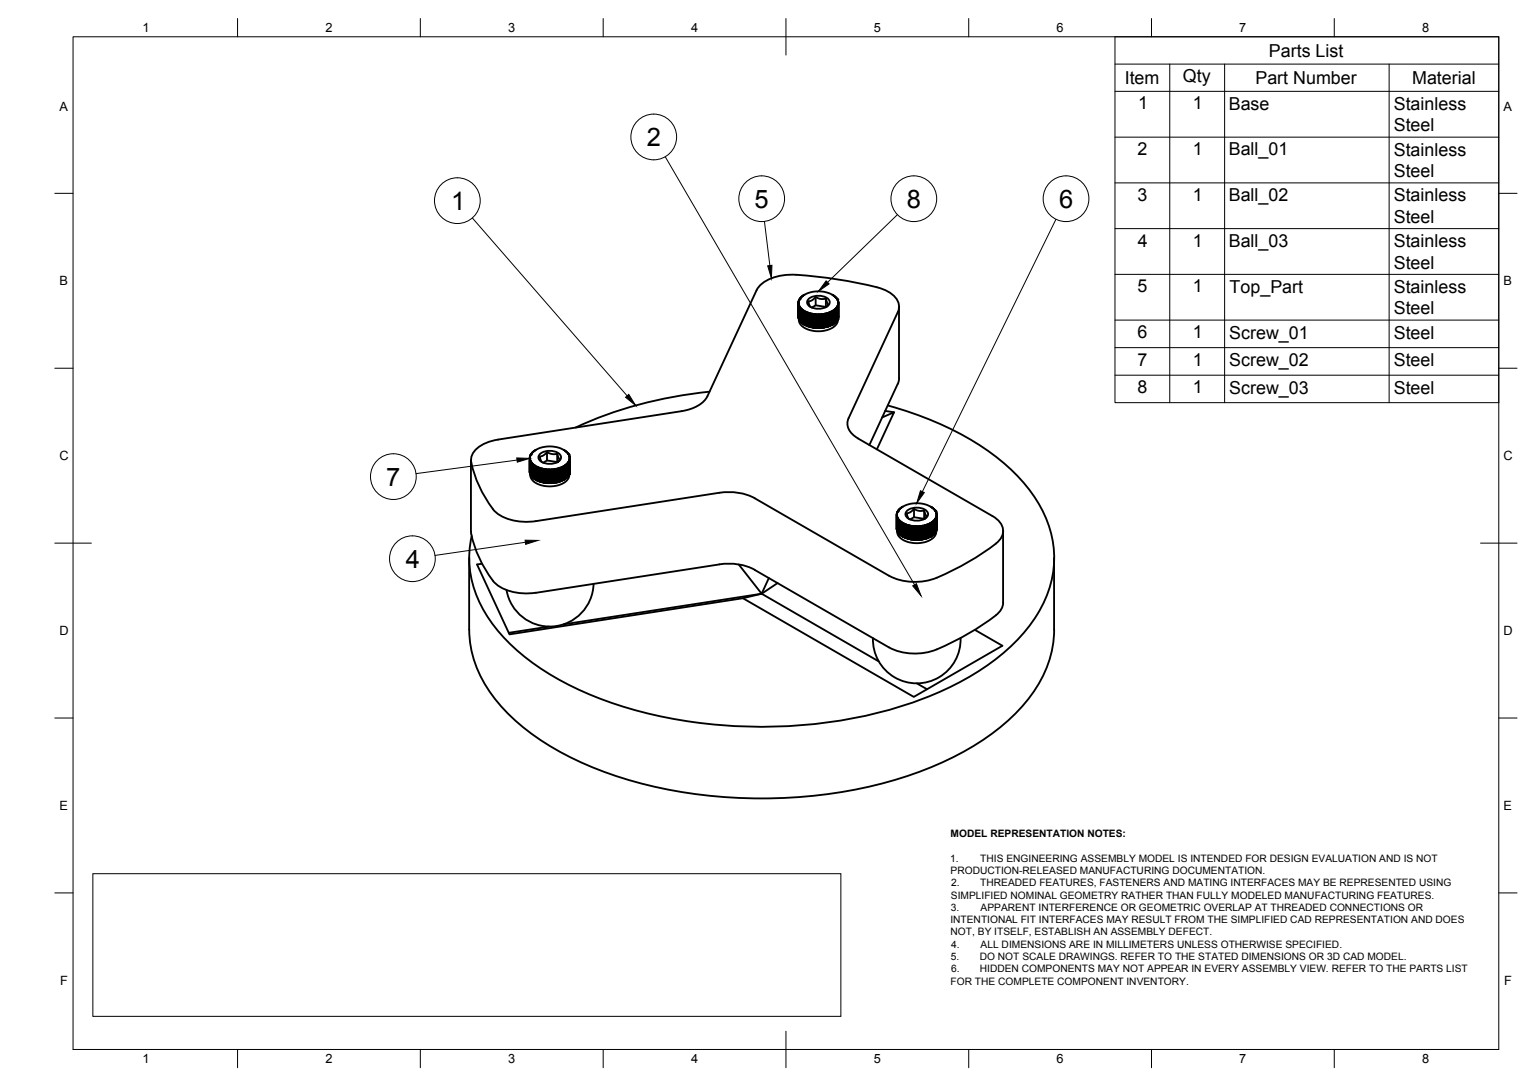
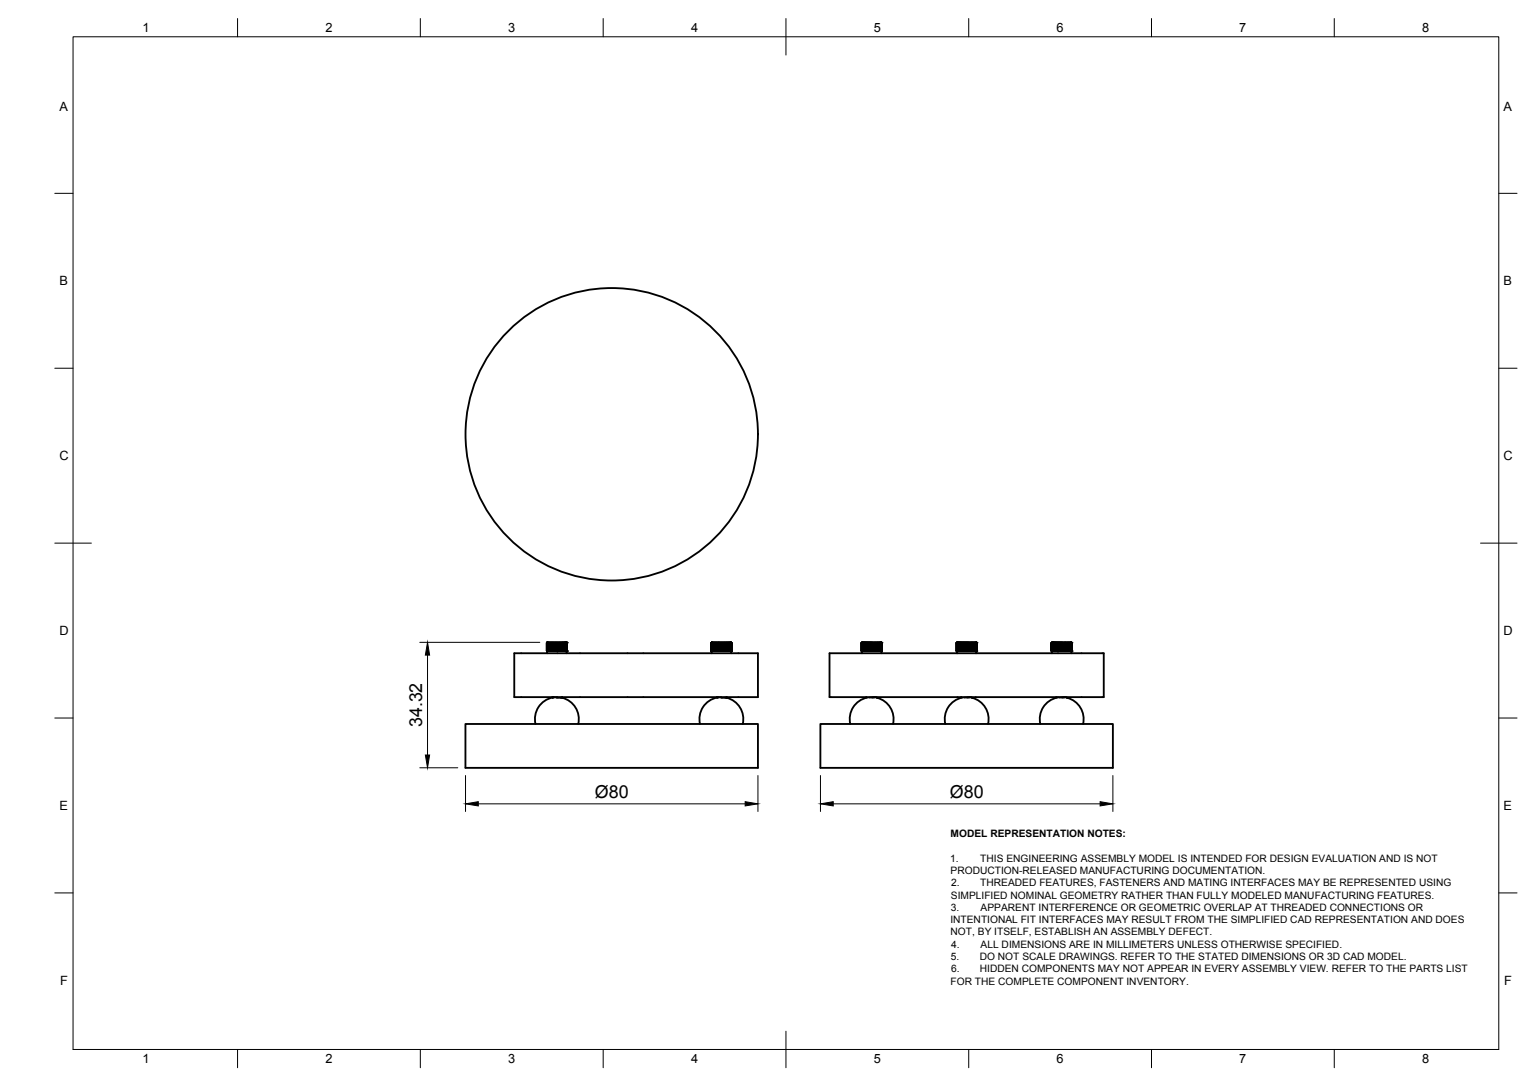
ISO-10303-21;
HEADER;
/* Generated by software containing ST-Developer
 * from STEP Tools, Inc. (www.steptools.com) 
 */

FILE_DESCRIPTION(
/* description */ (''),
/* implementation_level */ '2;1');

FILE_NAME(
/* name */ 'BR-152',
/* time_stamp */ '2026-10-05T00:14:20-07:00',
/* author */ (''),
/* organization */ (''),
/* preprocessor_version */ 'ST-DEVELOPER v20.2',
/* originating_system */ 'Autodesk Translation Framework v15.15.0.0',
/* authorisation */ '');

FILE_SCHEMA (('AUTOMOTIVE_DESIGN { 1 0 10303 214 3 1 1 }'));
ENDSEC;

DATA;
#10=MECHANICAL_DESIGN_GEOMETRIC_PRESENTATION_REPRESENTATION('',(#3371,#3372,
#3373,#3374,#3375,#3376,#3377,#3378),#75336);
#11=ITEM_DEFINED_TRANSFORMATION($,$,#32119,#36337);
#12=ITEM_DEFINED_TRANSFORMATION($,$,#32134,#36338);
#13=ITEM_DEFINED_TRANSFORMATION($,$,#32137,#36339);
#14=ITEM_DEFINED_TRANSFORMATION($,$,#32140,#36340);
#15=ITEM_DEFINED_TRANSFORMATION($,$,#32143,#36341);
#16=ITEM_DEFINED_TRANSFORMATION($,$,#32197,#36342);
#17=ITEM_DEFINED_TRANSFORMATION($,$,#33577,#36343);
#18=ITEM_DEFINED_TRANSFORMATION($,$,#34957,#36344);
#19=(
REPRESENTATION_RELATIONSHIP($,$,#75368,#75367)
REPRESENTATION_RELATIONSHIP_WITH_TRANSFORMATION(#11)
SHAPE_REPRESENTATION_RELATIONSHIP()
);
#20=(
REPRESENTATION_RELATIONSHIP($,$,#75369,#75367)
REPRESENTATION_RELATIONSHIP_WITH_TRANSFORMATION(#12)
SHAPE_REPRESENTATION_RELATIONSHIP()
);
#21=(
REPRESENTATION_RELATIONSHIP($,$,#75370,#75367)
REPRESENTATION_RELATIONSHIP_WITH_TRANSFORMATION(#13)
SHAPE_REPRESENTATION_RELATIONSHIP()
);
#22=(
REPRESENTATION_RELATIONSHIP($,$,#75371,#75367)
REPRESENTATION_RELATIONSHIP_WITH_TRANSFORMATION(#14)
SHAPE_REPRESENTATION_RELATIONSHIP()
);
#23=(
REPRESENTATION_RELATIONSHIP($,$,#75372,#75367)
REPRESENTATION_RELATIONSHIP_WITH_TRANSFORMATION(#15)
SHAPE_REPRESENTATION_RELATIONSHIP()
);
#24=(
REPRESENTATION_RELATIONSHIP($,$,#75373,#75367)
REPRESENTATION_RELATIONSHIP_WITH_TRANSFORMATION(#16)
SHAPE_REPRESENTATION_RELATIONSHIP()
);
#25=(
REPRESENTATION_RELATIONSHIP($,$,#75374,#75367)
REPRESENTATION_RELATIONSHIP_WITH_TRANSFORMATION(#17)
SHAPE_REPRESENTATION_RELATIONSHIP()
);
#26=(
REPRESENTATION_RELATIONSHIP($,$,#75375,#75367)
REPRESENTATION_RELATIONSHIP_WITH_TRANSFORMATION(#18)
SHAPE_REPRESENTATION_RELATIONSHIP()
);
#27=CONTEXT_DEPENDENT_SHAPE_REPRESENTATION(#19,#75359);
#28=CONTEXT_DEPENDENT_SHAPE_REPRESENTATION(#20,#75360);
#29=CONTEXT_DEPENDENT_SHAPE_REPRESENTATION(#21,#75361);
#30=CONTEXT_DEPENDENT_SHAPE_REPRESENTATION(#22,#75362);
#31=CONTEXT_DEPENDENT_SHAPE_REPRESENTATION(#23,#75363);
#32=CONTEXT_DEPENDENT_SHAPE_REPRESENTATION(#24,#75364);
#33=CONTEXT_DEPENDENT_SHAPE_REPRESENTATION(#25,#75365);
#34=CONTEXT_DEPENDENT_SHAPE_REPRESENTATION(#26,#75366);
#35=NEXT_ASSEMBLY_USAGE_OCCURRENCE('Base:1','Base:1','Base:1',#75377,#75378,
'Base:1');
#36=NEXT_ASSEMBLY_USAGE_OCCURRENCE('Ball_01:1','Ball_01:1','Ball_01:1',
#75377,#75379,'Ball_01:1');
#37=NEXT_ASSEMBLY_USAGE_OCCURRENCE('Ball_02:1','Ball_02:1','Ball_02:1',
#75377,#75380,'Ball_02:1');
#38=NEXT_ASSEMBLY_USAGE_OCCURRENCE('Ball_03:1','Ball_03:1','Ball_03:1',
#75377,#75381,'Ball_03:1');
#39=NEXT_ASSEMBLY_USAGE_OCCURRENCE('Top_Part:1','Top_Part:1',
'Top_Part:1',#75377,#75382,'Top_Part:1');
#40=NEXT_ASSEMBLY_USAGE_OCCURRENCE('Screw_01:1','Screw_01:1',
'Screw_01:1',#75377,#75383,'Screw_01:1');
#41=NEXT_ASSEMBLY_USAGE_OCCURRENCE('Screw_02:1','Screw_02:1',
'Screw_02:1',#75377,#75384,'Screw_02:1');
#42=NEXT_ASSEMBLY_USAGE_OCCURRENCE('Screw_03:1','Screw_03:1',
'Screw_03:1',#75377,#75385,'Screw_03:1');
#43=(
BOUNDED_SURFACE()
B_SPLINE_SURFACE(1,2,((#54054,#54055,#54056,#54057,#54058,#54059,#54060,
#54061,#54062,#54063,#54064,#54065,#54066,#54067,#54068,#54069,#54070,#54071,
#54072,#54073,#54074,#54075,#54076,#54077,#54078,#54079,#54080,#54081,#54082,
#54083,#54084,#54085,#54086,#54087,#54088,#54089,#54090,#54091,#54092,#54093,
#54094,#54095,#54096,#54097,#54098,#54099,#54100,#54101,#54102,#54103,#54104,
#54105,#54106,#54107,#54108,#54109,#54110,#54111,#54112,#54113,#54114,#54115,
#54116,#54117,#54118,#54119,#54120,#54121,#54122,#54123,#54124,#54125,#54126,
#54127,#54128,#54129,#54130,#54131,#54132,#54133,#54134,#54135,#54136,#54137,
#54138,#54139,#54140,#54141,#54142,#54143,#54144,#54145,#54146,#54147,#54148,
#54149,#54150,#54151,#54152,#54153,#54154,#54155,#54156,#54157,#54158,#54159,
#54160,#54161,#54162,#54163,#54164,#54165,#54166,#54167,#54168,#54169,#54170,
#54171,#54172,#54173,#54174,#54175,#54176,#54177,#54178,#54179,#54180,#54181,
#54182,#54183,#54184,#54185,#54186,#54187,#54188,#54189,#54190,#54191,#54192,
#54193,#54194,#54195,#54196,#54197,#54198,#54199,#54200,#54201,#54202,#54203,
#54204,#54205,#54206,#54207,#54208,#54209,#54210,#54211,#54212,#54213,#54214,
#54215,#54216,#54217,#54218,#54219,#54220,#54221,#54222,#54223,#54224,#54225,
#54226,#54227,#54228,#54229,#54230,#54231,#54232,#54233,#54234,#54235,#54236,
#54237,#54238,#54239,#54240,#54241,#54242,#54243,#54244,#54245,#54246,#54247,
#54248,#54249,#54250,#54251,#54252,#54253,#54254,#54255,#54256,#54257,#54258,
#54259,#54260,#54261,#54262,#54263,#54264,#54265,#54266,#54267,#54268,#54269,
#54270,#54271,#54272,#54273,#54274,#54275,#54276,#54277,#54278,#54279,#54280,
#54281,#54282,#54283,#54284,#54285,#54286,#54287,#54288,#54289,#54290,#54291,
#54292,#54293,#54294,#54295,#54296,#54297,#54298,#54299,#54300,#54301,#54302,
#54303,#54304,#54305,#54306,#54307,#54308,#54309,#54310,#54311,#54312,#54313,
#54314,#54315,#54316,#54317,#54318,#54319,#54320,#54321,#54322,#54323,#54324,
#54325,#54326,#54327,#54328,#54329,#54330,#54331,#54332,#54333,#54334,#54335,
#54336,#54337,#54338,#54339,#54340,#54341,#54342,#54343,#54344,#54345,#54346,
#54347,#54348,#54349,#54350,#54351,#54352,#54353,#54354,#54355,#54356,#54357,
#54358,#54359,#54360,#54361,#54362,#54363,#54364,#54365,#54366,#54367,#54368,
#54369,#54370,#54371,#54372,#54373,#54374,#54375,#54376,#54377,#54378,#54379,
#54380,#54381,#54382,#54383,#54384,#54385,#54386,#54387,#54388,#54389,#54390,
#54391,#54392,#54393,#54394,#54395,#54396,#54397,#54398,#54399,#54400,#54401,
#54402,#54403,#54404,#54405,#54406,#54407,#54408,#54409,#54410,#54411,#54412,
#54413,#54414,#54415,#54416,#54417,#54418,#54419,#54420,#54421,#54422,#54423,
#54424,#54425,#54426),(#54427,#54428,#54429,#54430,#54431,#54432,#54433,
#54434,#54435,#54436,#54437,#54438,#54439,#54440,#54441,#54442,#54443,#54444,
#54445,#54446,#54447,#54448,#54449,#54450,#54451,#54452,#54453,#54454,#54455,
#54456,#54457,#54458,#54459,#54460,#54461,#54462,#54463,#54464,#54465,#54466,
#54467,#54468,#54469,#54470,#54471,#54472,#54473,#54474,#54475,#54476,#54477,
#54478,#54479,#54480,#54481,#54482,#54483,#54484,#54485,#54486,#54487,#54488,
#54489,#54490,#54491,#54492,#54493,#54494,#54495,#54496,#54497,#54498,#54499,
#54500,#54501,#54502,#54503,#54504,#54505,#54506,#54507,#54508,#54509,#54510,
#54511,#54512,#54513,#54514,#54515,#54516,#54517,#54518,#54519,#54520,#54521,
#54522,#54523,#54524,#54525,#54526,#54527,#54528,#54529,#54530,#54531,#54532,
#54533,#54534,#54535,#54536,#54537,#54538,#54539,#54540,#54541,#54542,#54543,
#54544,#54545,#54546,#54547,#54548,#54549,#54550,#54551,#54552,#54553,#54554,
#54555,#54556,#54557,#54558,#54559,#54560,#54561,#54562,#54563,#54564,#54565,
#54566,#54567,#54568,#54569,#54570,#54571,#54572,#54573,#54574,#54575,#54576,
#54577,#54578,#54579,#54580,#54581,#54582,#54583,#54584,#54585,#54586,#54587,
#54588,#54589,#54590,#54591,#54592,#54593,#54594,#54595,#54596,#54597,#54598,
#54599,#54600,#54601,#54602,#54603,#54604,#54605,#54606,#54607,#54608,#54609,
#54610,#54611,#54612,#54613,#54614,#54615,#54616,#54617,#54618,#54619,#54620,
#54621,#54622,#54623,#54624,#54625,#54626,#54627,#54628,#54629,#54630,#54631,
#54632,#54633,#54634,#54635,#54636,#54637,#54638,#54639,#54640,#54641,#54642,
#54643,#54644,#54645,#54646,#54647,#54648,#54649,#54650,#54651,#54652,#54653,
#54654,#54655,#54656,#54657,#54658,#54659,#54660,#54661,#54662,#54663,#54664,
#54665,#54666,#54667,#54668,#54669,#54670,#54671,#54672,#54673,#54674,#54675,
#54676,#54677,#54678,#54679,#54680,#54681,#54682,#54683,#54684,#54685,#54686,
#54687,#54688,#54689,#54690,#54691,#54692,#54693,#54694,#54695,#54696,#54697,
#54698,#54699,#54700,#54701,#54702,#54703,#54704,#54705,#54706,#54707,#54708,
#54709,#54710,#54711,#54712,#54713,#54714,#54715,#54716,#54717,#54718,#54719,
#54720,#54721,#54722,#54723,#54724,#54725,#54726,#54727,#54728,#54729,#54730,
#54731,#54732,#54733,#54734,#54735,#54736,#54737,#54738,#54739,#54740,#54741,
#54742,#54743,#54744,#54745,#54746,#54747,#54748,#54749,#54750,#54751,#54752,
#54753,#54754,#54755,#54756,#54757,#54758,#54759,#54760,#54761,#54762,#54763,
#54764,#54765,#54766,#54767,#54768,#54769,#54770,#54771,#54772,#54773,#54774,
#54775,#54776,#54777,#54778,#54779,#54780,#54781,#54782,#54783,#54784,#54785,
#54786,#54787,#54788,#54789,#54790,#54791,#54792,#54793,#54794,#54795,#54796,
#54797,#54798,#54799)),.UNSPECIFIED.,.F.,.F.,.F.)
B_SPLINE_SURFACE_WITH_KNOTS((2,2),(3,2,2,2,2,2,2,2,2,2,2,2,2,2,2,2,2,2,
2,2,2,2,2,2,2,2,2,2,2,2,2,2,2,2,2,2,2,2,2,2,2,2,2,2,2,2,2,2,2,2,2,2,2,2,
2,2,2,2,2,2,2,2,2,2,2,2,2,2,2,2,2,2,2,2,2,2,2,2,2,2,2,2,2,2,2,2,2,2,2,2,
2,2,2,2,2,2,2,2,2,2,2,2,2,2,2,2,2,2,2,2,2,2,2,2,2,2,2,2,2,2,2,2,2,2,2,2,
2,2,2,2,2,2,2,2,2,2,2,2,2,2,2,2,2,2,2,2,2,2,2,2,2,2,2,2,2,2,2,2,2,2,2,2,
2,2,2,2,2,2,2,2,2,2,2,2,2,2,2,2,2,2,2,2,2,2,2,2,3),(-2.30253870309941E-5,
1.),(0.,0.00537634408602151,0.010752688172043,0.0161290322580645,0.021505376344086,
0.0268817204301075,0.032258064516129,0.0376344086021505,0.043010752688172,
0.0483870967741935,0.0537634408602151,0.0591397849462366,0.0645161290322581,
0.0698924731182796,0.0752688172043011,0.0806451612903226,0.0860215053763441,
0.0913978494623656,0.0967741935483871,0.102150537634409,0.10752688172043,
0.112903225806452,0.118279569892473,0.123655913978495,0.129032258064516,
0.134408602150538,0.139784946236559,0.145161290322581,0.150537634408602,
0.155913978494624,0.161290322580645,0.166666666666667,0.172043010752688,
0.17741935483871,0.182795698924731,0.188172043010753,0.193548387096774,
0.198924731182796,0.204301075268817,0.209677419354839,0.21505376344086,
0.220430107526882,0.225806451612903,0.231182795698925,0.236559139784946,
0.241935483870968,0.247311827956989,0.252688172043011,0.258064516129032,
0.263440860215054,0.268817204301075,0.274193548387097,0.279569892473118,
0.28494623655914,0.290322580645161,0.295698924731183,0.301075268817204,
0.306451612903226,0.311827956989247,0.317204301075269,0.32258064516129,
0.327956989247312,0.333333333333333,0.338709677419355,0.344086021505376,
0.349462365591398,0.354838709677419,0.360215053763441,0.365591397849462,
0.370967741935484,0.376344086021505,0.381720430107527,0.387096774193548,
0.39247311827957,0.397849462365591,0.403225806451613,0.408602150537634,
0.413978494623656,0.419354838709677,0.424731182795699,0.43010752688172,
0.435483870967742,0.440860215053763,0.446236559139785,0.451612903225806,
0.456989247311828,0.462365591397849,0.467741935483871,0.473118279569892,
0.478494623655914,0.483870967741935,0.489247311827957,0.494623655913978,
0.5,0.505376344086022,0.510752688172043,0.516129032258065,0.521505376344086,
0.526881720430108,0.532258064516129,0.537634408602151,0.543010752688172,
0.548387096774194,0.553763440860215,0.559139784946237,0.564516129032258,
0.56989247311828,0.575268817204301,0.580645161290323,0.586021505376344,
0.591397849462366,0.596774193548387,0.602150537634409,0.60752688172043,
0.612903225806452,0.618279569892473,0.623655913978495,0.629032258064516,
0.634408602150538,0.639784946236559,0.645161290322581,0.650537634408602,
0.655913978494624,0.661290322580645,0.666666666666667,0.672043010752688,
0.67741935483871,0.682795698924731,0.688172043010753,0.693548387096774,
0.698924731182796,0.704301075268817,0.709677419354839,0.71505376344086,
0.720430107526882,0.725806451612903,0.731182795698925,0.736559139784946,
0.741935483870968,0.747311827956989,0.752688172043011,0.758064516129032,
0.763440860215054,0.768817204301075,0.774193548387097,0.779569892473118,
0.78494623655914,0.790322580645161,0.795698924731183,0.801075268817204,
0.806451612903226,0.811827956989247,0.817204301075269,0.82258064516129,
0.827956989247312,0.833333333333333,0.838709677419355,0.844086021505376,
0.849462365591398,0.854838709677419,0.860215053763441,0.865591397849462,
0.870967741935484,0.876344086021505,0.881720430107527,0.887096774193548,
0.89247311827957,0.897849462365591,0.903225806451613,0.908602150537634,
0.913978494623656,0.919354838709677,0.924731182795699,0.93010752688172,
0.935483870967742,0.940860215053763,0.946236559139785,0.951612903225806,
0.956989247311828,0.962365591397849,0.967741935483871,0.973118279569892,
0.978494623655914,0.983870967741935,0.989247311827957,0.994623655913978,
1.),.UNSPECIFIED.)
GEOMETRIC_REPRESENTATION_ITEM()
RATIONAL_B_SPLINE_SURFACE(((1.,0.866025403784439,1.,0.866025403784439,1.,
0.866025403784439,1.,0.866025403784439,1.,0.866025403784439,1.,0.866025403784439,
1.,0.866025403784439,1.,0.866025403784439,1.,0.866025403784439,1.,0.866025403784439,
1.,0.866025403784439,1.,0.866025403784439,1.,0.866025403784439,1.,0.866025403784439,
1.,0.866025403784439,1.,0.866025403784439,1.,0.866025403784439,1.,0.866025403784439,
1.,0.866025403784439,1.,0.866025403784439,1.,0.866025403784439,1.,0.866025403784439,
1.,0.866025403784439,1.,0.866025403784439,1.,0.866025403784439,1.,0.866025403784439,
1.,0.866025403784439,1.,0.866025403784439,1.,0.866025403784439,1.,0.866025403784439,
1.,0.866025403784439,1.,0.866025403784439,1.,0.866025403784439,1.,0.866025403784439,
1.,0.866025403784439,1.,0.866025403784439,1.,0.866025403784439,1.,0.866025403784439,
1.,0.866025403784439,1.,0.866025403784439,1.,0.866025403784439,1.,0.866025403784439,
1.,0.866025403784439,1.,0.866025403784439,1.,0.866025403784439,1.,0.866025403784439,
1.,0.866025403784439,1.,0.866025403784439,1.,0.866025403784439,1.,0.866025403784439,
1.,0.866025403784439,1.,0.866025403784439,1.,0.866025403784439,1.,0.866025403784439,
1.,0.866025403784439,1.,0.866025403784439,1.,0.866025403784439,1.,0.866025403784439,
1.,0.866025403784439,1.,0.866025403784439,1.,0.866025403784439,1.,0.866025403784439,
1.,0.866025403784439,1.,0.866025403784439,1.,0.866025403784439,1.,0.866025403784439,
1.,0.866025403784439,1.,0.866025403784439,1.,0.866025403784439,1.,0.866025403784439,
1.,0.866025403784439,1.,0.866025403784439,1.,0.866025403784439,1.,0.866025403784439,
1.,0.866025403784439,1.,0.866025403784439,1.,0.866025403784439,1.,0.866025403784439,
1.,0.866025403784439,1.,0.866025403784439,1.,0.866025403784439,1.,0.866025403784439,
1.,0.866025403784439,1.,0.866025403784439,1.,0.866025403784439,1.,0.866025403784439,
1.,0.866025403784439,1.,0.866025403784439,1.,0.866025403784439,1.,0.866025403784439,
1.,0.866025403784439,1.,0.866025403784439,1.,0.866025403784439,1.,0.866025403784439,
1.,0.866025403784439,1.,0.866025403784439,1.,0.866025403784439,1.,0.866025403784439,
1.,0.866025403784439,1.,0.866025403784439,1.,0.866025403784439,1.,0.866025403784439,
1.,0.866025403784439,1.,0.866025403784439,1.,0.866025403784439,1.,0.866025403784439,
1.,0.866025403784439,1.,0.866025403784439,1.,0.866025403784439,1.,0.866025403784439,
1.,0.866025403784439,1.,0.866025403784439,1.,0.866025403784439,1.,0.866025403784439,
1.,0.866025403784439,1.,0.866025403784439,1.,0.866025403784439,1.,0.866025403784439,
1.,0.866025403784439,1.,0.866025403784439,1.,0.866025403784439,1.,0.866025403784439,
1.,0.866025403784439,1.,0.866025403784439,1.,0.866025403784439,1.,0.866025403784439,
1.,0.866025403784439,1.,0.866025403784439,1.,0.866025403784439,1.,0.866025403784439,
1.,0.866025403784439,1.,0.866025403784439,1.,0.866025403784439,1.,0.866025403784439,
1.,0.866025403784439,1.,0.866025403784439,1.,0.866025403784439,1.,0.866025403784439,
1.,0.866025403784439,1.,0.866025403784439,1.,0.866025403784439,1.,0.866025403784439,
1.,0.866025403784439,1.,0.866025403784439,1.,0.866025403784439,1.,0.866025403784439,
1.,0.866025403784439,1.,0.866025403784439,1.,0.866025403784439,1.,0.866025403784439,
1.,0.866025403784439,1.,0.866025403784439,1.,0.866025403784439,1.,0.866025403784439,
1.,0.866025403784439,1.,0.866025403784439,1.,0.866025403784439,1.,0.866025403784439,
1.,0.866025403784439,1.,0.866025403784439,1.,0.866025403784439,1.,0.866025403784439,
1.,0.866025403784439,1.,0.866025403784439,1.,0.866025403784439,1.,0.866025403784439,
1.,0.866025403784439,1.,0.866025403784439,1.,0.866025403784439,1.,0.866025403784439,
1.,0.866025403784439,1.,0.866025403784439,1.,0.866025403784439,1.,0.866025403784439,
1.,0.866025403784439,1.,0.866025403784439,1.,0.866025403784439,1.,0.866025403784439,
1.,0.866025403784439,1.,0.866025403784439,1.,0.866025403784439,1.,0.866025403784439,
1.,0.866025403784439,1.,0.866025403784439,1.,0.866025403784439,1.,0.866025403784439,
1.),(1.,0.866025403784439,1.,0.866025403784439,1.,0.866025403784439,1.,
0.866025403784439,1.,0.866025403784439,1.,0.866025403784439,1.,0.866025403784439,
1.,0.866025403784439,1.,0.866025403784439,1.,0.866025403784439,1.,0.866025403784439,
1.,0.866025403784439,1.,0.866025403784439,1.,0.866025403784439,1.,0.866025403784439,
1.,0.866025403784439,1.,0.866025403784439,1.,0.866025403784439,1.,0.866025403784439,
1.,0.866025403784439,1.,0.866025403784439,1.,0.866025403784439,1.,0.866025403784439,
1.,0.866025403784439,1.,0.866025403784439,1.,0.866025403784439,1.,0.866025403784439,
1.,0.866025403784439,1.,0.866025403784439,1.,0.866025403784439,1.,0.866025403784439,
1.,0.866025403784439,1.,0.866025403784439,1.,0.866025403784439,1.,0.866025403784439,
1.,0.866025403784439,1.,0.866025403784439,1.,0.866025403784439,1.,0.866025403784439,
1.,0.866025403784439,1.,0.866025403784439,1.,0.866025403784439,1.,0.866025403784439,
1.,0.866025403784439,1.,0.866025403784439,1.,0.866025403784439,1.,0.866025403784439,
1.,0.866025403784439,1.,0.866025403784439,1.,0.866025403784439,1.,0.866025403784439,
1.,0.866025403784439,1.,0.866025403784439,1.,0.866025403784439,1.,0.866025403784439,
1.,0.866025403784439,1.,0.866025403784439,1.,0.866025403784439,1.,0.866025403784439,
1.,0.866025403784439,1.,0.866025403784439,1.,0.866025403784439,1.,0.866025403784439,
1.,0.866025403784439,1.,0.866025403784439,1.,0.866025403784439,1.,0.866025403784439,
1.,0.866025403784439,1.,0.866025403784439,1.,0.866025403784439,1.,0.866025403784439,
1.,0.866025403784439,1.,0.866025403784439,1.,0.866025403784439,1.,0.866025403784439,
1.,0.866025403784439,1.,0.866025403784439,1.,0.866025403784439,1.,0.866025403784439,
1.,0.866025403784439,1.,0.866025403784439,1.,0.866025403784439,1.,0.866025403784439,
1.,0.866025403784439,1.,0.866025403784439,1.,0.866025403784439,1.,0.866025403784439,
1.,0.866025403784439,1.,0.866025403784439,1.,0.866025403784439,1.,0.866025403784439,
1.,0.866025403784439,1.,0.866025403784439,1.,0.866025403784439,1.,0.866025403784439,
1.,0.866025403784439,1.,0.866025403784439,1.,0.866025403784439,1.,0.866025403784439,
1.,0.866025403784439,1.,0.866025403784439,1.,0.866025403784439,1.,0.866025403784439,
1.,0.866025403784439,1.,0.866025403784439,1.,0.866025403784439,1.,0.866025403784439,
1.,0.866025403784439,1.,0.866025403784439,1.,0.866025403784439,1.,0.866025403784439,
1.,0.866025403784439,1.,0.866025403784439,1.,0.866025403784439,1.,0.866025403784439,
1.,0.866025403784439,1.,0.866025403784439,1.,0.866025403784439,1.,0.866025403784439,
1.,0.866025403784439,1.,0.866025403784439,1.,0.866025403784439,1.,0.866025403784439,
1.,0.866025403784439,1.,0.866025403784439,1.,0.866025403784439,1.,0.866025403784439,
1.,0.866025403784439,1.,0.866025403784439,1.,0.866025403784439,1.,0.866025403784439,
1.,0.866025403784439,1.,0.866025403784439,1.,0.866025403784439,1.,0.866025403784439,
1.,0.866025403784439,1.,0.866025403784439,1.,0.866025403784439,1.,0.866025403784439,
1.,0.866025403784439,1.,0.866025403784439,1.,0.866025403784439,1.,0.866025403784439,
1.,0.866025403784439,1.,0.866025403784439,1.,0.866025403784439,1.,0.866025403784439,
1.,0.866025403784439,1.,0.866025403784439,1.,0.866025403784439,1.,0.866025403784439,
1.,0.866025403784439,1.,0.866025403784439,1.,0.866025403784439,1.,0.866025403784439,
1.,0.866025403784439,1.,0.866025403784439,1.,0.866025403784439,1.,0.866025403784439,
1.,0.866025403784439,1.,0.866025403784439,1.,0.866025403784439,1.,0.866025403784439,
1.,0.866025403784439,1.,0.866025403784439,1.,0.866025403784439,1.,0.866025403784439,
1.,0.866025403784439,1.,0.866025403784439,1.,0.866025403784439,1.,0.866025403784439,
1.,0.866025403784439,1.,0.866025403784439,1.,0.866025403784439,1.,0.866025403784439,
1.,0.866025403784439,1.,0.866025403784439,1.,0.866025403784439,1.,0.866025403784439,
1.,0.866025403784439,1.,0.866025403784439,1.,0.866025403784439,1.,0.866025403784439,
1.,0.866025403784439,1.,0.866025403784439,1.,0.866025403784439,1.)))
REPRESENTATION_ITEM('')
SURFACE()
);
#44=(
BOUNDED_SURFACE()
B_SPLINE_SURFACE(1,2,((#54828,#54829,#54830,#54831,#54832,#54833,#54834,
#54835,#54836,#54837,#54838,#54839,#54840,#54841,#54842,#54843,#54844,#54845,
#54846,#54847,#54848,#54849,#54850,#54851,#54852,#54853,#54854,#54855,#54856,
#54857,#54858,#54859,#54860,#54861,#54862,#54863,#54864,#54865,#54866,#54867,
#54868,#54869,#54870,#54871,#54872,#54873,#54874,#54875,#54876,#54877,#54878,
#54879,#54880,#54881,#54882,#54883,#54884,#54885,#54886,#54887,#54888,#54889,
#54890,#54891,#54892,#54893,#54894,#54895,#54896,#54897,#54898,#54899,#54900,
#54901,#54902,#54903,#54904,#54905,#54906,#54907,#54908,#54909,#54910,#54911,
#54912,#54913,#54914,#54915,#54916,#54917,#54918,#54919,#54920,#54921,#54922,
#54923,#54924,#54925,#54926,#54927,#54928,#54929,#54930,#54931,#54932,#54933,
#54934,#54935,#54936,#54937,#54938,#54939,#54940,#54941,#54942,#54943,#54944,
#54945,#54946,#54947,#54948,#54949,#54950,#54951,#54952,#54953,#54954,#54955,
#54956,#54957,#54958,#54959,#54960,#54961,#54962,#54963,#54964,#54965,#54966,
#54967,#54968,#54969,#54970,#54971,#54972,#54973,#54974,#54975,#54976,#54977,
#54978,#54979,#54980,#54981,#54982,#54983,#54984,#54985,#54986,#54987,#54988,
#54989,#54990,#54991,#54992,#54993,#54994,#54995,#54996,#54997,#54998,#54999,
#55000,#55001,#55002,#55003,#55004,#55005,#55006,#55007,#55008,#55009,#55010,
#55011,#55012,#55013,#55014,#55015,#55016,#55017,#55018,#55019,#55020,#55021,
#55022,#55023,#55024,#55025,#55026,#55027,#55028,#55029,#55030,#55031,#55032,
#55033,#55034,#55035,#55036,#55037,#55038,#55039,#55040,#55041,#55042,#55043,
#55044,#55045,#55046,#55047,#55048,#55049,#55050,#55051,#55052,#55053,#55054,
#55055,#55056,#55057,#55058,#55059,#55060,#55061,#55062,#55063,#55064,#55065,
#55066,#55067,#55068,#55069,#55070,#55071,#55072,#55073,#55074,#55075,#55076,
#55077,#55078,#55079,#55080,#55081,#55082,#55083,#55084,#55085,#55086,#55087,
#55088,#55089,#55090,#55091,#55092,#55093,#55094,#55095,#55096,#55097,#55098,
#55099,#55100,#55101,#55102,#55103,#55104,#55105,#55106,#55107,#55108,#55109,
#55110,#55111,#55112,#55113,#55114,#55115,#55116,#55117,#55118,#55119,#55120,
#55121,#55122,#55123,#55124,#55125,#55126,#55127,#55128,#55129,#55130,#55131,
#55132,#55133,#55134,#55135,#55136,#55137,#55138,#55139,#55140,#55141,#55142,
#55143,#55144,#55145,#55146,#55147,#55148,#55149,#55150,#55151,#55152,#55153,
#55154,#55155,#55156,#55157,#55158,#55159,#55160,#55161,#55162,#55163,#55164,
#55165,#55166,#55167,#55168,#55169,#55170,#55171,#55172,#55173,#55174,#55175,
#55176,#55177,#55178,#55179,#55180,#55181,#55182,#55183,#55184,#55185,#55186,
#55187,#55188,#55189,#55190,#55191,#55192,#55193,#55194,#55195,#55196,#55197,
#55198,#55199,#55200),(#55201,#55202,#55203,#55204,#55205,#55206,#55207,
#55208,#55209,#55210,#55211,#55212,#55213,#55214,#55215,#55216,#55217,#55218,
#55219,#55220,#55221,#55222,#55223,#55224,#55225,#55226,#55227,#55228,#55229,
#55230,#55231,#55232,#55233,#55234,#55235,#55236,#55237,#55238,#55239,#55240,
#55241,#55242,#55243,#55244,#55245,#55246,#55247,#55248,#55249,#55250,#55251,
#55252,#55253,#55254,#55255,#55256,#55257,#55258,#55259,#55260,#55261,#55262,
#55263,#55264,#55265,#55266,#55267,#55268,#55269,#55270,#55271,#55272,#55273,
#55274,#55275,#55276,#55277,#55278,#55279,#55280,#55281,#55282,#55283,#55284,
#55285,#55286,#55287,#55288,#55289,#55290,#55291,#55292,#55293,#55294,#55295,
#55296,#55297,#55298,#55299,#55300,#55301,#55302,#55303,#55304,#55305,#55306,
#55307,#55308,#55309,#55310,#55311,#55312,#55313,#55314,#55315,#55316,#55317,
#55318,#55319,#55320,#55321,#55322,#55323,#55324,#55325,#55326,#55327,#55328,
#55329,#55330,#55331,#55332,#55333,#55334,#55335,#55336,#55337,#55338,#55339,
#55340,#55341,#55342,#55343,#55344,#55345,#55346,#55347,#55348,#55349,#55350,
#55351,#55352,#55353,#55354,#55355,#55356,#55357,#55358,#55359,#55360,#55361,
#55362,#55363,#55364,#55365,#55366,#55367,#55368,#55369,#55370,#55371,#55372,
#55373,#55374,#55375,#55376,#55377,#55378,#55379,#55380,#55381,#55382,#55383,
#55384,#55385,#55386,#55387,#55388,#55389,#55390,#55391,#55392,#55393,#55394,
#55395,#55396,#55397,#55398,#55399,#55400,#55401,#55402,#55403,#55404,#55405,
#55406,#55407,#55408,#55409,#55410,#55411,#55412,#55413,#55414,#55415,#55416,
#55417,#55418,#55419,#55420,#55421,#55422,#55423,#55424,#55425,#55426,#55427,
#55428,#55429,#55430,#55431,#55432,#55433,#55434,#55435,#55436,#55437,#55438,
#55439,#55440,#55441,#55442,#55443,#55444,#55445,#55446,#55447,#55448,#55449,
#55450,#55451,#55452,#55453,#55454,#55455,#55456,#55457,#55458,#55459,#55460,
#55461,#55462,#55463,#55464,#55465,#55466,#55467,#55468,#55469,#55470,#55471,
#55472,#55473,#55474,#55475,#55476,#55477,#55478,#55479,#55480,#55481,#55482,
#55483,#55484,#55485,#55486,#55487,#55488,#55489,#55490,#55491,#55492,#55493,
#55494,#55495,#55496,#55497,#55498,#55499,#55500,#55501,#55502,#55503,#55504,
#55505,#55506,#55507,#55508,#55509,#55510,#55511,#55512,#55513,#55514,#55515,
#55516,#55517,#55518,#55519,#55520,#55521,#55522,#55523,#55524,#55525,#55526,
#55527,#55528,#55529,#55530,#55531,#55532,#55533,#55534,#55535,#55536,#55537,
#55538,#55539,#55540,#55541,#55542,#55543,#55544,#55545,#55546,#55547,#55548,
#55549,#55550,#55551,#55552,#55553,#55554,#55555,#55556,#55557,#55558,#55559,
#55560,#55561,#55562,#55563,#55564,#55565,#55566,#55567,#55568,#55569,#55570,
#55571,#55572,#55573)),.UNSPECIFIED.,.F.,.F.,.F.)
B_SPLINE_SURFACE_WITH_KNOTS((2,2),(3,2,2,2,2,2,2,2,2,2,2,2,2,2,2,2,2,2,
2,2,2,2,2,2,2,2,2,2,2,2,2,2,2,2,2,2,2,2,2,2,2,2,2,2,2,2,2,2,2,2,2,2,2,2,
2,2,2,2,2,2,2,2,2,2,2,2,2,2,2,2,2,2,2,2,2,2,2,2,2,2,2,2,2,2,2,2,2,2,2,2,
2,2,2,2,2,2,2,2,2,2,2,2,2,2,2,2,2,2,2,2,2,2,2,2,2,2,2,2,2,2,2,2,2,2,2,2,
2,2,2,2,2,2,2,2,2,2,2,2,2,2,2,2,2,2,2,2,2,2,2,2,2,2,2,2,2,2,2,2,2,2,2,2,
2,2,2,2,2,2,2,2,2,2,2,2,2,2,2,2,2,2,2,2,2,2,2,2,3),(0.,1.00001535537392),
(0.,0.00537634408602151,0.010752688172043,0.0161290322580645,0.021505376344086,
0.0268817204301075,0.032258064516129,0.0376344086021505,0.043010752688172,
0.0483870967741935,0.0537634408602151,0.0591397849462366,0.0645161290322581,
0.0698924731182796,0.0752688172043011,0.0806451612903226,0.0860215053763441,
0.0913978494623656,0.0967741935483871,0.102150537634409,0.10752688172043,
0.112903225806452,0.118279569892473,0.123655913978495,0.129032258064516,
0.134408602150538,0.139784946236559,0.145161290322581,0.150537634408602,
0.155913978494624,0.161290322580645,0.166666666666667,0.172043010752688,
0.17741935483871,0.182795698924731,0.188172043010753,0.193548387096774,
0.198924731182796,0.204301075268817,0.209677419354839,0.21505376344086,
0.220430107526882,0.225806451612903,0.231182795698925,0.236559139784946,
0.241935483870968,0.247311827956989,0.252688172043011,0.258064516129032,
0.263440860215054,0.268817204301075,0.274193548387097,0.279569892473118,
0.28494623655914,0.290322580645161,0.295698924731183,0.301075268817204,
0.306451612903226,0.311827956989247,0.317204301075269,0.32258064516129,
0.327956989247312,0.333333333333333,0.338709677419355,0.344086021505376,
0.349462365591398,0.354838709677419,0.360215053763441,0.365591397849462,
0.370967741935484,0.376344086021505,0.381720430107527,0.387096774193548,
0.39247311827957,0.397849462365591,0.403225806451613,0.408602150537634,
0.413978494623656,0.419354838709677,0.424731182795699,0.43010752688172,
0.435483870967742,0.440860215053763,0.446236559139785,0.451612903225806,
0.456989247311828,0.462365591397849,0.467741935483871,0.473118279569892,
0.478494623655914,0.483870967741935,0.489247311827957,0.494623655913978,
0.5,0.505376344086022,0.510752688172043,0.516129032258065,0.521505376344086,
0.526881720430108,0.532258064516129,0.537634408602151,0.543010752688172,
0.548387096774194,0.553763440860215,0.559139784946237,0.564516129032258,
0.56989247311828,0.575268817204301,0.580645161290323,0.586021505376344,
0.591397849462366,0.596774193548387,0.602150537634409,0.60752688172043,
0.612903225806452,0.618279569892473,0.623655913978495,0.629032258064516,
0.634408602150538,0.639784946236559,0.645161290322581,0.650537634408602,
0.655913978494624,0.661290322580645,0.666666666666667,0.672043010752688,
0.67741935483871,0.682795698924731,0.688172043010753,0.693548387096774,
0.698924731182796,0.704301075268817,0.709677419354839,0.71505376344086,
0.720430107526882,0.725806451612903,0.731182795698925,0.736559139784946,
0.741935483870968,0.747311827956989,0.752688172043011,0.758064516129032,
0.763440860215054,0.768817204301075,0.774193548387097,0.779569892473118,
0.78494623655914,0.790322580645161,0.795698924731183,0.801075268817204,
0.806451612903226,0.811827956989247,0.817204301075269,0.82258064516129,
0.827956989247312,0.833333333333333,0.838709677419355,0.844086021505376,
0.849462365591398,0.854838709677419,0.860215053763441,0.865591397849462,
0.870967741935484,0.876344086021505,0.881720430107527,0.887096774193548,
0.89247311827957,0.897849462365591,0.903225806451613,0.908602150537634,
0.913978494623656,0.919354838709677,0.924731182795699,0.93010752688172,
0.935483870967742,0.940860215053763,0.946236559139785,0.951612903225806,
0.956989247311828,0.962365591397849,0.967741935483871,0.973118279569892,
0.978494623655914,0.983870967741935,0.989247311827957,0.994623655913978,
1.),.UNSPECIFIED.)
GEOMETRIC_REPRESENTATION_ITEM()
RATIONAL_B_SPLINE_SURFACE(((1.,0.866025403784439,1.,0.866025403784439,1.,
0.866025403784439,1.,0.866025403784439,1.,0.866025403784439,1.,0.866025403784439,
1.,0.866025403784439,1.,0.866025403784439,1.,0.866025403784439,1.,0.866025403784439,
1.,0.866025403784439,1.,0.866025403784439,1.,0.866025403784439,1.,0.866025403784439,
1.,0.866025403784439,1.,0.866025403784439,1.,0.866025403784439,1.,0.866025403784439,
1.,0.866025403784439,1.,0.866025403784439,1.,0.866025403784439,1.,0.866025403784439,
1.,0.866025403784439,1.,0.866025403784439,1.,0.866025403784439,1.,0.866025403784439,
1.,0.866025403784439,1.,0.866025403784439,1.,0.866025403784439,1.,0.866025403784439,
1.,0.866025403784439,1.,0.866025403784439,1.,0.866025403784439,1.,0.866025403784439,
1.,0.866025403784439,1.,0.866025403784439,1.,0.866025403784439,1.,0.866025403784439,
1.,0.866025403784439,1.,0.866025403784439,1.,0.866025403784439,1.,0.866025403784439,
1.,0.866025403784439,1.,0.866025403784439,1.,0.866025403784439,1.,0.866025403784439,
1.,0.866025403784439,1.,0.866025403784439,1.,0.866025403784439,1.,0.866025403784439,
1.,0.866025403784439,1.,0.866025403784439,1.,0.866025403784439,1.,0.866025403784439,
1.,0.866025403784439,1.,0.866025403784439,1.,0.866025403784439,1.,0.866025403784439,
1.,0.866025403784439,1.,0.866025403784439,1.,0.866025403784439,1.,0.866025403784439,
1.,0.866025403784439,1.,0.866025403784439,1.,0.866025403784439,1.,0.866025403784439,
1.,0.866025403784439,1.,0.866025403784439,1.,0.866025403784439,1.,0.866025403784439,
1.,0.866025403784439,1.,0.866025403784439,1.,0.866025403784439,1.,0.866025403784439,
1.,0.866025403784439,1.,0.866025403784439,1.,0.866025403784439,1.,0.866025403784439,
1.,0.866025403784439,1.,0.866025403784439,1.,0.866025403784439,1.,0.866025403784439,
1.,0.866025403784439,1.,0.866025403784439,1.,0.866025403784439,1.,0.866025403784439,
1.,0.866025403784439,1.,0.866025403784439,1.,0.866025403784439,1.,0.866025403784439,
1.,0.866025403784439,1.,0.866025403784439,1.,0.866025403784439,1.,0.866025403784439,
1.,0.866025403784439,1.,0.866025403784439,1.,0.866025403784439,1.,0.866025403784439,
1.,0.866025403784439,1.,0.866025403784439,1.,0.866025403784439,1.,0.866025403784439,
1.,0.866025403784439,1.,0.866025403784439,1.,0.866025403784439,1.,0.866025403784439,
1.,0.866025403784439,1.,0.866025403784439,1.,0.866025403784439,1.,0.866025403784439,
1.,0.866025403784439,1.,0.866025403784439,1.,0.866025403784439,1.,0.866025403784439,
1.,0.866025403784439,1.,0.866025403784439,1.,0.866025403784439,1.,0.866025403784439,
1.,0.866025403784439,1.,0.866025403784439,1.,0.866025403784439,1.,0.866025403784439,
1.,0.866025403784439,1.,0.866025403784439,1.,0.866025403784439,1.,0.866025403784439,
1.,0.866025403784439,1.,0.866025403784439,1.,0.866025403784439,1.,0.866025403784439,
1.,0.866025403784439,1.,0.866025403784439,1.,0.866025403784439,1.,0.866025403784439,
1.,0.866025403784439,1.,0.866025403784439,1.,0.866025403784439,1.,0.866025403784439,
1.,0.866025403784439,1.,0.866025403784439,1.,0.866025403784439,1.,0.866025403784439,
1.,0.866025403784439,1.,0.866025403784439,1.,0.866025403784439,1.,0.866025403784439,
1.,0.866025403784439,1.,0.866025403784439,1.,0.866025403784439,1.,0.866025403784439,
1.,0.866025403784439,1.,0.866025403784439,1.,0.866025403784439,1.,0.866025403784439,
1.,0.866025403784439,1.,0.866025403784439,1.,0.866025403784439,1.,0.866025403784439,
1.,0.866025403784439,1.,0.866025403784439,1.,0.866025403784439,1.,0.866025403784439,
1.,0.866025403784439,1.,0.866025403784439,1.,0.866025403784439,1.,0.866025403784439,
1.,0.866025403784439,1.,0.866025403784439,1.,0.866025403784439,1.,0.866025403784439,
1.,0.866025403784439,1.,0.866025403784439,1.,0.866025403784439,1.,0.866025403784439,
1.,0.866025403784439,1.,0.866025403784439,1.,0.866025403784439,1.,0.866025403784439,
1.,0.866025403784439,1.,0.866025403784439,1.,0.866025403784439,1.,0.866025403784439,
1.,0.866025403784439,1.,0.866025403784439,1.,0.866025403784439,1.,0.866025403784439,
1.),(1.,0.866025403784439,1.,0.866025403784439,1.,0.866025403784439,1.,
0.866025403784439,1.,0.866025403784439,1.,0.866025403784439,1.,0.866025403784439,
1.,0.866025403784439,1.,0.866025403784439,1.,0.866025403784439,1.,0.866025403784439,
1.,0.866025403784439,1.,0.866025403784439,1.,0.866025403784439,1.,0.866025403784439,
1.,0.866025403784439,1.,0.866025403784439,1.,0.866025403784439,1.,0.866025403784439,
1.,0.866025403784439,1.,0.866025403784439,1.,0.866025403784439,1.,0.866025403784439,
1.,0.866025403784439,1.,0.866025403784439,1.,0.866025403784439,1.,0.866025403784439,
1.,0.866025403784439,1.,0.866025403784439,1.,0.866025403784439,1.,0.866025403784439,
1.,0.866025403784439,1.,0.866025403784439,1.,0.866025403784439,1.,0.866025403784439,
1.,0.866025403784439,1.,0.866025403784439,1.,0.866025403784439,1.,0.866025403784439,
1.,0.866025403784439,1.,0.866025403784439,1.,0.866025403784439,1.,0.866025403784439,
1.,0.866025403784439,1.,0.866025403784439,1.,0.866025403784439,1.,0.866025403784439,
1.,0.866025403784439,1.,0.866025403784439,1.,0.866025403784439,1.,0.866025403784439,
1.,0.866025403784439,1.,0.866025403784439,1.,0.866025403784439,1.,0.866025403784439,
1.,0.866025403784439,1.,0.866025403784439,1.,0.866025403784439,1.,0.866025403784439,
1.,0.866025403784439,1.,0.866025403784439,1.,0.866025403784439,1.,0.866025403784439,
1.,0.866025403784439,1.,0.866025403784439,1.,0.866025403784439,1.,0.866025403784439,
1.,0.866025403784439,1.,0.866025403784439,1.,0.866025403784439,1.,0.866025403784439,
1.,0.866025403784439,1.,0.866025403784439,1.,0.866025403784439,1.,0.866025403784439,
1.,0.866025403784439,1.,0.866025403784439,1.,0.866025403784439,1.,0.866025403784439,
1.,0.866025403784439,1.,0.866025403784439,1.,0.866025403784439,1.,0.866025403784439,
1.,0.866025403784439,1.,0.866025403784439,1.,0.866025403784439,1.,0.866025403784439,
1.,0.866025403784439,1.,0.866025403784439,1.,0.866025403784439,1.,0.866025403784439,
1.,0.866025403784439,1.,0.866025403784439,1.,0.866025403784439,1.,0.866025403784439,
1.,0.866025403784439,1.,0.866025403784439,1.,0.866025403784439,1.,0.866025403784439,
1.,0.866025403784439,1.,0.866025403784439,1.,0.866025403784439,1.,0.866025403784439,
1.,0.866025403784439,1.,0.866025403784439,1.,0.866025403784439,1.,0.866025403784439,
1.,0.866025403784439,1.,0.866025403784439,1.,0.866025403784439,1.,0.866025403784439,
1.,0.866025403784439,1.,0.866025403784439,1.,0.866025403784439,1.,0.866025403784439,
1.,0.866025403784439,1.,0.866025403784439,1.,0.866025403784439,1.,0.866025403784439,
1.,0.866025403784439,1.,0.866025403784439,1.,0.866025403784439,1.,0.866025403784439,
1.,0.866025403784439,1.,0.866025403784439,1.,0.866025403784439,1.,0.866025403784439,
1.,0.866025403784439,1.,0.866025403784439,1.,0.866025403784439,1.,0.866025403784439,
1.,0.866025403784439,1.,0.866025403784439,1.,0.866025403784439,1.,0.866025403784439,
1.,0.866025403784439,1.,0.866025403784439,1.,0.866025403784439,1.,0.866025403784439,
1.,0.866025403784439,1.,0.866025403784439,1.,0.866025403784439,1.,0.866025403784439,
1.,0.866025403784439,1.,0.866025403784439,1.,0.866025403784439,1.,0.866025403784439,
1.,0.866025403784439,1.,0.866025403784439,1.,0.866025403784439,1.,0.866025403784439,
1.,0.866025403784439,1.,0.866025403784439,1.,0.866025403784439,1.,0.866025403784439,
1.,0.866025403784439,1.,0.866025403784439,1.,0.866025403784439,1.,0.866025403784439,
1.,0.866025403784439,1.,0.866025403784439,1.,0.866025403784439,1.,0.866025403784439,
1.,0.866025403784439,1.,0.866025403784439,1.,0.866025403784439,1.,0.866025403784439,
1.,0.866025403784439,1.,0.866025403784439,1.,0.866025403784439,1.,0.866025403784439,
1.,0.866025403784439,1.,0.866025403784439,1.,0.866025403784439,1.,0.866025403784439,
1.,0.866025403784439,1.,0.866025403784439,1.,0.866025403784439,1.,0.866025403784439,
1.,0.866025403784439,1.,0.866025403784439,1.,0.866025403784439,1.,0.866025403784439,
1.,0.866025403784439,1.,0.866025403784439,1.,0.866025403784439,1.)))
REPRESENTATION_ITEM('')
SURFACE()
);
#45=(
BOUNDED_SURFACE()
B_SPLINE_SURFACE(1,2,((#63743,#63744,#63745,#63746,#63747,#63748,#63749,
#63750,#63751,#63752,#63753,#63754,#63755,#63756,#63757,#63758,#63759,#63760,
#63761,#63762,#63763,#63764,#63765,#63766,#63767,#63768,#63769,#63770,#63771,
#63772,#63773,#63774,#63775,#63776,#63777,#63778,#63779,#63780,#63781,#63782,
#63783,#63784,#63785,#63786,#63787,#63788,#63789,#63790,#63791,#63792,#63793,
#63794,#63795,#63796,#63797,#63798,#63799,#63800,#63801,#63802,#63803,#63804,
#63805,#63806,#63807,#63808,#63809,#63810,#63811,#63812,#63813,#63814,#63815,
#63816,#63817,#63818,#63819,#63820,#63821,#63822,#63823,#63824,#63825,#63826,
#63827,#63828,#63829,#63830,#63831,#63832,#63833,#63834,#63835,#63836,#63837,
#63838,#63839,#63840,#63841,#63842,#63843,#63844,#63845,#63846,#63847,#63848,
#63849,#63850,#63851,#63852,#63853,#63854,#63855,#63856,#63857,#63858,#63859,
#63860,#63861,#63862,#63863,#63864,#63865,#63866,#63867,#63868,#63869,#63870,
#63871,#63872,#63873,#63874,#63875,#63876,#63877,#63878,#63879,#63880,#63881,
#63882,#63883,#63884,#63885,#63886,#63887,#63888,#63889,#63890,#63891,#63892,
#63893,#63894,#63895,#63896,#63897,#63898,#63899,#63900,#63901,#63902,#63903,
#63904,#63905,#63906,#63907,#63908,#63909,#63910,#63911,#63912,#63913,#63914,
#63915,#63916,#63917,#63918,#63919,#63920,#63921,#63922,#63923,#63924,#63925,
#63926,#63927,#63928,#63929,#63930,#63931,#63932,#63933,#63934,#63935,#63936,
#63937,#63938,#63939,#63940,#63941,#63942,#63943,#63944,#63945,#63946,#63947,
#63948,#63949,#63950,#63951,#63952,#63953,#63954,#63955,#63956,#63957,#63958,
#63959,#63960,#63961,#63962,#63963,#63964,#63965,#63966,#63967,#63968,#63969,
#63970,#63971,#63972,#63973,#63974,#63975,#63976,#63977,#63978,#63979,#63980,
#63981,#63982,#63983,#63984,#63985,#63986,#63987,#63988,#63989,#63990,#63991,
#63992,#63993,#63994,#63995,#63996,#63997,#63998,#63999,#64000,#64001,#64002,
#64003,#64004,#64005,#64006,#64007,#64008,#64009,#64010,#64011,#64012,#64013,
#64014,#64015,#64016,#64017,#64018,#64019,#64020,#64021,#64022,#64023,#64024,
#64025,#64026,#64027,#64028,#64029,#64030,#64031,#64032,#64033,#64034,#64035,
#64036,#64037,#64038,#64039,#64040,#64041,#64042,#64043,#64044,#64045,#64046,
#64047,#64048,#64049,#64050,#64051,#64052,#64053,#64054,#64055,#64056,#64057,
#64058,#64059,#64060,#64061,#64062,#64063,#64064,#64065,#64066,#64067,#64068,
#64069,#64070,#64071,#64072,#64073,#64074,#64075,#64076,#64077,#64078,#64079,
#64080,#64081,#64082,#64083,#64084,#64085,#64086,#64087,#64088,#64089,#64090,
#64091,#64092,#64093,#64094,#64095,#64096,#64097,#64098,#64099,#64100,#64101,
#64102,#64103,#64104,#64105,#64106,#64107,#64108,#64109,#64110,#64111,#64112,
#64113,#64114,#64115),(#64116,#64117,#64118,#64119,#64120,#64121,#64122,
#64123,#64124,#64125,#64126,#64127,#64128,#64129,#64130,#64131,#64132,#64133,
#64134,#64135,#64136,#64137,#64138,#64139,#64140,#64141,#64142,#64143,#64144,
#64145,#64146,#64147,#64148,#64149,#64150,#64151,#64152,#64153,#64154,#64155,
#64156,#64157,#64158,#64159,#64160,#64161,#64162,#64163,#64164,#64165,#64166,
#64167,#64168,#64169,#64170,#64171,#64172,#64173,#64174,#64175,#64176,#64177,
#64178,#64179,#64180,#64181,#64182,#64183,#64184,#64185,#64186,#64187,#64188,
#64189,#64190,#64191,#64192,#64193,#64194,#64195,#64196,#64197,#64198,#64199,
#64200,#64201,#64202,#64203,#64204,#64205,#64206,#64207,#64208,#64209,#64210,
#64211,#64212,#64213,#64214,#64215,#64216,#64217,#64218,#64219,#64220,#64221,
#64222,#64223,#64224,#64225,#64226,#64227,#64228,#64229,#64230,#64231,#64232,
#64233,#64234,#64235,#64236,#64237,#64238,#64239,#64240,#64241,#64242,#64243,
#64244,#64245,#64246,#64247,#64248,#64249,#64250,#64251,#64252,#64253,#64254,
#64255,#64256,#64257,#64258,#64259,#64260,#64261,#64262,#64263,#64264,#64265,
#64266,#64267,#64268,#64269,#64270,#64271,#64272,#64273,#64274,#64275,#64276,
#64277,#64278,#64279,#64280,#64281,#64282,#64283,#64284,#64285,#64286,#64287,
#64288,#64289,#64290,#64291,#64292,#64293,#64294,#64295,#64296,#64297,#64298,
#64299,#64300,#64301,#64302,#64303,#64304,#64305,#64306,#64307,#64308,#64309,
#64310,#64311,#64312,#64313,#64314,#64315,#64316,#64317,#64318,#64319,#64320,
#64321,#64322,#64323,#64324,#64325,#64326,#64327,#64328,#64329,#64330,#64331,
#64332,#64333,#64334,#64335,#64336,#64337,#64338,#64339,#64340,#64341,#64342,
#64343,#64344,#64345,#64346,#64347,#64348,#64349,#64350,#64351,#64352,#64353,
#64354,#64355,#64356,#64357,#64358,#64359,#64360,#64361,#64362,#64363,#64364,
#64365,#64366,#64367,#64368,#64369,#64370,#64371,#64372,#64373,#64374,#64375,
#64376,#64377,#64378,#64379,#64380,#64381,#64382,#64383,#64384,#64385,#64386,
#64387,#64388,#64389,#64390,#64391,#64392,#64393,#64394,#64395,#64396,#64397,
#64398,#64399,#64400,#64401,#64402,#64403,#64404,#64405,#64406,#64407,#64408,
#64409,#64410,#64411,#64412,#64413,#64414,#64415,#64416,#64417,#64418,#64419,
#64420,#64421,#64422,#64423,#64424,#64425,#64426,#64427,#64428,#64429,#64430,
#64431,#64432,#64433,#64434,#64435,#64436,#64437,#64438,#64439,#64440,#64441,
#64442,#64443,#64444,#64445,#64446,#64447,#64448,#64449,#64450,#64451,#64452,
#64453,#64454,#64455,#64456,#64457,#64458,#64459,#64460,#64461,#64462,#64463,
#64464,#64465,#64466,#64467,#64468,#64469,#64470,#64471,#64472,#64473,#64474,
#64475,#64476,#64477,#64478,#64479,#64480,#64481,#64482,#64483,#64484,#64485,
#64486,#64487,#64488)),.UNSPECIFIED.,.F.,.F.,.F.)
B_SPLINE_SURFACE_WITH_KNOTS((2,2),(3,2,2,2,2,2,2,2,2,2,2,2,2,2,2,2,2,2,
2,2,2,2,2,2,2,2,2,2,2,2,2,2,2,2,2,2,2,2,2,2,2,2,2,2,2,2,2,2,2,2,2,2,2,2,
2,2,2,2,2,2,2,2,2,2,2,2,2,2,2,2,2,2,2,2,2,2,2,2,2,2,2,2,2,2,2,2,2,2,2,2,
2,2,2,2,2,2,2,2,2,2,2,2,2,2,2,2,2,2,2,2,2,2,2,2,2,2,2,2,2,2,2,2,2,2,2,2,
2,2,2,2,2,2,2,2,2,2,2,2,2,2,2,2,2,2,2,2,2,2,2,2,2,2,2,2,2,2,2,2,2,2,2,2,
2,2,2,2,2,2,2,2,2,2,2,2,2,2,2,2,2,2,2,2,2,2,2,2,3),(-2.30253870309941E-5,
1.),(0.,0.00537634408602151,0.010752688172043,0.0161290322580645,0.021505376344086,
0.0268817204301075,0.032258064516129,0.0376344086021505,0.043010752688172,
0.0483870967741935,0.0537634408602151,0.0591397849462366,0.0645161290322581,
0.0698924731182796,0.0752688172043011,0.0806451612903226,0.0860215053763441,
0.0913978494623656,0.0967741935483871,0.102150537634409,0.10752688172043,
0.112903225806452,0.118279569892473,0.123655913978495,0.129032258064516,
0.134408602150538,0.139784946236559,0.145161290322581,0.150537634408602,
0.155913978494624,0.161290322580645,0.166666666666667,0.172043010752688,
0.17741935483871,0.182795698924731,0.188172043010753,0.193548387096774,
0.198924731182796,0.204301075268817,0.209677419354839,0.21505376344086,
0.220430107526882,0.225806451612903,0.231182795698925,0.236559139784946,
0.241935483870968,0.247311827956989,0.252688172043011,0.258064516129032,
0.263440860215054,0.268817204301075,0.274193548387097,0.279569892473118,
0.28494623655914,0.290322580645161,0.295698924731183,0.301075268817204,
0.306451612903226,0.311827956989247,0.317204301075269,0.32258064516129,
0.327956989247312,0.333333333333333,0.338709677419355,0.344086021505376,
0.349462365591398,0.354838709677419,0.360215053763441,0.365591397849462,
0.370967741935484,0.376344086021505,0.381720430107527,0.387096774193548,
0.39247311827957,0.397849462365591,0.403225806451613,0.408602150537634,
0.413978494623656,0.419354838709677,0.424731182795699,0.43010752688172,
0.435483870967742,0.440860215053763,0.446236559139785,0.451612903225806,
0.456989247311828,0.462365591397849,0.467741935483871,0.473118279569892,
0.478494623655914,0.483870967741935,0.489247311827957,0.494623655913978,
0.5,0.505376344086022,0.510752688172043,0.516129032258065,0.521505376344086,
0.526881720430108,0.532258064516129,0.537634408602151,0.543010752688172,
0.548387096774194,0.553763440860215,0.559139784946237,0.564516129032258,
0.56989247311828,0.575268817204301,0.580645161290323,0.586021505376344,
0.591397849462366,0.596774193548387,0.602150537634409,0.60752688172043,
0.612903225806452,0.618279569892473,0.623655913978495,0.629032258064516,
0.634408602150538,0.639784946236559,0.645161290322581,0.650537634408602,
0.655913978494624,0.661290322580645,0.666666666666667,0.672043010752688,
0.67741935483871,0.682795698924731,0.688172043010753,0.693548387096774,
0.698924731182796,0.704301075268817,0.709677419354839,0.71505376344086,
0.720430107526882,0.725806451612903,0.731182795698925,0.736559139784946,
0.741935483870968,0.747311827956989,0.752688172043011,0.758064516129032,
0.763440860215054,0.768817204301075,0.774193548387097,0.779569892473118,
0.78494623655914,0.790322580645161,0.795698924731183,0.801075268817204,
0.806451612903226,0.811827956989247,0.817204301075269,0.82258064516129,
0.827956989247312,0.833333333333333,0.838709677419355,0.844086021505376,
0.849462365591398,0.854838709677419,0.860215053763441,0.865591397849462,
0.870967741935484,0.876344086021505,0.881720430107527,0.887096774193548,
0.89247311827957,0.897849462365591,0.903225806451613,0.908602150537634,
0.913978494623656,0.919354838709677,0.924731182795699,0.93010752688172,
0.935483870967742,0.940860215053763,0.946236559139785,0.951612903225806,
0.956989247311828,0.962365591397849,0.967741935483871,0.973118279569892,
0.978494623655914,0.983870967741935,0.989247311827957,0.994623655913978,
1.),.UNSPECIFIED.)
GEOMETRIC_REPRESENTATION_ITEM()
RATIONAL_B_SPLINE_SURFACE(((1.,0.866025403784439,1.,0.866025403784439,1.,
0.866025403784439,1.,0.866025403784439,1.,0.866025403784439,1.,0.866025403784439,
1.,0.866025403784439,1.,0.866025403784439,1.,0.866025403784439,1.,0.866025403784439,
1.,0.866025403784439,1.,0.866025403784439,1.,0.866025403784439,1.,0.866025403784439,
1.,0.866025403784439,1.,0.866025403784439,1.,0.866025403784439,1.,0.866025403784439,
1.,0.866025403784439,1.,0.866025403784439,1.,0.866025403784439,1.,0.866025403784439,
1.,0.866025403784439,1.,0.866025403784439,1.,0.866025403784439,1.,0.866025403784439,
1.,0.866025403784439,1.,0.866025403784439,1.,0.866025403784439,1.,0.866025403784439,
1.,0.866025403784439,1.,0.866025403784439,1.,0.866025403784439,1.,0.866025403784439,
1.,0.866025403784439,1.,0.866025403784439,1.,0.866025403784439,1.,0.866025403784439,
1.,0.866025403784439,1.,0.866025403784439,1.,0.866025403784439,1.,0.866025403784439,
1.,0.866025403784439,1.,0.866025403784439,1.,0.866025403784439,1.,0.866025403784439,
1.,0.866025403784439,1.,0.866025403784439,1.,0.866025403784439,1.,0.866025403784439,
1.,0.866025403784439,1.,0.866025403784439,1.,0.866025403784439,1.,0.866025403784439,
1.,0.866025403784439,1.,0.866025403784439,1.,0.866025403784439,1.,0.866025403784439,
1.,0.866025403784439,1.,0.866025403784439,1.,0.866025403784439,1.,0.866025403784439,
1.,0.866025403784439,1.,0.866025403784439,1.,0.866025403784439,1.,0.866025403784439,
1.,0.866025403784439,1.,0.866025403784439,1.,0.866025403784439,1.,0.866025403784439,
1.,0.866025403784439,1.,0.866025403784439,1.,0.866025403784439,1.,0.866025403784439,
1.,0.866025403784439,1.,0.866025403784439,1.,0.866025403784439,1.,0.866025403784439,
1.,0.866025403784439,1.,0.866025403784439,1.,0.866025403784439,1.,0.866025403784439,
1.,0.866025403784439,1.,0.866025403784439,1.,0.866025403784439,1.,0.866025403784439,
1.,0.866025403784439,1.,0.866025403784439,1.,0.866025403784439,1.,0.866025403784439,
1.,0.866025403784439,1.,0.866025403784439,1.,0.866025403784439,1.,0.866025403784439,
1.,0.866025403784439,1.,0.866025403784439,1.,0.866025403784439,1.,0.866025403784439,
1.,0.866025403784439,1.,0.866025403784439,1.,0.866025403784439,1.,0.866025403784439,
1.,0.866025403784439,1.,0.866025403784439,1.,0.866025403784439,1.,0.866025403784439,
1.,0.866025403784439,1.,0.866025403784439,1.,0.866025403784439,1.,0.866025403784439,
1.,0.866025403784439,1.,0.866025403784439,1.,0.866025403784439,1.,0.866025403784439,
1.,0.866025403784439,1.,0.866025403784439,1.,0.866025403784439,1.,0.866025403784439,
1.,0.866025403784439,1.,0.866025403784439,1.,0.866025403784439,1.,0.866025403784439,
1.,0.866025403784439,1.,0.866025403784439,1.,0.866025403784439,1.,0.866025403784439,
1.,0.866025403784439,1.,0.866025403784439,1.,0.866025403784439,1.,0.866025403784439,
1.,0.866025403784439,1.,0.866025403784439,1.,0.866025403784439,1.,0.866025403784439,
1.,0.866025403784439,1.,0.866025403784439,1.,0.866025403784439,1.,0.866025403784439,
1.,0.866025403784439,1.,0.866025403784439,1.,0.866025403784439,1.,0.866025403784439,
1.,0.866025403784439,1.,0.866025403784439,1.,0.866025403784439,1.,0.866025403784439,
1.,0.866025403784439,1.,0.866025403784439,1.,0.866025403784439,1.,0.866025403784439,
1.,0.866025403784439,1.,0.866025403784439,1.,0.866025403784439,1.,0.866025403784439,
1.,0.866025403784439,1.,0.866025403784439,1.,0.866025403784439,1.,0.866025403784439,
1.,0.866025403784439,1.,0.866025403784439,1.,0.866025403784439,1.,0.866025403784439,
1.,0.866025403784439,1.,0.866025403784439,1.,0.866025403784439,1.,0.866025403784439,
1.,0.866025403784439,1.,0.866025403784439,1.,0.866025403784439,1.,0.866025403784439,
1.,0.866025403784439,1.,0.866025403784439,1.,0.866025403784439,1.,0.866025403784439,
1.,0.866025403784439,1.,0.866025403784439,1.,0.866025403784439,1.,0.866025403784439,
1.,0.866025403784439,1.,0.866025403784439,1.,0.866025403784439,1.,0.866025403784439,
1.,0.866025403784439,1.,0.866025403784439,1.,0.866025403784439,1.,0.866025403784439,
1.),(1.,0.866025403784439,1.,0.866025403784439,1.,0.866025403784439,1.,
0.866025403784439,1.,0.866025403784439,1.,0.866025403784439,1.,0.866025403784439,
1.,0.866025403784439,1.,0.866025403784439,1.,0.866025403784439,1.,0.866025403784439,
1.,0.866025403784439,1.,0.866025403784439,1.,0.866025403784439,1.,0.866025403784439,
1.,0.866025403784439,1.,0.866025403784439,1.,0.866025403784439,1.,0.866025403784439,
1.,0.866025403784439,1.,0.866025403784439,1.,0.866025403784439,1.,0.866025403784439,
1.,0.866025403784439,1.,0.866025403784439,1.,0.866025403784439,1.,0.866025403784439,
1.,0.866025403784439,1.,0.866025403784439,1.,0.866025403784439,1.,0.866025403784439,
1.,0.866025403784439,1.,0.866025403784439,1.,0.866025403784439,1.,0.866025403784439,
1.,0.866025403784439,1.,0.866025403784439,1.,0.866025403784439,1.,0.866025403784439,
1.,0.866025403784439,1.,0.866025403784439,1.,0.866025403784439,1.,0.866025403784439,
1.,0.866025403784439,1.,0.866025403784439,1.,0.866025403784439,1.,0.866025403784439,
1.,0.866025403784439,1.,0.866025403784439,1.,0.866025403784439,1.,0.866025403784439,
1.,0.866025403784439,1.,0.866025403784439,1.,0.866025403784439,1.,0.866025403784439,
1.,0.866025403784439,1.,0.866025403784439,1.,0.866025403784439,1.,0.866025403784439,
1.,0.866025403784439,1.,0.866025403784439,1.,0.866025403784439,1.,0.866025403784439,
1.,0.866025403784439,1.,0.866025403784439,1.,0.866025403784439,1.,0.866025403784439,
1.,0.866025403784439,1.,0.866025403784439,1.,0.866025403784439,1.,0.866025403784439,
1.,0.866025403784439,1.,0.866025403784439,1.,0.866025403784439,1.,0.866025403784439,
1.,0.866025403784439,1.,0.866025403784439,1.,0.866025403784439,1.,0.866025403784439,
1.,0.866025403784439,1.,0.866025403784439,1.,0.866025403784439,1.,0.866025403784439,
1.,0.866025403784439,1.,0.866025403784439,1.,0.866025403784439,1.,0.866025403784439,
1.,0.866025403784439,1.,0.866025403784439,1.,0.866025403784439,1.,0.866025403784439,
1.,0.866025403784439,1.,0.866025403784439,1.,0.866025403784439,1.,0.866025403784439,
1.,0.866025403784439,1.,0.866025403784439,1.,0.866025403784439,1.,0.866025403784439,
1.,0.866025403784439,1.,0.866025403784439,1.,0.866025403784439,1.,0.866025403784439,
1.,0.866025403784439,1.,0.866025403784439,1.,0.866025403784439,1.,0.866025403784439,
1.,0.866025403784439,1.,0.866025403784439,1.,0.866025403784439,1.,0.866025403784439,
1.,0.866025403784439,1.,0.866025403784439,1.,0.866025403784439,1.,0.866025403784439,
1.,0.866025403784439,1.,0.866025403784439,1.,0.866025403784439,1.,0.866025403784439,
1.,0.866025403784439,1.,0.866025403784439,1.,0.866025403784439,1.,0.866025403784439,
1.,0.866025403784439,1.,0.866025403784439,1.,0.866025403784439,1.,0.866025403784439,
1.,0.866025403784439,1.,0.866025403784439,1.,0.866025403784439,1.,0.866025403784439,
1.,0.866025403784439,1.,0.866025403784439,1.,0.866025403784439,1.,0.866025403784439,
1.,0.866025403784439,1.,0.866025403784439,1.,0.866025403784439,1.,0.866025403784439,
1.,0.866025403784439,1.,0.866025403784439,1.,0.866025403784439,1.,0.866025403784439,
1.,0.866025403784439,1.,0.866025403784439,1.,0.866025403784439,1.,0.866025403784439,
1.,0.866025403784439,1.,0.866025403784439,1.,0.866025403784439,1.,0.866025403784439,
1.,0.866025403784439,1.,0.866025403784439,1.,0.866025403784439,1.,0.866025403784439,
1.,0.866025403784439,1.,0.866025403784439,1.,0.866025403784439,1.,0.866025403784439,
1.,0.866025403784439,1.,0.866025403784439,1.,0.866025403784439,1.,0.866025403784439,
1.,0.866025403784439,1.,0.866025403784439,1.,0.866025403784439,1.,0.866025403784439,
1.,0.866025403784439,1.,0.866025403784439,1.,0.866025403784439,1.,0.866025403784439,
1.,0.866025403784439,1.,0.866025403784439,1.,0.866025403784439,1.,0.866025403784439,
1.,0.866025403784439,1.,0.866025403784439,1.,0.866025403784439,1.,0.866025403784439,
1.,0.866025403784439,1.,0.866025403784439,1.,0.866025403784439,1.,0.866025403784439,
1.,0.866025403784439,1.,0.866025403784439,1.,0.866025403784439,1.)))
REPRESENTATION_ITEM('')
SURFACE()
);
#46=(
BOUNDED_SURFACE()
B_SPLINE_SURFACE(1,2,((#64517,#64518,#64519,#64520,#64521,#64522,#64523,
#64524,#64525,#64526,#64527,#64528,#64529,#64530,#64531,#64532,#64533,#64534,
#64535,#64536,#64537,#64538,#64539,#64540,#64541,#64542,#64543,#64544,#64545,
#64546,#64547,#64548,#64549,#64550,#64551,#64552,#64553,#64554,#64555,#64556,
#64557,#64558,#64559,#64560,#64561,#64562,#64563,#64564,#64565,#64566,#64567,
#64568,#64569,#64570,#64571,#64572,#64573,#64574,#64575,#64576,#64577,#64578,
#64579,#64580,#64581,#64582,#64583,#64584,#64585,#64586,#64587,#64588,#64589,
#64590,#64591,#64592,#64593,#64594,#64595,#64596,#64597,#64598,#64599,#64600,
#64601,#64602,#64603,#64604,#64605,#64606,#64607,#64608,#64609,#64610,#64611,
#64612,#64613,#64614,#64615,#64616,#64617,#64618,#64619,#64620,#64621,#64622,
#64623,#64624,#64625,#64626,#64627,#64628,#64629,#64630,#64631,#64632,#64633,
#64634,#64635,#64636,#64637,#64638,#64639,#64640,#64641,#64642,#64643,#64644,
#64645,#64646,#64647,#64648,#64649,#64650,#64651,#64652,#64653,#64654,#64655,
#64656,#64657,#64658,#64659,#64660,#64661,#64662,#64663,#64664,#64665,#64666,
#64667,#64668,#64669,#64670,#64671,#64672,#64673,#64674,#64675,#64676,#64677,
#64678,#64679,#64680,#64681,#64682,#64683,#64684,#64685,#64686,#64687,#64688,
#64689,#64690,#64691,#64692,#64693,#64694,#64695,#64696,#64697,#64698,#64699,
#64700,#64701,#64702,#64703,#64704,#64705,#64706,#64707,#64708,#64709,#64710,
#64711,#64712,#64713,#64714,#64715,#64716,#64717,#64718,#64719,#64720,#64721,
#64722,#64723,#64724,#64725,#64726,#64727,#64728,#64729,#64730,#64731,#64732,
#64733,#64734,#64735,#64736,#64737,#64738,#64739,#64740,#64741,#64742,#64743,
#64744,#64745,#64746,#64747,#64748,#64749,#64750,#64751,#64752,#64753,#64754,
#64755,#64756,#64757,#64758,#64759,#64760,#64761,#64762,#64763,#64764,#64765,
#64766,#64767,#64768,#64769,#64770,#64771,#64772,#64773,#64774,#64775,#64776,
#64777,#64778,#64779,#64780,#64781,#64782,#64783,#64784,#64785,#64786,#64787,
#64788,#64789,#64790,#64791,#64792,#64793,#64794,#64795,#64796,#64797,#64798,
#64799,#64800,#64801,#64802,#64803,#64804,#64805,#64806,#64807,#64808,#64809,
#64810,#64811,#64812,#64813,#64814,#64815,#64816,#64817,#64818,#64819,#64820,
#64821,#64822,#64823,#64824,#64825,#64826,#64827,#64828,#64829,#64830,#64831,
#64832,#64833,#64834,#64835,#64836,#64837,#64838,#64839,#64840,#64841,#64842,
#64843,#64844,#64845,#64846,#64847,#64848,#64849,#64850,#64851,#64852,#64853,
#64854,#64855,#64856,#64857,#64858,#64859,#64860,#64861,#64862,#64863,#64864,
#64865,#64866,#64867,#64868,#64869,#64870,#64871,#64872,#64873,#64874,#64875,
#64876,#64877,#64878,#64879,#64880,#64881,#64882,#64883,#64884,#64885,#64886,
#64887,#64888,#64889),(#64890,#64891,#64892,#64893,#64894,#64895,#64896,
#64897,#64898,#64899,#64900,#64901,#64902,#64903,#64904,#64905,#64906,#64907,
#64908,#64909,#64910,#64911,#64912,#64913,#64914,#64915,#64916,#64917,#64918,
#64919,#64920,#64921,#64922,#64923,#64924,#64925,#64926,#64927,#64928,#64929,
#64930,#64931,#64932,#64933,#64934,#64935,#64936,#64937,#64938,#64939,#64940,
#64941,#64942,#64943,#64944,#64945,#64946,#64947,#64948,#64949,#64950,#64951,
#64952,#64953,#64954,#64955,#64956,#64957,#64958,#64959,#64960,#64961,#64962,
#64963,#64964,#64965,#64966,#64967,#64968,#64969,#64970,#64971,#64972,#64973,
#64974,#64975,#64976,#64977,#64978,#64979,#64980,#64981,#64982,#64983,#64984,
#64985,#64986,#64987,#64988,#64989,#64990,#64991,#64992,#64993,#64994,#64995,
#64996,#64997,#64998,#64999,#65000,#65001,#65002,#65003,#65004,#65005,#65006,
#65007,#65008,#65009,#65010,#65011,#65012,#65013,#65014,#65015,#65016,#65017,
#65018,#65019,#65020,#65021,#65022,#65023,#65024,#65025,#65026,#65027,#65028,
#65029,#65030,#65031,#65032,#65033,#65034,#65035,#65036,#65037,#65038,#65039,
#65040,#65041,#65042,#65043,#65044,#65045,#65046,#65047,#65048,#65049,#65050,
#65051,#65052,#65053,#65054,#65055,#65056,#65057,#65058,#65059,#65060,#65061,
#65062,#65063,#65064,#65065,#65066,#65067,#65068,#65069,#65070,#65071,#65072,
#65073,#65074,#65075,#65076,#65077,#65078,#65079,#65080,#65081,#65082,#65083,
#65084,#65085,#65086,#65087,#65088,#65089,#65090,#65091,#65092,#65093,#65094,
#65095,#65096,#65097,#65098,#65099,#65100,#65101,#65102,#65103,#65104,#65105,
#65106,#65107,#65108,#65109,#65110,#65111,#65112,#65113,#65114,#65115,#65116,
#65117,#65118,#65119,#65120,#65121,#65122,#65123,#65124,#65125,#65126,#65127,
#65128,#65129,#65130,#65131,#65132,#65133,#65134,#65135,#65136,#65137,#65138,
#65139,#65140,#65141,#65142,#65143,#65144,#65145,#65146,#65147,#65148,#65149,
#65150,#65151,#65152,#65153,#65154,#65155,#65156,#65157,#65158,#65159,#65160,
#65161,#65162,#65163,#65164,#65165,#65166,#65167,#65168,#65169,#65170,#65171,
#65172,#65173,#65174,#65175,#65176,#65177,#65178,#65179,#65180,#65181,#65182,
#65183,#65184,#65185,#65186,#65187,#65188,#65189,#65190,#65191,#65192,#65193,
#65194,#65195,#65196,#65197,#65198,#65199,#65200,#65201,#65202,#65203,#65204,
#65205,#65206,#65207,#65208,#65209,#65210,#65211,#65212,#65213,#65214,#65215,
#65216,#65217,#65218,#65219,#65220,#65221,#65222,#65223,#65224,#65225,#65226,
#65227,#65228,#65229,#65230,#65231,#65232,#65233,#65234,#65235,#65236,#65237,
#65238,#65239,#65240,#65241,#65242,#65243,#65244,#65245,#65246,#65247,#65248,
#65249,#65250,#65251,#65252,#65253,#65254,#65255,#65256,#65257,#65258,#65259,
#65260,#65261,#65262)),.UNSPECIFIED.,.F.,.F.,.F.)
B_SPLINE_SURFACE_WITH_KNOTS((2,2),(3,2,2,2,2,2,2,2,2,2,2,2,2,2,2,2,2,2,
2,2,2,2,2,2,2,2,2,2,2,2,2,2,2,2,2,2,2,2,2,2,2,2,2,2,2,2,2,2,2,2,2,2,2,2,
2,2,2,2,2,2,2,2,2,2,2,2,2,2,2,2,2,2,2,2,2,2,2,2,2,2,2,2,2,2,2,2,2,2,2,2,
2,2,2,2,2,2,2,2,2,2,2,2,2,2,2,2,2,2,2,2,2,2,2,2,2,2,2,2,2,2,2,2,2,2,2,2,
2,2,2,2,2,2,2,2,2,2,2,2,2,2,2,2,2,2,2,2,2,2,2,2,2,2,2,2,2,2,2,2,2,2,2,2,
2,2,2,2,2,2,2,2,2,2,2,2,2,2,2,2,2,2,2,2,2,2,2,2,3),(0.,1.00001535537392),
(0.,0.00537634408602151,0.010752688172043,0.0161290322580645,0.021505376344086,
0.0268817204301075,0.032258064516129,0.0376344086021505,0.043010752688172,
0.0483870967741935,0.0537634408602151,0.0591397849462366,0.0645161290322581,
0.0698924731182796,0.0752688172043011,0.0806451612903226,0.0860215053763441,
0.0913978494623656,0.0967741935483871,0.102150537634409,0.10752688172043,
0.112903225806452,0.118279569892473,0.123655913978495,0.129032258064516,
0.134408602150538,0.139784946236559,0.145161290322581,0.150537634408602,
0.155913978494624,0.161290322580645,0.166666666666667,0.172043010752688,
0.17741935483871,0.182795698924731,0.188172043010753,0.193548387096774,
0.198924731182796,0.204301075268817,0.209677419354839,0.21505376344086,
0.220430107526882,0.225806451612903,0.231182795698925,0.236559139784946,
0.241935483870968,0.247311827956989,0.252688172043011,0.258064516129032,
0.263440860215054,0.268817204301075,0.274193548387097,0.279569892473118,
0.28494623655914,0.290322580645161,0.295698924731183,0.301075268817204,
0.306451612903226,0.311827956989247,0.317204301075269,0.32258064516129,
0.327956989247312,0.333333333333333,0.338709677419355,0.344086021505376,
0.349462365591398,0.354838709677419,0.360215053763441,0.365591397849462,
0.370967741935484,0.376344086021505,0.381720430107527,0.387096774193548,
0.39247311827957,0.397849462365591,0.403225806451613,0.408602150537634,
0.413978494623656,0.419354838709677,0.424731182795699,0.43010752688172,
0.435483870967742,0.440860215053763,0.446236559139785,0.451612903225806,
0.456989247311828,0.462365591397849,0.467741935483871,0.473118279569892,
0.478494623655914,0.483870967741935,0.489247311827957,0.494623655913978,
0.5,0.505376344086022,0.510752688172043,0.516129032258065,0.521505376344086,
0.526881720430108,0.532258064516129,0.537634408602151,0.543010752688172,
0.548387096774194,0.553763440860215,0.559139784946237,0.564516129032258,
0.56989247311828,0.575268817204301,0.580645161290323,0.586021505376344,
0.591397849462366,0.596774193548387,0.602150537634409,0.60752688172043,
0.612903225806452,0.618279569892473,0.623655913978495,0.629032258064516,
0.634408602150538,0.639784946236559,0.645161290322581,0.650537634408602,
0.655913978494624,0.661290322580645,0.666666666666667,0.672043010752688,
0.67741935483871,0.682795698924731,0.688172043010753,0.693548387096774,
0.698924731182796,0.704301075268817,0.709677419354839,0.71505376344086,
0.720430107526882,0.725806451612903,0.731182795698925,0.736559139784946,
0.741935483870968,0.747311827956989,0.752688172043011,0.758064516129032,
0.763440860215054,0.768817204301075,0.774193548387097,0.779569892473118,
0.78494623655914,0.790322580645161,0.795698924731183,0.801075268817204,
0.806451612903226,0.811827956989247,0.817204301075269,0.82258064516129,
0.827956989247312,0.833333333333333,0.838709677419355,0.844086021505376,
0.849462365591398,0.854838709677419,0.860215053763441,0.865591397849462,
0.870967741935484,0.876344086021505,0.881720430107527,0.887096774193548,
0.89247311827957,0.897849462365591,0.903225806451613,0.908602150537634,
0.913978494623656,0.919354838709677,0.924731182795699,0.93010752688172,
0.935483870967742,0.940860215053763,0.946236559139785,0.951612903225806,
0.956989247311828,0.962365591397849,0.967741935483871,0.973118279569892,
0.978494623655914,0.983870967741935,0.989247311827957,0.994623655913978,
1.),.UNSPECIFIED.)
GEOMETRIC_REPRESENTATION_ITEM()
RATIONAL_B_SPLINE_SURFACE(((1.,0.866025403784439,1.,0.866025403784439,1.,
0.866025403784439,1.,0.866025403784439,1.,0.866025403784439,1.,0.866025403784439,
1.,0.866025403784439,1.,0.866025403784439,1.,0.866025403784439,1.,0.866025403784439,
1.,0.866025403784439,1.,0.866025403784439,1.,0.866025403784439,1.,0.866025403784439,
1.,0.866025403784439,1.,0.866025403784439,1.,0.866025403784439,1.,0.866025403784439,
1.,0.866025403784439,1.,0.866025403784439,1.,0.866025403784439,1.,0.866025403784439,
1.,0.866025403784439,1.,0.866025403784439,1.,0.866025403784439,1.,0.866025403784439,
1.,0.866025403784439,1.,0.866025403784439,1.,0.866025403784439,1.,0.866025403784439,
1.,0.866025403784439,1.,0.866025403784439,1.,0.866025403784439,1.,0.866025403784439,
1.,0.866025403784439,1.,0.866025403784439,1.,0.866025403784439,1.,0.866025403784439,
1.,0.866025403784439,1.,0.866025403784439,1.,0.866025403784439,1.,0.866025403784439,
1.,0.866025403784439,1.,0.866025403784439,1.,0.866025403784439,1.,0.866025403784439,
1.,0.866025403784439,1.,0.866025403784439,1.,0.866025403784439,1.,0.866025403784439,
1.,0.866025403784439,1.,0.866025403784439,1.,0.866025403784439,1.,0.866025403784439,
1.,0.866025403784439,1.,0.866025403784439,1.,0.866025403784439,1.,0.866025403784439,
1.,0.866025403784439,1.,0.866025403784439,1.,0.866025403784439,1.,0.866025403784439,
1.,0.866025403784439,1.,0.866025403784439,1.,0.866025403784439,1.,0.866025403784439,
1.,0.866025403784439,1.,0.866025403784439,1.,0.866025403784439,1.,0.866025403784439,
1.,0.866025403784439,1.,0.866025403784439,1.,0.866025403784439,1.,0.866025403784439,
1.,0.866025403784439,1.,0.866025403784439,1.,0.866025403784439,1.,0.866025403784439,
1.,0.866025403784439,1.,0.866025403784439,1.,0.866025403784439,1.,0.866025403784439,
1.,0.866025403784439,1.,0.866025403784439,1.,0.866025403784439,1.,0.866025403784439,
1.,0.866025403784439,1.,0.866025403784439,1.,0.866025403784439,1.,0.866025403784439,
1.,0.866025403784439,1.,0.866025403784439,1.,0.866025403784439,1.,0.866025403784439,
1.,0.866025403784439,1.,0.866025403784439,1.,0.866025403784439,1.,0.866025403784439,
1.,0.866025403784439,1.,0.866025403784439,1.,0.866025403784439,1.,0.866025403784439,
1.,0.866025403784439,1.,0.866025403784439,1.,0.866025403784439,1.,0.866025403784439,
1.,0.866025403784439,1.,0.866025403784439,1.,0.866025403784439,1.,0.866025403784439,
1.,0.866025403784439,1.,0.866025403784439,1.,0.866025403784439,1.,0.866025403784439,
1.,0.866025403784439,1.,0.866025403784439,1.,0.866025403784439,1.,0.866025403784439,
1.,0.866025403784439,1.,0.866025403784439,1.,0.866025403784439,1.,0.866025403784439,
1.,0.866025403784439,1.,0.866025403784439,1.,0.866025403784439,1.,0.866025403784439,
1.,0.866025403784439,1.,0.866025403784439,1.,0.866025403784439,1.,0.866025403784439,
1.,0.866025403784439,1.,0.866025403784439,1.,0.866025403784439,1.,0.866025403784439,
1.,0.866025403784439,1.,0.866025403784439,1.,0.866025403784439,1.,0.866025403784439,
1.,0.866025403784439,1.,0.866025403784439,1.,0.866025403784439,1.,0.866025403784439,
1.,0.866025403784439,1.,0.866025403784439,1.,0.866025403784439,1.,0.866025403784439,
1.,0.866025403784439,1.,0.866025403784439,1.,0.866025403784439,1.,0.866025403784439,
1.,0.866025403784439,1.,0.866025403784439,1.,0.866025403784439,1.,0.866025403784439,
1.,0.866025403784439,1.,0.866025403784439,1.,0.866025403784439,1.,0.866025403784439,
1.,0.866025403784439,1.,0.866025403784439,1.,0.866025403784439,1.,0.866025403784439,
1.,0.866025403784439,1.,0.866025403784439,1.,0.866025403784439,1.,0.866025403784439,
1.,0.866025403784439,1.,0.866025403784439,1.,0.866025403784439,1.,0.866025403784439,
1.,0.866025403784439,1.,0.866025403784439,1.,0.866025403784439,1.,0.866025403784439,
1.,0.866025403784439,1.,0.866025403784439,1.,0.866025403784439,1.,0.866025403784439,
1.,0.866025403784439,1.,0.866025403784439,1.,0.866025403784439,1.,0.866025403784439,
1.,0.866025403784439,1.,0.866025403784439,1.,0.866025403784439,1.,0.866025403784439,
1.),(1.,0.866025403784439,1.,0.866025403784439,1.,0.866025403784439,1.,
0.866025403784439,1.,0.866025403784439,1.,0.866025403784439,1.,0.866025403784439,
1.,0.866025403784439,1.,0.866025403784439,1.,0.866025403784439,1.,0.866025403784439,
1.,0.866025403784439,1.,0.866025403784439,1.,0.866025403784439,1.,0.866025403784439,
1.,0.866025403784439,1.,0.866025403784439,1.,0.866025403784439,1.,0.866025403784439,
1.,0.866025403784439,1.,0.866025403784439,1.,0.866025403784439,1.,0.866025403784439,
1.,0.866025403784439,1.,0.866025403784439,1.,0.866025403784439,1.,0.866025403784439,
1.,0.866025403784439,1.,0.866025403784439,1.,0.866025403784439,1.,0.866025403784439,
1.,0.866025403784439,1.,0.866025403784439,1.,0.866025403784439,1.,0.866025403784439,
1.,0.866025403784439,1.,0.866025403784439,1.,0.866025403784439,1.,0.866025403784439,
1.,0.866025403784439,1.,0.866025403784439,1.,0.866025403784439,1.,0.866025403784439,
1.,0.866025403784439,1.,0.866025403784439,1.,0.866025403784439,1.,0.866025403784439,
1.,0.866025403784439,1.,0.866025403784439,1.,0.866025403784439,1.,0.866025403784439,
1.,0.866025403784439,1.,0.866025403784439,1.,0.866025403784439,1.,0.866025403784439,
1.,0.866025403784439,1.,0.866025403784439,1.,0.866025403784439,1.,0.866025403784439,
1.,0.866025403784439,1.,0.866025403784439,1.,0.866025403784439,1.,0.866025403784439,
1.,0.866025403784439,1.,0.866025403784439,1.,0.866025403784439,1.,0.866025403784439,
1.,0.866025403784439,1.,0.866025403784439,1.,0.866025403784439,1.,0.866025403784439,
1.,0.866025403784439,1.,0.866025403784439,1.,0.866025403784439,1.,0.866025403784439,
1.,0.866025403784439,1.,0.866025403784439,1.,0.866025403784439,1.,0.866025403784439,
1.,0.866025403784439,1.,0.866025403784439,1.,0.866025403784439,1.,0.866025403784439,
1.,0.866025403784439,1.,0.866025403784439,1.,0.866025403784439,1.,0.866025403784439,
1.,0.866025403784439,1.,0.866025403784439,1.,0.866025403784439,1.,0.866025403784439,
1.,0.866025403784439,1.,0.866025403784439,1.,0.866025403784439,1.,0.866025403784439,
1.,0.866025403784439,1.,0.866025403784439,1.,0.866025403784439,1.,0.866025403784439,
1.,0.866025403784439,1.,0.866025403784439,1.,0.866025403784439,1.,0.866025403784439,
1.,0.866025403784439,1.,0.866025403784439,1.,0.866025403784439,1.,0.866025403784439,
1.,0.866025403784439,1.,0.866025403784439,1.,0.866025403784439,1.,0.866025403784439,
1.,0.866025403784439,1.,0.866025403784439,1.,0.866025403784439,1.,0.866025403784439,
1.,0.866025403784439,1.,0.866025403784439,1.,0.866025403784439,1.,0.866025403784439,
1.,0.866025403784439,1.,0.866025403784439,1.,0.866025403784439,1.,0.866025403784439,
1.,0.866025403784439,1.,0.866025403784439,1.,0.866025403784439,1.,0.866025403784439,
1.,0.866025403784439,1.,0.866025403784439,1.,0.866025403784439,1.,0.866025403784439,
1.,0.866025403784439,1.,0.866025403784439,1.,0.866025403784439,1.,0.866025403784439,
1.,0.866025403784439,1.,0.866025403784439,1.,0.866025403784439,1.,0.866025403784439,
1.,0.866025403784439,1.,0.866025403784439,1.,0.866025403784439,1.,0.866025403784439,
1.,0.866025403784439,1.,0.866025403784439,1.,0.866025403784439,1.,0.866025403784439,
1.,0.866025403784439,1.,0.866025403784439,1.,0.866025403784439,1.,0.866025403784439,
1.,0.866025403784439,1.,0.866025403784439,1.,0.866025403784439,1.,0.866025403784439,
1.,0.866025403784439,1.,0.866025403784439,1.,0.866025403784439,1.,0.866025403784439,
1.,0.866025403784439,1.,0.866025403784439,1.,0.866025403784439,1.,0.866025403784439,
1.,0.866025403784439,1.,0.866025403784439,1.,0.866025403784439,1.,0.866025403784439,
1.,0.866025403784439,1.,0.866025403784439,1.,0.866025403784439,1.,0.866025403784439,
1.,0.866025403784439,1.,0.866025403784439,1.,0.866025403784439,1.,0.866025403784439,
1.,0.866025403784439,1.,0.866025403784439,1.,0.866025403784439,1.,0.866025403784439,
1.,0.866025403784439,1.,0.866025403784439,1.,0.866025403784439,1.,0.866025403784439,
1.,0.866025403784439,1.,0.866025403784439,1.,0.866025403784439,1.)))
REPRESENTATION_ITEM('')
SURFACE()
);
#47=(
BOUNDED_SURFACE()
B_SPLINE_SURFACE(1,2,((#73432,#73433,#73434,#73435,#73436,#73437,#73438,
#73439,#73440,#73441,#73442,#73443,#73444,#73445,#73446,#73447,#73448,#73449,
#73450,#73451,#73452,#73453,#73454,#73455,#73456,#73457,#73458,#73459,#73460,
#73461,#73462,#73463,#73464,#73465,#73466,#73467,#73468,#73469,#73470,#73471,
#73472,#73473,#73474,#73475,#73476,#73477,#73478,#73479,#73480,#73481,#73482,
#73483,#73484,#73485,#73486,#73487,#73488,#73489,#73490,#73491,#73492,#73493,
#73494,#73495,#73496,#73497,#73498,#73499,#73500,#73501,#73502,#73503,#73504,
#73505,#73506,#73507,#73508,#73509,#73510,#73511,#73512,#73513,#73514,#73515,
#73516,#73517,#73518,#73519,#73520,#73521,#73522,#73523,#73524,#73525,#73526,
#73527,#73528,#73529,#73530,#73531,#73532,#73533,#73534,#73535,#73536,#73537,
#73538,#73539,#73540,#73541,#73542,#73543,#73544,#73545,#73546,#73547,#73548,
#73549,#73550,#73551,#73552,#73553,#73554,#73555,#73556,#73557,#73558,#73559,
#73560,#73561,#73562,#73563,#73564,#73565,#73566,#73567,#73568,#73569,#73570,
#73571,#73572,#73573,#73574,#73575,#73576,#73577,#73578,#73579,#73580,#73581,
#73582,#73583,#73584,#73585,#73586,#73587,#73588,#73589,#73590,#73591,#73592,
#73593,#73594,#73595,#73596,#73597,#73598,#73599,#73600,#73601,#73602,#73603,
#73604,#73605,#73606,#73607,#73608,#73609,#73610,#73611,#73612,#73613,#73614,
#73615,#73616,#73617,#73618,#73619,#73620,#73621,#73622,#73623,#73624,#73625,
#73626,#73627,#73628,#73629,#73630,#73631,#73632,#73633,#73634,#73635,#73636,
#73637,#73638,#73639,#73640,#73641,#73642,#73643,#73644,#73645,#73646,#73647,
#73648,#73649,#73650,#73651,#73652,#73653,#73654,#73655,#73656,#73657,#73658,
#73659,#73660,#73661,#73662,#73663,#73664,#73665,#73666,#73667,#73668,#73669,
#73670,#73671,#73672,#73673,#73674,#73675,#73676,#73677,#73678,#73679,#73680,
#73681,#73682,#73683,#73684,#73685,#73686,#73687,#73688,#73689,#73690,#73691,
#73692,#73693,#73694,#73695,#73696,#73697,#73698,#73699,#73700,#73701,#73702,
#73703,#73704,#73705,#73706,#73707,#73708,#73709,#73710,#73711,#73712,#73713,
#73714,#73715,#73716,#73717,#73718,#73719,#73720,#73721,#73722,#73723,#73724,
#73725,#73726,#73727,#73728,#73729,#73730,#73731,#73732,#73733,#73734,#73735,
#73736,#73737,#73738,#73739,#73740,#73741,#73742,#73743,#73744,#73745,#73746,
#73747,#73748,#73749,#73750,#73751,#73752,#73753,#73754,#73755,#73756,#73757,
#73758,#73759,#73760,#73761,#73762,#73763,#73764,#73765,#73766,#73767,#73768,
#73769,#73770,#73771,#73772,#73773,#73774,#73775,#73776,#73777,#73778,#73779,
#73780,#73781,#73782,#73783,#73784,#73785,#73786,#73787,#73788,#73789,#73790,
#73791,#73792,#73793,#73794,#73795,#73796,#73797,#73798,#73799,#73800,#73801,
#73802,#73803,#73804),(#73805,#73806,#73807,#73808,#73809,#73810,#73811,
#73812,#73813,#73814,#73815,#73816,#73817,#73818,#73819,#73820,#73821,#73822,
#73823,#73824,#73825,#73826,#73827,#73828,#73829,#73830,#73831,#73832,#73833,
#73834,#73835,#73836,#73837,#73838,#73839,#73840,#73841,#73842,#73843,#73844,
#73845,#73846,#73847,#73848,#73849,#73850,#73851,#73852,#73853,#73854,#73855,
#73856,#73857,#73858,#73859,#73860,#73861,#73862,#73863,#73864,#73865,#73866,
#73867,#73868,#73869,#73870,#73871,#73872,#73873,#73874,#73875,#73876,#73877,
#73878,#73879,#73880,#73881,#73882,#73883,#73884,#73885,#73886,#73887,#73888,
#73889,#73890,#73891,#73892,#73893,#73894,#73895,#73896,#73897,#73898,#73899,
#73900,#73901,#73902,#73903,#73904,#73905,#73906,#73907,#73908,#73909,#73910,
#73911,#73912,#73913,#73914,#73915,#73916,#73917,#73918,#73919,#73920,#73921,
#73922,#73923,#73924,#73925,#73926,#73927,#73928,#73929,#73930,#73931,#73932,
#73933,#73934,#73935,#73936,#73937,#73938,#73939,#73940,#73941,#73942,#73943,
#73944,#73945,#73946,#73947,#73948,#73949,#73950,#73951,#73952,#73953,#73954,
#73955,#73956,#73957,#73958,#73959,#73960,#73961,#73962,#73963,#73964,#73965,
#73966,#73967,#73968,#73969,#73970,#73971,#73972,#73973,#73974,#73975,#73976,
#73977,#73978,#73979,#73980,#73981,#73982,#73983,#73984,#73985,#73986,#73987,
#73988,#73989,#73990,#73991,#73992,#73993,#73994,#73995,#73996,#73997,#73998,
#73999,#74000,#74001,#74002,#74003,#74004,#74005,#74006,#74007,#74008,#74009,
#74010,#74011,#74012,#74013,#74014,#74015,#74016,#74017,#74018,#74019,#74020,
#74021,#74022,#74023,#74024,#74025,#74026,#74027,#74028,#74029,#74030,#74031,
#74032,#74033,#74034,#74035,#74036,#74037,#74038,#74039,#74040,#74041,#74042,
#74043,#74044,#74045,#74046,#74047,#74048,#74049,#74050,#74051,#74052,#74053,
#74054,#74055,#74056,#74057,#74058,#74059,#74060,#74061,#74062,#74063,#74064,
#74065,#74066,#74067,#74068,#74069,#74070,#74071,#74072,#74073,#74074,#74075,
#74076,#74077,#74078,#74079,#74080,#74081,#74082,#74083,#74084,#74085,#74086,
#74087,#74088,#74089,#74090,#74091,#74092,#74093,#74094,#74095,#74096,#74097,
#74098,#74099,#74100,#74101,#74102,#74103,#74104,#74105,#74106,#74107,#74108,
#74109,#74110,#74111,#74112,#74113,#74114,#74115,#74116,#74117,#74118,#74119,
#74120,#74121,#74122,#74123,#74124,#74125,#74126,#74127,#74128,#74129,#74130,
#74131,#74132,#74133,#74134,#74135,#74136,#74137,#74138,#74139,#74140,#74141,
#74142,#74143,#74144,#74145,#74146,#74147,#74148,#74149,#74150,#74151,#74152,
#74153,#74154,#74155,#74156,#74157,#74158,#74159,#74160,#74161,#74162,#74163,
#74164,#74165,#74166,#74167,#74168,#74169,#74170,#74171,#74172,#74173,#74174,
#74175,#74176,#74177)),.UNSPECIFIED.,.F.,.F.,.F.)
B_SPLINE_SURFACE_WITH_KNOTS((2,2),(3,2,2,2,2,2,2,2,2,2,2,2,2,2,2,2,2,2,
2,2,2,2,2,2,2,2,2,2,2,2,2,2,2,2,2,2,2,2,2,2,2,2,2,2,2,2,2,2,2,2,2,2,2,2,
2,2,2,2,2,2,2,2,2,2,2,2,2,2,2,2,2,2,2,2,2,2,2,2,2,2,2,2,2,2,2,2,2,2,2,2,
2,2,2,2,2,2,2,2,2,2,2,2,2,2,2,2,2,2,2,2,2,2,2,2,2,2,2,2,2,2,2,2,2,2,2,2,
2,2,2,2,2,2,2,2,2,2,2,2,2,2,2,2,2,2,2,2,2,2,2,2,2,2,2,2,2,2,2,2,2,2,2,2,
2,2,2,2,2,2,2,2,2,2,2,2,2,2,2,2,2,2,2,2,2,2,2,2,3),(-2.30253870309941E-5,
1.),(0.,0.00537634408602151,0.010752688172043,0.0161290322580645,0.021505376344086,
0.0268817204301075,0.032258064516129,0.0376344086021505,0.043010752688172,
0.0483870967741935,0.0537634408602151,0.0591397849462366,0.0645161290322581,
0.0698924731182796,0.0752688172043011,0.0806451612903226,0.0860215053763441,
0.0913978494623656,0.0967741935483871,0.102150537634409,0.10752688172043,
0.112903225806452,0.118279569892473,0.123655913978495,0.129032258064516,
0.134408602150538,0.139784946236559,0.145161290322581,0.150537634408602,
0.155913978494624,0.161290322580645,0.166666666666667,0.172043010752688,
0.17741935483871,0.182795698924731,0.188172043010753,0.193548387096774,
0.198924731182796,0.204301075268817,0.209677419354839,0.21505376344086,
0.220430107526882,0.225806451612903,0.231182795698925,0.236559139784946,
0.241935483870968,0.247311827956989,0.252688172043011,0.258064516129032,
0.263440860215054,0.268817204301075,0.274193548387097,0.279569892473118,
0.28494623655914,0.290322580645161,0.295698924731183,0.301075268817204,
0.306451612903226,0.311827956989247,0.317204301075269,0.32258064516129,
0.327956989247312,0.333333333333333,0.338709677419355,0.344086021505376,
0.349462365591398,0.354838709677419,0.360215053763441,0.365591397849462,
0.370967741935484,0.376344086021505,0.381720430107527,0.387096774193548,
0.39247311827957,0.397849462365591,0.403225806451613,0.408602150537634,
0.413978494623656,0.419354838709677,0.424731182795699,0.43010752688172,
0.435483870967742,0.440860215053763,0.446236559139785,0.451612903225806,
0.456989247311828,0.462365591397849,0.467741935483871,0.473118279569892,
0.478494623655914,0.483870967741935,0.489247311827957,0.494623655913978,
0.5,0.505376344086022,0.510752688172043,0.516129032258065,0.521505376344086,
0.526881720430108,0.532258064516129,0.537634408602151,0.543010752688172,
0.548387096774194,0.553763440860215,0.559139784946237,0.564516129032258,
0.56989247311828,0.575268817204301,0.580645161290323,0.586021505376344,
0.591397849462366,0.596774193548387,0.602150537634409,0.60752688172043,
0.612903225806452,0.618279569892473,0.623655913978495,0.629032258064516,
0.634408602150538,0.639784946236559,0.645161290322581,0.650537634408602,
0.655913978494624,0.661290322580645,0.666666666666667,0.672043010752688,
0.67741935483871,0.682795698924731,0.688172043010753,0.693548387096774,
0.698924731182796,0.704301075268817,0.709677419354839,0.71505376344086,
0.720430107526882,0.725806451612903,0.731182795698925,0.736559139784946,
0.741935483870968,0.747311827956989,0.752688172043011,0.758064516129032,
0.763440860215054,0.768817204301075,0.774193548387097,0.779569892473118,
0.78494623655914,0.790322580645161,0.795698924731183,0.801075268817204,
0.806451612903226,0.811827956989247,0.817204301075269,0.82258064516129,
0.827956989247312,0.833333333333333,0.838709677419355,0.844086021505376,
0.849462365591398,0.854838709677419,0.860215053763441,0.865591397849462,
0.870967741935484,0.876344086021505,0.881720430107527,0.887096774193548,
0.89247311827957,0.897849462365591,0.903225806451613,0.908602150537634,
0.913978494623656,0.919354838709677,0.924731182795699,0.93010752688172,
0.935483870967742,0.940860215053763,0.946236559139785,0.951612903225806,
0.956989247311828,0.962365591397849,0.967741935483871,0.973118279569892,
0.978494623655914,0.983870967741935,0.989247311827957,0.994623655913978,
1.),.UNSPECIFIED.)
GEOMETRIC_REPRESENTATION_ITEM()
RATIONAL_B_SPLINE_SURFACE(((1.,0.866025403784439,1.,0.866025403784439,1.,
0.866025403784439,1.,0.866025403784439,1.,0.866025403784439,1.,0.866025403784439,
1.,0.866025403784439,1.,0.866025403784439,1.,0.866025403784439,1.,0.866025403784439,
1.,0.866025403784439,1.,0.866025403784439,1.,0.866025403784439,1.,0.866025403784439,
1.,0.866025403784439,1.,0.866025403784439,1.,0.866025403784439,1.,0.866025403784439,
1.,0.866025403784439,1.,0.866025403784439,1.,0.866025403784439,1.,0.866025403784439,
1.,0.866025403784439,1.,0.866025403784439,1.,0.866025403784439,1.,0.866025403784439,
1.,0.866025403784439,1.,0.866025403784439,1.,0.866025403784439,1.,0.866025403784439,
1.,0.866025403784439,1.,0.866025403784439,1.,0.866025403784439,1.,0.866025403784439,
1.,0.866025403784439,1.,0.866025403784439,1.,0.866025403784439,1.,0.866025403784439,
1.,0.866025403784439,1.,0.866025403784439,1.,0.866025403784439,1.,0.866025403784439,
1.,0.866025403784439,1.,0.866025403784439,1.,0.866025403784439,1.,0.866025403784439,
1.,0.866025403784439,1.,0.866025403784439,1.,0.866025403784439,1.,0.866025403784439,
1.,0.866025403784439,1.,0.866025403784439,1.,0.866025403784439,1.,0.866025403784439,
1.,0.866025403784439,1.,0.866025403784439,1.,0.866025403784439,1.,0.866025403784439,
1.,0.866025403784439,1.,0.866025403784439,1.,0.866025403784439,1.,0.866025403784439,
1.,0.866025403784439,1.,0.866025403784439,1.,0.866025403784439,1.,0.866025403784439,
1.,0.866025403784439,1.,0.866025403784439,1.,0.866025403784439,1.,0.866025403784439,
1.,0.866025403784439,1.,0.866025403784439,1.,0.866025403784439,1.,0.866025403784439,
1.,0.866025403784439,1.,0.866025403784439,1.,0.866025403784439,1.,0.866025403784439,
1.,0.866025403784439,1.,0.866025403784439,1.,0.866025403784439,1.,0.866025403784439,
1.,0.866025403784439,1.,0.866025403784439,1.,0.866025403784439,1.,0.866025403784439,
1.,0.866025403784439,1.,0.866025403784439,1.,0.866025403784439,1.,0.866025403784439,
1.,0.866025403784439,1.,0.866025403784439,1.,0.866025403784439,1.,0.866025403784439,
1.,0.866025403784439,1.,0.866025403784439,1.,0.866025403784439,1.,0.866025403784439,
1.,0.866025403784439,1.,0.866025403784439,1.,0.866025403784439,1.,0.866025403784439,
1.,0.866025403784439,1.,0.866025403784439,1.,0.866025403784439,1.,0.866025403784439,
1.,0.866025403784439,1.,0.866025403784439,1.,0.866025403784439,1.,0.866025403784439,
1.,0.866025403784439,1.,0.866025403784439,1.,0.866025403784439,1.,0.866025403784439,
1.,0.866025403784439,1.,0.866025403784439,1.,0.866025403784439,1.,0.866025403784439,
1.,0.866025403784439,1.,0.866025403784439,1.,0.866025403784439,1.,0.866025403784439,
1.,0.866025403784439,1.,0.866025403784439,1.,0.866025403784439,1.,0.866025403784439,
1.,0.866025403784439,1.,0.866025403784439,1.,0.866025403784439,1.,0.866025403784439,
1.,0.866025403784439,1.,0.866025403784439,1.,0.866025403784439,1.,0.866025403784439,
1.,0.866025403784439,1.,0.866025403784439,1.,0.866025403784439,1.,0.866025403784439,
1.,0.866025403784439,1.,0.866025403784439,1.,0.866025403784439,1.,0.866025403784439,
1.,0.866025403784439,1.,0.866025403784439,1.,0.866025403784439,1.,0.866025403784439,
1.,0.866025403784439,1.,0.866025403784439,1.,0.866025403784439,1.,0.866025403784439,
1.,0.866025403784439,1.,0.866025403784439,1.,0.866025403784439,1.,0.866025403784439,
1.,0.866025403784439,1.,0.866025403784439,1.,0.866025403784439,1.,0.866025403784439,
1.,0.866025403784439,1.,0.866025403784439,1.,0.866025403784439,1.,0.866025403784439,
1.,0.866025403784439,1.,0.866025403784439,1.,0.866025403784439,1.,0.866025403784439,
1.,0.866025403784439,1.,0.866025403784439,1.,0.866025403784439,1.,0.866025403784439,
1.,0.866025403784439,1.,0.866025403784439,1.,0.866025403784439,1.,0.866025403784439,
1.,0.866025403784439,1.,0.866025403784439,1.,0.866025403784439,1.,0.866025403784439,
1.,0.866025403784439,1.,0.866025403784439,1.,0.866025403784439,1.,0.866025403784439,
1.,0.866025403784439,1.,0.866025403784439,1.,0.866025403784439,1.,0.866025403784439,
1.),(1.,0.866025403784439,1.,0.866025403784439,1.,0.866025403784439,1.,
0.866025403784439,1.,0.866025403784439,1.,0.866025403784439,1.,0.866025403784439,
1.,0.866025403784439,1.,0.866025403784439,1.,0.866025403784439,1.,0.866025403784439,
1.,0.866025403784439,1.,0.866025403784439,1.,0.866025403784439,1.,0.866025403784439,
1.,0.866025403784439,1.,0.866025403784439,1.,0.866025403784439,1.,0.866025403784439,
1.,0.866025403784439,1.,0.866025403784439,1.,0.866025403784439,1.,0.866025403784439,
1.,0.866025403784439,1.,0.866025403784439,1.,0.866025403784439,1.,0.866025403784439,
1.,0.866025403784439,1.,0.866025403784439,1.,0.866025403784439,1.,0.866025403784439,
1.,0.866025403784439,1.,0.866025403784439,1.,0.866025403784439,1.,0.866025403784439,
1.,0.866025403784439,1.,0.866025403784439,1.,0.866025403784439,1.,0.866025403784439,
1.,0.866025403784439,1.,0.866025403784439,1.,0.866025403784439,1.,0.866025403784439,
1.,0.866025403784439,1.,0.866025403784439,1.,0.866025403784439,1.,0.866025403784439,
1.,0.866025403784439,1.,0.866025403784439,1.,0.866025403784439,1.,0.866025403784439,
1.,0.866025403784439,1.,0.866025403784439,1.,0.866025403784439,1.,0.866025403784439,
1.,0.866025403784439,1.,0.866025403784439,1.,0.866025403784439,1.,0.866025403784439,
1.,0.866025403784439,1.,0.866025403784439,1.,0.866025403784439,1.,0.866025403784439,
1.,0.866025403784439,1.,0.866025403784439,1.,0.866025403784439,1.,0.866025403784439,
1.,0.866025403784439,1.,0.866025403784439,1.,0.866025403784439,1.,0.866025403784439,
1.,0.866025403784439,1.,0.866025403784439,1.,0.866025403784439,1.,0.866025403784439,
1.,0.866025403784439,1.,0.866025403784439,1.,0.866025403784439,1.,0.866025403784439,
1.,0.866025403784439,1.,0.866025403784439,1.,0.866025403784439,1.,0.866025403784439,
1.,0.866025403784439,1.,0.866025403784439,1.,0.866025403784439,1.,0.866025403784439,
1.,0.866025403784439,1.,0.866025403784439,1.,0.866025403784439,1.,0.866025403784439,
1.,0.866025403784439,1.,0.866025403784439,1.,0.866025403784439,1.,0.866025403784439,
1.,0.866025403784439,1.,0.866025403784439,1.,0.866025403784439,1.,0.866025403784439,
1.,0.866025403784439,1.,0.866025403784439,1.,0.866025403784439,1.,0.866025403784439,
1.,0.866025403784439,1.,0.866025403784439,1.,0.866025403784439,1.,0.866025403784439,
1.,0.866025403784439,1.,0.866025403784439,1.,0.866025403784439,1.,0.866025403784439,
1.,0.866025403784439,1.,0.866025403784439,1.,0.866025403784439,1.,0.866025403784439,
1.,0.866025403784439,1.,0.866025403784439,1.,0.866025403784439,1.,0.866025403784439,
1.,0.866025403784439,1.,0.866025403784439,1.,0.866025403784439,1.,0.866025403784439,
1.,0.866025403784439,1.,0.866025403784439,1.,0.866025403784439,1.,0.866025403784439,
1.,0.866025403784439,1.,0.866025403784439,1.,0.866025403784439,1.,0.866025403784439,
1.,0.866025403784439,1.,0.866025403784439,1.,0.866025403784439,1.,0.866025403784439,
1.,0.866025403784439,1.,0.866025403784439,1.,0.866025403784439,1.,0.866025403784439,
1.,0.866025403784439,1.,0.866025403784439,1.,0.866025403784439,1.,0.866025403784439,
1.,0.866025403784439,1.,0.866025403784439,1.,0.866025403784439,1.,0.866025403784439,
1.,0.866025403784439,1.,0.866025403784439,1.,0.866025403784439,1.,0.866025403784439,
1.,0.866025403784439,1.,0.866025403784439,1.,0.866025403784439,1.,0.866025403784439,
1.,0.866025403784439,1.,0.866025403784439,1.,0.866025403784439,1.,0.866025403784439,
1.,0.866025403784439,1.,0.866025403784439,1.,0.866025403784439,1.,0.866025403784439,
1.,0.866025403784439,1.,0.866025403784439,1.,0.866025403784439,1.,0.866025403784439,
1.,0.866025403784439,1.,0.866025403784439,1.,0.866025403784439,1.,0.866025403784439,
1.,0.866025403784439,1.,0.866025403784439,1.,0.866025403784439,1.,0.866025403784439,
1.,0.866025403784439,1.,0.866025403784439,1.,0.866025403784439,1.,0.866025403784439,
1.,0.866025403784439,1.,0.866025403784439,1.,0.866025403784439,1.,0.866025403784439,
1.,0.866025403784439,1.,0.866025403784439,1.,0.866025403784439,1.)))
REPRESENTATION_ITEM('')
SURFACE()
);
#48=(
BOUNDED_SURFACE()
B_SPLINE_SURFACE(1,2,((#74206,#74207,#74208,#74209,#74210,#74211,#74212,
#74213,#74214,#74215,#74216,#74217,#74218,#74219,#74220,#74221,#74222,#74223,
#74224,#74225,#74226,#74227,#74228,#74229,#74230,#74231,#74232,#74233,#74234,
#74235,#74236,#74237,#74238,#74239,#74240,#74241,#74242,#74243,#74244,#74245,
#74246,#74247,#74248,#74249,#74250,#74251,#74252,#74253,#74254,#74255,#74256,
#74257,#74258,#74259,#74260,#74261,#74262,#74263,#74264,#74265,#74266,#74267,
#74268,#74269,#74270,#74271,#74272,#74273,#74274,#74275,#74276,#74277,#74278,
#74279,#74280,#74281,#74282,#74283,#74284,#74285,#74286,#74287,#74288,#74289,
#74290,#74291,#74292,#74293,#74294,#74295,#74296,#74297,#74298,#74299,#74300,
#74301,#74302,#74303,#74304,#74305,#74306,#74307,#74308,#74309,#74310,#74311,
#74312,#74313,#74314,#74315,#74316,#74317,#74318,#74319,#74320,#74321,#74322,
#74323,#74324,#74325,#74326,#74327,#74328,#74329,#74330,#74331,#74332,#74333,
#74334,#74335,#74336,#74337,#74338,#74339,#74340,#74341,#74342,#74343,#74344,
#74345,#74346,#74347,#74348,#74349,#74350,#74351,#74352,#74353,#74354,#74355,
#74356,#74357,#74358,#74359,#74360,#74361,#74362,#74363,#74364,#74365,#74366,
#74367,#74368,#74369,#74370,#74371,#74372,#74373,#74374,#74375,#74376,#74377,
#74378,#74379,#74380,#74381,#74382,#74383,#74384,#74385,#74386,#74387,#74388,
#74389,#74390,#74391,#74392,#74393,#74394,#74395,#74396,#74397,#74398,#74399,
#74400,#74401,#74402,#74403,#74404,#74405,#74406,#74407,#74408,#74409,#74410,
#74411,#74412,#74413,#74414,#74415,#74416,#74417,#74418,#74419,#74420,#74421,
#74422,#74423,#74424,#74425,#74426,#74427,#74428,#74429,#74430,#74431,#74432,
#74433,#74434,#74435,#74436,#74437,#74438,#74439,#74440,#74441,#74442,#74443,
#74444,#74445,#74446,#74447,#74448,#74449,#74450,#74451,#74452,#74453,#74454,
#74455,#74456,#74457,#74458,#74459,#74460,#74461,#74462,#74463,#74464,#74465,
#74466,#74467,#74468,#74469,#74470,#74471,#74472,#74473,#74474,#74475,#74476,
#74477,#74478,#74479,#74480,#74481,#74482,#74483,#74484,#74485,#74486,#74487,
#74488,#74489,#74490,#74491,#74492,#74493,#74494,#74495,#74496,#74497,#74498,
#74499,#74500,#74501,#74502,#74503,#74504,#74505,#74506,#74507,#74508,#74509,
#74510,#74511,#74512,#74513,#74514,#74515,#74516,#74517,#74518,#74519,#74520,
#74521,#74522,#74523,#74524,#74525,#74526,#74527,#74528,#74529,#74530,#74531,
#74532,#74533,#74534,#74535,#74536,#74537,#74538,#74539,#74540,#74541,#74542,
#74543,#74544,#74545,#74546,#74547,#74548,#74549,#74550,#74551,#74552,#74553,
#74554,#74555,#74556,#74557,#74558,#74559,#74560,#74561,#74562,#74563,#74564,
#74565,#74566,#74567,#74568,#74569,#74570,#74571,#74572,#74573,#74574,#74575,
#74576,#74577,#74578),(#74579,#74580,#74581,#74582,#74583,#74584,#74585,
#74586,#74587,#74588,#74589,#74590,#74591,#74592,#74593,#74594,#74595,#74596,
#74597,#74598,#74599,#74600,#74601,#74602,#74603,#74604,#74605,#74606,#74607,
#74608,#74609,#74610,#74611,#74612,#74613,#74614,#74615,#74616,#74617,#74618,
#74619,#74620,#74621,#74622,#74623,#74624,#74625,#74626,#74627,#74628,#74629,
#74630,#74631,#74632,#74633,#74634,#74635,#74636,#74637,#74638,#74639,#74640,
#74641,#74642,#74643,#74644,#74645,#74646,#74647,#74648,#74649,#74650,#74651,
#74652,#74653,#74654,#74655,#74656,#74657,#74658,#74659,#74660,#74661,#74662,
#74663,#74664,#74665,#74666,#74667,#74668,#74669,#74670,#74671,#74672,#74673,
#74674,#74675,#74676,#74677,#74678,#74679,#74680,#74681,#74682,#74683,#74684,
#74685,#74686,#74687,#74688,#74689,#74690,#74691,#74692,#74693,#74694,#74695,
#74696,#74697,#74698,#74699,#74700,#74701,#74702,#74703,#74704,#74705,#74706,
#74707,#74708,#74709,#74710,#74711,#74712,#74713,#74714,#74715,#74716,#74717,
#74718,#74719,#74720,#74721,#74722,#74723,#74724,#74725,#74726,#74727,#74728,
#74729,#74730,#74731,#74732,#74733,#74734,#74735,#74736,#74737,#74738,#74739,
#74740,#74741,#74742,#74743,#74744,#74745,#74746,#74747,#74748,#74749,#74750,
#74751,#74752,#74753,#74754,#74755,#74756,#74757,#74758,#74759,#74760,#74761,
#74762,#74763,#74764,#74765,#74766,#74767,#74768,#74769,#74770,#74771,#74772,
#74773,#74774,#74775,#74776,#74777,#74778,#74779,#74780,#74781,#74782,#74783,
#74784,#74785,#74786,#74787,#74788,#74789,#74790,#74791,#74792,#74793,#74794,
#74795,#74796,#74797,#74798,#74799,#74800,#74801,#74802,#74803,#74804,#74805,
#74806,#74807,#74808,#74809,#74810,#74811,#74812,#74813,#74814,#74815,#74816,
#74817,#74818,#74819,#74820,#74821,#74822,#74823,#74824,#74825,#74826,#74827,
#74828,#74829,#74830,#74831,#74832,#74833,#74834,#74835,#74836,#74837,#74838,
#74839,#74840,#74841,#74842,#74843,#74844,#74845,#74846,#74847,#74848,#74849,
#74850,#74851,#74852,#74853,#74854,#74855,#74856,#74857,#74858,#74859,#74860,
#74861,#74862,#74863,#74864,#74865,#74866,#74867,#74868,#74869,#74870,#74871,
#74872,#74873,#74874,#74875,#74876,#74877,#74878,#74879,#74880,#74881,#74882,
#74883,#74884,#74885,#74886,#74887,#74888,#74889,#74890,#74891,#74892,#74893,
#74894,#74895,#74896,#74897,#74898,#74899,#74900,#74901,#74902,#74903,#74904,
#74905,#74906,#74907,#74908,#74909,#74910,#74911,#74912,#74913,#74914,#74915,
#74916,#74917,#74918,#74919,#74920,#74921,#74922,#74923,#74924,#74925,#74926,
#74927,#74928,#74929,#74930,#74931,#74932,#74933,#74934,#74935,#74936,#74937,
#74938,#74939,#74940,#74941,#74942,#74943,#74944,#74945,#74946,#74947,#74948,
#74949,#74950,#74951)),.UNSPECIFIED.,.F.,.F.,.F.)
B_SPLINE_SURFACE_WITH_KNOTS((2,2),(3,2,2,2,2,2,2,2,2,2,2,2,2,2,2,2,2,2,
2,2,2,2,2,2,2,2,2,2,2,2,2,2,2,2,2,2,2,2,2,2,2,2,2,2,2,2,2,2,2,2,2,2,2,2,
2,2,2,2,2,2,2,2,2,2,2,2,2,2,2,2,2,2,2,2,2,2,2,2,2,2,2,2,2,2,2,2,2,2,2,2,
2,2,2,2,2,2,2,2,2,2,2,2,2,2,2,2,2,2,2,2,2,2,2,2,2,2,2,2,2,2,2,2,2,2,2,2,
2,2,2,2,2,2,2,2,2,2,2,2,2,2,2,2,2,2,2,2,2,2,2,2,2,2,2,2,2,2,2,2,2,2,2,2,
2,2,2,2,2,2,2,2,2,2,2,2,2,2,2,2,2,2,2,2,2,2,2,2,3),(0.,1.00001535537392),
(0.,0.00537634408602151,0.010752688172043,0.0161290322580645,0.021505376344086,
0.0268817204301075,0.032258064516129,0.0376344086021505,0.043010752688172,
0.0483870967741935,0.0537634408602151,0.0591397849462366,0.0645161290322581,
0.0698924731182796,0.0752688172043011,0.0806451612903226,0.0860215053763441,
0.0913978494623656,0.0967741935483871,0.102150537634409,0.10752688172043,
0.112903225806452,0.118279569892473,0.123655913978495,0.129032258064516,
0.134408602150538,0.139784946236559,0.145161290322581,0.150537634408602,
0.155913978494624,0.161290322580645,0.166666666666667,0.172043010752688,
0.17741935483871,0.182795698924731,0.188172043010753,0.193548387096774,
0.198924731182796,0.204301075268817,0.209677419354839,0.21505376344086,
0.220430107526882,0.225806451612903,0.231182795698925,0.236559139784946,
0.241935483870968,0.247311827956989,0.252688172043011,0.258064516129032,
0.263440860215054,0.268817204301075,0.274193548387097,0.279569892473118,
0.28494623655914,0.290322580645161,0.295698924731183,0.301075268817204,
0.306451612903226,0.311827956989247,0.317204301075269,0.32258064516129,
0.327956989247312,0.333333333333333,0.338709677419355,0.344086021505376,
0.349462365591398,0.354838709677419,0.360215053763441,0.365591397849462,
0.370967741935484,0.376344086021505,0.381720430107527,0.387096774193548,
0.39247311827957,0.397849462365591,0.403225806451613,0.408602150537634,
0.413978494623656,0.419354838709677,0.424731182795699,0.43010752688172,
0.435483870967742,0.440860215053763,0.446236559139785,0.451612903225806,
0.456989247311828,0.462365591397849,0.467741935483871,0.473118279569892,
0.478494623655914,0.483870967741935,0.489247311827957,0.494623655913978,
0.5,0.505376344086022,0.510752688172043,0.516129032258065,0.521505376344086,
0.526881720430108,0.532258064516129,0.537634408602151,0.543010752688172,
0.548387096774194,0.553763440860215,0.559139784946237,0.564516129032258,
0.56989247311828,0.575268817204301,0.580645161290323,0.586021505376344,
0.591397849462366,0.596774193548387,0.602150537634409,0.60752688172043,
0.612903225806452,0.618279569892473,0.623655913978495,0.629032258064516,
0.634408602150538,0.639784946236559,0.645161290322581,0.650537634408602,
0.655913978494624,0.661290322580645,0.666666666666667,0.672043010752688,
0.67741935483871,0.682795698924731,0.688172043010753,0.693548387096774,
0.698924731182796,0.704301075268817,0.709677419354839,0.71505376344086,
0.720430107526882,0.725806451612903,0.731182795698925,0.736559139784946,
0.741935483870968,0.747311827956989,0.752688172043011,0.758064516129032,
0.763440860215054,0.768817204301075,0.774193548387097,0.779569892473118,
0.78494623655914,0.790322580645161,0.795698924731183,0.801075268817204,
0.806451612903226,0.811827956989247,0.817204301075269,0.82258064516129,
0.827956989247312,0.833333333333333,0.838709677419355,0.844086021505376,
0.849462365591398,0.854838709677419,0.860215053763441,0.865591397849462,
0.870967741935484,0.876344086021505,0.881720430107527,0.887096774193548,
0.89247311827957,0.897849462365591,0.903225806451613,0.908602150537634,
0.913978494623656,0.919354838709677,0.924731182795699,0.93010752688172,
0.935483870967742,0.940860215053763,0.946236559139785,0.951612903225806,
0.956989247311828,0.962365591397849,0.967741935483871,0.973118279569892,
0.978494623655914,0.983870967741935,0.989247311827957,0.994623655913978,
1.),.UNSPECIFIED.)
GEOMETRIC_REPRESENTATION_ITEM()
RATIONAL_B_SPLINE_SURFACE(((1.,0.866025403784439,1.,0.866025403784439,1.,
0.866025403784439,1.,0.866025403784439,1.,0.866025403784439,1.,0.866025403784439,
1.,0.866025403784439,1.,0.866025403784439,1.,0.866025403784439,1.,0.866025403784439,
1.,0.866025403784439,1.,0.866025403784439,1.,0.866025403784439,1.,0.866025403784439,
1.,0.866025403784439,1.,0.866025403784439,1.,0.866025403784439,1.,0.866025403784439,
1.,0.866025403784439,1.,0.866025403784439,1.,0.866025403784439,1.,0.866025403784439,
1.,0.866025403784439,1.,0.866025403784439,1.,0.866025403784439,1.,0.866025403784439,
1.,0.866025403784439,1.,0.866025403784439,1.,0.866025403784439,1.,0.866025403784439,
1.,0.866025403784439,1.,0.866025403784439,1.,0.866025403784439,1.,0.866025403784439,
1.,0.866025403784439,1.,0.866025403784439,1.,0.866025403784439,1.,0.866025403784439,
1.,0.866025403784439,1.,0.866025403784439,1.,0.866025403784439,1.,0.866025403784439,
1.,0.866025403784439,1.,0.866025403784439,1.,0.866025403784439,1.,0.866025403784439,
1.,0.866025403784439,1.,0.866025403784439,1.,0.866025403784439,1.,0.866025403784439,
1.,0.866025403784439,1.,0.866025403784439,1.,0.866025403784439,1.,0.866025403784439,
1.,0.866025403784439,1.,0.866025403784439,1.,0.866025403784439,1.,0.866025403784439,
1.,0.866025403784439,1.,0.866025403784439,1.,0.866025403784439,1.,0.866025403784439,
1.,0.866025403784439,1.,0.866025403784439,1.,0.866025403784439,1.,0.866025403784439,
1.,0.866025403784439,1.,0.866025403784439,1.,0.866025403784439,1.,0.866025403784439,
1.,0.866025403784439,1.,0.866025403784439,1.,0.866025403784439,1.,0.866025403784439,
1.,0.866025403784439,1.,0.866025403784439,1.,0.866025403784439,1.,0.866025403784439,
1.,0.866025403784439,1.,0.866025403784439,1.,0.866025403784439,1.,0.866025403784439,
1.,0.866025403784439,1.,0.866025403784439,1.,0.866025403784439,1.,0.866025403784439,
1.,0.866025403784439,1.,0.866025403784439,1.,0.866025403784439,1.,0.866025403784439,
1.,0.866025403784439,1.,0.866025403784439,1.,0.866025403784439,1.,0.866025403784439,
1.,0.866025403784439,1.,0.866025403784439,1.,0.866025403784439,1.,0.866025403784439,
1.,0.866025403784439,1.,0.866025403784439,1.,0.866025403784439,1.,0.866025403784439,
1.,0.866025403784439,1.,0.866025403784439,1.,0.866025403784439,1.,0.866025403784439,
1.,0.866025403784439,1.,0.866025403784439,1.,0.866025403784439,1.,0.866025403784439,
1.,0.866025403784439,1.,0.866025403784439,1.,0.866025403784439,1.,0.866025403784439,
1.,0.866025403784439,1.,0.866025403784439,1.,0.866025403784439,1.,0.866025403784439,
1.,0.866025403784439,1.,0.866025403784439,1.,0.866025403784439,1.,0.866025403784439,
1.,0.866025403784439,1.,0.866025403784439,1.,0.866025403784439,1.,0.866025403784439,
1.,0.866025403784439,1.,0.866025403784439,1.,0.866025403784439,1.,0.866025403784439,
1.,0.866025403784439,1.,0.866025403784439,1.,0.866025403784439,1.,0.866025403784439,
1.,0.866025403784439,1.,0.866025403784439,1.,0.866025403784439,1.,0.866025403784439,
1.,0.866025403784439,1.,0.866025403784439,1.,0.866025403784439,1.,0.866025403784439,
1.,0.866025403784439,1.,0.866025403784439,1.,0.866025403784439,1.,0.866025403784439,
1.,0.866025403784439,1.,0.866025403784439,1.,0.866025403784439,1.,0.866025403784439,
1.,0.866025403784439,1.,0.866025403784439,1.,0.866025403784439,1.,0.866025403784439,
1.,0.866025403784439,1.,0.866025403784439,1.,0.866025403784439,1.,0.866025403784439,
1.,0.866025403784439,1.,0.866025403784439,1.,0.866025403784439,1.,0.866025403784439,
1.,0.866025403784439,1.,0.866025403784439,1.,0.866025403784439,1.,0.866025403784439,
1.,0.866025403784439,1.,0.866025403784439,1.,0.866025403784439,1.,0.866025403784439,
1.,0.866025403784439,1.,0.866025403784439,1.,0.866025403784439,1.,0.866025403784439,
1.,0.866025403784439,1.,0.866025403784439,1.,0.866025403784439,1.,0.866025403784439,
1.,0.866025403784439,1.,0.866025403784439,1.,0.866025403784439,1.,0.866025403784439,
1.,0.866025403784439,1.,0.866025403784439,1.,0.866025403784439,1.,0.866025403784439,
1.),(1.,0.866025403784439,1.,0.866025403784439,1.,0.866025403784439,1.,
0.866025403784439,1.,0.866025403784439,1.,0.866025403784439,1.,0.866025403784439,
1.,0.866025403784439,1.,0.866025403784439,1.,0.866025403784439,1.,0.866025403784439,
1.,0.866025403784439,1.,0.866025403784439,1.,0.866025403784439,1.,0.866025403784439,
1.,0.866025403784439,1.,0.866025403784439,1.,0.866025403784439,1.,0.866025403784439,
1.,0.866025403784439,1.,0.866025403784439,1.,0.866025403784439,1.,0.866025403784439,
1.,0.866025403784439,1.,0.866025403784439,1.,0.866025403784439,1.,0.866025403784439,
1.,0.866025403784439,1.,0.866025403784439,1.,0.866025403784439,1.,0.866025403784439,
1.,0.866025403784439,1.,0.866025403784439,1.,0.866025403784439,1.,0.866025403784439,
1.,0.866025403784439,1.,0.866025403784439,1.,0.866025403784439,1.,0.866025403784439,
1.,0.866025403784439,1.,0.866025403784439,1.,0.866025403784439,1.,0.866025403784439,
1.,0.866025403784439,1.,0.866025403784439,1.,0.866025403784439,1.,0.866025403784439,
1.,0.866025403784439,1.,0.866025403784439,1.,0.866025403784439,1.,0.866025403784439,
1.,0.866025403784439,1.,0.866025403784439,1.,0.866025403784439,1.,0.866025403784439,
1.,0.866025403784439,1.,0.866025403784439,1.,0.866025403784439,1.,0.866025403784439,
1.,0.866025403784439,1.,0.866025403784439,1.,0.866025403784439,1.,0.866025403784439,
1.,0.866025403784439,1.,0.866025403784439,1.,0.866025403784439,1.,0.866025403784439,
1.,0.866025403784439,1.,0.866025403784439,1.,0.866025403784439,1.,0.866025403784439,
1.,0.866025403784439,1.,0.866025403784439,1.,0.866025403784439,1.,0.866025403784439,
1.,0.866025403784439,1.,0.866025403784439,1.,0.866025403784439,1.,0.866025403784439,
1.,0.866025403784439,1.,0.866025403784439,1.,0.866025403784439,1.,0.866025403784439,
1.,0.866025403784439,1.,0.866025403784439,1.,0.866025403784439,1.,0.866025403784439,
1.,0.866025403784439,1.,0.866025403784439,1.,0.866025403784439,1.,0.866025403784439,
1.,0.866025403784439,1.,0.866025403784439,1.,0.866025403784439,1.,0.866025403784439,
1.,0.866025403784439,1.,0.866025403784439,1.,0.866025403784439,1.,0.866025403784439,
1.,0.866025403784439,1.,0.866025403784439,1.,0.866025403784439,1.,0.866025403784439,
1.,0.866025403784439,1.,0.866025403784439,1.,0.866025403784439,1.,0.866025403784439,
1.,0.866025403784439,1.,0.866025403784439,1.,0.866025403784439,1.,0.866025403784439,
1.,0.866025403784439,1.,0.866025403784439,1.,0.866025403784439,1.,0.866025403784439,
1.,0.866025403784439,1.,0.866025403784439,1.,0.866025403784439,1.,0.866025403784439,
1.,0.866025403784439,1.,0.866025403784439,1.,0.866025403784439,1.,0.866025403784439,
1.,0.866025403784439,1.,0.866025403784439,1.,0.866025403784439,1.,0.866025403784439,
1.,0.866025403784439,1.,0.866025403784439,1.,0.866025403784439,1.,0.866025403784439,
1.,0.866025403784439,1.,0.866025403784439,1.,0.866025403784439,1.,0.866025403784439,
1.,0.866025403784439,1.,0.866025403784439,1.,0.866025403784439,1.,0.866025403784439,
1.,0.866025403784439,1.,0.866025403784439,1.,0.866025403784439,1.,0.866025403784439,
1.,0.866025403784439,1.,0.866025403784439,1.,0.866025403784439,1.,0.866025403784439,
1.,0.866025403784439,1.,0.866025403784439,1.,0.866025403784439,1.,0.866025403784439,
1.,0.866025403784439,1.,0.866025403784439,1.,0.866025403784439,1.,0.866025403784439,
1.,0.866025403784439,1.,0.866025403784439,1.,0.866025403784439,1.,0.866025403784439,
1.,0.866025403784439,1.,0.866025403784439,1.,0.866025403784439,1.,0.866025403784439,
1.,0.866025403784439,1.,0.866025403784439,1.,0.866025403784439,1.,0.866025403784439,
1.,0.866025403784439,1.,0.866025403784439,1.,0.866025403784439,1.,0.866025403784439,
1.,0.866025403784439,1.,0.866025403784439,1.,0.866025403784439,1.,0.866025403784439,
1.,0.866025403784439,1.,0.866025403784439,1.,0.866025403784439,1.,0.866025403784439,
1.,0.866025403784439,1.,0.866025403784439,1.,0.866025403784439,1.,0.866025403784439,
1.,0.866025403784439,1.,0.866025403784439,1.,0.866025403784439,1.)))
REPRESENTATION_ITEM('')
SURFACE()
);
#49=TOROIDAL_SURFACE('',#32314,2.58058373926377,0.0468749999999982);
#50=TOROIDAL_SURFACE('',#32610,2.721875,0.0468749999999996);
#51=TOROIDAL_SURFACE('',#32615,2.60625,0.0687500000000002);
#52=TOROIDAL_SURFACE('',#32618,1.65,0.15);
#53=TOROIDAL_SURFACE('',#32621,2.703125,0.0468750000000018);
#54=TOROIDAL_SURFACE('',#32625,2.703125,0.0468750000000018);
#55=TOROIDAL_SURFACE('',#32629,2.703125,0.0468750000000018);
#56=TOROIDAL_SURFACE('',#32633,2.703125,0.0468750000000018);
#57=TOROIDAL_SURFACE('',#32637,2.703125,0.0468750000000018);
#58=TOROIDAL_SURFACE('',#32641,2.703125,0.0468750000000018);
#59=TOROIDAL_SURFACE('',#32645,2.703125,0.0468750000000018);
#60=TOROIDAL_SURFACE('',#32649,2.703125,0.0468750000000018);
#61=TOROIDAL_SURFACE('',#32653,2.703125,0.0468750000000018);
#62=TOROIDAL_SURFACE('',#32657,2.703125,0.0468750000000018);
#63=TOROIDAL_SURFACE('',#32661,2.703125,0.0468750000000018);
#64=TOROIDAL_SURFACE('',#32665,2.703125,0.0468750000000018);
#65=TOROIDAL_SURFACE('',#32669,2.703125,0.0468750000000018);
#66=TOROIDAL_SURFACE('',#32673,2.703125,0.0468750000000018);
#67=TOROIDAL_SURFACE('',#32677,2.703125,0.0468750000000018);
#68=TOROIDAL_SURFACE('',#32681,2.703125,0.0468750000000018);
#69=TOROIDAL_SURFACE('',#32685,2.703125,0.0468750000000018);
#70=TOROIDAL_SURFACE('',#32689,2.703125,0.0468750000000018);
#71=TOROIDAL_SURFACE('',#32693,2.703125,0.0468750000000018);
#72=TOROIDAL_SURFACE('',#32697,2.703125,0.0468750000000018);
#73=TOROIDAL_SURFACE('',#32701,2.703125,0.0468750000000018);
#74=TOROIDAL_SURFACE('',#32705,2.703125,0.0468750000000018);
#75=TOROIDAL_SURFACE('',#32709,2.703125,0.0468750000000018);
#76=TOROIDAL_SURFACE('',#32713,2.703125,0.0468750000000018);
#77=TOROIDAL_SURFACE('',#32717,2.703125,0.0468750000000018);
#78=TOROIDAL_SURFACE('',#32721,2.703125,0.0468750000000018);
#79=TOROIDAL_SURFACE('',#32725,2.703125,0.0468750000000018);
#80=TOROIDAL_SURFACE('',#32729,2.703125,0.0468750000000018);
#81=TOROIDAL_SURFACE('',#32733,2.703125,0.0468750000000018);
#82=TOROIDAL_SURFACE('',#32737,2.703125,0.0468750000000018);
#83=TOROIDAL_SURFACE('',#32741,2.703125,0.0468750000000018);
#84=TOROIDAL_SURFACE('',#32745,2.703125,0.0468750000000018);
#85=TOROIDAL_SURFACE('',#32749,2.703125,0.0468750000000018);
#86=TOROIDAL_SURFACE('',#32753,2.703125,0.0468750000000018);
#87=TOROIDAL_SURFACE('',#32757,2.703125,0.0468750000000018);
#88=TOROIDAL_SURFACE('',#32761,2.703125,0.0468750000000018);
#89=TOROIDAL_SURFACE('',#32765,2.703125,0.0468750000000018);
#90=TOROIDAL_SURFACE('',#32769,2.703125,0.0468750000000018);
#91=TOROIDAL_SURFACE('',#32773,2.703125,0.0468750000000018);
#92=TOROIDAL_SURFACE('',#32777,2.703125,0.0468750000000018);
#93=TOROIDAL_SURFACE('',#32781,2.703125,0.0468750000000018);
#94=TOROIDAL_SURFACE('',#32785,2.703125,0.0468750000000018);
#95=TOROIDAL_SURFACE('',#32789,2.703125,0.0468750000000018);
#96=TOROIDAL_SURFACE('',#32793,2.703125,0.0468750000000018);
#97=TOROIDAL_SURFACE('',#32797,2.703125,0.0468750000000018);
#98=TOROIDAL_SURFACE('',#32801,2.703125,0.0468750000000018);
#99=TOROIDAL_SURFACE('',#32805,2.703125,0.0468750000000018);
#100=TOROIDAL_SURFACE('',#32809,2.703125,0.0468750000000018);
#101=TOROIDAL_SURFACE('',#32813,2.703125,0.0468750000000018);
#102=TOROIDAL_SURFACE('',#32817,2.703125,0.0468750000000018);
#103=TOROIDAL_SURFACE('',#32821,2.703125,0.0468750000000018);
#104=TOROIDAL_SURFACE('',#32825,2.703125,0.0468750000000018);
#105=TOROIDAL_SURFACE('',#32829,2.703125,0.0468750000000018);
#106=TOROIDAL_SURFACE('',#32833,2.703125,0.0468750000000018);
#107=TOROIDAL_SURFACE('',#32837,2.703125,0.0468750000000018);
#108=TOROIDAL_SURFACE('',#32841,2.703125,0.0468750000000018);
#109=TOROIDAL_SURFACE('',#32845,2.703125,0.0468750000000018);
#110=TOROIDAL_SURFACE('',#32849,2.703125,0.0468750000000018);
#111=TOROIDAL_SURFACE('',#32853,2.703125,0.0468750000000018);
#112=TOROIDAL_SURFACE('',#32857,2.703125,0.0468750000000018);
#113=TOROIDAL_SURFACE('',#32861,2.703125,0.0468750000000018);
#114=TOROIDAL_SURFACE('',#32865,2.703125,0.0468750000000018);
#115=TOROIDAL_SURFACE('',#32869,2.703125,0.0468750000000018);
#116=TOROIDAL_SURFACE('',#32873,2.703125,0.0468750000000018);
#117=TOROIDAL_SURFACE('',#32877,2.703125,0.0468750000000018);
#118=TOROIDAL_SURFACE('',#32881,2.703125,0.0468750000000018);
#119=TOROIDAL_SURFACE('',#32885,2.703125,0.0468750000000018);
#120=TOROIDAL_SURFACE('',#32889,2.703125,0.0468750000000018);
#121=TOROIDAL_SURFACE('',#32893,2.703125,0.0468750000000018);
#122=TOROIDAL_SURFACE('',#32897,2.703125,0.0468750000000018);
#123=TOROIDAL_SURFACE('',#32901,2.703125,0.0468750000000018);
#124=TOROIDAL_SURFACE('',#32905,2.703125,0.0468750000000018);
#125=TOROIDAL_SURFACE('',#32909,2.703125,0.0468750000000018);
#126=TOROIDAL_SURFACE('',#32913,2.703125,0.0468750000000018);
#127=TOROIDAL_SURFACE('',#32917,2.703125,0.0468750000000018);
#128=TOROIDAL_SURFACE('',#32921,2.703125,0.0468750000000018);
#129=TOROIDAL_SURFACE('',#32925,2.703125,0.0468750000000018);
#130=TOROIDAL_SURFACE('',#32929,2.703125,0.0468750000000018);
#131=TOROIDAL_SURFACE('',#32933,2.703125,0.0468750000000018);
#132=TOROIDAL_SURFACE('',#33095,2.703125,0.046874999999999);
#133=TOROIDAL_SURFACE('',#33098,2.703125,0.046874999999999);
#134=TOROIDAL_SURFACE('',#33101,2.703125,0.046874999999999);
#135=TOROIDAL_SURFACE('',#33104,2.703125,0.046874999999999);
#136=TOROIDAL_SURFACE('',#33107,2.703125,0.046874999999999);
#137=TOROIDAL_SURFACE('',#33110,2.703125,0.046874999999999);
#138=TOROIDAL_SURFACE('',#33113,2.703125,0.046874999999999);
#139=TOROIDAL_SURFACE('',#33116,2.703125,0.046874999999999);
#140=TOROIDAL_SURFACE('',#33119,2.703125,0.046874999999999);
#141=TOROIDAL_SURFACE('',#33122,2.703125,0.046874999999999);
#142=TOROIDAL_SURFACE('',#33125,2.703125,0.046874999999999);
#143=TOROIDAL_SURFACE('',#33128,2.703125,0.046874999999999);
#144=TOROIDAL_SURFACE('',#33131,2.703125,0.046874999999999);
#145=TOROIDAL_SURFACE('',#33134,2.703125,0.046874999999999);
#146=TOROIDAL_SURFACE('',#33137,2.703125,0.046874999999999);
#147=TOROIDAL_SURFACE('',#33140,2.703125,0.046874999999999);
#148=TOROIDAL_SURFACE('',#33143,2.703125,0.046874999999999);
#149=TOROIDAL_SURFACE('',#33146,2.703125,0.046874999999999);
#150=TOROIDAL_SURFACE('',#33149,2.703125,0.046874999999999);
#151=TOROIDAL_SURFACE('',#33152,2.703125,0.046874999999999);
#152=TOROIDAL_SURFACE('',#33155,2.703125,0.046874999999999);
#153=TOROIDAL_SURFACE('',#33158,2.703125,0.046874999999999);
#154=TOROIDAL_SURFACE('',#33161,2.703125,0.046874999999999);
#155=TOROIDAL_SURFACE('',#33164,2.703125,0.046874999999999);
#156=TOROIDAL_SURFACE('',#33167,2.703125,0.046874999999999);
#157=TOROIDAL_SURFACE('',#33170,2.703125,0.046874999999999);
#158=TOROIDAL_SURFACE('',#33173,2.703125,0.046874999999999);
#159=TOROIDAL_SURFACE('',#33176,2.703125,0.046874999999999);
#160=TOROIDAL_SURFACE('',#33179,2.703125,0.046874999999999);
#161=TOROIDAL_SURFACE('',#33182,2.703125,0.046874999999999);
#162=TOROIDAL_SURFACE('',#33185,2.703125,0.046874999999999);
#163=TOROIDAL_SURFACE('',#33188,2.703125,0.046874999999999);
#164=TOROIDAL_SURFACE('',#33191,2.703125,0.046874999999999);
#165=TOROIDAL_SURFACE('',#33194,2.703125,0.046874999999999);
#166=TOROIDAL_SURFACE('',#33197,2.703125,0.046874999999999);
#167=TOROIDAL_SURFACE('',#33200,2.703125,0.046874999999999);
#168=TOROIDAL_SURFACE('',#33203,2.703125,0.046874999999999);
#169=TOROIDAL_SURFACE('',#33206,2.703125,0.046874999999999);
#170=TOROIDAL_SURFACE('',#33209,2.703125,0.046874999999999);
#171=TOROIDAL_SURFACE('',#33212,2.703125,0.046874999999999);
#172=TOROIDAL_SURFACE('',#33215,2.703125,0.046874999999999);
#173=TOROIDAL_SURFACE('',#33218,2.703125,0.046874999999999);
#174=TOROIDAL_SURFACE('',#33221,2.703125,0.046874999999999);
#175=TOROIDAL_SURFACE('',#33224,2.703125,0.046874999999999);
#176=TOROIDAL_SURFACE('',#33227,2.703125,0.046874999999999);
#177=TOROIDAL_SURFACE('',#33230,2.703125,0.046874999999999);
#178=TOROIDAL_SURFACE('',#33233,2.703125,0.046874999999999);
#179=TOROIDAL_SURFACE('',#33236,2.703125,0.046874999999999);
#180=TOROIDAL_SURFACE('',#33239,2.703125,0.046874999999999);
#181=TOROIDAL_SURFACE('',#33242,2.703125,0.046874999999999);
#182=TOROIDAL_SURFACE('',#33245,2.703125,0.046874999999999);
#183=TOROIDAL_SURFACE('',#33248,2.703125,0.046874999999999);
#184=TOROIDAL_SURFACE('',#33251,2.703125,0.046874999999999);
#185=TOROIDAL_SURFACE('',#33254,2.703125,0.046874999999999);
#186=TOROIDAL_SURFACE('',#33257,2.703125,0.046874999999999);
#187=TOROIDAL_SURFACE('',#33260,2.703125,0.046874999999999);
#188=TOROIDAL_SURFACE('',#33263,2.703125,0.046874999999999);
#189=TOROIDAL_SURFACE('',#33266,2.703125,0.046874999999999);
#190=TOROIDAL_SURFACE('',#33269,2.703125,0.046874999999999);
#191=TOROIDAL_SURFACE('',#33272,2.703125,0.046874999999999);
#192=TOROIDAL_SURFACE('',#33275,2.703125,0.046874999999999);
#193=TOROIDAL_SURFACE('',#33278,2.703125,0.046874999999999);
#194=TOROIDAL_SURFACE('',#33281,2.703125,0.046874999999999);
#195=TOROIDAL_SURFACE('',#33284,2.703125,0.046874999999999);
#196=TOROIDAL_SURFACE('',#33287,2.703125,0.046874999999999);
#197=TOROIDAL_SURFACE('',#33290,2.703125,0.046874999999999);
#198=TOROIDAL_SURFACE('',#33293,2.703125,0.046874999999999);
#199=TOROIDAL_SURFACE('',#33296,2.703125,0.046874999999999);
#200=TOROIDAL_SURFACE('',#33299,2.703125,0.046874999999999);
#201=TOROIDAL_SURFACE('',#33302,2.703125,0.046874999999999);
#202=TOROIDAL_SURFACE('',#33305,2.703125,0.046874999999999);
#203=TOROIDAL_SURFACE('',#33308,2.703125,0.046874999999999);
#204=TOROIDAL_SURFACE('',#33311,2.703125,0.046874999999999);
#205=TOROIDAL_SURFACE('',#33314,2.703125,0.046874999999999);
#206=TOROIDAL_SURFACE('',#33317,2.703125,0.046874999999999);
#207=TOROIDAL_SURFACE('',#33320,2.703125,0.046874999999999);
#208=TOROIDAL_SURFACE('',#33323,2.703125,0.046874999999999);
#209=TOROIDAL_SURFACE('',#33326,2.703125,0.046874999999999);
#210=TOROIDAL_SURFACE('',#33329,2.703125,0.046874999999999);
#211=TOROIDAL_SURFACE('',#33334,2.703125,0.0468750000000018);
#212=TOROIDAL_SURFACE('',#33340,2.703125,0.046874999999999);
#213=TOROIDAL_SURFACE('',#33694,2.58058373926377,0.0468749999999982);
#214=TOROIDAL_SURFACE('',#33990,2.721875,0.0468749999999996);
#215=TOROIDAL_SURFACE('',#33995,2.60625,0.0687500000000002);
#216=TOROIDAL_SURFACE('',#33998,1.65,0.15);
#217=TOROIDAL_SURFACE('',#34001,2.703125,0.0468750000000018);
#218=TOROIDAL_SURFACE('',#34005,2.703125,0.0468750000000018);
#219=TOROIDAL_SURFACE('',#34009,2.703125,0.0468750000000018);
#220=TOROIDAL_SURFACE('',#34013,2.703125,0.0468750000000018);
#221=TOROIDAL_SURFACE('',#34017,2.703125,0.0468750000000018);
#222=TOROIDAL_SURFACE('',#34021,2.703125,0.0468750000000018);
#223=TOROIDAL_SURFACE('',#34025,2.703125,0.0468750000000018);
#224=TOROIDAL_SURFACE('',#34029,2.703125,0.0468750000000018);
#225=TOROIDAL_SURFACE('',#34033,2.703125,0.0468750000000018);
#226=TOROIDAL_SURFACE('',#34037,2.703125,0.0468750000000018);
#227=TOROIDAL_SURFACE('',#34041,2.703125,0.0468750000000018);
#228=TOROIDAL_SURFACE('',#34045,2.703125,0.0468750000000018);
#229=TOROIDAL_SURFACE('',#34049,2.703125,0.0468750000000018);
#230=TOROIDAL_SURFACE('',#34053,2.703125,0.0468750000000018);
#231=TOROIDAL_SURFACE('',#34057,2.703125,0.0468750000000018);
#232=TOROIDAL_SURFACE('',#34061,2.703125,0.0468750000000018);
#233=TOROIDAL_SURFACE('',#34065,2.703125,0.0468750000000018);
#234=TOROIDAL_SURFACE('',#34069,2.703125,0.0468750000000018);
#235=TOROIDAL_SURFACE('',#34073,2.703125,0.0468750000000018);
#236=TOROIDAL_SURFACE('',#34077,2.703125,0.0468750000000018);
#237=TOROIDAL_SURFACE('',#34081,2.703125,0.0468750000000018);
#238=TOROIDAL_SURFACE('',#34085,2.703125,0.0468750000000018);
#239=TOROIDAL_SURFACE('',#34089,2.703125,0.0468750000000018);
#240=TOROIDAL_SURFACE('',#34093,2.703125,0.0468750000000018);
#241=TOROIDAL_SURFACE('',#34097,2.703125,0.0468750000000018);
#242=TOROIDAL_SURFACE('',#34101,2.703125,0.0468750000000018);
#243=TOROIDAL_SURFACE('',#34105,2.703125,0.0468750000000018);
#244=TOROIDAL_SURFACE('',#34109,2.703125,0.0468750000000018);
#245=TOROIDAL_SURFACE('',#34113,2.703125,0.0468750000000018);
#246=TOROIDAL_SURFACE('',#34117,2.703125,0.0468750000000018);
#247=TOROIDAL_SURFACE('',#34121,2.703125,0.0468750000000018);
#248=TOROIDAL_SURFACE('',#34125,2.703125,0.0468750000000018);
#249=TOROIDAL_SURFACE('',#34129,2.703125,0.0468750000000018);
#250=TOROIDAL_SURFACE('',#34133,2.703125,0.0468750000000018);
#251=TOROIDAL_SURFACE('',#34137,2.703125,0.0468750000000018);
#252=TOROIDAL_SURFACE('',#34141,2.703125,0.0468750000000018);
#253=TOROIDAL_SURFACE('',#34145,2.703125,0.0468750000000018);
#254=TOROIDAL_SURFACE('',#34149,2.703125,0.0468750000000018);
#255=TOROIDAL_SURFACE('',#34153,2.703125,0.0468750000000018);
#256=TOROIDAL_SURFACE('',#34157,2.703125,0.0468750000000018);
#257=TOROIDAL_SURFACE('',#34161,2.703125,0.0468750000000018);
#258=TOROIDAL_SURFACE('',#34165,2.703125,0.0468750000000018);
#259=TOROIDAL_SURFACE('',#34169,2.703125,0.0468750000000018);
#260=TOROIDAL_SURFACE('',#34173,2.703125,0.0468750000000018);
#261=TOROIDAL_SURFACE('',#34177,2.703125,0.0468750000000018);
#262=TOROIDAL_SURFACE('',#34181,2.703125,0.0468750000000018);
#263=TOROIDAL_SURFACE('',#34185,2.703125,0.0468750000000018);
#264=TOROIDAL_SURFACE('',#34189,2.703125,0.0468750000000018);
#265=TOROIDAL_SURFACE('',#34193,2.703125,0.0468750000000018);
#266=TOROIDAL_SURFACE('',#34197,2.703125,0.0468750000000018);
#267=TOROIDAL_SURFACE('',#34201,2.703125,0.0468750000000018);
#268=TOROIDAL_SURFACE('',#34205,2.703125,0.0468750000000018);
#269=TOROIDAL_SURFACE('',#34209,2.703125,0.0468750000000018);
#270=TOROIDAL_SURFACE('',#34213,2.703125,0.0468750000000018);
#271=TOROIDAL_SURFACE('',#34217,2.703125,0.0468750000000018);
#272=TOROIDAL_SURFACE('',#34221,2.703125,0.0468750000000018);
#273=TOROIDAL_SURFACE('',#34225,2.703125,0.0468750000000018);
#274=TOROIDAL_SURFACE('',#34229,2.703125,0.0468750000000018);
#275=TOROIDAL_SURFACE('',#34233,2.703125,0.0468750000000018);
#276=TOROIDAL_SURFACE('',#34237,2.703125,0.0468750000000018);
#277=TOROIDAL_SURFACE('',#34241,2.703125,0.0468750000000018);
#278=TOROIDAL_SURFACE('',#34245,2.703125,0.0468750000000018);
#279=TOROIDAL_SURFACE('',#34249,2.703125,0.0468750000000018);
#280=TOROIDAL_SURFACE('',#34253,2.703125,0.0468750000000018);
#281=TOROIDAL_SURFACE('',#34257,2.703125,0.0468750000000018);
#282=TOROIDAL_SURFACE('',#34261,2.703125,0.0468750000000018);
#283=TOROIDAL_SURFACE('',#34265,2.703125,0.0468750000000018);
#284=TOROIDAL_SURFACE('',#34269,2.703125,0.0468750000000018);
#285=TOROIDAL_SURFACE('',#34273,2.703125,0.0468750000000018);
#286=TOROIDAL_SURFACE('',#34277,2.703125,0.0468750000000018);
#287=TOROIDAL_SURFACE('',#34281,2.703125,0.0468750000000018);
#288=TOROIDAL_SURFACE('',#34285,2.703125,0.0468750000000018);
#289=TOROIDAL_SURFACE('',#34289,2.703125,0.0468750000000018);
#290=TOROIDAL_SURFACE('',#34293,2.703125,0.0468750000000018);
#291=TOROIDAL_SURFACE('',#34297,2.703125,0.0468750000000018);
#292=TOROIDAL_SURFACE('',#34301,2.703125,0.0468750000000018);
#293=TOROIDAL_SURFACE('',#34305,2.703125,0.0468750000000018);
#294=TOROIDAL_SURFACE('',#34309,2.703125,0.0468750000000018);
#295=TOROIDAL_SURFACE('',#34313,2.703125,0.0468750000000018);
#296=TOROIDAL_SURFACE('',#34475,2.703125,0.046874999999999);
#297=TOROIDAL_SURFACE('',#34478,2.703125,0.046874999999999);
#298=TOROIDAL_SURFACE('',#34481,2.703125,0.046874999999999);
#299=TOROIDAL_SURFACE('',#34484,2.703125,0.046874999999999);
#300=TOROIDAL_SURFACE('',#34487,2.703125,0.046874999999999);
#301=TOROIDAL_SURFACE('',#34490,2.703125,0.046874999999999);
#302=TOROIDAL_SURFACE('',#34493,2.703125,0.046874999999999);
#303=TOROIDAL_SURFACE('',#34496,2.703125,0.046874999999999);
#304=TOROIDAL_SURFACE('',#34499,2.703125,0.046874999999999);
#305=TOROIDAL_SURFACE('',#34502,2.703125,0.046874999999999);
#306=TOROIDAL_SURFACE('',#34505,2.703125,0.046874999999999);
#307=TOROIDAL_SURFACE('',#34508,2.703125,0.046874999999999);
#308=TOROIDAL_SURFACE('',#34511,2.703125,0.046874999999999);
#309=TOROIDAL_SURFACE('',#34514,2.703125,0.046874999999999);
#310=TOROIDAL_SURFACE('',#34517,2.703125,0.046874999999999);
#311=TOROIDAL_SURFACE('',#34520,2.703125,0.046874999999999);
#312=TOROIDAL_SURFACE('',#34523,2.703125,0.046874999999999);
#313=TOROIDAL_SURFACE('',#34526,2.703125,0.046874999999999);
#314=TOROIDAL_SURFACE('',#34529,2.703125,0.046874999999999);
#315=TOROIDAL_SURFACE('',#34532,2.703125,0.046874999999999);
#316=TOROIDAL_SURFACE('',#34535,2.703125,0.046874999999999);
#317=TOROIDAL_SURFACE('',#34538,2.703125,0.046874999999999);
#318=TOROIDAL_SURFACE('',#34541,2.703125,0.046874999999999);
#319=TOROIDAL_SURFACE('',#34544,2.703125,0.046874999999999);
#320=TOROIDAL_SURFACE('',#34547,2.703125,0.046874999999999);
#321=TOROIDAL_SURFACE('',#34550,2.703125,0.046874999999999);
#322=TOROIDAL_SURFACE('',#34553,2.703125,0.046874999999999);
#323=TOROIDAL_SURFACE('',#34556,2.703125,0.046874999999999);
#324=TOROIDAL_SURFACE('',#34559,2.703125,0.046874999999999);
#325=TOROIDAL_SURFACE('',#34562,2.703125,0.046874999999999);
#326=TOROIDAL_SURFACE('',#34565,2.703125,0.046874999999999);
#327=TOROIDAL_SURFACE('',#34568,2.703125,0.046874999999999);
#328=TOROIDAL_SURFACE('',#34571,2.703125,0.046874999999999);
#329=TOROIDAL_SURFACE('',#34574,2.703125,0.046874999999999);
#330=TOROIDAL_SURFACE('',#34577,2.703125,0.046874999999999);
#331=TOROIDAL_SURFACE('',#34580,2.703125,0.046874999999999);
#332=TOROIDAL_SURFACE('',#34583,2.703125,0.046874999999999);
#333=TOROIDAL_SURFACE('',#34586,2.703125,0.046874999999999);
#334=TOROIDAL_SURFACE('',#34589,2.703125,0.046874999999999);
#335=TOROIDAL_SURFACE('',#34592,2.703125,0.046874999999999);
#336=TOROIDAL_SURFACE('',#34595,2.703125,0.046874999999999);
#337=TOROIDAL_SURFACE('',#34598,2.703125,0.046874999999999);
#338=TOROIDAL_SURFACE('',#34601,2.703125,0.046874999999999);
#339=TOROIDAL_SURFACE('',#34604,2.703125,0.046874999999999);
#340=TOROIDAL_SURFACE('',#34607,2.703125,0.046874999999999);
#341=TOROIDAL_SURFACE('',#34610,2.703125,0.046874999999999);
#342=TOROIDAL_SURFACE('',#34613,2.703125,0.046874999999999);
#343=TOROIDAL_SURFACE('',#34616,2.703125,0.046874999999999);
#344=TOROIDAL_SURFACE('',#34619,2.703125,0.046874999999999);
#345=TOROIDAL_SURFACE('',#34622,2.703125,0.046874999999999);
#346=TOROIDAL_SURFACE('',#34625,2.703125,0.046874999999999);
#347=TOROIDAL_SURFACE('',#34628,2.703125,0.046874999999999);
#348=TOROIDAL_SURFACE('',#34631,2.703125,0.046874999999999);
#349=TOROIDAL_SURFACE('',#34634,2.703125,0.046874999999999);
#350=TOROIDAL_SURFACE('',#34637,2.703125,0.046874999999999);
#351=TOROIDAL_SURFACE('',#34640,2.703125,0.046874999999999);
#352=TOROIDAL_SURFACE('',#34643,2.703125,0.046874999999999);
#353=TOROIDAL_SURFACE('',#34646,2.703125,0.046874999999999);
#354=TOROIDAL_SURFACE('',#34649,2.703125,0.046874999999999);
#355=TOROIDAL_SURFACE('',#34652,2.703125,0.046874999999999);
#356=TOROIDAL_SURFACE('',#34655,2.703125,0.046874999999999);
#357=TOROIDAL_SURFACE('',#34658,2.703125,0.046874999999999);
#358=TOROIDAL_SURFACE('',#34661,2.703125,0.046874999999999);
#359=TOROIDAL_SURFACE('',#34664,2.703125,0.046874999999999);
#360=TOROIDAL_SURFACE('',#34667,2.703125,0.046874999999999);
#361=TOROIDAL_SURFACE('',#34670,2.703125,0.046874999999999);
#362=TOROIDAL_SURFACE('',#34673,2.703125,0.046874999999999);
#363=TOROIDAL_SURFACE('',#34676,2.703125,0.046874999999999);
#364=TOROIDAL_SURFACE('',#34679,2.703125,0.046874999999999);
#365=TOROIDAL_SURFACE('',#34682,2.703125,0.046874999999999);
#366=TOROIDAL_SURFACE('',#34685,2.703125,0.046874999999999);
#367=TOROIDAL_SURFACE('',#34688,2.703125,0.046874999999999);
#368=TOROIDAL_SURFACE('',#34691,2.703125,0.046874999999999);
#369=TOROIDAL_SURFACE('',#34694,2.703125,0.046874999999999);
#370=TOROIDAL_SURFACE('',#34697,2.703125,0.046874999999999);
#371=TOROIDAL_SURFACE('',#34700,2.703125,0.046874999999999);
#372=TOROIDAL_SURFACE('',#34703,2.703125,0.046874999999999);
#373=TOROIDAL_SURFACE('',#34706,2.703125,0.046874999999999);
#374=TOROIDAL_SURFACE('',#34709,2.703125,0.046874999999999);
#375=TOROIDAL_SURFACE('',#34714,2.703125,0.0468750000000018);
#376=TOROIDAL_SURFACE('',#34720,2.703125,0.046874999999999);
#377=TOROIDAL_SURFACE('',#35074,2.58058373926377,0.0468749999999982);
#378=TOROIDAL_SURFACE('',#35370,2.721875,0.0468749999999996);
#379=TOROIDAL_SURFACE('',#35375,2.60625,0.0687500000000002);
#380=TOROIDAL_SURFACE('',#35378,1.65,0.15);
#381=TOROIDAL_SURFACE('',#35381,2.703125,0.0468750000000018);
#382=TOROIDAL_SURFACE('',#35385,2.703125,0.0468750000000018);
#383=TOROIDAL_SURFACE('',#35389,2.703125,0.0468750000000018);
#384=TOROIDAL_SURFACE('',#35393,2.703125,0.0468750000000018);
#385=TOROIDAL_SURFACE('',#35397,2.703125,0.0468750000000018);
#386=TOROIDAL_SURFACE('',#35401,2.703125,0.0468750000000018);
#387=TOROIDAL_SURFACE('',#35405,2.703125,0.0468750000000018);
#388=TOROIDAL_SURFACE('',#35409,2.703125,0.0468750000000018);
#389=TOROIDAL_SURFACE('',#35413,2.703125,0.0468750000000018);
#390=TOROIDAL_SURFACE('',#35417,2.703125,0.0468750000000018);
#391=TOROIDAL_SURFACE('',#35421,2.703125,0.0468750000000018);
#392=TOROIDAL_SURFACE('',#35425,2.703125,0.0468750000000018);
#393=TOROIDAL_SURFACE('',#35429,2.703125,0.0468750000000018);
#394=TOROIDAL_SURFACE('',#35433,2.703125,0.0468750000000018);
#395=TOROIDAL_SURFACE('',#35437,2.703125,0.0468750000000018);
#396=TOROIDAL_SURFACE('',#35441,2.703125,0.0468750000000018);
#397=TOROIDAL_SURFACE('',#35445,2.703125,0.0468750000000018);
#398=TOROIDAL_SURFACE('',#35449,2.703125,0.0468750000000018);
#399=TOROIDAL_SURFACE('',#35453,2.703125,0.0468750000000018);
#400=TOROIDAL_SURFACE('',#35457,2.703125,0.0468750000000018);
#401=TOROIDAL_SURFACE('',#35461,2.703125,0.0468750000000018);
#402=TOROIDAL_SURFACE('',#35465,2.703125,0.0468750000000018);
#403=TOROIDAL_SURFACE('',#35469,2.703125,0.0468750000000018);
#404=TOROIDAL_SURFACE('',#35473,2.703125,0.0468750000000018);
#405=TOROIDAL_SURFACE('',#35477,2.703125,0.0468750000000018);
#406=TOROIDAL_SURFACE('',#35481,2.703125,0.0468750000000018);
#407=TOROIDAL_SURFACE('',#35485,2.703125,0.0468750000000018);
#408=TOROIDAL_SURFACE('',#35489,2.703125,0.0468750000000018);
#409=TOROIDAL_SURFACE('',#35493,2.703125,0.0468750000000018);
#410=TOROIDAL_SURFACE('',#35497,2.703125,0.0468750000000018);
#411=TOROIDAL_SURFACE('',#35501,2.703125,0.0468750000000018);
#412=TOROIDAL_SURFACE('',#35505,2.703125,0.0468750000000018);
#413=TOROIDAL_SURFACE('',#35509,2.703125,0.0468750000000018);
#414=TOROIDAL_SURFACE('',#35513,2.703125,0.0468750000000018);
#415=TOROIDAL_SURFACE('',#35517,2.703125,0.0468750000000018);
#416=TOROIDAL_SURFACE('',#35521,2.703125,0.0468750000000018);
#417=TOROIDAL_SURFACE('',#35525,2.703125,0.0468750000000018);
#418=TOROIDAL_SURFACE('',#35529,2.703125,0.0468750000000018);
#419=TOROIDAL_SURFACE('',#35533,2.703125,0.0468750000000018);
#420=TOROIDAL_SURFACE('',#35537,2.703125,0.0468750000000018);
#421=TOROIDAL_SURFACE('',#35541,2.703125,0.0468750000000018);
#422=TOROIDAL_SURFACE('',#35545,2.703125,0.0468750000000018);
#423=TOROIDAL_SURFACE('',#35549,2.703125,0.0468750000000018);
#424=TOROIDAL_SURFACE('',#35553,2.703125,0.0468750000000018);
#425=TOROIDAL_SURFACE('',#35557,2.703125,0.0468750000000018);
#426=TOROIDAL_SURFACE('',#35561,2.703125,0.0468750000000018);
#427=TOROIDAL_SURFACE('',#35565,2.703125,0.0468750000000018);
#428=TOROIDAL_SURFACE('',#35569,2.703125,0.0468750000000018);
#429=TOROIDAL_SURFACE('',#35573,2.703125,0.0468750000000018);
#430=TOROIDAL_SURFACE('',#35577,2.703125,0.0468750000000018);
#431=TOROIDAL_SURFACE('',#35581,2.703125,0.0468750000000018);
#432=TOROIDAL_SURFACE('',#35585,2.703125,0.0468750000000018);
#433=TOROIDAL_SURFACE('',#35589,2.703125,0.0468750000000018);
#434=TOROIDAL_SURFACE('',#35593,2.703125,0.0468750000000018);
#435=TOROIDAL_SURFACE('',#35597,2.703125,0.0468750000000018);
#436=TOROIDAL_SURFACE('',#35601,2.703125,0.0468750000000018);
#437=TOROIDAL_SURFACE('',#35605,2.703125,0.0468750000000018);
#438=TOROIDAL_SURFACE('',#35609,2.703125,0.0468750000000018);
#439=TOROIDAL_SURFACE('',#35613,2.703125,0.0468750000000018);
#440=TOROIDAL_SURFACE('',#35617,2.703125,0.0468750000000018);
#441=TOROIDAL_SURFACE('',#35621,2.703125,0.0468750000000018);
#442=TOROIDAL_SURFACE('',#35625,2.703125,0.0468750000000018);
#443=TOROIDAL_SURFACE('',#35629,2.703125,0.0468750000000018);
#444=TOROIDAL_SURFACE('',#35633,2.703125,0.0468750000000018);
#445=TOROIDAL_SURFACE('',#35637,2.703125,0.0468750000000018);
#446=TOROIDAL_SURFACE('',#35641,2.703125,0.0468750000000018);
#447=TOROIDAL_SURFACE('',#35645,2.703125,0.0468750000000018);
#448=TOROIDAL_SURFACE('',#35649,2.703125,0.0468750000000018);
#449=TOROIDAL_SURFACE('',#35653,2.703125,0.0468750000000018);
#450=TOROIDAL_SURFACE('',#35657,2.703125,0.0468750000000018);
#451=TOROIDAL_SURFACE('',#35661,2.703125,0.0468750000000018);
#452=TOROIDAL_SURFACE('',#35665,2.703125,0.0468750000000018);
#453=TOROIDAL_SURFACE('',#35669,2.703125,0.0468750000000018);
#454=TOROIDAL_SURFACE('',#35673,2.703125,0.0468750000000018);
#455=TOROIDAL_SURFACE('',#35677,2.703125,0.0468750000000018);
#456=TOROIDAL_SURFACE('',#35681,2.703125,0.0468750000000018);
#457=TOROIDAL_SURFACE('',#35685,2.703125,0.0468750000000018);
#458=TOROIDAL_SURFACE('',#35689,2.703125,0.0468750000000018);
#459=TOROIDAL_SURFACE('',#35693,2.703125,0.0468750000000018);
#460=TOROIDAL_SURFACE('',#35855,2.703125,0.046874999999999);
#461=TOROIDAL_SURFACE('',#35858,2.703125,0.046874999999999);
#462=TOROIDAL_SURFACE('',#35861,2.703125,0.046874999999999);
#463=TOROIDAL_SURFACE('',#35864,2.703125,0.046874999999999);
#464=TOROIDAL_SURFACE('',#35867,2.703125,0.046874999999999);
#465=TOROIDAL_SURFACE('',#35870,2.703125,0.046874999999999);
#466=TOROIDAL_SURFACE('',#35873,2.703125,0.046874999999999);
#467=TOROIDAL_SURFACE('',#35876,2.703125,0.046874999999999);
#468=TOROIDAL_SURFACE('',#35879,2.703125,0.046874999999999);
#469=TOROIDAL_SURFACE('',#35882,2.703125,0.046874999999999);
#470=TOROIDAL_SURFACE('',#35885,2.703125,0.046874999999999);
#471=TOROIDAL_SURFACE('',#35888,2.703125,0.046874999999999);
#472=TOROIDAL_SURFACE('',#35891,2.703125,0.046874999999999);
#473=TOROIDAL_SURFACE('',#35894,2.703125,0.046874999999999);
#474=TOROIDAL_SURFACE('',#35897,2.703125,0.046874999999999);
#475=TOROIDAL_SURFACE('',#35900,2.703125,0.046874999999999);
#476=TOROIDAL_SURFACE('',#35903,2.703125,0.046874999999999);
#477=TOROIDAL_SURFACE('',#35906,2.703125,0.046874999999999);
#478=TOROIDAL_SURFACE('',#35909,2.703125,0.046874999999999);
#479=TOROIDAL_SURFACE('',#35912,2.703125,0.046874999999999);
#480=TOROIDAL_SURFACE('',#35915,2.703125,0.046874999999999);
#481=TOROIDAL_SURFACE('',#35918,2.703125,0.046874999999999);
#482=TOROIDAL_SURFACE('',#35921,2.703125,0.046874999999999);
#483=TOROIDAL_SURFACE('',#35924,2.703125,0.046874999999999);
#484=TOROIDAL_SURFACE('',#35927,2.703125,0.046874999999999);
#485=TOROIDAL_SURFACE('',#35930,2.703125,0.046874999999999);
#486=TOROIDAL_SURFACE('',#35933,2.703125,0.046874999999999);
#487=TOROIDAL_SURFACE('',#35936,2.703125,0.046874999999999);
#488=TOROIDAL_SURFACE('',#35939,2.703125,0.046874999999999);
#489=TOROIDAL_SURFACE('',#35942,2.703125,0.046874999999999);
#490=TOROIDAL_SURFACE('',#35945,2.703125,0.046874999999999);
#491=TOROIDAL_SURFACE('',#35948,2.703125,0.046874999999999);
#492=TOROIDAL_SURFACE('',#35951,2.703125,0.046874999999999);
#493=TOROIDAL_SURFACE('',#35954,2.703125,0.046874999999999);
#494=TOROIDAL_SURFACE('',#35957,2.703125,0.046874999999999);
#495=TOROIDAL_SURFACE('',#35960,2.703125,0.046874999999999);
#496=TOROIDAL_SURFACE('',#35963,2.703125,0.046874999999999);
#497=TOROIDAL_SURFACE('',#35966,2.703125,0.046874999999999);
#498=TOROIDAL_SURFACE('',#35969,2.703125,0.046874999999999);
#499=TOROIDAL_SURFACE('',#35972,2.703125,0.046874999999999);
#500=TOROIDAL_SURFACE('',#35975,2.703125,0.046874999999999);
#501=TOROIDAL_SURFACE('',#35978,2.703125,0.046874999999999);
#502=TOROIDAL_SURFACE('',#35981,2.703125,0.046874999999999);
#503=TOROIDAL_SURFACE('',#35984,2.703125,0.046874999999999);
#504=TOROIDAL_SURFACE('',#35987,2.703125,0.046874999999999);
#505=TOROIDAL_SURFACE('',#35990,2.703125,0.046874999999999);
#506=TOROIDAL_SURFACE('',#35993,2.703125,0.046874999999999);
#507=TOROIDAL_SURFACE('',#35996,2.703125,0.046874999999999);
#508=TOROIDAL_SURFACE('',#35999,2.703125,0.046874999999999);
#509=TOROIDAL_SURFACE('',#36002,2.703125,0.046874999999999);
#510=TOROIDAL_SURFACE('',#36005,2.703125,0.046874999999999);
#511=TOROIDAL_SURFACE('',#36008,2.703125,0.046874999999999);
#512=TOROIDAL_SURFACE('',#36011,2.703125,0.046874999999999);
#513=TOROIDAL_SURFACE('',#36014,2.703125,0.046874999999999);
#514=TOROIDAL_SURFACE('',#36017,2.703125,0.046874999999999);
#515=TOROIDAL_SURFACE('',#36020,2.703125,0.046874999999999);
#516=TOROIDAL_SURFACE('',#36023,2.703125,0.046874999999999);
#517=TOROIDAL_SURFACE('',#36026,2.703125,0.046874999999999);
#518=TOROIDAL_SURFACE('',#36029,2.703125,0.046874999999999);
#519=TOROIDAL_SURFACE('',#36032,2.703125,0.046874999999999);
#520=TOROIDAL_SURFACE('',#36035,2.703125,0.046874999999999);
#521=TOROIDAL_SURFACE('',#36038,2.703125,0.046874999999999);
#522=TOROIDAL_SURFACE('',#36041,2.703125,0.046874999999999);
#523=TOROIDAL_SURFACE('',#36044,2.703125,0.046874999999999);
#524=TOROIDAL_SURFACE('',#36047,2.703125,0.046874999999999);
#525=TOROIDAL_SURFACE('',#36050,2.703125,0.046874999999999);
#526=TOROIDAL_SURFACE('',#36053,2.703125,0.046874999999999);
#527=TOROIDAL_SURFACE('',#36056,2.703125,0.046874999999999);
#528=TOROIDAL_SURFACE('',#36059,2.703125,0.046874999999999);
#529=TOROIDAL_SURFACE('',#36062,2.703125,0.046874999999999);
#530=TOROIDAL_SURFACE('',#36065,2.703125,0.046874999999999);
#531=TOROIDAL_SURFACE('',#36068,2.703125,0.046874999999999);
#532=TOROIDAL_SURFACE('',#36071,2.703125,0.046874999999999);
#533=TOROIDAL_SURFACE('',#36074,2.703125,0.046874999999999);
#534=TOROIDAL_SURFACE('',#36077,2.703125,0.046874999999999);
#535=TOROIDAL_SURFACE('',#36080,2.703125,0.046874999999999);
#536=TOROIDAL_SURFACE('',#36083,2.703125,0.046874999999999);
#537=TOROIDAL_SURFACE('',#36086,2.703125,0.046874999999999);
#538=TOROIDAL_SURFACE('',#36089,2.703125,0.046874999999999);
#539=TOROIDAL_SURFACE('',#36094,2.703125,0.0468750000000018);
#540=TOROIDAL_SURFACE('',#36100,2.703125,0.046874999999999);
#541=(
BOUNDED_CURVE()
B_SPLINE_CURVE(2,(#50905,#50906,#50907),.UNSPECIFIED.,.F.,.F.)
B_SPLINE_CURVE_WITH_KNOTS((3,3),(-0.375752880509706,-0.25773139970398),
 .UNSPECIFIED.)
CURVE()
GEOMETRIC_REPRESENTATION_ITEM()
RATIONAL_B_SPLINE_CURVE((1.41147367097488,1.52065153937885,1.52065153937885))
REPRESENTATION_ITEM('')
);
#542=(
BOUNDED_CURVE()
B_SPLINE_CURVE(2,(#50909,#50910,#50911),.UNSPECIFIED.,.F.,.F.)
B_SPLINE_CURVE_WITH_KNOTS((3,3),(-0.375752880509709,-0.139709918898254),
 .UNSPECIFIED.)
CURVE()
GEOMETRIC_REPRESENTATION_ITEM()
RATIONAL_B_SPLINE_CURVE((1.41147367097488,1.62982940778282,1.41147367097488))
REPRESENTATION_ITEM('')
);
#543=(
BOUNDED_CURVE()
B_SPLINE_CURVE(2,(#50913,#50914,#50915),.UNSPECIFIED.,.F.,.F.)
B_SPLINE_CURVE_WITH_KNOTS((3,3),(-0.375752880509709,-0.139709918898254),
 .UNSPECIFIED.)
CURVE()
GEOMETRIC_REPRESENTATION_ITEM()
RATIONAL_B_SPLINE_CURVE((1.41147367097488,1.62982940778282,1.41147367097488))
REPRESENTATION_ITEM('')
);
#544=(
BOUNDED_CURVE()
B_SPLINE_CURVE(2,(#50917,#50918,#50919),.UNSPECIFIED.,.F.,.F.)
B_SPLINE_CURVE_WITH_KNOTS((3,3),(-0.375752880509708,-0.139709918898254),
 .UNSPECIFIED.)
CURVE()
GEOMETRIC_REPRESENTATION_ITEM()
RATIONAL_B_SPLINE_CURVE((1.41147367097487,1.62982940778281,1.41147367097487))
REPRESENTATION_ITEM('')
);
#545=(
BOUNDED_CURVE()
B_SPLINE_CURVE(2,(#50921,#50922,#50923),.UNSPECIFIED.,.F.,.F.)
B_SPLINE_CURVE_WITH_KNOTS((3,3),(-0.375752880509709,-0.139709918898253),
 .UNSPECIFIED.)
CURVE()
GEOMETRIC_REPRESENTATION_ITEM()
RATIONAL_B_SPLINE_CURVE((1.41147367097488,1.62982940778282,1.41147367097488))
REPRESENTATION_ITEM('')
);
#546=(
BOUNDED_CURVE()
B_SPLINE_CURVE(2,(#50925,#50926,#50927),.UNSPECIFIED.,.F.,.F.)
B_SPLINE_CURVE_WITH_KNOTS((3,3),(-0.375752880509709,-0.139709918898254),
 .UNSPECIFIED.)
CURVE()
GEOMETRIC_REPRESENTATION_ITEM()
RATIONAL_B_SPLINE_CURVE((1.41147367097488,1.62982940778282,1.41147367097488))
REPRESENTATION_ITEM('')
);
#547=(
BOUNDED_CURVE()
B_SPLINE_CURVE(2,(#50928,#50929,#50930),.UNSPECIFIED.,.F.,.F.)
B_SPLINE_CURVE_WITH_KNOTS((3,3),(-0.25773139970398,-0.139709918898256),
 .UNSPECIFIED.)
CURVE()
GEOMETRIC_REPRESENTATION_ITEM()
RATIONAL_B_SPLINE_CURVE((1.52065153937885,1.52065153937885,1.41147367097488))
REPRESENTATION_ITEM('')
);
#548=(
BOUNDED_CURVE()
B_SPLINE_CURVE(2,(#50952,#50953,#50954),.UNSPECIFIED.,.F.,.F.)
B_SPLINE_CURVE_WITH_KNOTS((3,3),(0.367644516946548,0.373830527582523),
 .UNSPECIFIED.)
CURVE()
GEOMETRIC_REPRESENTATION_ITEM()
RATIONAL_B_SPLINE_CURVE((1.13426390111316,1.13389822901309,1.13348223894575))
REPRESENTATION_ITEM('')
);
#549=(
BOUNDED_CURVE()
B_SPLINE_CURVE(2,(#50958,#50959,#50960),.UNSPECIFIED.,.F.,.F.)
B_SPLINE_CURVE_WITH_KNOTS((3,3),(0.271548216895916,0.277734227531904),
 .UNSPECIFIED.)
CURVE()
GEOMETRIC_REPRESENTATION_ITEM()
RATIONAL_B_SPLINE_CURVE((1.13348223894615,1.1338982290135,1.13426390111357))
REPRESENTATION_ITEM('')
);
#550=(
BOUNDED_CURVE()
B_SPLINE_CURVE(2,(#50964,#50965,#50966),.UNSPECIFIED.,.F.,.F.)
B_SPLINE_CURVE_WITH_KNOTS((3,3),(0.36764451694656,0.373830527582529),
 .UNSPECIFIED.)
CURVE()
GEOMETRIC_REPRESENTATION_ITEM()
RATIONAL_B_SPLINE_CURVE((1.13426390111306,1.13389822901299,1.13348223894565))
REPRESENTATION_ITEM('')
);
#551=(
BOUNDED_CURVE()
B_SPLINE_CURVE(2,(#50970,#50971,#50972),.UNSPECIFIED.,.F.,.F.)
B_SPLINE_CURVE_WITH_KNOTS((3,3),(0.271548216895914,0.277734227531901),
 .UNSPECIFIED.)
CURVE()
GEOMETRIC_REPRESENTATION_ITEM()
RATIONAL_B_SPLINE_CURVE((1.13348223894612,1.13389822901347,1.13426390111354))
REPRESENTATION_ITEM('')
);
#552=(
BOUNDED_CURVE()
B_SPLINE_CURVE(2,(#50976,#50977,#50978),.UNSPECIFIED.,.F.,.F.)
B_SPLINE_CURVE_WITH_KNOTS((3,3),(0.367644516946562,0.373830527582532),
 .UNSPECIFIED.)
CURVE()
GEOMETRIC_REPRESENTATION_ITEM()
RATIONAL_B_SPLINE_CURVE((1.13426390111304,1.13389822901297,1.13348223894563))
REPRESENTATION_ITEM('')
);
#553=(
BOUNDED_CURVE()
B_SPLINE_CURVE(2,(#50982,#50983,#50984),.UNSPECIFIED.,.F.,.F.)
B_SPLINE_CURVE_WITH_KNOTS((3,3),(0.27154821689591,0.277734227531895),
 .UNSPECIFIED.)
CURVE()
GEOMETRIC_REPRESENTATION_ITEM()
RATIONAL_B_SPLINE_CURVE((1.13348223894613,1.13389822901348,1.13426390111355))
REPRESENTATION_ITEM('')
);
#554=(
BOUNDED_CURVE()
B_SPLINE_CURVE(2,(#50988,#50989,#50990),.UNSPECIFIED.,.F.,.F.)
B_SPLINE_CURVE_WITH_KNOTS((3,3),(0.367644516946554,0.373830527582529),
 .UNSPECIFIED.)
CURVE()
GEOMETRIC_REPRESENTATION_ITEM()
RATIONAL_B_SPLINE_CURVE((1.13426390111305,1.13389822901299,1.13348223894564))
REPRESENTATION_ITEM('')
);
#555=(
BOUNDED_CURVE()
B_SPLINE_CURVE(2,(#50994,#50995,#50996),.UNSPECIFIED.,.F.,.F.)
B_SPLINE_CURVE_WITH_KNOTS((3,3),(0.271548216895907,0.277734227531893),
 .UNSPECIFIED.)
CURVE()
GEOMETRIC_REPRESENTATION_ITEM()
RATIONAL_B_SPLINE_CURVE((1.13348223894611,1.13389822901346,1.13426390111353))
REPRESENTATION_ITEM('')
);
#556=(
BOUNDED_CURVE()
B_SPLINE_CURVE(2,(#51000,#51001,#51002),.UNSPECIFIED.,.F.,.F.)
B_SPLINE_CURVE_WITH_KNOTS((3,3),(0.367644516946562,0.373830527582532),
 .UNSPECIFIED.)
CURVE()
GEOMETRIC_REPRESENTATION_ITEM()
RATIONAL_B_SPLINE_CURVE((1.13426390111302,1.13389822901296,1.13348223894561))
REPRESENTATION_ITEM('')
);
#557=(
BOUNDED_CURVE()
B_SPLINE_CURVE(2,(#51006,#51007,#51008),.UNSPECIFIED.,.F.,.F.)
B_SPLINE_CURVE_WITH_KNOTS((3,3),(0.271548216895914,0.277734227531899),
 .UNSPECIFIED.)
CURVE()
GEOMETRIC_REPRESENTATION_ITEM()
RATIONAL_B_SPLINE_CURVE((1.13348223894609,1.13389822901344,1.13426390111351))
REPRESENTATION_ITEM('')
);
#558=(
BOUNDED_CURVE()
B_SPLINE_CURVE(2,(#51012,#51013,#51014),.UNSPECIFIED.,.F.,.F.)
B_SPLINE_CURVE_WITH_KNOTS((3,3),(0.36764451694656,0.373830527582535),
 .UNSPECIFIED.)
CURVE()
GEOMETRIC_REPRESENTATION_ITEM()
RATIONAL_B_SPLINE_CURVE((1.13426390111302,1.13389822901295,1.1334822389456))
REPRESENTATION_ITEM('')
);
#559=(
BOUNDED_CURVE()
B_SPLINE_CURVE(2,(#51018,#51019,#51020),.UNSPECIFIED.,.F.,.F.)
B_SPLINE_CURVE_WITH_KNOTS((3,3),(0.271548216895908,0.277734227531894),
 .UNSPECIFIED.)
CURVE()
GEOMETRIC_REPRESENTATION_ITEM()
RATIONAL_B_SPLINE_CURVE((1.1334822389461,1.13389822901345,1.13426390111352))
REPRESENTATION_ITEM('')
);
#560=(
BOUNDED_CURVE()
B_SPLINE_CURVE(2,(#51024,#51025,#51026),.UNSPECIFIED.,.F.,.F.)
B_SPLINE_CURVE_WITH_KNOTS((3,3),(0.367644516946558,0.373830527582536),
 .UNSPECIFIED.)
CURVE()
GEOMETRIC_REPRESENTATION_ITEM()
RATIONAL_B_SPLINE_CURVE((1.13426390111302,1.13389822901295,1.13348223894561))
REPRESENTATION_ITEM('')
);
#561=(
BOUNDED_CURVE()
B_SPLINE_CURVE(2,(#51030,#51031,#51032),.UNSPECIFIED.,.F.,.F.)
B_SPLINE_CURVE_WITH_KNOTS((3,3),(0.271548216895914,0.277734227531899),
 .UNSPECIFIED.)
CURVE()
GEOMETRIC_REPRESENTATION_ITEM()
RATIONAL_B_SPLINE_CURVE((1.13348223894613,1.13389822901348,1.13426390111355))
REPRESENTATION_ITEM('')
);
#562=(
BOUNDED_CURVE()
B_SPLINE_CURVE(2,(#51036,#51037,#51038),.UNSPECIFIED.,.F.,.F.)
B_SPLINE_CURVE_WITH_KNOTS((3,3),(0.367644516946564,0.373830527582534),
 .UNSPECIFIED.)
CURVE()
GEOMETRIC_REPRESENTATION_ITEM()
RATIONAL_B_SPLINE_CURVE((1.13426390111303,1.13389822901296,1.13348223894561))
REPRESENTATION_ITEM('')
);
#563=(
BOUNDED_CURVE()
B_SPLINE_CURVE(2,(#51042,#51043,#51044),.UNSPECIFIED.,.F.,.F.)
B_SPLINE_CURVE_WITH_KNOTS((3,3),(0.271548216895916,0.277734227531901),
 .UNSPECIFIED.)
CURVE()
GEOMETRIC_REPRESENTATION_ITEM()
RATIONAL_B_SPLINE_CURVE((1.13348223894614,1.13389822901349,1.13426390111357))
REPRESENTATION_ITEM('')
);
#564=(
BOUNDED_CURVE()
B_SPLINE_CURVE(2,(#51048,#51049,#51050),.UNSPECIFIED.,.F.,.F.)
B_SPLINE_CURVE_WITH_KNOTS((3,3),(0.367644516946554,0.373830527582527),
 .UNSPECIFIED.)
CURVE()
GEOMETRIC_REPRESENTATION_ITEM()
RATIONAL_B_SPLINE_CURVE((1.13426390111312,1.13389822901305,1.13348223894571))
REPRESENTATION_ITEM('')
);
#565=(
BOUNDED_CURVE()
B_SPLINE_CURVE(2,(#51054,#51055,#51056),.UNSPECIFIED.,.F.,.F.)
B_SPLINE_CURVE_WITH_KNOTS((3,3),(0.271548216895913,0.2777342275319),
 .UNSPECIFIED.)
CURVE()
GEOMETRIC_REPRESENTATION_ITEM()
RATIONAL_B_SPLINE_CURVE((1.13348223894615,1.1338982290135,1.13426390111358))
REPRESENTATION_ITEM('')
);
#566=(
BOUNDED_CURVE()
B_SPLINE_CURVE(2,(#51060,#51061,#51062),.UNSPECIFIED.,.F.,.F.)
B_SPLINE_CURVE_WITH_KNOTS((3,3),(0.367644516946564,0.373830527582538),
 .UNSPECIFIED.)
CURVE()
GEOMETRIC_REPRESENTATION_ITEM()
RATIONAL_B_SPLINE_CURVE((1.134263901113,1.13389822901293,1.13348223894559))
REPRESENTATION_ITEM('')
);
#567=(
BOUNDED_CURVE()
B_SPLINE_CURVE(2,(#51066,#51067,#51068),.UNSPECIFIED.,.F.,.F.)
B_SPLINE_CURVE_WITH_KNOTS((3,3),(0.271548216895908,0.277734227531895),
 .UNSPECIFIED.)
CURVE()
GEOMETRIC_REPRESENTATION_ITEM()
RATIONAL_B_SPLINE_CURVE((1.13348223894615,1.1338982290135,1.13426390111358))
REPRESENTATION_ITEM('')
);
#568=(
BOUNDED_CURVE()
B_SPLINE_CURVE(2,(#51072,#51073,#51074),.UNSPECIFIED.,.F.,.F.)
B_SPLINE_CURVE_WITH_KNOTS((3,3),(0.367644516946561,0.373830527582532),
 .UNSPECIFIED.)
CURVE()
GEOMETRIC_REPRESENTATION_ITEM()
RATIONAL_B_SPLINE_CURVE((1.13426390111309,1.13389822901302,1.13348223894568))
REPRESENTATION_ITEM('')
);
#569=(
BOUNDED_CURVE()
B_SPLINE_CURVE(2,(#51078,#51079,#51080),.UNSPECIFIED.,.F.,.F.)
B_SPLINE_CURVE_WITH_KNOTS((3,3),(0.271548216895921,0.277734227531907),
 .UNSPECIFIED.)
CURVE()
GEOMETRIC_REPRESENTATION_ITEM()
RATIONAL_B_SPLINE_CURVE((1.13348223894616,1.13389822901351,1.13426390111358))
REPRESENTATION_ITEM('')
);
#570=(
BOUNDED_CURVE()
B_SPLINE_CURVE(2,(#51084,#51085,#51086),.UNSPECIFIED.,.F.,.F.)
B_SPLINE_CURVE_WITH_KNOTS((3,3),(0.367644516946558,0.373830527582535),
 .UNSPECIFIED.)
CURVE()
GEOMETRIC_REPRESENTATION_ITEM()
RATIONAL_B_SPLINE_CURVE((1.13426390111305,1.13389822901298,1.13348223894564))
REPRESENTATION_ITEM('')
);
#571=(
BOUNDED_CURVE()
B_SPLINE_CURVE(2,(#51090,#51091,#51092),.UNSPECIFIED.,.F.,.F.)
B_SPLINE_CURVE_WITH_KNOTS((3,3),(0.271548216895908,0.27773422753189),
 .UNSPECIFIED.)
CURVE()
GEOMETRIC_REPRESENTATION_ITEM()
RATIONAL_B_SPLINE_CURVE((1.13348223894616,1.13389822901351,1.13426390111359))
REPRESENTATION_ITEM('')
);
#572=(
BOUNDED_CURVE()
B_SPLINE_CURVE(2,(#51096,#51097,#51098),.UNSPECIFIED.,.F.,.F.)
B_SPLINE_CURVE_WITH_KNOTS((3,3),(0.367644516946548,0.373830527582523),
 .UNSPECIFIED.)
CURVE()
GEOMETRIC_REPRESENTATION_ITEM()
RATIONAL_B_SPLINE_CURVE((1.13426390111314,1.13389822901308,1.13348223894573))
REPRESENTATION_ITEM('')
);
#573=(
BOUNDED_CURVE()
B_SPLINE_CURVE(2,(#51102,#51103,#51104),.UNSPECIFIED.,.F.,.F.)
B_SPLINE_CURVE_WITH_KNOTS((3,3),(0.271548216895905,0.277734227531892),
 .UNSPECIFIED.)
CURVE()
GEOMETRIC_REPRESENTATION_ITEM()
RATIONAL_B_SPLINE_CURVE((1.13348223894608,1.13389822901343,1.1342639011135))
REPRESENTATION_ITEM('')
);
#574=(
BOUNDED_CURVE()
B_SPLINE_CURVE(2,(#51108,#51109,#51110),.UNSPECIFIED.,.F.,.F.)
B_SPLINE_CURVE_WITH_KNOTS((3,3),(0.36764451694655,0.373830527582528),
 .UNSPECIFIED.)
CURVE()
GEOMETRIC_REPRESENTATION_ITEM()
RATIONAL_B_SPLINE_CURVE((1.1342639011131,1.13389822901304,1.13348223894569))
REPRESENTATION_ITEM('')
);
#575=(
BOUNDED_CURVE()
B_SPLINE_CURVE(2,(#51114,#51115,#51116),.UNSPECIFIED.,.F.,.F.)
B_SPLINE_CURVE_WITH_KNOTS((3,3),(0.27154821689591,0.277734227531895),
 .UNSPECIFIED.)
CURVE()
GEOMETRIC_REPRESENTATION_ITEM()
RATIONAL_B_SPLINE_CURVE((1.13348223894612,1.13389822901347,1.13426390111354))
REPRESENTATION_ITEM('')
);
#576=(
BOUNDED_CURVE()
B_SPLINE_CURVE(2,(#51120,#51121,#51122),.UNSPECIFIED.,.F.,.F.)
B_SPLINE_CURVE_WITH_KNOTS((3,3),(0.367644516946551,0.373830527582525),
 .UNSPECIFIED.)
CURVE()
GEOMETRIC_REPRESENTATION_ITEM()
RATIONAL_B_SPLINE_CURVE((1.13426390111313,1.13389822901307,1.13348223894572))
REPRESENTATION_ITEM('')
);
#577=(
BOUNDED_CURVE()
B_SPLINE_CURVE(2,(#51126,#51127,#51128),.UNSPECIFIED.,.F.,.F.)
B_SPLINE_CURVE_WITH_KNOTS((3,3),(0.271548216895914,0.277734227531894),
 .UNSPECIFIED.)
CURVE()
GEOMETRIC_REPRESENTATION_ITEM()
RATIONAL_B_SPLINE_CURVE((1.13348223894619,1.13389822901354,1.13426390111361))
REPRESENTATION_ITEM('')
);
#578=(
BOUNDED_CURVE()
B_SPLINE_CURVE(2,(#51132,#51133,#51134),.UNSPECIFIED.,.F.,.F.)
B_SPLINE_CURVE_WITH_KNOTS((3,3),(0.367644516946565,0.373830527582531),
 .UNSPECIFIED.)
CURVE()
GEOMETRIC_REPRESENTATION_ITEM()
RATIONAL_B_SPLINE_CURVE((1.134263901113,1.13389822901293,1.13348223894559))
REPRESENTATION_ITEM('')
);
#579=(
BOUNDED_CURVE()
B_SPLINE_CURVE(2,(#51138,#51139,#51140),.UNSPECIFIED.,.F.,.F.)
B_SPLINE_CURVE_WITH_KNOTS((3,3),(0.271548216895912,0.277734227531896),
 .UNSPECIFIED.)
CURVE()
GEOMETRIC_REPRESENTATION_ITEM()
RATIONAL_B_SPLINE_CURVE((1.13348223894612,1.13389822901347,1.13426390111354))
REPRESENTATION_ITEM('')
);
#580=(
BOUNDED_CURVE()
B_SPLINE_CURVE(2,(#51144,#51145,#51146),.UNSPECIFIED.,.F.,.F.)
B_SPLINE_CURVE_WITH_KNOTS((3,3),(0.367644516946563,0.373830527582537),
 .UNSPECIFIED.)
CURVE()
GEOMETRIC_REPRESENTATION_ITEM()
RATIONAL_B_SPLINE_CURVE((1.13426390111305,1.13389822901298,1.13348223894564))
REPRESENTATION_ITEM('')
);
#581=(
BOUNDED_CURVE()
B_SPLINE_CURVE(2,(#51150,#51151,#51152),.UNSPECIFIED.,.F.,.F.)
B_SPLINE_CURVE_WITH_KNOTS((3,3),(0.271548216895909,0.277734227531891),
 .UNSPECIFIED.)
CURVE()
GEOMETRIC_REPRESENTATION_ITEM()
RATIONAL_B_SPLINE_CURVE((1.13348223894604,1.13389822901339,1.13426390111346))
REPRESENTATION_ITEM('')
);
#582=(
BOUNDED_CURVE()
B_SPLINE_CURVE(2,(#51156,#51157,#51158),.UNSPECIFIED.,.F.,.F.)
B_SPLINE_CURVE_WITH_KNOTS((3,3),(0.367644516946552,0.373830527582532),
 .UNSPECIFIED.)
CURVE()
GEOMETRIC_REPRESENTATION_ITEM()
RATIONAL_B_SPLINE_CURVE((1.13426390111305,1.13389822901299,1.13348223894564))
REPRESENTATION_ITEM('')
);
#583=(
BOUNDED_CURVE()
B_SPLINE_CURVE(2,(#51162,#51163,#51164),.UNSPECIFIED.,.F.,.F.)
B_SPLINE_CURVE_WITH_KNOTS((3,3),(0.271548216895916,0.277734227531902),
 .UNSPECIFIED.)
CURVE()
GEOMETRIC_REPRESENTATION_ITEM()
RATIONAL_B_SPLINE_CURVE((1.13348223894616,1.13389822901351,1.13426390111359))
REPRESENTATION_ITEM('')
);
#584=(
BOUNDED_CURVE()
B_SPLINE_CURVE(2,(#51168,#51169,#51170),.UNSPECIFIED.,.F.,.F.)
B_SPLINE_CURVE_WITH_KNOTS((3,3),(0.367644516946562,0.373830527582535),
 .UNSPECIFIED.)
CURVE()
GEOMETRIC_REPRESENTATION_ITEM()
RATIONAL_B_SPLINE_CURVE((1.13426390111309,1.13389822901302,1.13348223894568))
REPRESENTATION_ITEM('')
);
#585=(
BOUNDED_CURVE()
B_SPLINE_CURVE(2,(#51174,#51175,#51176),.UNSPECIFIED.,.F.,.F.)
B_SPLINE_CURVE_WITH_KNOTS((3,3),(0.271548216895913,0.277734227531904),
 .UNSPECIFIED.)
CURVE()
GEOMETRIC_REPRESENTATION_ITEM()
RATIONAL_B_SPLINE_CURVE((1.13348223894619,1.13389822901354,1.13426390111362))
REPRESENTATION_ITEM('')
);
#586=(
BOUNDED_CURVE()
B_SPLINE_CURVE(2,(#51180,#51181,#51182),.UNSPECIFIED.,.F.,.F.)
B_SPLINE_CURVE_WITH_KNOTS((3,3),(0.36764451694655,0.373830527582524),
 .UNSPECIFIED.)
CURVE()
GEOMETRIC_REPRESENTATION_ITEM()
RATIONAL_B_SPLINE_CURVE((1.13426390111312,1.13389822901305,1.13348223894571))
REPRESENTATION_ITEM('')
);
#587=(
BOUNDED_CURVE()
B_SPLINE_CURVE(2,(#51186,#51187,#51188),.UNSPECIFIED.,.F.,.F.)
B_SPLINE_CURVE_WITH_KNOTS((3,3),(0.271548216895921,0.277734227531899),
 .UNSPECIFIED.)
CURVE()
GEOMETRIC_REPRESENTATION_ITEM()
RATIONAL_B_SPLINE_CURVE((1.13348223894619,1.13389822901354,1.13426390111361))
REPRESENTATION_ITEM('')
);
#588=(
BOUNDED_CURVE()
B_SPLINE_CURVE(2,(#51192,#51193,#51194),.UNSPECIFIED.,.F.,.F.)
B_SPLINE_CURVE_WITH_KNOTS((3,3),(0.367644516946559,0.373830527582526),
 .UNSPECIFIED.)
CURVE()
GEOMETRIC_REPRESENTATION_ITEM()
RATIONAL_B_SPLINE_CURVE((1.1342639011131,1.13389822901303,1.13348223894569))
REPRESENTATION_ITEM('')
);
#589=(
BOUNDED_CURVE()
B_SPLINE_CURVE(2,(#51198,#51199,#51200),.UNSPECIFIED.,.F.,.F.)
B_SPLINE_CURVE_WITH_KNOTS((3,3),(0.271548216895914,0.2777342275319),
 .UNSPECIFIED.)
CURVE()
GEOMETRIC_REPRESENTATION_ITEM()
RATIONAL_B_SPLINE_CURVE((1.13348223894616,1.13389822901351,1.13426390111358))
REPRESENTATION_ITEM('')
);
#590=(
BOUNDED_CURVE()
B_SPLINE_CURVE(2,(#51204,#51205,#51206),.UNSPECIFIED.,.F.,.F.)
B_SPLINE_CURVE_WITH_KNOTS((3,3),(0.367644516946557,0.373830527582536),
 .UNSPECIFIED.)
CURVE()
GEOMETRIC_REPRESENTATION_ITEM()
RATIONAL_B_SPLINE_CURVE((1.13426390111309,1.13389822901303,1.13348223894568))
REPRESENTATION_ITEM('')
);
#591=(
BOUNDED_CURVE()
B_SPLINE_CURVE(2,(#51210,#51211,#51212),.UNSPECIFIED.,.F.,.F.)
B_SPLINE_CURVE_WITH_KNOTS((3,3),(0.271548216895912,0.277734227531897),
 .UNSPECIFIED.)
CURVE()
GEOMETRIC_REPRESENTATION_ITEM()
RATIONAL_B_SPLINE_CURVE((1.13348223894616,1.13389822901351,1.13426390111358))
REPRESENTATION_ITEM('')
);
#592=(
BOUNDED_CURVE()
B_SPLINE_CURVE(2,(#51216,#51217,#51218),.UNSPECIFIED.,.F.,.F.)
B_SPLINE_CURVE_WITH_KNOTS((3,3),(0.367644516946558,0.373830527582532),
 .UNSPECIFIED.)
CURVE()
GEOMETRIC_REPRESENTATION_ITEM()
RATIONAL_B_SPLINE_CURVE((1.13426390111307,1.13389822901301,1.13348223894566))
REPRESENTATION_ITEM('')
);
#593=(
BOUNDED_CURVE()
B_SPLINE_CURVE(2,(#51222,#51223,#51224),.UNSPECIFIED.,.F.,.F.)
B_SPLINE_CURVE_WITH_KNOTS((3,3),(0.271548216895914,0.277734227531905),
 .UNSPECIFIED.)
CURVE()
GEOMETRIC_REPRESENTATION_ITEM()
RATIONAL_B_SPLINE_CURVE((1.13348223894616,1.13389822901351,1.13426390111358))
REPRESENTATION_ITEM('')
);
#594=(
BOUNDED_CURVE()
B_SPLINE_CURVE(2,(#51228,#51229,#51230),.UNSPECIFIED.,.F.,.F.)
B_SPLINE_CURVE_WITH_KNOTS((3,3),(0.367644516946569,0.373830527582539),
 .UNSPECIFIED.)
CURVE()
GEOMETRIC_REPRESENTATION_ITEM()
RATIONAL_B_SPLINE_CURVE((1.13426390111301,1.13389822901295,1.1334822389456))
REPRESENTATION_ITEM('')
);
#595=(
BOUNDED_CURVE()
B_SPLINE_CURVE(2,(#51234,#51235,#51236),.UNSPECIFIED.,.F.,.F.)
B_SPLINE_CURVE_WITH_KNOTS((3,3),(0.271548216895913,0.2777342275319),
 .UNSPECIFIED.)
CURVE()
GEOMETRIC_REPRESENTATION_ITEM()
RATIONAL_B_SPLINE_CURVE((1.13348223894614,1.13389822901349,1.13426390111356))
REPRESENTATION_ITEM('')
);
#596=(
BOUNDED_CURVE()
B_SPLINE_CURVE(2,(#51240,#51241,#51242),.UNSPECIFIED.,.F.,.F.)
B_SPLINE_CURVE_WITH_KNOTS((3,3),(0.367644516946566,0.373830527582539),
 .UNSPECIFIED.)
CURVE()
GEOMETRIC_REPRESENTATION_ITEM()
RATIONAL_B_SPLINE_CURVE((1.13426390111297,1.1338982290129,1.13348223894556))
REPRESENTATION_ITEM('')
);
#597=(
BOUNDED_CURVE()
B_SPLINE_CURVE(2,(#51246,#51247,#51248),.UNSPECIFIED.,.F.,.F.)
B_SPLINE_CURVE_WITH_KNOTS((3,3),(0.271548216895926,0.277734227531904),
 .UNSPECIFIED.)
CURVE()
GEOMETRIC_REPRESENTATION_ITEM()
RATIONAL_B_SPLINE_CURVE((1.13348223894627,1.13389822901362,1.1342639011137))
REPRESENTATION_ITEM('')
);
#598=(
BOUNDED_CURVE()
B_SPLINE_CURVE(2,(#51252,#51253,#51254),.UNSPECIFIED.,.F.,.F.)
B_SPLINE_CURVE_WITH_KNOTS((3,3),(0.367644516946557,0.373830527582532),
 .UNSPECIFIED.)
CURVE()
GEOMETRIC_REPRESENTATION_ITEM()
RATIONAL_B_SPLINE_CURVE((1.13426390111306,1.13389822901299,1.13348223894565))
REPRESENTATION_ITEM('')
);
#599=(
BOUNDED_CURVE()
B_SPLINE_CURVE(2,(#51258,#51259,#51260),.UNSPECIFIED.,.F.,.F.)
B_SPLINE_CURVE_WITH_KNOTS((3,3),(0.271548216895913,0.277734227531899),
 .UNSPECIFIED.)
CURVE()
GEOMETRIC_REPRESENTATION_ITEM()
RATIONAL_B_SPLINE_CURVE((1.13348223894618,1.13389822901353,1.13426390111361))
REPRESENTATION_ITEM('')
);
#600=(
BOUNDED_CURVE()
B_SPLINE_CURVE(2,(#51264,#51265,#51266),.UNSPECIFIED.,.F.,.F.)
B_SPLINE_CURVE_WITH_KNOTS((3,3),(0.367644516946561,0.373830527582535),
 .UNSPECIFIED.)
CURVE()
GEOMETRIC_REPRESENTATION_ITEM()
RATIONAL_B_SPLINE_CURVE((1.13426390111305,1.13389822901298,1.13348223894564))
REPRESENTATION_ITEM('')
);
#601=(
BOUNDED_CURVE()
B_SPLINE_CURVE(2,(#51270,#51271,#51272),.UNSPECIFIED.,.F.,.F.)
B_SPLINE_CURVE_WITH_KNOTS((3,3),(0.271548216895915,0.277734227531905),
 .UNSPECIFIED.)
CURVE()
GEOMETRIC_REPRESENTATION_ITEM()
RATIONAL_B_SPLINE_CURVE((1.13348223894613,1.13389822901348,1.13426390111356))
REPRESENTATION_ITEM('')
);
#602=(
BOUNDED_CURVE()
B_SPLINE_CURVE(2,(#51276,#51277,#51278),.UNSPECIFIED.,.F.,.F.)
B_SPLINE_CURVE_WITH_KNOTS((3,3),(0.367644516946559,0.373830527582528),
 .UNSPECIFIED.)
CURVE()
GEOMETRIC_REPRESENTATION_ITEM()
RATIONAL_B_SPLINE_CURVE((1.13426390111303,1.13389822901297,1.13348223894562))
REPRESENTATION_ITEM('')
);
#603=(
BOUNDED_CURVE()
B_SPLINE_CURVE(2,(#51282,#51283,#51284),.UNSPECIFIED.,.F.,.F.)
B_SPLINE_CURVE_WITH_KNOTS((3,3),(0.271548216895913,0.277734227531899),
 .UNSPECIFIED.)
CURVE()
GEOMETRIC_REPRESENTATION_ITEM()
RATIONAL_B_SPLINE_CURVE((1.13348223894613,1.13389822901348,1.13426390111356))
REPRESENTATION_ITEM('')
);
#604=(
BOUNDED_CURVE()
B_SPLINE_CURVE(2,(#51288,#51289,#51290),.UNSPECIFIED.,.F.,.F.)
B_SPLINE_CURVE_WITH_KNOTS((3,3),(0.367644516946557,0.373830527582533),
 .UNSPECIFIED.)
CURVE()
GEOMETRIC_REPRESENTATION_ITEM()
RATIONAL_B_SPLINE_CURVE((1.13426390111302,1.13389822901296,1.13348223894561))
REPRESENTATION_ITEM('')
);
#605=(
BOUNDED_CURVE()
B_SPLINE_CURVE(2,(#51294,#51295,#51296),.UNSPECIFIED.,.F.,.F.)
B_SPLINE_CURVE_WITH_KNOTS((3,3),(0.271548216895926,0.277734227531906),
 .UNSPECIFIED.)
CURVE()
GEOMETRIC_REPRESENTATION_ITEM()
RATIONAL_B_SPLINE_CURVE((1.13348223894624,1.13389822901359,1.13426390111366))
REPRESENTATION_ITEM('')
);
#606=(
BOUNDED_CURVE()
B_SPLINE_CURVE(2,(#51300,#51301,#51302),.UNSPECIFIED.,.F.,.F.)
B_SPLINE_CURVE_WITH_KNOTS((3,3),(0.367644516946561,0.373830527582536),
 .UNSPECIFIED.)
CURVE()
GEOMETRIC_REPRESENTATION_ITEM()
RATIONAL_B_SPLINE_CURVE((1.13426390111306,1.13389822901299,1.13348223894564))
REPRESENTATION_ITEM('')
);
#607=(
BOUNDED_CURVE()
B_SPLINE_CURVE(2,(#51306,#51307,#51308),.UNSPECIFIED.,.F.,.F.)
B_SPLINE_CURVE_WITH_KNOTS((3,3),(0.271548216895911,0.277734227531901),
 .UNSPECIFIED.)
CURVE()
GEOMETRIC_REPRESENTATION_ITEM()
RATIONAL_B_SPLINE_CURVE((1.13348223894609,1.13389822901344,1.13426390111352))
REPRESENTATION_ITEM('')
);
#608=(
BOUNDED_CURVE()
B_SPLINE_CURVE(2,(#51312,#51313,#51314),.UNSPECIFIED.,.F.,.F.)
B_SPLINE_CURVE_WITH_KNOTS((3,3),(0.367644516946558,0.373830527582533),
 .UNSPECIFIED.)
CURVE()
GEOMETRIC_REPRESENTATION_ITEM()
RATIONAL_B_SPLINE_CURVE((1.1342639011131,1.13389822901303,1.13348223894569))
REPRESENTATION_ITEM('')
);
#609=(
BOUNDED_CURVE()
B_SPLINE_CURVE(2,(#51318,#51319,#51320),.UNSPECIFIED.,.F.,.F.)
B_SPLINE_CURVE_WITH_KNOTS((3,3),(0.271548216895922,0.277734227531909),
 .UNSPECIFIED.)
CURVE()
GEOMETRIC_REPRESENTATION_ITEM()
RATIONAL_B_SPLINE_CURVE((1.13348223894623,1.13389822901358,1.13426390111366))
REPRESENTATION_ITEM('')
);
#610=(
BOUNDED_CURVE()
B_SPLINE_CURVE(2,(#51324,#51325,#51326),.UNSPECIFIED.,.F.,.F.)
B_SPLINE_CURVE_WITH_KNOTS((3,3),(0.367644516946562,0.373830527582538),
 .UNSPECIFIED.)
CURVE()
GEOMETRIC_REPRESENTATION_ITEM()
RATIONAL_B_SPLINE_CURVE((1.13426390111305,1.13389822901298,1.13348223894563))
REPRESENTATION_ITEM('')
);
#611=(
BOUNDED_CURVE()
B_SPLINE_CURVE(2,(#51330,#51331,#51332),.UNSPECIFIED.,.F.,.F.)
B_SPLINE_CURVE_WITH_KNOTS((3,3),(0.271548216895906,0.277734227531898),
 .UNSPECIFIED.)
CURVE()
GEOMETRIC_REPRESENTATION_ITEM()
RATIONAL_B_SPLINE_CURVE((1.13348223894604,1.13389822901339,1.13426390111346))
REPRESENTATION_ITEM('')
);
#612=(
BOUNDED_CURVE()
B_SPLINE_CURVE(2,(#51336,#51337,#51338),.UNSPECIFIED.,.F.,.F.)
B_SPLINE_CURVE_WITH_KNOTS((3,3),(0.367644516946563,0.373830527582537),
 .UNSPECIFIED.)
CURVE()
GEOMETRIC_REPRESENTATION_ITEM()
RATIONAL_B_SPLINE_CURVE((1.134263901113,1.13389822901294,1.13348223894559))
REPRESENTATION_ITEM('')
);
#613=(
BOUNDED_CURVE()
B_SPLINE_CURVE(2,(#51342,#51343,#51344),.UNSPECIFIED.,.F.,.F.)
B_SPLINE_CURVE_WITH_KNOTS((3,3),(0.271548216895914,0.277734227531897),
 .UNSPECIFIED.)
CURVE()
GEOMETRIC_REPRESENTATION_ITEM()
RATIONAL_B_SPLINE_CURVE((1.13348223894613,1.13389822901348,1.13426390111355))
REPRESENTATION_ITEM('')
);
#614=(
BOUNDED_CURVE()
B_SPLINE_CURVE(2,(#51348,#51349,#51350),.UNSPECIFIED.,.F.,.F.)
B_SPLINE_CURVE_WITH_KNOTS((3,3),(0.367644516946558,0.373830527582532),
 .UNSPECIFIED.)
CURVE()
GEOMETRIC_REPRESENTATION_ITEM()
RATIONAL_B_SPLINE_CURVE((1.13426390111307,1.133898229013,1.13348223894566))
REPRESENTATION_ITEM('')
);
#615=(
BOUNDED_CURVE()
B_SPLINE_CURVE(2,(#51354,#51355,#51356),.UNSPECIFIED.,.F.,.F.)
B_SPLINE_CURVE_WITH_KNOTS((3,3),(0.271548216895917,0.277734227531901),
 .UNSPECIFIED.)
CURVE()
GEOMETRIC_REPRESENTATION_ITEM()
RATIONAL_B_SPLINE_CURVE((1.13348223894616,1.1338982290135,1.13426390111358))
REPRESENTATION_ITEM('')
);
#616=(
BOUNDED_CURVE()
B_SPLINE_CURVE(2,(#51360,#51361,#51362),.UNSPECIFIED.,.F.,.F.)
B_SPLINE_CURVE_WITH_KNOTS((3,3),(0.367644516946556,0.37383052758253),
 .UNSPECIFIED.)
CURVE()
GEOMETRIC_REPRESENTATION_ITEM()
RATIONAL_B_SPLINE_CURVE((1.13426390111304,1.13389822901297,1.13348223894563))
REPRESENTATION_ITEM('')
);
#617=(
BOUNDED_CURVE()
B_SPLINE_CURVE(2,(#51366,#51367,#51368),.UNSPECIFIED.,.F.,.F.)
B_SPLINE_CURVE_WITH_KNOTS((3,3),(0.271548216895911,0.277734227531893),
 .UNSPECIFIED.)
CURVE()
GEOMETRIC_REPRESENTATION_ITEM()
RATIONAL_B_SPLINE_CURVE((1.13348223894607,1.13389822901342,1.13426390111349))
REPRESENTATION_ITEM('')
);
#618=(
BOUNDED_CURVE()
B_SPLINE_CURVE(2,(#51372,#51373,#51374),.UNSPECIFIED.,.F.,.F.)
B_SPLINE_CURVE_WITH_KNOTS((3,3),(0.367644516946565,0.373830527582539),
 .UNSPECIFIED.)
CURVE()
GEOMETRIC_REPRESENTATION_ITEM()
RATIONAL_B_SPLINE_CURVE((1.13426390111301,1.13389822901295,1.1334822389456))
REPRESENTATION_ITEM('')
);
#619=(
BOUNDED_CURVE()
B_SPLINE_CURVE(2,(#51378,#51379,#51380),.UNSPECIFIED.,.F.,.F.)
B_SPLINE_CURVE_WITH_KNOTS((3,3),(0.271548216895916,0.277734227531897),
 .UNSPECIFIED.)
CURVE()
GEOMETRIC_REPRESENTATION_ITEM()
RATIONAL_B_SPLINE_CURVE((1.13348223894613,1.13389822901348,1.13426390111355))
REPRESENTATION_ITEM('')
);
#620=(
BOUNDED_CURVE()
B_SPLINE_CURVE(2,(#51384,#51385,#51386),.UNSPECIFIED.,.F.,.F.)
B_SPLINE_CURVE_WITH_KNOTS((3,3),(0.36764451694656,0.373830527582534),
 .UNSPECIFIED.)
CURVE()
GEOMETRIC_REPRESENTATION_ITEM()
RATIONAL_B_SPLINE_CURVE((1.13426390111306,1.13389822901299,1.13348223894564))
REPRESENTATION_ITEM('')
);
#621=(
BOUNDED_CURVE()
B_SPLINE_CURVE(2,(#51390,#51391,#51392),.UNSPECIFIED.,.F.,.F.)
B_SPLINE_CURVE_WITH_KNOTS((3,3),(0.271548216895918,0.277734227531904),
 .UNSPECIFIED.)
CURVE()
GEOMETRIC_REPRESENTATION_ITEM()
RATIONAL_B_SPLINE_CURVE((1.13348223894613,1.13389822901348,1.13426390111355))
REPRESENTATION_ITEM('')
);
#622=(
BOUNDED_CURVE()
B_SPLINE_CURVE(2,(#51396,#51397,#51398),.UNSPECIFIED.,.F.,.F.)
B_SPLINE_CURVE_WITH_KNOTS((3,3),(0.367644516946555,0.373830527582533),
 .UNSPECIFIED.)
CURVE()
GEOMETRIC_REPRESENTATION_ITEM()
RATIONAL_B_SPLINE_CURVE((1.13426390111305,1.13389822901298,1.13348223894564))
REPRESENTATION_ITEM('')
);
#623=(
BOUNDED_CURVE()
B_SPLINE_CURVE(2,(#51402,#51403,#51404),.UNSPECIFIED.,.F.,.F.)
B_SPLINE_CURVE_WITH_KNOTS((3,3),(0.271548216895928,0.277734227531916),
 .UNSPECIFIED.)
CURVE()
GEOMETRIC_REPRESENTATION_ITEM()
RATIONAL_B_SPLINE_CURVE((1.13348223894621,1.13389822901356,1.13426390111363))
REPRESENTATION_ITEM('')
);
#624=(
BOUNDED_CURVE()
B_SPLINE_CURVE(2,(#51408,#51409,#51410),.UNSPECIFIED.,.F.,.F.)
B_SPLINE_CURVE_WITH_KNOTS((3,3),(0.367644516946548,0.373830527582523),
 .UNSPECIFIED.)
CURVE()
GEOMETRIC_REPRESENTATION_ITEM()
RATIONAL_B_SPLINE_CURVE((1.13426390111312,1.13389822901305,1.13348223894571))
REPRESENTATION_ITEM('')
);
#625=(
BOUNDED_CURVE()
B_SPLINE_CURVE(2,(#51414,#51415,#51416),.UNSPECIFIED.,.F.,.F.)
B_SPLINE_CURVE_WITH_KNOTS((3,3),(0.271548216895918,0.277734227531905),
 .UNSPECIFIED.)
CURVE()
GEOMETRIC_REPRESENTATION_ITEM()
RATIONAL_B_SPLINE_CURVE((1.13348223894611,1.13389822901346,1.13426390111354))
REPRESENTATION_ITEM('')
);
#626=(
BOUNDED_CURVE()
B_SPLINE_CURVE(2,(#51420,#51421,#51422),.UNSPECIFIED.,.F.,.F.)
B_SPLINE_CURVE_WITH_KNOTS((3,3),(0.367644516946559,0.373830527582532),
 .UNSPECIFIED.)
CURVE()
GEOMETRIC_REPRESENTATION_ITEM()
RATIONAL_B_SPLINE_CURVE((1.13426390111305,1.13389822901298,1.13348223894564))
REPRESENTATION_ITEM('')
);
#627=(
BOUNDED_CURVE()
B_SPLINE_CURVE(2,(#51426,#51427,#51428),.UNSPECIFIED.,.F.,.F.)
B_SPLINE_CURVE_WITH_KNOTS((3,3),(0.271548216895915,0.277734227531901),
 .UNSPECIFIED.)
CURVE()
GEOMETRIC_REPRESENTATION_ITEM()
RATIONAL_B_SPLINE_CURVE((1.13348223894615,1.1338982290135,1.13426390111357))
REPRESENTATION_ITEM('')
);
#628=(
BOUNDED_CURVE()
B_SPLINE_CURVE(2,(#51432,#51433,#51434),.UNSPECIFIED.,.F.,.F.)
B_SPLINE_CURVE_WITH_KNOTS((3,3),(0.367644516946548,0.373830527582526),
 .UNSPECIFIED.)
CURVE()
GEOMETRIC_REPRESENTATION_ITEM()
RATIONAL_B_SPLINE_CURVE((1.13426390111308,1.13389822901302,1.13348223894567))
REPRESENTATION_ITEM('')
);
#629=(
BOUNDED_CURVE()
B_SPLINE_CURVE(2,(#51438,#51439,#51440),.UNSPECIFIED.,.F.,.F.)
B_SPLINE_CURVE_WITH_KNOTS((3,3),(0.271548216895917,0.277734227531902),
 .UNSPECIFIED.)
CURVE()
GEOMETRIC_REPRESENTATION_ITEM()
RATIONAL_B_SPLINE_CURVE((1.13348223894615,1.1338982290135,1.13426390111358))
REPRESENTATION_ITEM('')
);
#630=(
BOUNDED_CURVE()
B_SPLINE_CURVE(2,(#51444,#51445,#51446),.UNSPECIFIED.,.F.,.F.)
B_SPLINE_CURVE_WITH_KNOTS((3,3),(0.367644516946561,0.373830527582534),
 .UNSPECIFIED.)
CURVE()
GEOMETRIC_REPRESENTATION_ITEM()
RATIONAL_B_SPLINE_CURVE((1.13426390111303,1.13389822901296,1.13348223894562))
REPRESENTATION_ITEM('')
);
#631=(
BOUNDED_CURVE()
B_SPLINE_CURVE(2,(#51450,#51451,#51452),.UNSPECIFIED.,.F.,.F.)
B_SPLINE_CURVE_WITH_KNOTS((3,3),(0.271548216895922,0.277734227531908),
 .UNSPECIFIED.)
CURVE()
GEOMETRIC_REPRESENTATION_ITEM()
RATIONAL_B_SPLINE_CURVE((1.13348223894617,1.13389822901352,1.1342639011136))
REPRESENTATION_ITEM('')
);
#632=(
BOUNDED_CURVE()
B_SPLINE_CURVE(2,(#51456,#51457,#51458),.UNSPECIFIED.,.F.,.F.)
B_SPLINE_CURVE_WITH_KNOTS((3,3),(0.367644516946555,0.373830527582532),
 .UNSPECIFIED.)
CURVE()
GEOMETRIC_REPRESENTATION_ITEM()
RATIONAL_B_SPLINE_CURVE((1.13426390111307,1.133898229013,1.13348223894566))
REPRESENTATION_ITEM('')
);
#633=(
BOUNDED_CURVE()
B_SPLINE_CURVE(2,(#51462,#51463,#51464),.UNSPECIFIED.,.F.,.F.)
B_SPLINE_CURVE_WITH_KNOTS((3,3),(0.27154821689592,0.277734227531907),
 .UNSPECIFIED.)
CURVE()
GEOMETRIC_REPRESENTATION_ITEM()
RATIONAL_B_SPLINE_CURVE((1.13348223894614,1.13389822901349,1.13426390111356))
REPRESENTATION_ITEM('')
);
#634=(
BOUNDED_CURVE()
B_SPLINE_CURVE(2,(#51468,#51469,#51470),.UNSPECIFIED.,.F.,.F.)
B_SPLINE_CURVE_WITH_KNOTS((3,3),(0.367644516946564,0.373830527582538),
 .UNSPECIFIED.)
CURVE()
GEOMETRIC_REPRESENTATION_ITEM()
RATIONAL_B_SPLINE_CURVE((1.13426390111299,1.13389822901292,1.13348223894557))
REPRESENTATION_ITEM('')
);
#635=(
BOUNDED_CURVE()
B_SPLINE_CURVE(2,(#51474,#51475,#51476),.UNSPECIFIED.,.F.,.F.)
B_SPLINE_CURVE_WITH_KNOTS((3,3),(0.271548216895926,0.277734227531912),
 .UNSPECIFIED.)
CURVE()
GEOMETRIC_REPRESENTATION_ITEM()
RATIONAL_B_SPLINE_CURVE((1.13348223894617,1.13389822901352,1.13426390111359))
REPRESENTATION_ITEM('')
);
#636=(
BOUNDED_CURVE()
B_SPLINE_CURVE(2,(#51480,#51481,#51482),.UNSPECIFIED.,.F.,.F.)
B_SPLINE_CURVE_WITH_KNOTS((3,3),(0.367644516946548,0.373830527582525),
 .UNSPECIFIED.)
CURVE()
GEOMETRIC_REPRESENTATION_ITEM()
RATIONAL_B_SPLINE_CURVE((1.13426390111308,1.13389822901301,1.13348223894567))
REPRESENTATION_ITEM('')
);
#637=(
BOUNDED_CURVE()
B_SPLINE_CURVE(2,(#51486,#51487,#51488),.UNSPECIFIED.,.F.,.F.)
B_SPLINE_CURVE_WITH_KNOTS((3,3),(0.271548216895921,0.277734227531907),
 .UNSPECIFIED.)
CURVE()
GEOMETRIC_REPRESENTATION_ITEM()
RATIONAL_B_SPLINE_CURVE((1.13348223894617,1.13389822901352,1.13426390111359))
REPRESENTATION_ITEM('')
);
#638=(
BOUNDED_CURVE()
B_SPLINE_CURVE(2,(#51492,#51493,#51494),.UNSPECIFIED.,.F.,.F.)
B_SPLINE_CURVE_WITH_KNOTS((3,3),(0.367644516946557,0.373830527582527),
 .UNSPECIFIED.)
CURVE()
GEOMETRIC_REPRESENTATION_ITEM()
RATIONAL_B_SPLINE_CURVE((1.1342639011131,1.13389822901303,1.13348223894569))
REPRESENTATION_ITEM('')
);
#639=(
BOUNDED_CURVE()
B_SPLINE_CURVE(2,(#51497,#51498,#51499),.UNSPECIFIED.,.F.,.F.)
B_SPLINE_CURVE_WITH_KNOTS((3,3),(0.271548216895922,0.277734227531908),
 .UNSPECIFIED.)
CURVE()
GEOMETRIC_REPRESENTATION_ITEM()
RATIONAL_B_SPLINE_CURVE((1.13348223894615,1.1338982290135,1.13426390111358))
REPRESENTATION_ITEM('')
);
#640=(
BOUNDED_CURVE()
B_SPLINE_CURVE(2,(#51501,#51502,#51503),.UNSPECIFIED.,.F.,.F.)
B_SPLINE_CURVE_WITH_KNOTS((3,3),(0.367644516946556,0.373830527582529),
 .UNSPECIFIED.)
CURVE()
GEOMETRIC_REPRESENTATION_ITEM()
RATIONAL_B_SPLINE_CURVE((1.13426390111308,1.13389822901301,1.13348223894567))
REPRESENTATION_ITEM('')
);
#641=(
BOUNDED_CURVE()
B_SPLINE_CURVE(2,(#51506,#51507,#51508),.UNSPECIFIED.,.F.,.F.)
B_SPLINE_CURVE_WITH_KNOTS((3,3),(0.271548216895921,0.277734227531909),
 .UNSPECIFIED.)
CURVE()
GEOMETRIC_REPRESENTATION_ITEM()
RATIONAL_B_SPLINE_CURVE((1.13348223894619,1.13389822901354,1.13426390111361))
REPRESENTATION_ITEM('')
);
#642=(
BOUNDED_CURVE()
B_SPLINE_CURVE(2,(#51510,#51511,#51512),.UNSPECIFIED.,.F.,.F.)
B_SPLINE_CURVE_WITH_KNOTS((3,3),(0.36764451694656,0.37383052758253),
 .UNSPECIFIED.)
CURVE()
GEOMETRIC_REPRESENTATION_ITEM()
RATIONAL_B_SPLINE_CURVE((1.13426390111303,1.13389822901296,1.13348223894562))
REPRESENTATION_ITEM('')
);
#643=(
BOUNDED_CURVE()
B_SPLINE_CURVE(2,(#51515,#51516,#51517),.UNSPECIFIED.,.F.,.F.)
B_SPLINE_CURVE_WITH_KNOTS((3,3),(0.271548216895921,0.277734227531907),
 .UNSPECIFIED.)
CURVE()
GEOMETRIC_REPRESENTATION_ITEM()
RATIONAL_B_SPLINE_CURVE((1.13348223894618,1.13389822901353,1.1342639011136))
REPRESENTATION_ITEM('')
);
#644=(
BOUNDED_CURVE()
B_SPLINE_CURVE(2,(#51519,#51520,#51521),.UNSPECIFIED.,.F.,.F.)
B_SPLINE_CURVE_WITH_KNOTS((3,3),(0.367644516946553,0.373830527582534),
 .UNSPECIFIED.)
CURVE()
GEOMETRIC_REPRESENTATION_ITEM()
RATIONAL_B_SPLINE_CURVE((1.13426390111306,1.13389822901299,1.13348223894565))
REPRESENTATION_ITEM('')
);
#645=(
BOUNDED_CURVE()
B_SPLINE_CURVE(2,(#51524,#51525,#51526),.UNSPECIFIED.,.F.,.F.)
B_SPLINE_CURVE_WITH_KNOTS((3,3),(0.271548216895916,0.277734227531903),
 .UNSPECIFIED.)
CURVE()
GEOMETRIC_REPRESENTATION_ITEM()
RATIONAL_B_SPLINE_CURVE((1.13348223894615,1.1338982290135,1.13426390111357))
REPRESENTATION_ITEM('')
);
#646=(
BOUNDED_CURVE()
B_SPLINE_CURVE(2,(#51528,#51529,#51530),.UNSPECIFIED.,.F.,.F.)
B_SPLINE_CURVE_WITH_KNOTS((3,3),(0.367644516946558,0.373830527582532),
 .UNSPECIFIED.)
CURVE()
GEOMETRIC_REPRESENTATION_ITEM()
RATIONAL_B_SPLINE_CURVE((1.13426390111307,1.13389822901301,1.13348223894566))
REPRESENTATION_ITEM('')
);
#647=(
BOUNDED_CURVE()
B_SPLINE_CURVE(2,(#51533,#51534,#51535),.UNSPECIFIED.,.F.,.F.)
B_SPLINE_CURVE_WITH_KNOTS((3,3),(0.271548216895911,0.277734227531895),
 .UNSPECIFIED.)
CURVE()
GEOMETRIC_REPRESENTATION_ITEM()
RATIONAL_B_SPLINE_CURVE((1.13348223894606,1.13389822901341,1.13426390111348))
REPRESENTATION_ITEM('')
);
#648=(
BOUNDED_CURVE()
B_SPLINE_CURVE(2,(#51537,#51538,#51539),.UNSPECIFIED.,.F.,.F.)
B_SPLINE_CURVE_WITH_KNOTS((3,3),(0.367644516946553,0.373830527582531),
 .UNSPECIFIED.)
CURVE()
GEOMETRIC_REPRESENTATION_ITEM()
RATIONAL_B_SPLINE_CURVE((1.13426390111307,1.133898229013,1.13348223894566))
REPRESENTATION_ITEM('')
);
#649=(
BOUNDED_CURVE()
B_SPLINE_CURVE(2,(#51542,#51543,#51544),.UNSPECIFIED.,.F.,.F.)
B_SPLINE_CURVE_WITH_KNOTS((3,3),(0.271548216895918,0.277734227531903),
 .UNSPECIFIED.)
CURVE()
GEOMETRIC_REPRESENTATION_ITEM()
RATIONAL_B_SPLINE_CURVE((1.13348223894611,1.13389822901346,1.13426390111353))
REPRESENTATION_ITEM('')
);
#650=(
BOUNDED_CURVE()
B_SPLINE_CURVE(2,(#51546,#51547,#51548),.UNSPECIFIED.,.F.,.F.)
B_SPLINE_CURVE_WITH_KNOTS((3,3),(0.367644516946551,0.373830527582526),
 .UNSPECIFIED.)
CURVE()
GEOMETRIC_REPRESENTATION_ITEM()
RATIONAL_B_SPLINE_CURVE((1.1342639011131,1.13389822901304,1.13348223894569))
REPRESENTATION_ITEM('')
);
#651=(
BOUNDED_CURVE()
B_SPLINE_CURVE(2,(#51551,#51552,#51553),.UNSPECIFIED.,.F.,.F.)
B_SPLINE_CURVE_WITH_KNOTS((3,3),(0.271548216895922,0.277734227531909),
 .UNSPECIFIED.)
CURVE()
GEOMETRIC_REPRESENTATION_ITEM()
RATIONAL_B_SPLINE_CURVE((1.13348223894615,1.1338982290135,1.13426390111357))
REPRESENTATION_ITEM('')
);
#652=(
BOUNDED_CURVE()
B_SPLINE_CURVE(2,(#51555,#51556,#51557),.UNSPECIFIED.,.F.,.F.)
B_SPLINE_CURVE_WITH_KNOTS((3,3),(0.36764451694656,0.373830527582534),
 .UNSPECIFIED.)
CURVE()
GEOMETRIC_REPRESENTATION_ITEM()
RATIONAL_B_SPLINE_CURVE((1.13426390111304,1.13389822901297,1.13348223894563))
REPRESENTATION_ITEM('')
);
#653=(
BOUNDED_CURVE()
B_SPLINE_CURVE(2,(#51560,#51561,#51562),.UNSPECIFIED.,.F.,.F.)
B_SPLINE_CURVE_WITH_KNOTS((3,3),(0.271548216895917,0.277734227531904),
 .UNSPECIFIED.)
CURVE()
GEOMETRIC_REPRESENTATION_ITEM()
RATIONAL_B_SPLINE_CURVE((1.13348223894616,1.13389822901351,1.13426390111359))
REPRESENTATION_ITEM('')
);
#654=(
BOUNDED_CURVE()
B_SPLINE_CURVE(2,(#51564,#51565,#51566),.UNSPECIFIED.,.F.,.F.)
B_SPLINE_CURVE_WITH_KNOTS((3,3),(0.367644516946562,0.373830527582537),
 .UNSPECIFIED.)
CURVE()
GEOMETRIC_REPRESENTATION_ITEM()
RATIONAL_B_SPLINE_CURVE((1.13426390111298,1.13389822901291,1.13348223894556))
REPRESENTATION_ITEM('')
);
#655=(
BOUNDED_CURVE()
B_SPLINE_CURVE(2,(#51569,#51570,#51571),.UNSPECIFIED.,.F.,.F.)
B_SPLINE_CURVE_WITH_KNOTS((3,3),(0.271548216895925,0.277734227531911),
 .UNSPECIFIED.)
CURVE()
GEOMETRIC_REPRESENTATION_ITEM()
RATIONAL_B_SPLINE_CURVE((1.13348223894616,1.13389822901351,1.13426390111359))
REPRESENTATION_ITEM('')
);
#656=(
BOUNDED_CURVE()
B_SPLINE_CURVE(2,(#51573,#51574,#51575),.UNSPECIFIED.,.F.,.F.)
B_SPLINE_CURVE_WITH_KNOTS((3,3),(0.367644516946555,0.373830527582529),
 .UNSPECIFIED.)
CURVE()
GEOMETRIC_REPRESENTATION_ITEM()
RATIONAL_B_SPLINE_CURVE((1.13426390111312,1.13389822901305,1.13348223894571))
REPRESENTATION_ITEM('')
);
#657=(
BOUNDED_CURVE()
B_SPLINE_CURVE(2,(#51578,#51579,#51580),.UNSPECIFIED.,.F.,.F.)
B_SPLINE_CURVE_WITH_KNOTS((3,3),(0.271548216895925,0.277734227531912),
 .UNSPECIFIED.)
CURVE()
GEOMETRIC_REPRESENTATION_ITEM()
RATIONAL_B_SPLINE_CURVE((1.13348223894618,1.13389822901353,1.1342639011136))
REPRESENTATION_ITEM('')
);
#658=(
BOUNDED_CURVE()
B_SPLINE_CURVE(2,(#51582,#51583,#51584),.UNSPECIFIED.,.F.,.F.)
B_SPLINE_CURVE_WITH_KNOTS((3,3),(0.367644516946557,0.373830527582532),
 .UNSPECIFIED.)
CURVE()
GEOMETRIC_REPRESENTATION_ITEM()
RATIONAL_B_SPLINE_CURVE((1.13426390111306,1.13389822901299,1.13348223894564))
REPRESENTATION_ITEM('')
);
#659=(
BOUNDED_CURVE()
B_SPLINE_CURVE(2,(#51587,#51588,#51589),.UNSPECIFIED.,.F.,.F.)
B_SPLINE_CURVE_WITH_KNOTS((3,3),(0.271548216895908,0.277734227531892),
 .UNSPECIFIED.)
CURVE()
GEOMETRIC_REPRESENTATION_ITEM()
RATIONAL_B_SPLINE_CURVE((1.13348223894609,1.13389822901344,1.13426390111352))
REPRESENTATION_ITEM('')
);
#660=(
BOUNDED_CURVE()
B_SPLINE_CURVE(2,(#51591,#51592,#51593),.UNSPECIFIED.,.F.,.F.)
B_SPLINE_CURVE_WITH_KNOTS((3,3),(0.367644516946557,0.373830527582522),
 .UNSPECIFIED.)
CURVE()
GEOMETRIC_REPRESENTATION_ITEM()
RATIONAL_B_SPLINE_CURVE((1.13426390111309,1.13389822901302,1.13348223894568))
REPRESENTATION_ITEM('')
);
#661=(
BOUNDED_CURVE()
B_SPLINE_CURVE(2,(#51596,#51597,#51598),.UNSPECIFIED.,.F.,.F.)
B_SPLINE_CURVE_WITH_KNOTS((3,3),(0.271548216895913,0.277734227531902),
 .UNSPECIFIED.)
CURVE()
GEOMETRIC_REPRESENTATION_ITEM()
RATIONAL_B_SPLINE_CURVE((1.1334822389461,1.13389822901345,1.13426390111352))
REPRESENTATION_ITEM('')
);
#662=(
BOUNDED_CURVE()
B_SPLINE_CURVE(2,(#51600,#51601,#51602),.UNSPECIFIED.,.F.,.F.)
B_SPLINE_CURVE_WITH_KNOTS((3,3),(0.367644516946559,0.373830527582539),
 .UNSPECIFIED.)
CURVE()
GEOMETRIC_REPRESENTATION_ITEM()
RATIONAL_B_SPLINE_CURVE((1.13426390111296,1.13389822901289,1.13348223894555))
REPRESENTATION_ITEM('')
);
#663=(
BOUNDED_CURVE()
B_SPLINE_CURVE(2,(#51605,#51606,#51607),.UNSPECIFIED.,.F.,.F.)
B_SPLINE_CURVE_WITH_KNOTS((3,3),(0.271548216895926,0.277734227531913),
 .UNSPECIFIED.)
CURVE()
GEOMETRIC_REPRESENTATION_ITEM()
RATIONAL_B_SPLINE_CURVE((1.13348223894622,1.13389822901357,1.13426390111365))
REPRESENTATION_ITEM('')
);
#664=(
BOUNDED_CURVE()
B_SPLINE_CURVE(2,(#51609,#51610,#51611),.UNSPECIFIED.,.F.,.F.)
B_SPLINE_CURVE_WITH_KNOTS((3,3),(0.36764451694656,0.373830527582534),
 .UNSPECIFIED.)
CURVE()
GEOMETRIC_REPRESENTATION_ITEM()
RATIONAL_B_SPLINE_CURVE((1.13426390111298,1.13389822901291,1.13348223894557))
REPRESENTATION_ITEM('')
);
#665=(
BOUNDED_CURVE()
B_SPLINE_CURVE(2,(#51614,#51615,#51616),.UNSPECIFIED.,.F.,.F.)
B_SPLINE_CURVE_WITH_KNOTS((3,3),(0.271548216895926,0.277734227531909),
 .UNSPECIFIED.)
CURVE()
GEOMETRIC_REPRESENTATION_ITEM()
RATIONAL_B_SPLINE_CURVE((1.13348223894617,1.13389822901352,1.13426390111359))
REPRESENTATION_ITEM('')
);
#666=(
BOUNDED_CURVE()
B_SPLINE_CURVE(2,(#51618,#51619,#51620),.UNSPECIFIED.,.F.,.F.)
B_SPLINE_CURVE_WITH_KNOTS((3,3),(0.367644516946566,0.373830527582539),
 .UNSPECIFIED.)
CURVE()
GEOMETRIC_REPRESENTATION_ITEM()
RATIONAL_B_SPLINE_CURVE((1.13426390111296,1.13389822901289,1.13348223894555))
REPRESENTATION_ITEM('')
);
#667=(
BOUNDED_CURVE()
B_SPLINE_CURVE(2,(#51623,#51624,#51625),.UNSPECIFIED.,.F.,.F.)
B_SPLINE_CURVE_WITH_KNOTS((3,3),(0.271548216895918,0.277734227531904),
 .UNSPECIFIED.)
CURVE()
GEOMETRIC_REPRESENTATION_ITEM()
RATIONAL_B_SPLINE_CURVE((1.13348223894611,1.13389822901346,1.13426390111353))
REPRESENTATION_ITEM('')
);
#668=(
BOUNDED_CURVE()
B_SPLINE_CURVE(2,(#51627,#51628,#51629),.UNSPECIFIED.,.F.,.F.)
B_SPLINE_CURVE_WITH_KNOTS((3,3),(0.367644516946555,0.373830527582529),
 .UNSPECIFIED.)
CURVE()
GEOMETRIC_REPRESENTATION_ITEM()
RATIONAL_B_SPLINE_CURVE((1.13426390111303,1.13389822901296,1.13348223894562))
REPRESENTATION_ITEM('')
);
#669=(
BOUNDED_CURVE()
B_SPLINE_CURVE(2,(#51633,#51634,#51635),.UNSPECIFIED.,.F.,.F.)
B_SPLINE_CURVE_WITH_KNOTS((3,3),(0.271548216895927,0.277734227531913),
 .UNSPECIFIED.)
CURVE()
GEOMETRIC_REPRESENTATION_ITEM()
RATIONAL_B_SPLINE_CURVE((1.13348223894624,1.13389822901359,1.13426390111366))
REPRESENTATION_ITEM('')
);
#670=(
BOUNDED_CURVE()
B_SPLINE_CURVE(2,(#51639,#51640,#51641),.UNSPECIFIED.,.F.,.F.)
B_SPLINE_CURVE_WITH_KNOTS((3,3),(0.367644516946557,0.373830527582527),
 .UNSPECIFIED.)
CURVE()
GEOMETRIC_REPRESENTATION_ITEM()
RATIONAL_B_SPLINE_CURVE((1.1342639011131,1.13389822901303,1.13348223894569))
REPRESENTATION_ITEM('')
);
#671=(
BOUNDED_CURVE()
B_SPLINE_CURVE(2,(#51645,#51646,#51647),.UNSPECIFIED.,.F.,.F.)
B_SPLINE_CURVE_WITH_KNOTS((3,3),(0.27154821689592,0.277734227531904),
 .UNSPECIFIED.)
CURVE()
GEOMETRIC_REPRESENTATION_ITEM()
RATIONAL_B_SPLINE_CURVE((1.13348223894613,1.13389822901348,1.13426390111355))
REPRESENTATION_ITEM('')
);
#672=(
BOUNDED_CURVE()
B_SPLINE_CURVE(2,(#51651,#51652,#51653),.UNSPECIFIED.,.F.,.F.)
B_SPLINE_CURVE_WITH_KNOTS((3,3),(0.367644516946566,0.373830527582538),
 .UNSPECIFIED.)
CURVE()
GEOMETRIC_REPRESENTATION_ITEM()
RATIONAL_B_SPLINE_CURVE((1.13426390111301,1.13389822901294,1.1334822389456))
REPRESENTATION_ITEM('')
);
#673=(
BOUNDED_CURVE()
B_SPLINE_CURVE(2,(#51657,#51658,#51659),.UNSPECIFIED.,.F.,.F.)
B_SPLINE_CURVE_WITH_KNOTS((3,3),(0.27154821689592,0.277734227531902),
 .UNSPECIFIED.)
CURVE()
GEOMETRIC_REPRESENTATION_ITEM()
RATIONAL_B_SPLINE_CURVE((1.1334822389461,1.13389822901344,1.13426390111352))
REPRESENTATION_ITEM('')
);
#674=(
BOUNDED_CURVE()
B_SPLINE_CURVE(2,(#51663,#51664,#51665),.UNSPECIFIED.,.F.,.F.)
B_SPLINE_CURVE_WITH_KNOTS((3,3),(0.367644516946558,0.373830527582536),
 .UNSPECIFIED.)
CURVE()
GEOMETRIC_REPRESENTATION_ITEM()
RATIONAL_B_SPLINE_CURVE((1.13426390111303,1.13389822901296,1.13348223894562))
REPRESENTATION_ITEM('')
);
#675=(
BOUNDED_CURVE()
B_SPLINE_CURVE(2,(#51669,#51670,#51671),.UNSPECIFIED.,.F.,.F.)
B_SPLINE_CURVE_WITH_KNOTS((3,3),(0.271548216895916,0.277734227531903),
 .UNSPECIFIED.)
CURVE()
GEOMETRIC_REPRESENTATION_ITEM()
RATIONAL_B_SPLINE_CURVE((1.13348223894608,1.13389822901343,1.1342639011135))
REPRESENTATION_ITEM('')
);
#676=(
BOUNDED_CURVE()
B_SPLINE_CURVE(2,(#51675,#51676,#51677),.UNSPECIFIED.,.F.,.F.)
B_SPLINE_CURVE_WITH_KNOTS((3,3),(0.367644516946558,0.373830527582538),
 .UNSPECIFIED.)
CURVE()
GEOMETRIC_REPRESENTATION_ITEM()
RATIONAL_B_SPLINE_CURVE((1.13426390111299,1.13389822901292,1.13348223894558))
REPRESENTATION_ITEM('')
);
#677=(
BOUNDED_CURVE()
B_SPLINE_CURVE(2,(#51681,#51682,#51683),.UNSPECIFIED.,.F.,.F.)
B_SPLINE_CURVE_WITH_KNOTS((3,3),(0.271548216895918,0.277734227531905),
 .UNSPECIFIED.)
CURVE()
GEOMETRIC_REPRESENTATION_ITEM()
RATIONAL_B_SPLINE_CURVE((1.13348223894618,1.13389822901353,1.1342639011136))
REPRESENTATION_ITEM('')
);
#678=(
BOUNDED_CURVE()
B_SPLINE_CURVE(2,(#51687,#51688,#51689),.UNSPECIFIED.,.F.,.F.)
B_SPLINE_CURVE_WITH_KNOTS((3,3),(0.367644516946549,0.373830527582523),
 .UNSPECIFIED.)
CURVE()
GEOMETRIC_REPRESENTATION_ITEM()
RATIONAL_B_SPLINE_CURVE((1.13426390111313,1.13389822901306,1.13348223894572))
REPRESENTATION_ITEM('')
);
#679=(
BOUNDED_CURVE()
B_SPLINE_CURVE(2,(#51693,#51694,#51695),.UNSPECIFIED.,.F.,.F.)
B_SPLINE_CURVE_WITH_KNOTS((3,3),(0.271548216895918,0.277734227531904),
 .UNSPECIFIED.)
CURVE()
GEOMETRIC_REPRESENTATION_ITEM()
RATIONAL_B_SPLINE_CURVE((1.13348223894607,1.13389822901342,1.1342639011135))
REPRESENTATION_ITEM('')
);
#680=(
BOUNDED_CURVE()
B_SPLINE_CURVE(2,(#51699,#51700,#51701),.UNSPECIFIED.,.F.,.F.)
B_SPLINE_CURVE_WITH_KNOTS((3,3),(0.367644516946553,0.373830527582525),
 .UNSPECIFIED.)
CURVE()
GEOMETRIC_REPRESENTATION_ITEM()
RATIONAL_B_SPLINE_CURVE((1.13426390111306,1.133898229013,1.13348223894565))
REPRESENTATION_ITEM('')
);
#681=(
BOUNDED_CURVE()
B_SPLINE_CURVE(2,(#51705,#51706,#51707),.UNSPECIFIED.,.F.,.F.)
B_SPLINE_CURVE_WITH_KNOTS((3,3),(0.271548216895918,0.277734227531897),
 .UNSPECIFIED.)
CURVE()
GEOMETRIC_REPRESENTATION_ITEM()
RATIONAL_B_SPLINE_CURVE((1.13348223894613,1.13389822901348,1.13426390111355))
REPRESENTATION_ITEM('')
);
#682=(
BOUNDED_CURVE()
B_SPLINE_CURVE(2,(#51711,#51712,#51713),.UNSPECIFIED.,.F.,.F.)
B_SPLINE_CURVE_WITH_KNOTS((3,3),(0.367644516946551,0.373830527582524),
 .UNSPECIFIED.)
CURVE()
GEOMETRIC_REPRESENTATION_ITEM()
RATIONAL_B_SPLINE_CURVE((1.13426390111309,1.13389822901302,1.13348223894568))
REPRESENTATION_ITEM('')
);
#683=(
BOUNDED_CURVE()
B_SPLINE_CURVE(2,(#51717,#51718,#51719),.UNSPECIFIED.,.F.,.F.)
B_SPLINE_CURVE_WITH_KNOTS((3,3),(0.271548216895914,0.2777342275319),
 .UNSPECIFIED.)
CURVE()
GEOMETRIC_REPRESENTATION_ITEM()
RATIONAL_B_SPLINE_CURVE((1.13348223894608,1.13389822901343,1.13426390111351))
REPRESENTATION_ITEM('')
);
#684=(
BOUNDED_CURVE()
B_SPLINE_CURVE(2,(#51723,#51724,#51725),.UNSPECIFIED.,.F.,.F.)
B_SPLINE_CURVE_WITH_KNOTS((3,3),(0.367644516946559,0.373830527582536),
 .UNSPECIFIED.)
CURVE()
GEOMETRIC_REPRESENTATION_ITEM()
RATIONAL_B_SPLINE_CURVE((1.13426390111305,1.13389822901298,1.13348223894564))
REPRESENTATION_ITEM('')
);
#685=(
BOUNDED_CURVE()
B_SPLINE_CURVE(2,(#51729,#51730,#51731),.UNSPECIFIED.,.F.,.F.)
B_SPLINE_CURVE_WITH_KNOTS((3,3),(0.27154821689591,0.277734227531898),
 .UNSPECIFIED.)
CURVE()
GEOMETRIC_REPRESENTATION_ITEM()
RATIONAL_B_SPLINE_CURVE((1.13348223894607,1.13389822901342,1.1342639011135))
REPRESENTATION_ITEM('')
);
#686=(
BOUNDED_CURVE()
B_SPLINE_CURVE(2,(#51735,#51736,#51737),.UNSPECIFIED.,.F.,.F.)
B_SPLINE_CURVE_WITH_KNOTS((3,3),(0.367644516946559,0.373830527582532),
 .UNSPECIFIED.)
CURVE()
GEOMETRIC_REPRESENTATION_ITEM()
RATIONAL_B_SPLINE_CURVE((1.13426390111307,1.133898229013,1.13348223894566))
REPRESENTATION_ITEM('')
);
#687=(
BOUNDED_CURVE()
B_SPLINE_CURVE(2,(#51741,#51742,#51743),.UNSPECIFIED.,.F.,.F.)
B_SPLINE_CURVE_WITH_KNOTS((3,3),(0.271548216895924,0.277734227531905),
 .UNSPECIFIED.)
CURVE()
GEOMETRIC_REPRESENTATION_ITEM()
RATIONAL_B_SPLINE_CURVE((1.13348223894618,1.13389822901353,1.1342639011136))
REPRESENTATION_ITEM('')
);
#688=(
BOUNDED_CURVE()
B_SPLINE_CURVE(2,(#51747,#51748,#51749),.UNSPECIFIED.,.F.,.F.)
B_SPLINE_CURVE_WITH_KNOTS((3,3),(0.367644516946555,0.373830527582531),
 .UNSPECIFIED.)
CURVE()
GEOMETRIC_REPRESENTATION_ITEM()
RATIONAL_B_SPLINE_CURVE((1.134263901113,1.13389822901293,1.13348223894559))
REPRESENTATION_ITEM('')
);
#689=(
BOUNDED_CURVE()
B_SPLINE_CURVE(2,(#51753,#51754,#51755),.UNSPECIFIED.,.F.,.F.)
B_SPLINE_CURVE_WITH_KNOTS((3,3),(0.271548216895916,0.277734227531902),
 .UNSPECIFIED.)
CURVE()
GEOMETRIC_REPRESENTATION_ITEM()
RATIONAL_B_SPLINE_CURVE((1.13348223894612,1.13389822901347,1.13426390111355))
REPRESENTATION_ITEM('')
);
#690=(
BOUNDED_CURVE()
B_SPLINE_CURVE(2,(#51759,#51760,#51761),.UNSPECIFIED.,.F.,.F.)
B_SPLINE_CURVE_WITH_KNOTS((3,3),(0.36764451694656,0.373830527582534),
 .UNSPECIFIED.)
CURVE()
GEOMETRIC_REPRESENTATION_ITEM()
RATIONAL_B_SPLINE_CURVE((1.13426390111302,1.13389822901296,1.13348223894561))
REPRESENTATION_ITEM('')
);
#691=(
BOUNDED_CURVE()
B_SPLINE_CURVE(2,(#51765,#51766,#51767),.UNSPECIFIED.,.F.,.F.)
B_SPLINE_CURVE_WITH_KNOTS((3,3),(0.271548216895913,0.277734227531896),
 .UNSPECIFIED.)
CURVE()
GEOMETRIC_REPRESENTATION_ITEM()
RATIONAL_B_SPLINE_CURVE((1.13348223894608,1.13389822901343,1.1342639011135))
REPRESENTATION_ITEM('')
);
#692=(
BOUNDED_CURVE()
B_SPLINE_CURVE(2,(#51771,#51772,#51773),.UNSPECIFIED.,.F.,.F.)
B_SPLINE_CURVE_WITH_KNOTS((3,3),(0.367644516946558,0.373830527582535),
 .UNSPECIFIED.)
CURVE()
GEOMETRIC_REPRESENTATION_ITEM()
RATIONAL_B_SPLINE_CURVE((1.13426390111305,1.13389822901298,1.13348223894563))
REPRESENTATION_ITEM('')
);
#693=(
BOUNDED_CURVE()
B_SPLINE_CURVE(2,(#51777,#51778,#51779),.UNSPECIFIED.,.F.,.F.)
B_SPLINE_CURVE_WITH_KNOTS((3,3),(0.271548216895911,0.277734227531902),
 .UNSPECIFIED.)
CURVE()
GEOMETRIC_REPRESENTATION_ITEM()
RATIONAL_B_SPLINE_CURVE((1.13348223894613,1.13389822901348,1.13426390111355))
REPRESENTATION_ITEM('')
);
#694=(
BOUNDED_CURVE()
B_SPLINE_CURVE(2,(#51783,#51784,#51785),.UNSPECIFIED.,.F.,.F.)
B_SPLINE_CURVE_WITH_KNOTS((3,3),(0.367644516946552,0.373830527582527),
 .UNSPECIFIED.)
CURVE()
GEOMETRIC_REPRESENTATION_ITEM()
RATIONAL_B_SPLINE_CURVE((1.13426390111308,1.13389822901301,1.13348223894567))
REPRESENTATION_ITEM('')
);
#695=(
BOUNDED_CURVE()
B_SPLINE_CURVE(2,(#51789,#51790,#51791),.UNSPECIFIED.,.F.,.F.)
B_SPLINE_CURVE_WITH_KNOTS((3,3),(0.271548216895913,0.277734227531896),
 .UNSPECIFIED.)
CURVE()
GEOMETRIC_REPRESENTATION_ITEM()
RATIONAL_B_SPLINE_CURVE((1.13348223894609,1.13389822901344,1.13426390111351))
REPRESENTATION_ITEM('')
);
#696=(
BOUNDED_CURVE()
B_SPLINE_CURVE(2,(#51795,#51796,#51797),.UNSPECIFIED.,.F.,.F.)
B_SPLINE_CURVE_WITH_KNOTS((3,3),(0.367644516946554,0.373830527582527),
 .UNSPECIFIED.)
CURVE()
GEOMETRIC_REPRESENTATION_ITEM()
RATIONAL_B_SPLINE_CURVE((1.13426390111307,1.13389822901301,1.13348223894566))
REPRESENTATION_ITEM('')
);
#697=(
BOUNDED_CURVE()
B_SPLINE_CURVE(2,(#51801,#51802,#51803),.UNSPECIFIED.,.F.,.F.)
B_SPLINE_CURVE_WITH_KNOTS((3,3),(0.271548216895912,0.277734227531901),
 .UNSPECIFIED.)
CURVE()
GEOMETRIC_REPRESENTATION_ITEM()
RATIONAL_B_SPLINE_CURVE((1.13348223894619,1.13389822901354,1.13426390111361))
REPRESENTATION_ITEM('')
);
#698=(
BOUNDED_CURVE()
B_SPLINE_CURVE(2,(#51807,#51808,#51809),.UNSPECIFIED.,.F.,.F.)
B_SPLINE_CURVE_WITH_KNOTS((3,3),(0.367644516946552,0.373830527582526),
 .UNSPECIFIED.)
CURVE()
GEOMETRIC_REPRESENTATION_ITEM()
RATIONAL_B_SPLINE_CURVE((1.13426390111306,1.13389822901299,1.13348223894565))
REPRESENTATION_ITEM('')
);
#699=(
BOUNDED_CURVE()
B_SPLINE_CURVE(2,(#51813,#51814,#51815),.UNSPECIFIED.,.F.,.F.)
B_SPLINE_CURVE_WITH_KNOTS((3,3),(0.271548216895908,0.277734227531896),
 .UNSPECIFIED.)
CURVE()
GEOMETRIC_REPRESENTATION_ITEM()
RATIONAL_B_SPLINE_CURVE((1.13348223894609,1.13389822901344,1.13426390111351))
REPRESENTATION_ITEM('')
);
#700=(
BOUNDED_CURVE()
B_SPLINE_CURVE(2,(#51819,#51820,#51821),.UNSPECIFIED.,.F.,.F.)
B_SPLINE_CURVE_WITH_KNOTS((3,3),(0.367644516946558,0.373830527582532),
 .UNSPECIFIED.)
CURVE()
GEOMETRIC_REPRESENTATION_ITEM()
RATIONAL_B_SPLINE_CURVE((1.13426390111305,1.13389822901298,1.13348223894564))
REPRESENTATION_ITEM('')
);
#701=(
BOUNDED_CURVE()
B_SPLINE_CURVE(2,(#51825,#51826,#51827),.UNSPECIFIED.,.F.,.F.)
B_SPLINE_CURVE_WITH_KNOTS((3,3),(0.271548216895918,0.27773422753191),
 .UNSPECIFIED.)
CURVE()
GEOMETRIC_REPRESENTATION_ITEM()
RATIONAL_B_SPLINE_CURVE((1.1334822389462,1.13389822901355,1.13426390111362))
REPRESENTATION_ITEM('')
);
#702=(
BOUNDED_CURVE()
B_SPLINE_CURVE(2,(#51831,#51832,#51833),.UNSPECIFIED.,.F.,.F.)
B_SPLINE_CURVE_WITH_KNOTS((3,3),(0.367644516946559,0.373830527582532),
 .UNSPECIFIED.)
CURVE()
GEOMETRIC_REPRESENTATION_ITEM()
RATIONAL_B_SPLINE_CURVE((1.13426390111305,1.13389822901299,1.13348223894564))
REPRESENTATION_ITEM('')
);
#703=(
BOUNDED_CURVE()
B_SPLINE_CURVE(2,(#51837,#51838,#51839),.UNSPECIFIED.,.F.,.F.)
B_SPLINE_CURVE_WITH_KNOTS((3,3),(0.271548216895917,0.277734227531899),
 .UNSPECIFIED.)
CURVE()
GEOMETRIC_REPRESENTATION_ITEM()
RATIONAL_B_SPLINE_CURVE((1.13348223894612,1.13389822901347,1.13426390111355))
REPRESENTATION_ITEM('')
);
#704=(
BOUNDED_CURVE()
B_SPLINE_CURVE(2,(#51843,#51844,#51845),.UNSPECIFIED.,.F.,.F.)
B_SPLINE_CURVE_WITH_KNOTS((3,3),(0.367644516946562,0.373830527582533),
 .UNSPECIFIED.)
CURVE()
GEOMETRIC_REPRESENTATION_ITEM()
RATIONAL_B_SPLINE_CURVE((1.13426390111306,1.13389822901299,1.13348223894564))
REPRESENTATION_ITEM('')
);
#705=(
BOUNDED_CURVE()
B_SPLINE_CURVE(2,(#51849,#51850,#51851),.UNSPECIFIED.,.F.,.F.)
B_SPLINE_CURVE_WITH_KNOTS((3,3),(0.271548216895905,0.277734227531891),
 .UNSPECIFIED.)
CURVE()
GEOMETRIC_REPRESENTATION_ITEM()
RATIONAL_B_SPLINE_CURVE((1.13348223894609,1.13389822901344,1.13426390111351))
REPRESENTATION_ITEM('')
);
#706=(
BOUNDED_CURVE()
B_SPLINE_CURVE(2,(#51855,#51856,#51857),.UNSPECIFIED.,.F.,.F.)
B_SPLINE_CURVE_WITH_KNOTS((3,3),(0.367644516946557,0.373830527582533),
 .UNSPECIFIED.)
CURVE()
GEOMETRIC_REPRESENTATION_ITEM()
RATIONAL_B_SPLINE_CURVE((1.13426390111305,1.13389822901299,1.13348223894564))
REPRESENTATION_ITEM('')
);
#707=(
BOUNDED_CURVE()
B_SPLINE_CURVE(2,(#51861,#51862,#51863),.UNSPECIFIED.,.F.,.F.)
B_SPLINE_CURVE_WITH_KNOTS((3,3),(0.271548216895918,0.277734227531906),
 .UNSPECIFIED.)
CURVE()
GEOMETRIC_REPRESENTATION_ITEM()
RATIONAL_B_SPLINE_CURVE((1.13348223894616,1.13389822901351,1.13426390111358))
REPRESENTATION_ITEM('')
);
#708=(
BOUNDED_CURVE()
B_SPLINE_CURVE(2,(#51885,#51886,#51887),.UNSPECIFIED.,.F.,.F.)
B_SPLINE_CURVE_WITH_KNOTS((3,3),(0.376641898803529,0.382940702095941),
 .UNSPECIFIED.)
CURVE()
GEOMETRIC_REPRESENTATION_ITEM()
RATIONAL_B_SPLINE_CURVE((1.12071541658433,1.1202411994692,1.11971735964528))
REPRESENTATION_ITEM('')
);
#709=(
BOUNDED_CURVE()
B_SPLINE_CURVE(2,(#51891,#51892,#51893),.UNSPECIFIED.,.F.,.F.)
B_SPLINE_CURVE_WITH_KNOTS((3,3),(0.249954652430657,0.25625345571807),
 .UNSPECIFIED.)
CURVE()
GEOMETRIC_REPRESENTATION_ITEM()
RATIONAL_B_SPLINE_CURVE((1.1197173596462,1.12024119946966,1.12071541658442))
REPRESENTATION_ITEM('')
);
#710=(
BOUNDED_CURVE()
B_SPLINE_CURVE(2,(#51897,#51898,#51899),.UNSPECIFIED.,.F.,.F.)
B_SPLINE_CURVE_WITH_KNOTS((3,3),(0.376641898803524,0.382940702095934),
 .UNSPECIFIED.)
CURVE()
GEOMETRIC_REPRESENTATION_ITEM()
RATIONAL_B_SPLINE_CURVE((1.12071541658448,1.12024119946934,1.11971735964542))
REPRESENTATION_ITEM('')
);
#711=(
BOUNDED_CURVE()
B_SPLINE_CURVE(2,(#51903,#51904,#51905),.UNSPECIFIED.,.F.,.F.)
B_SPLINE_CURVE_WITH_KNOTS((3,3),(0.249954652430655,0.256253455718069),
 .UNSPECIFIED.)
CURVE()
GEOMETRIC_REPRESENTATION_ITEM()
RATIONAL_B_SPLINE_CURVE((1.11971735964613,1.1202411994696,1.12071541658435))
REPRESENTATION_ITEM('')
);
#712=(
BOUNDED_CURVE()
B_SPLINE_CURVE(2,(#51909,#51910,#51911),.UNSPECIFIED.,.F.,.F.)
B_SPLINE_CURVE_WITH_KNOTS((3,3),(0.376641898803532,0.382940702095944),
 .UNSPECIFIED.)
CURVE()
GEOMETRIC_REPRESENTATION_ITEM()
RATIONAL_B_SPLINE_CURVE((1.12071541658434,1.12024119946921,1.11971735964529))
REPRESENTATION_ITEM('')
);
#713=(
BOUNDED_CURVE()
B_SPLINE_CURVE(2,(#51915,#51916,#51917),.UNSPECIFIED.,.F.,.F.)
B_SPLINE_CURVE_WITH_KNOTS((3,3),(0.249954652430645,0.256253455718059),
 .UNSPECIFIED.)
CURVE()
GEOMETRIC_REPRESENTATION_ITEM()
RATIONAL_B_SPLINE_CURVE((1.11971735964598,1.12024119946945,1.1207154165842))
REPRESENTATION_ITEM('')
);
#714=(
BOUNDED_CURVE()
B_SPLINE_CURVE(2,(#51921,#51922,#51923),.UNSPECIFIED.,.F.,.F.)
B_SPLINE_CURVE_WITH_KNOTS((3,3),(0.376641898803521,0.382940702095933),
 .UNSPECIFIED.)
CURVE()
GEOMETRIC_REPRESENTATION_ITEM()
RATIONAL_B_SPLINE_CURVE((1.1207154165845,1.12024119946936,1.11971735964544))
REPRESENTATION_ITEM('')
);
#715=(
BOUNDED_CURVE()
B_SPLINE_CURVE(2,(#51927,#51928,#51929),.UNSPECIFIED.,.F.,.F.)
B_SPLINE_CURVE_WITH_KNOTS((3,3),(0.249954652430661,0.256253455718076),
 .UNSPECIFIED.)
CURVE()
GEOMETRIC_REPRESENTATION_ITEM()
RATIONAL_B_SPLINE_CURVE((1.1197173596463,1.12024119946977,1.12071541658453))
REPRESENTATION_ITEM('')
);
#716=(
BOUNDED_CURVE()
B_SPLINE_CURVE(2,(#51933,#51934,#51935),.UNSPECIFIED.,.F.,.F.)
B_SPLINE_CURVE_WITH_KNOTS((3,3),(0.376641898803535,0.382940702095943),
 .UNSPECIFIED.)
CURVE()
GEOMETRIC_REPRESENTATION_ITEM()
RATIONAL_B_SPLINE_CURVE((1.12071541658437,1.12024119946923,1.11971735964532))
REPRESENTATION_ITEM('')
);
#717=(
BOUNDED_CURVE()
B_SPLINE_CURVE(2,(#51939,#51940,#51941),.UNSPECIFIED.,.F.,.F.)
B_SPLINE_CURVE_WITH_KNOTS((3,3),(0.249954652430645,0.256253455718058),
 .UNSPECIFIED.)
CURVE()
GEOMETRIC_REPRESENTATION_ITEM()
RATIONAL_B_SPLINE_CURVE((1.11971735964609,1.12024119946955,1.12071541658431))
REPRESENTATION_ITEM('')
);
#718=(
BOUNDED_CURVE()
B_SPLINE_CURVE(2,(#51945,#51946,#51947),.UNSPECIFIED.,.F.,.F.)
B_SPLINE_CURVE_WITH_KNOTS((3,3),(0.376641898803531,0.382940702095942),
 .UNSPECIFIED.)
CURVE()
GEOMETRIC_REPRESENTATION_ITEM()
RATIONAL_B_SPLINE_CURVE((1.12071541658437,1.12024119946923,1.11971735964532))
REPRESENTATION_ITEM('')
);
#719=(
BOUNDED_CURVE()
B_SPLINE_CURVE(2,(#51951,#51952,#51953),.UNSPECIFIED.,.F.,.F.)
B_SPLINE_CURVE_WITH_KNOTS((3,3),(0.249954652430646,0.256253455718059),
 .UNSPECIFIED.)
CURVE()
GEOMETRIC_REPRESENTATION_ITEM()
RATIONAL_B_SPLINE_CURVE((1.11971735964605,1.12024119946951,1.12071541658427))
REPRESENTATION_ITEM('')
);
#720=(
BOUNDED_CURVE()
B_SPLINE_CURVE(2,(#51957,#51958,#51959),.UNSPECIFIED.,.F.,.F.)
B_SPLINE_CURVE_WITH_KNOTS((3,3),(0.376641898803521,0.382940702095931),
 .UNSPECIFIED.)
CURVE()
GEOMETRIC_REPRESENTATION_ITEM()
RATIONAL_B_SPLINE_CURVE((1.12071541658451,1.12024119946938,1.11971735964546))
REPRESENTATION_ITEM('')
);
#721=(
BOUNDED_CURVE()
B_SPLINE_CURVE(2,(#51963,#51964,#51965),.UNSPECIFIED.,.F.,.F.)
B_SPLINE_CURVE_WITH_KNOTS((3,3),(0.249954652430639,0.256253455718052),
 .UNSPECIFIED.)
CURVE()
GEOMETRIC_REPRESENTATION_ITEM()
RATIONAL_B_SPLINE_CURVE((1.11971735964601,1.12024119946948,1.12071541658424))
REPRESENTATION_ITEM('')
);
#722=(
BOUNDED_CURVE()
B_SPLINE_CURVE(2,(#51969,#51970,#51971),.UNSPECIFIED.,.F.,.F.)
B_SPLINE_CURVE_WITH_KNOTS((3,3),(0.376641898803533,0.382940702095945),
 .UNSPECIFIED.)
CURVE()
GEOMETRIC_REPRESENTATION_ITEM()
RATIONAL_B_SPLINE_CURVE((1.12071541658434,1.1202411994692,1.11971735964528))
REPRESENTATION_ITEM('')
);
#723=(
BOUNDED_CURVE()
B_SPLINE_CURVE(2,(#51975,#51976,#51977),.UNSPECIFIED.,.F.,.F.)
B_SPLINE_CURVE_WITH_KNOTS((3,3),(0.249954652430659,0.256253455718072),
 .UNSPECIFIED.)
CURVE()
GEOMETRIC_REPRESENTATION_ITEM()
RATIONAL_B_SPLINE_CURVE((1.11971735964624,1.12024119946971,1.12071541658447))
REPRESENTATION_ITEM('')
);
#724=(
BOUNDED_CURVE()
B_SPLINE_CURVE(2,(#51981,#51982,#51983),.UNSPECIFIED.,.F.,.F.)
B_SPLINE_CURVE_WITH_KNOTS((3,3),(0.376641898803529,0.382940702095948),
 .UNSPECIFIED.)
CURVE()
GEOMETRIC_REPRESENTATION_ITEM()
RATIONAL_B_SPLINE_CURVE((1.12071541658446,1.12024119946932,1.1197173596454))
REPRESENTATION_ITEM('')
);
#725=(
BOUNDED_CURVE()
B_SPLINE_CURVE(2,(#51987,#51988,#51989),.UNSPECIFIED.,.F.,.F.)
B_SPLINE_CURVE_WITH_KNOTS((3,3),(0.249954652430643,0.256253455718057),
 .UNSPECIFIED.)
CURVE()
GEOMETRIC_REPRESENTATION_ITEM()
RATIONAL_B_SPLINE_CURVE((1.11971735964609,1.12024119946956,1.12071541658432))
REPRESENTATION_ITEM('')
);
#726=(
BOUNDED_CURVE()
B_SPLINE_CURVE(2,(#51993,#51994,#51995),.UNSPECIFIED.,.F.,.F.)
B_SPLINE_CURVE_WITH_KNOTS((3,3),(0.376641898803523,0.382940702095941),
 .UNSPECIFIED.)
CURVE()
GEOMETRIC_REPRESENTATION_ITEM()
RATIONAL_B_SPLINE_CURVE((1.12071541658451,1.12024119946937,1.11971735964545))
REPRESENTATION_ITEM('')
);
#727=(
BOUNDED_CURVE()
B_SPLINE_CURVE(2,(#51999,#52000,#52001),.UNSPECIFIED.,.F.,.F.)
B_SPLINE_CURVE_WITH_KNOTS((3,3),(0.249954652430644,0.256253455718058),
 .UNSPECIFIED.)
CURVE()
GEOMETRIC_REPRESENTATION_ITEM()
RATIONAL_B_SPLINE_CURVE((1.11971735964615,1.12024119946961,1.12071541658437))
REPRESENTATION_ITEM('')
);
#728=(
BOUNDED_CURVE()
B_SPLINE_CURVE(2,(#52005,#52006,#52007),.UNSPECIFIED.,.F.,.F.)
B_SPLINE_CURVE_WITH_KNOTS((3,3),(0.376641898803536,0.382940702095946),
 .UNSPECIFIED.)
CURVE()
GEOMETRIC_REPRESENTATION_ITEM()
RATIONAL_B_SPLINE_CURVE((1.12071541658451,1.12024119946938,1.11971735964546))
REPRESENTATION_ITEM('')
);
#729=(
BOUNDED_CURVE()
B_SPLINE_CURVE(2,(#52011,#52012,#52013),.UNSPECIFIED.,.F.,.F.)
B_SPLINE_CURVE_WITH_KNOTS((3,3),(0.24995465243065,0.256253455718062),
 .UNSPECIFIED.)
CURVE()
GEOMETRIC_REPRESENTATION_ITEM()
RATIONAL_B_SPLINE_CURVE((1.11971735964599,1.12024119946946,1.12071541658421))
REPRESENTATION_ITEM('')
);
#730=(
BOUNDED_CURVE()
B_SPLINE_CURVE(2,(#52017,#52018,#52019),.UNSPECIFIED.,.F.,.F.)
B_SPLINE_CURVE_WITH_KNOTS((3,3),(0.376641898803523,0.38294070209593),
 .UNSPECIFIED.)
CURVE()
GEOMETRIC_REPRESENTATION_ITEM()
RATIONAL_B_SPLINE_CURVE((1.1207154165845,1.12024119946936,1.11971735964544))
REPRESENTATION_ITEM('')
);
#731=(
BOUNDED_CURVE()
B_SPLINE_CURVE(2,(#52023,#52024,#52025),.UNSPECIFIED.,.F.,.F.)
B_SPLINE_CURVE_WITH_KNOTS((3,3),(0.249954652430653,0.256253455718064),
 .UNSPECIFIED.)
CURVE()
GEOMETRIC_REPRESENTATION_ITEM()
RATIONAL_B_SPLINE_CURVE((1.11971735964611,1.12024119946957,1.12071541658433))
REPRESENTATION_ITEM('')
);
#732=(
BOUNDED_CURVE()
B_SPLINE_CURVE(2,(#52029,#52030,#52031),.UNSPECIFIED.,.F.,.F.)
B_SPLINE_CURVE_WITH_KNOTS((3,3),(0.376641898803521,0.382940702095931),
 .UNSPECIFIED.)
CURVE()
GEOMETRIC_REPRESENTATION_ITEM()
RATIONAL_B_SPLINE_CURVE((1.12071541658461,1.12024119946947,1.11971735964555))
REPRESENTATION_ITEM('')
);
#733=(
BOUNDED_CURVE()
B_SPLINE_CURVE(2,(#52035,#52036,#52037),.UNSPECIFIED.,.F.,.F.)
B_SPLINE_CURVE_WITH_KNOTS((3,3),(0.249954652430661,0.256253455718072),
 .UNSPECIFIED.)
CURVE()
GEOMETRIC_REPRESENTATION_ITEM()
RATIONAL_B_SPLINE_CURVE((1.11971735964623,1.1202411994697,1.12071541658446))
REPRESENTATION_ITEM('')
);
#734=(
BOUNDED_CURVE()
B_SPLINE_CURVE(2,(#52041,#52042,#52043),.UNSPECIFIED.,.F.,.F.)
B_SPLINE_CURVE_WITH_KNOTS((3,3),(0.376641898803537,0.382940702095947),
 .UNSPECIFIED.)
CURVE()
GEOMETRIC_REPRESENTATION_ITEM()
RATIONAL_B_SPLINE_CURVE((1.1207154165845,1.12024119946936,1.11971735964544))
REPRESENTATION_ITEM('')
);
#735=(
BOUNDED_CURVE()
B_SPLINE_CURVE(2,(#52047,#52048,#52049),.UNSPECIFIED.,.F.,.F.)
B_SPLINE_CURVE_WITH_KNOTS((3,3),(0.249954652430645,0.256253455718056),
 .UNSPECIFIED.)
CURVE()
GEOMETRIC_REPRESENTATION_ITEM()
RATIONAL_B_SPLINE_CURVE((1.11971735964613,1.1202411994696,1.12071541658435))
REPRESENTATION_ITEM('')
);
#736=(
BOUNDED_CURVE()
B_SPLINE_CURVE(2,(#52053,#52054,#52055),.UNSPECIFIED.,.F.,.F.)
B_SPLINE_CURVE_WITH_KNOTS((3,3),(0.376641898803536,0.382940702095954),
 .UNSPECIFIED.)
CURVE()
GEOMETRIC_REPRESENTATION_ITEM()
RATIONAL_B_SPLINE_CURVE((1.12071541658435,1.12024119946922,1.1197173596453))
REPRESENTATION_ITEM('')
);
#737=(
BOUNDED_CURVE()
B_SPLINE_CURVE(2,(#52059,#52060,#52061),.UNSPECIFIED.,.F.,.F.)
B_SPLINE_CURVE_WITH_KNOTS((3,3),(0.249954652430663,0.256253455718072),
 .UNSPECIFIED.)
CURVE()
GEOMETRIC_REPRESENTATION_ITEM()
RATIONAL_B_SPLINE_CURVE((1.11971735964633,1.1202411994698,1.12071541658456))
REPRESENTATION_ITEM('')
);
#738=(
BOUNDED_CURVE()
B_SPLINE_CURVE(2,(#52065,#52066,#52067),.UNSPECIFIED.,.F.,.F.)
B_SPLINE_CURVE_WITH_KNOTS((3,3),(0.376641898803512,0.382940702095922),
 .UNSPECIFIED.)
CURVE()
GEOMETRIC_REPRESENTATION_ITEM()
RATIONAL_B_SPLINE_CURVE((1.12071541658461,1.12024119946947,1.11971735964555))
REPRESENTATION_ITEM('')
);
#739=(
BOUNDED_CURVE()
B_SPLINE_CURVE(2,(#52071,#52072,#52073),.UNSPECIFIED.,.F.,.F.)
B_SPLINE_CURVE_WITH_KNOTS((3,3),(0.249954652430648,0.256253455718062),
 .UNSPECIFIED.)
CURVE()
GEOMETRIC_REPRESENTATION_ITEM()
RATIONAL_B_SPLINE_CURVE((1.11971735964605,1.12024119946951,1.12071541658427))
REPRESENTATION_ITEM('')
);
#740=(
BOUNDED_CURVE()
B_SPLINE_CURVE(2,(#52077,#52078,#52079),.UNSPECIFIED.,.F.,.F.)
B_SPLINE_CURVE_WITH_KNOTS((3,3),(0.376641898803527,0.382940702095944),
 .UNSPECIFIED.)
CURVE()
GEOMETRIC_REPRESENTATION_ITEM()
RATIONAL_B_SPLINE_CURVE((1.12071541658444,1.12024119946931,1.11971735964539))
REPRESENTATION_ITEM('')
);
#741=(
BOUNDED_CURVE()
B_SPLINE_CURVE(2,(#52083,#52084,#52085),.UNSPECIFIED.,.F.,.F.)
B_SPLINE_CURVE_WITH_KNOTS((3,3),(0.24995465243065,0.256253455718066),
 .UNSPECIFIED.)
CURVE()
GEOMETRIC_REPRESENTATION_ITEM()
RATIONAL_B_SPLINE_CURVE((1.11971735964612,1.12024119946958,1.12071541658434))
REPRESENTATION_ITEM('')
);
#742=(
BOUNDED_CURVE()
B_SPLINE_CURVE(2,(#52089,#52090,#52091),.UNSPECIFIED.,.F.,.F.)
B_SPLINE_CURVE_WITH_KNOTS((3,3),(0.37664189880352,0.382940702095936),
 .UNSPECIFIED.)
CURVE()
GEOMETRIC_REPRESENTATION_ITEM()
RATIONAL_B_SPLINE_CURVE((1.12071541658452,1.12024119946938,1.11971735964546))
REPRESENTATION_ITEM('')
);
#743=(
BOUNDED_CURVE()
B_SPLINE_CURVE(2,(#52095,#52096,#52097),.UNSPECIFIED.,.F.,.F.)
B_SPLINE_CURVE_WITH_KNOTS((3,3),(0.249954652430664,0.25625345571808),
 .UNSPECIFIED.)
CURVE()
GEOMETRIC_REPRESENTATION_ITEM()
RATIONAL_B_SPLINE_CURVE((1.11971735964628,1.12024119946975,1.12071541658451))
REPRESENTATION_ITEM('')
);
#744=(
BOUNDED_CURVE()
B_SPLINE_CURVE(2,(#52101,#52102,#52103),.UNSPECIFIED.,.F.,.F.)
B_SPLINE_CURVE_WITH_KNOTS((3,3),(0.376641898803518,0.382940702095937),
 .UNSPECIFIED.)
CURVE()
GEOMETRIC_REPRESENTATION_ITEM()
RATIONAL_B_SPLINE_CURVE((1.12071541658454,1.12024119946941,1.11971735964549))
REPRESENTATION_ITEM('')
);
#745=(
BOUNDED_CURVE()
B_SPLINE_CURVE(2,(#52107,#52108,#52109),.UNSPECIFIED.,.F.,.F.)
B_SPLINE_CURVE_WITH_KNOTS((3,3),(0.249954652430639,0.256253455718056),
 .UNSPECIFIED.)
CURVE()
GEOMETRIC_REPRESENTATION_ITEM()
RATIONAL_B_SPLINE_CURVE((1.11971735964609,1.12024119946956,1.12071541658432))
REPRESENTATION_ITEM('')
);
#746=(
BOUNDED_CURVE()
B_SPLINE_CURVE(2,(#52113,#52114,#52115),.UNSPECIFIED.,.F.,.F.)
B_SPLINE_CURVE_WITH_KNOTS((3,3),(0.376641898803522,0.382940702095936),
 .UNSPECIFIED.)
CURVE()
GEOMETRIC_REPRESENTATION_ITEM()
RATIONAL_B_SPLINE_CURVE((1.12071541658447,1.12024119946934,1.11971735964542))
REPRESENTATION_ITEM('')
);
#747=(
BOUNDED_CURVE()
B_SPLINE_CURVE(2,(#52119,#52120,#52121),.UNSPECIFIED.,.F.,.F.)
B_SPLINE_CURVE_WITH_KNOTS((3,3),(0.249954652430657,0.256253455718066),
 .UNSPECIFIED.)
CURVE()
GEOMETRIC_REPRESENTATION_ITEM()
RATIONAL_B_SPLINE_CURVE((1.11971735964622,1.12024119946968,1.12071541658444))
REPRESENTATION_ITEM('')
);
#748=(
BOUNDED_CURVE()
B_SPLINE_CURVE(2,(#52125,#52126,#52127),.UNSPECIFIED.,.F.,.F.)
B_SPLINE_CURVE_WITH_KNOTS((3,3),(0.376641898803533,0.38294070209594),
 .UNSPECIFIED.)
CURVE()
GEOMETRIC_REPRESENTATION_ITEM()
RATIONAL_B_SPLINE_CURVE((1.12071541658433,1.1202411994692,1.11971735964528))
REPRESENTATION_ITEM('')
);
#749=(
BOUNDED_CURVE()
B_SPLINE_CURVE(2,(#52131,#52132,#52133),.UNSPECIFIED.,.F.,.F.)
B_SPLINE_CURVE_WITH_KNOTS((3,3),(0.249954652430642,0.256253455718055),
 .UNSPECIFIED.)
CURVE()
GEOMETRIC_REPRESENTATION_ITEM()
RATIONAL_B_SPLINE_CURVE((1.11971735964602,1.12024119946948,1.12071541658424))
REPRESENTATION_ITEM('')
);
#750=(
BOUNDED_CURVE()
B_SPLINE_CURVE(2,(#52137,#52138,#52139),.UNSPECIFIED.,.F.,.F.)
B_SPLINE_CURVE_WITH_KNOTS((3,3),(0.376641898803547,0.382940702095962),
 .UNSPECIFIED.)
CURVE()
GEOMETRIC_REPRESENTATION_ITEM()
RATIONAL_B_SPLINE_CURVE((1.12071541658418,1.12024119946904,1.11971735964512))
REPRESENTATION_ITEM('')
);
#751=(
BOUNDED_CURVE()
B_SPLINE_CURVE(2,(#52143,#52144,#52145),.UNSPECIFIED.,.F.,.F.)
B_SPLINE_CURVE_WITH_KNOTS((3,3),(0.249954652430658,0.256253455718078),
 .UNSPECIFIED.)
CURVE()
GEOMETRIC_REPRESENTATION_ITEM()
RATIONAL_B_SPLINE_CURVE((1.1197173596463,1.12024119946977,1.12071541658453))
REPRESENTATION_ITEM('')
);
#752=(
BOUNDED_CURVE()
B_SPLINE_CURVE(2,(#52149,#52150,#52151),.UNSPECIFIED.,.F.,.F.)
B_SPLINE_CURVE_WITH_KNOTS((3,3),(0.376641898803522,0.382940702095938),
 .UNSPECIFIED.)
CURVE()
GEOMETRIC_REPRESENTATION_ITEM()
RATIONAL_B_SPLINE_CURVE((1.12071541658451,1.12024119946937,1.11971735964545))
REPRESENTATION_ITEM('')
);
#753=(
BOUNDED_CURVE()
B_SPLINE_CURVE(2,(#52155,#52156,#52157),.UNSPECIFIED.,.F.,.F.)
B_SPLINE_CURVE_WITH_KNOTS((3,3),(0.249954652430655,0.25625345571807),
 .UNSPECIFIED.)
CURVE()
GEOMETRIC_REPRESENTATION_ITEM()
RATIONAL_B_SPLINE_CURVE((1.11971735964625,1.12024119946971,1.12071541658447))
REPRESENTATION_ITEM('')
);
#754=(
BOUNDED_CURVE()
B_SPLINE_CURVE(2,(#52161,#52162,#52163),.UNSPECIFIED.,.F.,.F.)
B_SPLINE_CURVE_WITH_KNOTS((3,3),(0.376641898803531,0.382940702095945),
 .UNSPECIFIED.)
CURVE()
GEOMETRIC_REPRESENTATION_ITEM()
RATIONAL_B_SPLINE_CURVE((1.12071541658432,1.12024119946919,1.11971735964527))
REPRESENTATION_ITEM('')
);
#755=(
BOUNDED_CURVE()
B_SPLINE_CURVE(2,(#52167,#52168,#52169),.UNSPECIFIED.,.F.,.F.)
B_SPLINE_CURVE_WITH_KNOTS((3,3),(0.249954652430637,0.256253455718055),
 .UNSPECIFIED.)
CURVE()
GEOMETRIC_REPRESENTATION_ITEM()
RATIONAL_B_SPLINE_CURVE((1.11971735964599,1.12024119946945,1.12071541658421))
REPRESENTATION_ITEM('')
);
#756=(
BOUNDED_CURVE()
B_SPLINE_CURVE(2,(#52173,#52174,#52175),.UNSPECIFIED.,.F.,.F.)
B_SPLINE_CURVE_WITH_KNOTS((3,3),(0.376641898803544,0.382940702095957),
 .UNSPECIFIED.)
CURVE()
GEOMETRIC_REPRESENTATION_ITEM()
RATIONAL_B_SPLINE_CURVE((1.12071541658422,1.12024119946908,1.11971735964516))
REPRESENTATION_ITEM('')
);
#757=(
BOUNDED_CURVE()
B_SPLINE_CURVE(2,(#52179,#52180,#52181),.UNSPECIFIED.,.F.,.F.)
B_SPLINE_CURVE_WITH_KNOTS((3,3),(0.249954652430653,0.256253455718062),
 .UNSPECIFIED.)
CURVE()
GEOMETRIC_REPRESENTATION_ITEM()
RATIONAL_B_SPLINE_CURVE((1.11971735964616,1.12024119946962,1.12071541658438))
REPRESENTATION_ITEM('')
);
#758=(
BOUNDED_CURVE()
B_SPLINE_CURVE(2,(#52185,#52186,#52187),.UNSPECIFIED.,.F.,.F.)
B_SPLINE_CURVE_WITH_KNOTS((3,3),(0.376641898803539,0.38294070209595),
 .UNSPECIFIED.)
CURVE()
GEOMETRIC_REPRESENTATION_ITEM()
RATIONAL_B_SPLINE_CURVE((1.12071541658449,1.12024119946935,1.11971735964543))
REPRESENTATION_ITEM('')
);
#759=(
BOUNDED_CURVE()
B_SPLINE_CURVE(2,(#52191,#52192,#52193),.UNSPECIFIED.,.F.,.F.)
B_SPLINE_CURVE_WITH_KNOTS((3,3),(0.249954652430653,0.256253455718071),
 .UNSPECIFIED.)
CURVE()
GEOMETRIC_REPRESENTATION_ITEM()
RATIONAL_B_SPLINE_CURVE((1.11971735964627,1.12024119946973,1.12071541658449))
REPRESENTATION_ITEM('')
);
#760=(
BOUNDED_CURVE()
B_SPLINE_CURVE(2,(#52197,#52198,#52199),.UNSPECIFIED.,.F.,.F.)
B_SPLINE_CURVE_WITH_KNOTS((3,3),(0.376641898803533,0.382940702095944),
 .UNSPECIFIED.)
CURVE()
GEOMETRIC_REPRESENTATION_ITEM()
RATIONAL_B_SPLINE_CURVE((1.12071541658435,1.12024119946922,1.1197173596453))
REPRESENTATION_ITEM('')
);
#761=(
BOUNDED_CURVE()
B_SPLINE_CURVE(2,(#52203,#52204,#52205),.UNSPECIFIED.,.F.,.F.)
B_SPLINE_CURVE_WITH_KNOTS((3,3),(0.249954652430647,0.256253455718059),
 .UNSPECIFIED.)
CURVE()
GEOMETRIC_REPRESENTATION_ITEM()
RATIONAL_B_SPLINE_CURVE((1.11971735964614,1.12024119946961,1.12071541658437))
REPRESENTATION_ITEM('')
);
#762=(
BOUNDED_CURVE()
B_SPLINE_CURVE(2,(#52209,#52210,#52211),.UNSPECIFIED.,.F.,.F.)
B_SPLINE_CURVE_WITH_KNOTS((3,3),(0.376641898803539,0.382940702095955),
 .UNSPECIFIED.)
CURVE()
GEOMETRIC_REPRESENTATION_ITEM()
RATIONAL_B_SPLINE_CURVE((1.12071541658434,1.1202411994692,1.11971735964528))
REPRESENTATION_ITEM('')
);
#763=(
BOUNDED_CURVE()
B_SPLINE_CURVE(2,(#52215,#52216,#52217),.UNSPECIFIED.,.F.,.F.)
B_SPLINE_CURVE_WITH_KNOTS((3,3),(0.249954652430656,0.256253455718067),
 .UNSPECIFIED.)
CURVE()
GEOMETRIC_REPRESENTATION_ITEM()
RATIONAL_B_SPLINE_CURVE((1.11971735964622,1.12024119946969,1.12071541658444))
REPRESENTATION_ITEM('')
);
#764=(
BOUNDED_CURVE()
B_SPLINE_CURVE(2,(#52221,#52222,#52223),.UNSPECIFIED.,.F.,.F.)
B_SPLINE_CURVE_WITH_KNOTS((3,3),(0.376641898803524,0.382940702095936),
 .UNSPECIFIED.)
CURVE()
GEOMETRIC_REPRESENTATION_ITEM()
RATIONAL_B_SPLINE_CURVE((1.12071541658457,1.12024119946943,1.11971735964551))
REPRESENTATION_ITEM('')
);
#765=(
BOUNDED_CURVE()
B_SPLINE_CURVE(2,(#52227,#52228,#52229),.UNSPECIFIED.,.F.,.F.)
B_SPLINE_CURVE_WITH_KNOTS((3,3),(0.249954652430651,0.256253455718065),
 .UNSPECIFIED.)
CURVE()
GEOMETRIC_REPRESENTATION_ITEM()
RATIONAL_B_SPLINE_CURVE((1.11971735964615,1.12024119946961,1.12071541658437))
REPRESENTATION_ITEM('')
);
#766=(
BOUNDED_CURVE()
B_SPLINE_CURVE(2,(#52233,#52234,#52235),.UNSPECIFIED.,.F.,.F.)
B_SPLINE_CURVE_WITH_KNOTS((3,3),(0.376641898803518,0.382940702095931),
 .UNSPECIFIED.)
CURVE()
GEOMETRIC_REPRESENTATION_ITEM()
RATIONAL_B_SPLINE_CURVE((1.12071541658449,1.12024119946936,1.11971735964544))
REPRESENTATION_ITEM('')
);
#767=(
BOUNDED_CURVE()
B_SPLINE_CURVE(2,(#52239,#52240,#52241),.UNSPECIFIED.,.F.,.F.)
B_SPLINE_CURVE_WITH_KNOTS((3,3),(0.249954652430648,0.256253455718058),
 .UNSPECIFIED.)
CURVE()
GEOMETRIC_REPRESENTATION_ITEM()
RATIONAL_B_SPLINE_CURVE((1.11971735964614,1.1202411994696,1.12071541658436))
REPRESENTATION_ITEM('')
);
#768=(
BOUNDED_CURVE()
B_SPLINE_CURVE(2,(#52245,#52246,#52247),.UNSPECIFIED.,.F.,.F.)
B_SPLINE_CURVE_WITH_KNOTS((3,3),(0.376641898803531,0.382940702095945),
 .UNSPECIFIED.)
CURVE()
GEOMETRIC_REPRESENTATION_ITEM()
RATIONAL_B_SPLINE_CURVE((1.12071541658451,1.12024119946937,1.11971735964545))
REPRESENTATION_ITEM('')
);
#769=(
BOUNDED_CURVE()
B_SPLINE_CURVE(2,(#52251,#52252,#52253),.UNSPECIFIED.,.F.,.F.)
B_SPLINE_CURVE_WITH_KNOTS((3,3),(0.249954652430648,0.256253455718067),
 .UNSPECIFIED.)
CURVE()
GEOMETRIC_REPRESENTATION_ITEM()
RATIONAL_B_SPLINE_CURVE((1.11971735964618,1.12024119946964,1.1207154165844))
REPRESENTATION_ITEM('')
);
#770=(
BOUNDED_CURVE()
B_SPLINE_CURVE(2,(#52257,#52258,#52259),.UNSPECIFIED.,.F.,.F.)
B_SPLINE_CURVE_WITH_KNOTS((3,3),(0.376641898803536,0.382940702095949),
 .UNSPECIFIED.)
CURVE()
GEOMETRIC_REPRESENTATION_ITEM()
RATIONAL_B_SPLINE_CURVE((1.12071541658431,1.12024119946918,1.11971735964526))
REPRESENTATION_ITEM('')
);
#771=(
BOUNDED_CURVE()
B_SPLINE_CURVE(2,(#52263,#52264,#52265),.UNSPECIFIED.,.F.,.F.)
B_SPLINE_CURVE_WITH_KNOTS((3,3),(0.249954652430665,0.256253455718077),
 .UNSPECIFIED.)
CURVE()
GEOMETRIC_REPRESENTATION_ITEM()
RATIONAL_B_SPLINE_CURVE((1.11971735964631,1.12024119946977,1.12071541658453))
REPRESENTATION_ITEM('')
);
#772=(
BOUNDED_CURVE()
B_SPLINE_CURVE(2,(#52269,#52270,#52271),.UNSPECIFIED.,.F.,.F.)
B_SPLINE_CURVE_WITH_KNOTS((3,3),(0.376641898803534,0.382940702095945),
 .UNSPECIFIED.)
CURVE()
GEOMETRIC_REPRESENTATION_ITEM()
RATIONAL_B_SPLINE_CURVE((1.12071541658427,1.12024119946914,1.11971735964522))
REPRESENTATION_ITEM('')
);
#773=(
BOUNDED_CURVE()
B_SPLINE_CURVE(2,(#52275,#52276,#52277),.UNSPECIFIED.,.F.,.F.)
B_SPLINE_CURVE_WITH_KNOTS((3,3),(0.249954652430654,0.256253455718069),
 .UNSPECIFIED.)
CURVE()
GEOMETRIC_REPRESENTATION_ITEM()
RATIONAL_B_SPLINE_CURVE((1.11971735964621,1.12024119946968,1.12071541658444))
REPRESENTATION_ITEM('')
);
#774=(
BOUNDED_CURVE()
B_SPLINE_CURVE(2,(#52281,#52282,#52283),.UNSPECIFIED.,.F.,.F.)
B_SPLINE_CURVE_WITH_KNOTS((3,3),(0.376641898803532,0.382940702095944),
 .UNSPECIFIED.)
CURVE()
GEOMETRIC_REPRESENTATION_ITEM()
RATIONAL_B_SPLINE_CURVE((1.12071541658432,1.12024119946919,1.11971735964527))
REPRESENTATION_ITEM('')
);
#775=(
BOUNDED_CURVE()
B_SPLINE_CURVE(2,(#52287,#52288,#52289),.UNSPECIFIED.,.F.,.F.)
B_SPLINE_CURVE_WITH_KNOTS((3,3),(0.249954652430654,0.256253455718072),
 .UNSPECIFIED.)
CURVE()
GEOMETRIC_REPRESENTATION_ITEM()
RATIONAL_B_SPLINE_CURVE((1.11971735964625,1.12024119946971,1.12071541658447))
REPRESENTATION_ITEM('')
);
#776=(
BOUNDED_CURVE()
B_SPLINE_CURVE(2,(#52293,#52294,#52295),.UNSPECIFIED.,.F.,.F.)
B_SPLINE_CURVE_WITH_KNOTS((3,3),(0.376641898803539,0.382940702095952),
 .UNSPECIFIED.)
CURVE()
GEOMETRIC_REPRESENTATION_ITEM()
RATIONAL_B_SPLINE_CURVE((1.1207154165844,1.12024119946926,1.11971735964534))
REPRESENTATION_ITEM('')
);
#777=(
BOUNDED_CURVE()
B_SPLINE_CURVE(2,(#52299,#52300,#52301),.UNSPECIFIED.,.F.,.F.)
B_SPLINE_CURVE_WITH_KNOTS((3,3),(0.249954652430648,0.256253455718062),
 .UNSPECIFIED.)
CURVE()
GEOMETRIC_REPRESENTATION_ITEM()
RATIONAL_B_SPLINE_CURVE((1.11971735964618,1.12024119946965,1.12071541658441))
REPRESENTATION_ITEM('')
);
#778=(
BOUNDED_CURVE()
B_SPLINE_CURVE(2,(#52305,#52306,#52307),.UNSPECIFIED.,.F.,.F.)
B_SPLINE_CURVE_WITH_KNOTS((3,3),(0.376641898803519,0.382940702095932),
 .UNSPECIFIED.)
CURVE()
GEOMETRIC_REPRESENTATION_ITEM()
RATIONAL_B_SPLINE_CURVE((1.12071541658452,1.12024119946938,1.11971735964546))
REPRESENTATION_ITEM('')
);
#779=(
BOUNDED_CURVE()
B_SPLINE_CURVE(2,(#52311,#52312,#52313),.UNSPECIFIED.,.F.,.F.)
B_SPLINE_CURVE_WITH_KNOTS((3,3),(0.249954652430659,0.256253455718071),
 .UNSPECIFIED.)
CURVE()
GEOMETRIC_REPRESENTATION_ITEM()
RATIONAL_B_SPLINE_CURVE((1.11971735964627,1.12024119946974,1.1207154165845))
REPRESENTATION_ITEM('')
);
#780=(
BOUNDED_CURVE()
B_SPLINE_CURVE(2,(#52317,#52318,#52319),.UNSPECIFIED.,.F.,.F.)
B_SPLINE_CURVE_WITH_KNOTS((3,3),(0.376641898803527,0.382940702095942),
 .UNSPECIFIED.)
CURVE()
GEOMETRIC_REPRESENTATION_ITEM()
RATIONAL_B_SPLINE_CURVE((1.12071541658453,1.1202411994694,1.11971735964547))
REPRESENTATION_ITEM('')
);
#781=(
BOUNDED_CURVE()
B_SPLINE_CURVE(2,(#52323,#52324,#52325),.UNSPECIFIED.,.F.,.F.)
B_SPLINE_CURVE_WITH_KNOTS((3,3),(0.249954652430662,0.256253455718075),
 .UNSPECIFIED.)
CURVE()
GEOMETRIC_REPRESENTATION_ITEM()
RATIONAL_B_SPLINE_CURVE((1.11971735964629,1.12024119946976,1.12071541658452))
REPRESENTATION_ITEM('')
);
#782=(
BOUNDED_CURVE()
B_SPLINE_CURVE(2,(#52329,#52330,#52331),.UNSPECIFIED.,.F.,.F.)
B_SPLINE_CURVE_WITH_KNOTS((3,3),(0.376641898803543,0.382940702095954),
 .UNSPECIFIED.)
CURVE()
GEOMETRIC_REPRESENTATION_ITEM()
RATIONAL_B_SPLINE_CURVE((1.12071541658423,1.1202411994691,1.11971735964518))
REPRESENTATION_ITEM('')
);
#783=(
BOUNDED_CURVE()
B_SPLINE_CURVE(2,(#52335,#52336,#52337),.UNSPECIFIED.,.F.,.F.)
B_SPLINE_CURVE_WITH_KNOTS((3,3),(0.249954652430648,0.256253455718061),
 .UNSPECIFIED.)
CURVE()
GEOMETRIC_REPRESENTATION_ITEM()
RATIONAL_B_SPLINE_CURVE((1.11971735964609,1.12024119946956,1.12071541658431))
REPRESENTATION_ITEM('')
);
#784=(
BOUNDED_CURVE()
B_SPLINE_CURVE(2,(#52341,#52342,#52343),.UNSPECIFIED.,.F.,.F.)
B_SPLINE_CURVE_WITH_KNOTS((3,3),(0.376641898803529,0.382940702095943),
 .UNSPECIFIED.)
CURVE()
GEOMETRIC_REPRESENTATION_ITEM()
RATIONAL_B_SPLINE_CURVE((1.12071541658438,1.12024119946925,1.11971735964533))
REPRESENTATION_ITEM('')
);
#785=(
BOUNDED_CURVE()
B_SPLINE_CURVE(2,(#52347,#52348,#52349),.UNSPECIFIED.,.F.,.F.)
B_SPLINE_CURVE_WITH_KNOTS((3,3),(0.249954652430657,0.256253455718069),
 .UNSPECIFIED.)
CURVE()
GEOMETRIC_REPRESENTATION_ITEM()
RATIONAL_B_SPLINE_CURVE((1.11971735964625,1.12024119946971,1.12071541658447))
REPRESENTATION_ITEM('')
);
#786=(
BOUNDED_CURVE()
B_SPLINE_CURVE(2,(#52353,#52354,#52355),.UNSPECIFIED.,.F.,.F.)
B_SPLINE_CURVE_WITH_KNOTS((3,3),(0.376641898803529,0.382940702095941),
 .UNSPECIFIED.)
CURVE()
GEOMETRIC_REPRESENTATION_ITEM()
RATIONAL_B_SPLINE_CURVE((1.12071541658439,1.12024119946925,1.11971735964533))
REPRESENTATION_ITEM('')
);
#787=(
BOUNDED_CURVE()
B_SPLINE_CURVE(2,(#52359,#52360,#52361),.UNSPECIFIED.,.F.,.F.)
B_SPLINE_CURVE_WITH_KNOTS((3,3),(0.24995465243065,0.256253455718062),
 .UNSPECIFIED.)
CURVE()
GEOMETRIC_REPRESENTATION_ITEM()
RATIONAL_B_SPLINE_CURVE((1.11971735964607,1.12024119946954,1.12071541658429))
REPRESENTATION_ITEM('')
);
#788=(
BOUNDED_CURVE()
B_SPLINE_CURVE(2,(#52365,#52366,#52367),.UNSPECIFIED.,.F.,.F.)
B_SPLINE_CURVE_WITH_KNOTS((3,3),(0.376641898803544,0.382940702095955),
 .UNSPECIFIED.)
CURVE()
GEOMETRIC_REPRESENTATION_ITEM()
RATIONAL_B_SPLINE_CURVE((1.12071541658421,1.12024119946907,1.11971735964515))
REPRESENTATION_ITEM('')
);
#789=(
BOUNDED_CURVE()
B_SPLINE_CURVE(2,(#52371,#52372,#52373),.UNSPECIFIED.,.F.,.F.)
B_SPLINE_CURVE_WITH_KNOTS((3,3),(0.249954652430658,0.256253455718075),
 .UNSPECIFIED.)
CURVE()
GEOMETRIC_REPRESENTATION_ITEM()
RATIONAL_B_SPLINE_CURVE((1.11971735964629,1.12024119946976,1.12071541658452))
REPRESENTATION_ITEM('')
);
#790=(
BOUNDED_CURVE()
B_SPLINE_CURVE(2,(#52377,#52378,#52379),.UNSPECIFIED.,.F.,.F.)
B_SPLINE_CURVE_WITH_KNOTS((3,3),(0.376641898803543,0.382940702095958),
 .UNSPECIFIED.)
CURVE()
GEOMETRIC_REPRESENTATION_ITEM()
RATIONAL_B_SPLINE_CURVE((1.12071541658432,1.12024119946919,1.11971735964527))
REPRESENTATION_ITEM('')
);
#791=(
BOUNDED_CURVE()
B_SPLINE_CURVE(2,(#52383,#52384,#52385),.UNSPECIFIED.,.F.,.F.)
B_SPLINE_CURVE_WITH_KNOTS((3,3),(0.249954652430663,0.256253455718076),
 .UNSPECIFIED.)
CURVE()
GEOMETRIC_REPRESENTATION_ITEM()
RATIONAL_B_SPLINE_CURVE((1.11971735964633,1.12024119946979,1.12071541658455))
REPRESENTATION_ITEM('')
);
#792=(
BOUNDED_CURVE()
B_SPLINE_CURVE(2,(#52389,#52390,#52391),.UNSPECIFIED.,.F.,.F.)
B_SPLINE_CURVE_WITH_KNOTS((3,3),(0.37664189880352,0.382940702095933),
 .UNSPECIFIED.)
CURVE()
GEOMETRIC_REPRESENTATION_ITEM()
RATIONAL_B_SPLINE_CURVE((1.1207154165845,1.12024119946936,1.11971735964544))
REPRESENTATION_ITEM('')
);
#793=(
BOUNDED_CURVE()
B_SPLINE_CURVE(2,(#52395,#52396,#52397),.UNSPECIFIED.,.F.,.F.)
B_SPLINE_CURVE_WITH_KNOTS((3,3),(0.249954652430661,0.256253455718074),
 .UNSPECIFIED.)
CURVE()
GEOMETRIC_REPRESENTATION_ITEM()
RATIONAL_B_SPLINE_CURVE((1.11971735964627,1.12024119946973,1.12071541658449))
REPRESENTATION_ITEM('')
);
#794=(
BOUNDED_CURVE()
B_SPLINE_CURVE(2,(#52401,#52402,#52403),.UNSPECIFIED.,.F.,.F.)
B_SPLINE_CURVE_WITH_KNOTS((3,3),(0.376641898803524,0.382940702095942),
 .UNSPECIFIED.)
CURVE()
GEOMETRIC_REPRESENTATION_ITEM()
RATIONAL_B_SPLINE_CURVE((1.12071541658449,1.12024119946935,1.11971735964543))
REPRESENTATION_ITEM('')
);
#795=(
BOUNDED_CURVE()
B_SPLINE_CURVE(2,(#52407,#52408,#52409),.UNSPECIFIED.,.F.,.F.)
B_SPLINE_CURVE_WITH_KNOTS((3,3),(0.249954652430645,0.256253455718058),
 .UNSPECIFIED.)
CURVE()
GEOMETRIC_REPRESENTATION_ITEM()
RATIONAL_B_SPLINE_CURVE((1.11971735964602,1.12024119946949,1.12071541658425))
REPRESENTATION_ITEM('')
);
#796=(
BOUNDED_CURVE()
B_SPLINE_CURVE(2,(#52413,#52414,#52415),.UNSPECIFIED.,.F.,.F.)
B_SPLINE_CURVE_WITH_KNOTS((3,3),(0.376641898803526,0.382940702095943),
 .UNSPECIFIED.)
CURVE()
GEOMETRIC_REPRESENTATION_ITEM()
RATIONAL_B_SPLINE_CURVE((1.12071541658447,1.12024119946934,1.11971735964542))
REPRESENTATION_ITEM('')
);
#797=(
BOUNDED_CURVE()
B_SPLINE_CURVE(2,(#52419,#52420,#52421),.UNSPECIFIED.,.F.,.F.)
B_SPLINE_CURVE_WITH_KNOTS((3,3),(0.249954652430656,0.25625345571807),
 .UNSPECIFIED.)
CURVE()
GEOMETRIC_REPRESENTATION_ITEM()
RATIONAL_B_SPLINE_CURVE((1.11971735964623,1.12024119946969,1.12071541658445))
REPRESENTATION_ITEM('')
);
#798=(
BOUNDED_CURVE()
B_SPLINE_CURVE(2,(#52425,#52426,#52427),.UNSPECIFIED.,.F.,.F.)
B_SPLINE_CURVE_WITH_KNOTS((3,3),(0.376641898803539,0.382940702095953),
 .UNSPECIFIED.)
CURVE()
GEOMETRIC_REPRESENTATION_ITEM()
RATIONAL_B_SPLINE_CURVE((1.12071541658437,1.12024119946923,1.11971735964531))
REPRESENTATION_ITEM('')
);
#799=(
BOUNDED_CURVE()
B_SPLINE_CURVE(2,(#52431,#52432,#52433),.UNSPECIFIED.,.F.,.F.)
B_SPLINE_CURVE_WITH_KNOTS((3,3),(0.249954652430661,0.256253455718075),
 .UNSPECIFIED.)
CURVE()
GEOMETRIC_REPRESENTATION_ITEM()
RATIONAL_B_SPLINE_CURVE((1.11971735964628,1.12024119946974,1.1207154165845))
REPRESENTATION_ITEM('')
);
#800=(
BOUNDED_CURVE()
B_SPLINE_CURVE(2,(#52437,#52438,#52439),.UNSPECIFIED.,.F.,.F.)
B_SPLINE_CURVE_WITH_KNOTS((3,3),(0.376641898803538,0.382940702095948),
 .UNSPECIFIED.)
CURVE()
GEOMETRIC_REPRESENTATION_ITEM()
RATIONAL_B_SPLINE_CURVE((1.12071541658433,1.1202411994692,1.11971735964528))
REPRESENTATION_ITEM('')
);
#801=(
BOUNDED_CURVE()
B_SPLINE_CURVE(2,(#52443,#52444,#52445),.UNSPECIFIED.,.F.,.F.)
B_SPLINE_CURVE_WITH_KNOTS((3,3),(0.249954652430662,0.256253455718076),
 .UNSPECIFIED.)
CURVE()
GEOMETRIC_REPRESENTATION_ITEM()
RATIONAL_B_SPLINE_CURVE((1.11971735964622,1.12024119946968,1.12071541658444))
REPRESENTATION_ITEM('')
);
#802=(
BOUNDED_CURVE()
B_SPLINE_CURVE(2,(#52449,#52450,#52451),.UNSPECIFIED.,.F.,.F.)
B_SPLINE_CURVE_WITH_KNOTS((3,3),(0.37664189880352,0.382940702095935),
 .UNSPECIFIED.)
CURVE()
GEOMETRIC_REPRESENTATION_ITEM()
RATIONAL_B_SPLINE_CURVE((1.12071541658454,1.12024119946941,1.11971735964549))
REPRESENTATION_ITEM('')
);
#803=(
BOUNDED_CURVE()
B_SPLINE_CURVE(2,(#52455,#52456,#52457),.UNSPECIFIED.,.F.,.F.)
B_SPLINE_CURVE_WITH_KNOTS((3,3),(0.24995465243066,0.256253455718075),
 .UNSPECIFIED.)
CURVE()
GEOMETRIC_REPRESENTATION_ITEM()
RATIONAL_B_SPLINE_CURVE((1.1197173596463,1.12024119946976,1.12071541658452))
REPRESENTATION_ITEM('')
);
#804=(
BOUNDED_CURVE()
B_SPLINE_CURVE(2,(#52461,#52462,#52463),.UNSPECIFIED.,.F.,.F.)
B_SPLINE_CURVE_WITH_KNOTS((3,3),(0.376641898803523,0.382940702095934),
 .UNSPECIFIED.)
CURVE()
GEOMETRIC_REPRESENTATION_ITEM()
RATIONAL_B_SPLINE_CURVE((1.12071541658448,1.12024119946934,1.11971735964542))
REPRESENTATION_ITEM('')
);
#805=(
BOUNDED_CURVE()
B_SPLINE_CURVE(2,(#52467,#52468,#52469),.UNSPECIFIED.,.F.,.F.)
B_SPLINE_CURVE_WITH_KNOTS((3,3),(0.249954652430663,0.256253455718077),
 .UNSPECIFIED.)
CURVE()
GEOMETRIC_REPRESENTATION_ITEM()
RATIONAL_B_SPLINE_CURVE((1.11971735964627,1.12024119946973,1.12071541658449))
REPRESENTATION_ITEM('')
);
#806=(
BOUNDED_CURVE()
B_SPLINE_CURVE(2,(#52473,#52474,#52475),.UNSPECIFIED.,.F.,.F.)
B_SPLINE_CURVE_WITH_KNOTS((3,3),(0.376641898803548,0.382940702095957),
 .UNSPECIFIED.)
CURVE()
GEOMETRIC_REPRESENTATION_ITEM()
RATIONAL_B_SPLINE_CURVE((1.12071541658418,1.12024119946905,1.11971735964513))
REPRESENTATION_ITEM('')
);
#807=(
BOUNDED_CURVE()
B_SPLINE_CURVE(2,(#52479,#52480,#52481),.UNSPECIFIED.,.F.,.F.)
B_SPLINE_CURVE_WITH_KNOTS((3,3),(0.249954652430651,0.256253455718065),
 .UNSPECIFIED.)
CURVE()
GEOMETRIC_REPRESENTATION_ITEM()
RATIONAL_B_SPLINE_CURVE((1.1197173596461,1.12024119946956,1.12071541658432))
REPRESENTATION_ITEM('')
);
#808=(
BOUNDED_CURVE()
B_SPLINE_CURVE(2,(#52485,#52486,#52487),.UNSPECIFIED.,.F.,.F.)
B_SPLINE_CURVE_WITH_KNOTS((3,3),(0.376641898803522,0.382940702095932),
 .UNSPECIFIED.)
CURVE()
GEOMETRIC_REPRESENTATION_ITEM()
RATIONAL_B_SPLINE_CURVE((1.12071541658448,1.12024119946934,1.11971735964542))
REPRESENTATION_ITEM('')
);
#809=(
BOUNDED_CURVE()
B_SPLINE_CURVE(2,(#52491,#52492,#52493),.UNSPECIFIED.,.F.,.F.)
B_SPLINE_CURVE_WITH_KNOTS((3,3),(0.249954652430654,0.256253455718068),
 .UNSPECIFIED.)
CURVE()
GEOMETRIC_REPRESENTATION_ITEM()
RATIONAL_B_SPLINE_CURVE((1.11971735964629,1.12024119946976,1.12071541658452))
REPRESENTATION_ITEM('')
);
#810=(
BOUNDED_CURVE()
B_SPLINE_CURVE(2,(#52497,#52498,#52499),.UNSPECIFIED.,.F.,.F.)
B_SPLINE_CURVE_WITH_KNOTS((3,3),(0.376641898803521,0.382940702095935),
 .UNSPECIFIED.)
CURVE()
GEOMETRIC_REPRESENTATION_ITEM()
RATIONAL_B_SPLINE_CURVE((1.12071541658442,1.12024119946928,1.11971735964536))
REPRESENTATION_ITEM('')
);
#811=(
BOUNDED_CURVE()
B_SPLINE_CURVE(2,(#52503,#52504,#52505),.UNSPECIFIED.,.F.,.F.)
B_SPLINE_CURVE_WITH_KNOTS((3,3),(0.24995465243066,0.256253455718076),
 .UNSPECIFIED.)
CURVE()
GEOMETRIC_REPRESENTATION_ITEM()
RATIONAL_B_SPLINE_CURVE((1.11971735964628,1.12024119946975,1.12071541658451))
REPRESENTATION_ITEM('')
);
#812=(
BOUNDED_CURVE()
B_SPLINE_CURVE(2,(#52509,#52510,#52511),.UNSPECIFIED.,.F.,.F.)
B_SPLINE_CURVE_WITH_KNOTS((3,3),(0.37664189880352,0.382940702095931),
 .UNSPECIFIED.)
CURVE()
GEOMETRIC_REPRESENTATION_ITEM()
RATIONAL_B_SPLINE_CURVE((1.12071541658452,1.12024119946938,1.11971735964546))
REPRESENTATION_ITEM('')
);
#813=(
BOUNDED_CURVE()
B_SPLINE_CURVE(2,(#52515,#52516,#52517),.UNSPECIFIED.,.F.,.F.)
B_SPLINE_CURVE_WITH_KNOTS((3,3),(0.249954652430663,0.25625345571808),
 .UNSPECIFIED.)
CURVE()
GEOMETRIC_REPRESENTATION_ITEM()
RATIONAL_B_SPLINE_CURVE((1.11971735964629,1.12024119946975,1.12071541658451))
REPRESENTATION_ITEM('')
);
#814=(
BOUNDED_CURVE()
B_SPLINE_CURVE(2,(#52521,#52522,#52523),.UNSPECIFIED.,.F.,.F.)
B_SPLINE_CURVE_WITH_KNOTS((3,3),(0.376641898803514,0.382940702095925),
 .UNSPECIFIED.)
CURVE()
GEOMETRIC_REPRESENTATION_ITEM()
RATIONAL_B_SPLINE_CURVE((1.12071541658449,1.12024119946936,1.11971735964544))
REPRESENTATION_ITEM('')
);
#815=(
BOUNDED_CURVE()
B_SPLINE_CURVE(2,(#52527,#52528,#52529),.UNSPECIFIED.,.F.,.F.)
B_SPLINE_CURVE_WITH_KNOTS((3,3),(0.249954652430668,0.25625345571808),
 .UNSPECIFIED.)
CURVE()
GEOMETRIC_REPRESENTATION_ITEM()
RATIONAL_B_SPLINE_CURVE((1.11971735964628,1.12024119946974,1.1207154165845))
REPRESENTATION_ITEM('')
);
#816=(
BOUNDED_CURVE()
B_SPLINE_CURVE(2,(#52533,#52534,#52535),.UNSPECIFIED.,.F.,.F.)
B_SPLINE_CURVE_WITH_KNOTS((3,3),(0.376641898803516,0.382940702095925),
 .UNSPECIFIED.)
CURVE()
GEOMETRIC_REPRESENTATION_ITEM()
RATIONAL_B_SPLINE_CURVE((1.1207154165845,1.12024119946936,1.11971735964544))
REPRESENTATION_ITEM('')
);
#817=(
BOUNDED_CURVE()
B_SPLINE_CURVE(2,(#52539,#52540,#52541),.UNSPECIFIED.,.F.,.F.)
B_SPLINE_CURVE_WITH_KNOTS((3,3),(0.24995465243065,0.256253455718064),
 .UNSPECIFIED.)
CURVE()
GEOMETRIC_REPRESENTATION_ITEM()
RATIONAL_B_SPLINE_CURVE((1.11971735964608,1.12024119946955,1.1207154165843))
REPRESENTATION_ITEM('')
);
#818=(
BOUNDED_CURVE()
B_SPLINE_CURVE(2,(#52545,#52546,#52547),.UNSPECIFIED.,.F.,.F.)
B_SPLINE_CURVE_WITH_KNOTS((3,3),(0.376641898803537,0.382940702095953),
 .UNSPECIFIED.)
CURVE()
GEOMETRIC_REPRESENTATION_ITEM()
RATIONAL_B_SPLINE_CURVE((1.12071541658421,1.12024119946908,1.11971735964516))
REPRESENTATION_ITEM('')
);
#819=(
BOUNDED_CURVE()
B_SPLINE_CURVE(2,(#52551,#52552,#52553),.UNSPECIFIED.,.F.,.F.)
B_SPLINE_CURVE_WITH_KNOTS((3,3),(0.249954652430652,0.256253455718068),
 .UNSPECIFIED.)
CURVE()
GEOMETRIC_REPRESENTATION_ITEM()
RATIONAL_B_SPLINE_CURVE((1.11971735964626,1.12024119946972,1.12071541658448))
REPRESENTATION_ITEM('')
);
#820=(
BOUNDED_CURVE()
B_SPLINE_CURVE(2,(#52557,#52558,#52559),.UNSPECIFIED.,.F.,.F.)
B_SPLINE_CURVE_WITH_KNOTS((3,3),(0.376641898803534,0.382940702095941),
 .UNSPECIFIED.)
CURVE()
GEOMETRIC_REPRESENTATION_ITEM()
RATIONAL_B_SPLINE_CURVE((1.12071541658423,1.1202411994691,1.11971735964518))
REPRESENTATION_ITEM('')
);
#821=(
BOUNDED_CURVE()
B_SPLINE_CURVE(2,(#52563,#52564,#52565),.UNSPECIFIED.,.F.,.F.)
B_SPLINE_CURVE_WITH_KNOTS((3,3),(0.249954652430639,0.256253455718054),
 .UNSPECIFIED.)
CURVE()
GEOMETRIC_REPRESENTATION_ITEM()
RATIONAL_B_SPLINE_CURVE((1.11971735964598,1.12024119946944,1.1207154165842))
REPRESENTATION_ITEM('')
);
#822=(
BOUNDED_CURVE()
B_SPLINE_CURVE(2,(#52569,#52570,#52571),.UNSPECIFIED.,.F.,.F.)
B_SPLINE_CURVE_WITH_KNOTS((3,3),(0.376641898803521,0.382940702095926),
 .UNSPECIFIED.)
CURVE()
GEOMETRIC_REPRESENTATION_ITEM()
RATIONAL_B_SPLINE_CURVE((1.12071541658441,1.12024119946928,1.11971735964536))
REPRESENTATION_ITEM('')
);
#823=(
BOUNDED_CURVE()
B_SPLINE_CURVE(2,(#52575,#52576,#52577),.UNSPECIFIED.,.F.,.F.)
B_SPLINE_CURVE_WITH_KNOTS((3,3),(0.249954652430644,0.256253455718059),
 .UNSPECIFIED.)
CURVE()
GEOMETRIC_REPRESENTATION_ITEM()
RATIONAL_B_SPLINE_CURVE((1.11971735964605,1.12024119946951,1.12071541658427))
REPRESENTATION_ITEM('')
);
#824=(
BOUNDED_CURVE()
B_SPLINE_CURVE(2,(#52581,#52582,#52583),.UNSPECIFIED.,.F.,.F.)
B_SPLINE_CURVE_WITH_KNOTS((3,3),(0.376641898803522,0.382940702095933),
 .UNSPECIFIED.)
CURVE()
GEOMETRIC_REPRESENTATION_ITEM()
RATIONAL_B_SPLINE_CURVE((1.12071541658452,1.12024119946939,1.11971735964547))
REPRESENTATION_ITEM('')
);
#825=(
BOUNDED_CURVE()
B_SPLINE_CURVE(2,(#52587,#52588,#52589),.UNSPECIFIED.,.F.,.F.)
B_SPLINE_CURVE_WITH_KNOTS((3,3),(0.249954652430652,0.256253455718069),
 .UNSPECIFIED.)
CURVE()
GEOMETRIC_REPRESENTATION_ITEM()
RATIONAL_B_SPLINE_CURVE((1.11971735964616,1.12024119946962,1.12071541658438))
REPRESENTATION_ITEM('')
);
#826=(
BOUNDED_CURVE()
B_SPLINE_CURVE(2,(#52593,#52594,#52595),.UNSPECIFIED.,.F.,.F.)
B_SPLINE_CURVE_WITH_KNOTS((3,3),(0.376641898803538,0.38294070209595),
 .UNSPECIFIED.)
CURVE()
GEOMETRIC_REPRESENTATION_ITEM()
RATIONAL_B_SPLINE_CURVE((1.12071541658426,1.12024119946913,1.11971735964521))
REPRESENTATION_ITEM('')
);
#827=(
BOUNDED_CURVE()
B_SPLINE_CURVE(2,(#52598,#52599,#52600),.UNSPECIFIED.,.F.,.F.)
B_SPLINE_CURVE_WITH_KNOTS((3,3),(0.249954652430655,0.256253455718073),
 .UNSPECIFIED.)
CURVE()
GEOMETRIC_REPRESENTATION_ITEM()
RATIONAL_B_SPLINE_CURVE((1.11971735964623,1.1202411994697,1.12071541658446))
REPRESENTATION_ITEM('')
);
#828=(
BOUNDED_CURVE()
B_SPLINE_CURVE(2,(#52602,#52603,#52604),.UNSPECIFIED.,.F.,.F.)
B_SPLINE_CURVE_WITH_KNOTS((3,3),(0.376641898803523,0.38294070209594),
 .UNSPECIFIED.)
CURVE()
GEOMETRIC_REPRESENTATION_ITEM()
RATIONAL_B_SPLINE_CURVE((1.12071541658441,1.12024119946928,1.11971735964536))
REPRESENTATION_ITEM('')
);
#829=(
BOUNDED_CURVE()
B_SPLINE_CURVE(2,(#52607,#52608,#52609),.UNSPECIFIED.,.F.,.F.)
B_SPLINE_CURVE_WITH_KNOTS((3,3),(0.249954652430659,0.256253455718073),
 .UNSPECIFIED.)
CURVE()
GEOMETRIC_REPRESENTATION_ITEM()
RATIONAL_B_SPLINE_CURVE((1.11971735964623,1.12024119946969,1.12071541658445))
REPRESENTATION_ITEM('')
);
#830=(
BOUNDED_CURVE()
B_SPLINE_CURVE(2,(#52611,#52612,#52613),.UNSPECIFIED.,.F.,.F.)
B_SPLINE_CURVE_WITH_KNOTS((3,3),(0.376641898803521,0.382940702095929),
 .UNSPECIFIED.)
CURVE()
GEOMETRIC_REPRESENTATION_ITEM()
RATIONAL_B_SPLINE_CURVE((1.12071541658454,1.1202411994694,1.11971735964548))
REPRESENTATION_ITEM('')
);
#831=(
BOUNDED_CURVE()
B_SPLINE_CURVE(2,(#52616,#52617,#52618),.UNSPECIFIED.,.F.,.F.)
B_SPLINE_CURVE_WITH_KNOTS((3,3),(0.249954652430646,0.256253455718056),
 .UNSPECIFIED.)
CURVE()
GEOMETRIC_REPRESENTATION_ITEM()
RATIONAL_B_SPLINE_CURVE((1.11971735964596,1.12024119946942,1.12071541658418))
REPRESENTATION_ITEM('')
);
#832=(
BOUNDED_CURVE()
B_SPLINE_CURVE(2,(#52620,#52621,#52622),.UNSPECIFIED.,.F.,.F.)
B_SPLINE_CURVE_WITH_KNOTS((3,3),(0.376641898803528,0.382940702095943),
 .UNSPECIFIED.)
CURVE()
GEOMETRIC_REPRESENTATION_ITEM()
RATIONAL_B_SPLINE_CURVE((1.12071541658433,1.1202411994692,1.11971735964528))
REPRESENTATION_ITEM('')
);
#833=(
BOUNDED_CURVE()
B_SPLINE_CURVE(2,(#52625,#52626,#52627),.UNSPECIFIED.,.F.,.F.)
B_SPLINE_CURVE_WITH_KNOTS((3,3),(0.24995465243066,0.256253455718077),
 .UNSPECIFIED.)
CURVE()
GEOMETRIC_REPRESENTATION_ITEM()
RATIONAL_B_SPLINE_CURVE((1.11971735964636,1.12024119946983,1.12071541658459))
REPRESENTATION_ITEM('')
);
#834=(
BOUNDED_CURVE()
B_SPLINE_CURVE(2,(#52629,#52630,#52631),.UNSPECIFIED.,.F.,.F.)
B_SPLINE_CURVE_WITH_KNOTS((3,3),(0.376641898803527,0.382940702095942),
 .UNSPECIFIED.)
CURVE()
GEOMETRIC_REPRESENTATION_ITEM()
RATIONAL_B_SPLINE_CURVE((1.12071541658443,1.12024119946929,1.11971735964537))
REPRESENTATION_ITEM('')
);
#835=(
BOUNDED_CURVE()
B_SPLINE_CURVE(2,(#52634,#52635,#52636),.UNSPECIFIED.,.F.,.F.)
B_SPLINE_CURVE_WITH_KNOTS((3,3),(0.249954652430663,0.256253455718073),
 .UNSPECIFIED.)
CURVE()
GEOMETRIC_REPRESENTATION_ITEM()
RATIONAL_B_SPLINE_CURVE((1.11971735964622,1.12024119946969,1.12071541658445))
REPRESENTATION_ITEM('')
);
#836=(
BOUNDED_CURVE()
B_SPLINE_CURVE(2,(#52638,#52639,#52640),.UNSPECIFIED.,.F.,.F.)
B_SPLINE_CURVE_WITH_KNOTS((3,3),(0.376641898803534,0.382940702095947),
 .UNSPECIFIED.)
CURVE()
GEOMETRIC_REPRESENTATION_ITEM()
RATIONAL_B_SPLINE_CURVE((1.12071541658425,1.12024119946912,1.1197173596452))
REPRESENTATION_ITEM('')
);
#837=(
BOUNDED_CURVE()
B_SPLINE_CURVE(2,(#52643,#52644,#52645),.UNSPECIFIED.,.F.,.F.)
B_SPLINE_CURVE_WITH_KNOTS((3,3),(0.249954652430658,0.256253455718067),
 .UNSPECIFIED.)
CURVE()
GEOMETRIC_REPRESENTATION_ITEM()
RATIONAL_B_SPLINE_CURVE((1.1197173596462,1.12024119946966,1.12071541658442))
REPRESENTATION_ITEM('')
);
#838=(
BOUNDED_CURVE()
B_SPLINE_CURVE(2,(#52647,#52648,#52649),.UNSPECIFIED.,.F.,.F.)
B_SPLINE_CURVE_WITH_KNOTS((3,3),(0.376641898803512,0.382940702095926),
 .UNSPECIFIED.)
CURVE()
GEOMETRIC_REPRESENTATION_ITEM()
RATIONAL_B_SPLINE_CURVE((1.12071541658454,1.12024119946941,1.11971735964549))
REPRESENTATION_ITEM('')
);
#839=(
BOUNDED_CURVE()
B_SPLINE_CURVE(2,(#52652,#52653,#52654),.UNSPECIFIED.,.F.,.F.)
B_SPLINE_CURVE_WITH_KNOTS((3,3),(0.249954652430648,0.256253455718064),
 .UNSPECIFIED.)
CURVE()
GEOMETRIC_REPRESENTATION_ITEM()
RATIONAL_B_SPLINE_CURVE((1.11971735964605,1.12024119946951,1.12071541658427))
REPRESENTATION_ITEM('')
);
#840=(
BOUNDED_CURVE()
B_SPLINE_CURVE(2,(#52656,#52657,#52658),.UNSPECIFIED.,.F.,.F.)
B_SPLINE_CURVE_WITH_KNOTS((3,3),(0.37664189880353,0.382940702095945),
 .UNSPECIFIED.)
CURVE()
GEOMETRIC_REPRESENTATION_ITEM()
RATIONAL_B_SPLINE_CURVE((1.12071541658432,1.12024119946919,1.11971735964527))
REPRESENTATION_ITEM('')
);
#841=(
BOUNDED_CURVE()
B_SPLINE_CURVE(2,(#52661,#52662,#52663),.UNSPECIFIED.,.F.,.F.)
B_SPLINE_CURVE_WITH_KNOTS((3,3),(0.24995465243065,0.256253455718062),
 .UNSPECIFIED.)
CURVE()
GEOMETRIC_REPRESENTATION_ITEM()
RATIONAL_B_SPLINE_CURVE((1.1197173596462,1.12024119946966,1.12071541658442))
REPRESENTATION_ITEM('')
);
#842=(
BOUNDED_CURVE()
B_SPLINE_CURVE(2,(#52665,#52666,#52667),.UNSPECIFIED.,.F.,.F.)
B_SPLINE_CURVE_WITH_KNOTS((3,3),(0.376641898803514,0.382940702095926),
 .UNSPECIFIED.)
CURVE()
GEOMETRIC_REPRESENTATION_ITEM()
RATIONAL_B_SPLINE_CURVE((1.12071541658458,1.12024119946944,1.11971735964552))
REPRESENTATION_ITEM('')
);
#843=(
BOUNDED_CURVE()
B_SPLINE_CURVE(2,(#52670,#52671,#52672),.UNSPECIFIED.,.F.,.F.)
B_SPLINE_CURVE_WITH_KNOTS((3,3),(0.249954652430654,0.256253455718075),
 .UNSPECIFIED.)
CURVE()
GEOMETRIC_REPRESENTATION_ITEM()
RATIONAL_B_SPLINE_CURVE((1.11971735964632,1.12024119946978,1.12071541658454))
REPRESENTATION_ITEM('')
);
#844=(
BOUNDED_CURVE()
B_SPLINE_CURVE(2,(#52674,#52675,#52676),.UNSPECIFIED.,.F.,.F.)
B_SPLINE_CURVE_WITH_KNOTS((3,3),(0.376641898803524,0.382940702095939),
 .UNSPECIFIED.)
CURVE()
GEOMETRIC_REPRESENTATION_ITEM()
RATIONAL_B_SPLINE_CURVE((1.12071541658443,1.1202411994693,1.11971735964538))
REPRESENTATION_ITEM('')
);
#845=(
BOUNDED_CURVE()
B_SPLINE_CURVE(2,(#52679,#52680,#52681),.UNSPECIFIED.,.F.,.F.)
B_SPLINE_CURVE_WITH_KNOTS((3,3),(0.249954652430651,0.256253455718065),
 .UNSPECIFIED.)
CURVE()
GEOMETRIC_REPRESENTATION_ITEM()
RATIONAL_B_SPLINE_CURVE((1.11971735964614,1.12024119946961,1.12071541658437))
REPRESENTATION_ITEM('')
);
#846=(
BOUNDED_CURVE()
B_SPLINE_CURVE(2,(#52683,#52684,#52685),.UNSPECIFIED.,.F.,.F.)
B_SPLINE_CURVE_WITH_KNOTS((3,3),(0.376641898803524,0.382940702095937),
 .UNSPECIFIED.)
CURVE()
GEOMETRIC_REPRESENTATION_ITEM()
RATIONAL_B_SPLINE_CURVE((1.12071541658443,1.1202411994693,1.11971735964538))
REPRESENTATION_ITEM('')
);
#847=(
BOUNDED_CURVE()
B_SPLINE_CURVE(2,(#52688,#52689,#52690),.UNSPECIFIED.,.F.,.F.)
B_SPLINE_CURVE_WITH_KNOTS((3,3),(0.24995465243066,0.256253455718078),
 .UNSPECIFIED.)
CURVE()
GEOMETRIC_REPRESENTATION_ITEM()
RATIONAL_B_SPLINE_CURVE((1.11971735964625,1.12024119946971,1.12071541658447))
REPRESENTATION_ITEM('')
);
#848=(
BOUNDED_CURVE()
B_SPLINE_CURVE(2,(#52692,#52693,#52694),.UNSPECIFIED.,.F.,.F.)
B_SPLINE_CURVE_WITH_KNOTS((3,3),(0.376641898803522,0.382940702095931),
 .UNSPECIFIED.)
CURVE()
GEOMETRIC_REPRESENTATION_ITEM()
RATIONAL_B_SPLINE_CURVE((1.1207154165845,1.12024119946936,1.11971735964544))
REPRESENTATION_ITEM('')
);
#849=(
BOUNDED_CURVE()
B_SPLINE_CURVE(2,(#52697,#52698,#52699),.UNSPECIFIED.,.F.,.F.)
B_SPLINE_CURVE_WITH_KNOTS((3,3),(0.249954652430652,0.256253455718071),
 .UNSPECIFIED.)
CURVE()
GEOMETRIC_REPRESENTATION_ITEM()
RATIONAL_B_SPLINE_CURVE((1.11971735964614,1.12024119946961,1.12071541658437))
REPRESENTATION_ITEM('')
);
#850=(
BOUNDED_CURVE()
B_SPLINE_CURVE(2,(#52701,#52702,#52703),.UNSPECIFIED.,.F.,.F.)
B_SPLINE_CURVE_WITH_KNOTS((3,3),(0.376641898803528,0.382940702095942),
 .UNSPECIFIED.)
CURVE()
GEOMETRIC_REPRESENTATION_ITEM()
RATIONAL_B_SPLINE_CURVE((1.12071541658436,1.12024119946922,1.1197173596453))
REPRESENTATION_ITEM('')
);
#851=(
BOUNDED_CURVE()
B_SPLINE_CURVE(2,(#52706,#52707,#52708),.UNSPECIFIED.,.F.,.F.)
B_SPLINE_CURVE_WITH_KNOTS((3,3),(0.249954652430651,0.256253455718071),
 .UNSPECIFIED.)
CURVE()
GEOMETRIC_REPRESENTATION_ITEM()
RATIONAL_B_SPLINE_CURVE((1.11971735964609,1.12024119946955,1.12071541658431))
REPRESENTATION_ITEM('')
);
#852=(
BOUNDED_CURVE()
B_SPLINE_CURVE(2,(#52710,#52711,#52712),.UNSPECIFIED.,.F.,.F.)
B_SPLINE_CURVE_WITH_KNOTS((3,3),(0.376641898803537,0.382940702095949),
 .UNSPECIFIED.)
CURVE()
GEOMETRIC_REPRESENTATION_ITEM()
RATIONAL_B_SPLINE_CURVE((1.12071541658424,1.1202411994691,1.11971735964519))
REPRESENTATION_ITEM('')
);
#853=(
BOUNDED_CURVE()
B_SPLINE_CURVE(2,(#52715,#52716,#52717),.UNSPECIFIED.,.F.,.F.)
B_SPLINE_CURVE_WITH_KNOTS((3,3),(0.249954652430663,0.256253455718077),
 .UNSPECIFIED.)
CURVE()
GEOMETRIC_REPRESENTATION_ITEM()
RATIONAL_B_SPLINE_CURVE((1.11971735964627,1.12024119946974,1.1207154165845))
REPRESENTATION_ITEM('')
);
#854=(
BOUNDED_CURVE()
B_SPLINE_CURVE(2,(#52719,#52720,#52721),.UNSPECIFIED.,.F.,.F.)
B_SPLINE_CURVE_WITH_KNOTS((3,3),(0.376641898803535,0.382940702095948),
 .UNSPECIFIED.)
CURVE()
GEOMETRIC_REPRESENTATION_ITEM()
RATIONAL_B_SPLINE_CURVE((1.12071541658433,1.1202411994692,1.11971735964528))
REPRESENTATION_ITEM('')
);
#855=(
BOUNDED_CURVE()
B_SPLINE_CURVE(2,(#52724,#52725,#52726),.UNSPECIFIED.,.F.,.F.)
B_SPLINE_CURVE_WITH_KNOTS((3,3),(0.249954652430657,0.256253455718068),
 .UNSPECIFIED.)
CURVE()
GEOMETRIC_REPRESENTATION_ITEM()
RATIONAL_B_SPLINE_CURVE((1.11971735964623,1.1202411994697,1.12071541658445))
REPRESENTATION_ITEM('')
);
#856=(
BOUNDED_CURVE()
B_SPLINE_CURVE(2,(#52728,#52729,#52730),.UNSPECIFIED.,.F.,.F.)
B_SPLINE_CURVE_WITH_KNOTS((3,3),(0.376641898803534,0.382940702095946),
 .UNSPECIFIED.)
CURVE()
GEOMETRIC_REPRESENTATION_ITEM()
RATIONAL_B_SPLINE_CURVE((1.12071541658428,1.12024119946915,1.11971735964523))
REPRESENTATION_ITEM('')
);
#857=(
BOUNDED_CURVE()
B_SPLINE_CURVE(2,(#52734,#52735,#52736),.UNSPECIFIED.,.F.,.F.)
B_SPLINE_CURVE_WITH_KNOTS((3,3),(0.249954652430652,0.256253455718065),
 .UNSPECIFIED.)
CURVE()
GEOMETRIC_REPRESENTATION_ITEM()
RATIONAL_B_SPLINE_CURVE((1.11971735964615,1.12024119946961,1.12071541658437))
REPRESENTATION_ITEM('')
);
#858=(
BOUNDED_CURVE()
B_SPLINE_CURVE(2,(#52740,#52741,#52742),.UNSPECIFIED.,.F.,.F.)
B_SPLINE_CURVE_WITH_KNOTS((3,3),(0.376641898803528,0.38294070209594),
 .UNSPECIFIED.)
CURVE()
GEOMETRIC_REPRESENTATION_ITEM()
RATIONAL_B_SPLINE_CURVE((1.12071541658438,1.12024119946925,1.11971735964533))
REPRESENTATION_ITEM('')
);
#859=(
BOUNDED_CURVE()
B_SPLINE_CURVE(2,(#52746,#52747,#52748),.UNSPECIFIED.,.F.,.F.)
B_SPLINE_CURVE_WITH_KNOTS((3,3),(0.249954652430646,0.256253455718057),
 .UNSPECIFIED.)
CURVE()
GEOMETRIC_REPRESENTATION_ITEM()
RATIONAL_B_SPLINE_CURVE((1.11971735964604,1.12024119946951,1.12071541658426))
REPRESENTATION_ITEM('')
);
#860=(
BOUNDED_CURVE()
B_SPLINE_CURVE(2,(#52752,#52753,#52754),.UNSPECIFIED.,.F.,.F.)
B_SPLINE_CURVE_WITH_KNOTS((3,3),(0.376641898803525,0.382940702095939),
 .UNSPECIFIED.)
CURVE()
GEOMETRIC_REPRESENTATION_ITEM()
RATIONAL_B_SPLINE_CURVE((1.12071541658443,1.1202411994693,1.11971735964538))
REPRESENTATION_ITEM('')
);
#861=(
BOUNDED_CURVE()
B_SPLINE_CURVE(2,(#52758,#52759,#52760),.UNSPECIFIED.,.F.,.F.)
B_SPLINE_CURVE_WITH_KNOTS((3,3),(0.249954652430639,0.256253455718051),
 .UNSPECIFIED.)
CURVE()
GEOMETRIC_REPRESENTATION_ITEM()
RATIONAL_B_SPLINE_CURVE((1.11971735964598,1.12024119946945,1.1207154165842))
REPRESENTATION_ITEM('')
);
#862=(
BOUNDED_CURVE()
B_SPLINE_CURVE(2,(#52764,#52765,#52766),.UNSPECIFIED.,.F.,.F.)
B_SPLINE_CURVE_WITH_KNOTS((3,3),(0.376641898803521,0.382940702095934),
 .UNSPECIFIED.)
CURVE()
GEOMETRIC_REPRESENTATION_ITEM()
RATIONAL_B_SPLINE_CURVE((1.12071541658441,1.12024119946928,1.11971735964536))
REPRESENTATION_ITEM('')
);
#863=(
BOUNDED_CURVE()
B_SPLINE_CURVE(2,(#52770,#52771,#52772),.UNSPECIFIED.,.F.,.F.)
B_SPLINE_CURVE_WITH_KNOTS((3,3),(0.249954652430652,0.256253455718065),
 .UNSPECIFIED.)
CURVE()
GEOMETRIC_REPRESENTATION_ITEM()
RATIONAL_B_SPLINE_CURVE((1.11971735964616,1.12024119946962,1.12071541658438))
REPRESENTATION_ITEM('')
);
#864=(
BOUNDED_CURVE()
B_SPLINE_CURVE(2,(#52776,#52777,#52778),.UNSPECIFIED.,.F.,.F.)
B_SPLINE_CURVE_WITH_KNOTS((3,3),(0.376641898803544,0.382940702095957),
 .UNSPECIFIED.)
CURVE()
GEOMETRIC_REPRESENTATION_ITEM()
RATIONAL_B_SPLINE_CURVE((1.12071541658424,1.1202411994691,1.11971735964518))
REPRESENTATION_ITEM('')
);
#865=(
BOUNDED_CURVE()
B_SPLINE_CURVE(2,(#52782,#52783,#52784),.UNSPECIFIED.,.F.,.F.)
B_SPLINE_CURVE_WITH_KNOTS((3,3),(0.249954652430643,0.256253455718053),
 .UNSPECIFIED.)
CURVE()
GEOMETRIC_REPRESENTATION_ITEM()
RATIONAL_B_SPLINE_CURVE((1.11971735964601,1.12024119946947,1.12071541658423))
REPRESENTATION_ITEM('')
);
#866=(
BOUNDED_CURVE()
B_SPLINE_CURVE(2,(#52788,#52789,#52790),.UNSPECIFIED.,.F.,.F.)
B_SPLINE_CURVE_WITH_KNOTS((3,3),(0.376641898803543,0.382940702095953),
 .UNSPECIFIED.)
CURVE()
GEOMETRIC_REPRESENTATION_ITEM()
RATIONAL_B_SPLINE_CURVE((1.12071541658425,1.12024119946911,1.1197173596452))
REPRESENTATION_ITEM('')
);
#867=(
BOUNDED_CURVE()
B_SPLINE_CURVE(2,(#52794,#52795,#52796),.UNSPECIFIED.,.F.,.F.)
B_SPLINE_CURVE_WITH_KNOTS((3,3),(0.249954652430649,0.256253455718062),
 .UNSPECIFIED.)
CURVE()
GEOMETRIC_REPRESENTATION_ITEM()
RATIONAL_B_SPLINE_CURVE((1.11971735964607,1.12024119946954,1.12071541658429))
REPRESENTATION_ITEM('')
);
#868=(
BOUNDED_CURVE()
B_SPLINE_CURVE(2,(#60594,#60595,#60596),.UNSPECIFIED.,.F.,.F.)
B_SPLINE_CURVE_WITH_KNOTS((3,3),(-0.375752880509706,-0.25773139970398),
 .UNSPECIFIED.)
CURVE()
GEOMETRIC_REPRESENTATION_ITEM()
RATIONAL_B_SPLINE_CURVE((1.41147367097488,1.52065153937885,1.52065153937885))
REPRESENTATION_ITEM('')
);
#869=(
BOUNDED_CURVE()
B_SPLINE_CURVE(2,(#60598,#60599,#60600),.UNSPECIFIED.,.F.,.F.)
B_SPLINE_CURVE_WITH_KNOTS((3,3),(-0.375752880509709,-0.139709918898254),
 .UNSPECIFIED.)
CURVE()
GEOMETRIC_REPRESENTATION_ITEM()
RATIONAL_B_SPLINE_CURVE((1.41147367097488,1.62982940778282,1.41147367097488))
REPRESENTATION_ITEM('')
);
#870=(
BOUNDED_CURVE()
B_SPLINE_CURVE(2,(#60602,#60603,#60604),.UNSPECIFIED.,.F.,.F.)
B_SPLINE_CURVE_WITH_KNOTS((3,3),(-0.375752880509709,-0.139709918898254),
 .UNSPECIFIED.)
CURVE()
GEOMETRIC_REPRESENTATION_ITEM()
RATIONAL_B_SPLINE_CURVE((1.41147367097488,1.62982940778282,1.41147367097488))
REPRESENTATION_ITEM('')
);
#871=(
BOUNDED_CURVE()
B_SPLINE_CURVE(2,(#60606,#60607,#60608),.UNSPECIFIED.,.F.,.F.)
B_SPLINE_CURVE_WITH_KNOTS((3,3),(-0.375752880509708,-0.139709918898254),
 .UNSPECIFIED.)
CURVE()
GEOMETRIC_REPRESENTATION_ITEM()
RATIONAL_B_SPLINE_CURVE((1.41147367097487,1.62982940778281,1.41147367097487))
REPRESENTATION_ITEM('')
);
#872=(
BOUNDED_CURVE()
B_SPLINE_CURVE(2,(#60610,#60611,#60612),.UNSPECIFIED.,.F.,.F.)
B_SPLINE_CURVE_WITH_KNOTS((3,3),(-0.375752880509709,-0.139709918898253),
 .UNSPECIFIED.)
CURVE()
GEOMETRIC_REPRESENTATION_ITEM()
RATIONAL_B_SPLINE_CURVE((1.41147367097488,1.62982940778282,1.41147367097488))
REPRESENTATION_ITEM('')
);
#873=(
BOUNDED_CURVE()
B_SPLINE_CURVE(2,(#60614,#60615,#60616),.UNSPECIFIED.,.F.,.F.)
B_SPLINE_CURVE_WITH_KNOTS((3,3),(-0.375752880509709,-0.139709918898254),
 .UNSPECIFIED.)
CURVE()
GEOMETRIC_REPRESENTATION_ITEM()
RATIONAL_B_SPLINE_CURVE((1.41147367097488,1.62982940778282,1.41147367097488))
REPRESENTATION_ITEM('')
);
#874=(
BOUNDED_CURVE()
B_SPLINE_CURVE(2,(#60617,#60618,#60619),.UNSPECIFIED.,.F.,.F.)
B_SPLINE_CURVE_WITH_KNOTS((3,3),(-0.25773139970398,-0.139709918898256),
 .UNSPECIFIED.)
CURVE()
GEOMETRIC_REPRESENTATION_ITEM()
RATIONAL_B_SPLINE_CURVE((1.52065153937885,1.52065153937885,1.41147367097488))
REPRESENTATION_ITEM('')
);
#875=(
BOUNDED_CURVE()
B_SPLINE_CURVE(2,(#60641,#60642,#60643),.UNSPECIFIED.,.F.,.F.)
B_SPLINE_CURVE_WITH_KNOTS((3,3),(0.367644516946548,0.373830527582523),
 .UNSPECIFIED.)
CURVE()
GEOMETRIC_REPRESENTATION_ITEM()
RATIONAL_B_SPLINE_CURVE((1.13426390111316,1.13389822901309,1.13348223894575))
REPRESENTATION_ITEM('')
);
#876=(
BOUNDED_CURVE()
B_SPLINE_CURVE(2,(#60647,#60648,#60649),.UNSPECIFIED.,.F.,.F.)
B_SPLINE_CURVE_WITH_KNOTS((3,3),(0.271548216895916,0.277734227531904),
 .UNSPECIFIED.)
CURVE()
GEOMETRIC_REPRESENTATION_ITEM()
RATIONAL_B_SPLINE_CURVE((1.13348223894615,1.1338982290135,1.13426390111357))
REPRESENTATION_ITEM('')
);
#877=(
BOUNDED_CURVE()
B_SPLINE_CURVE(2,(#60653,#60654,#60655),.UNSPECIFIED.,.F.,.F.)
B_SPLINE_CURVE_WITH_KNOTS((3,3),(0.36764451694656,0.373830527582529),
 .UNSPECIFIED.)
CURVE()
GEOMETRIC_REPRESENTATION_ITEM()
RATIONAL_B_SPLINE_CURVE((1.13426390111306,1.13389822901299,1.13348223894565))
REPRESENTATION_ITEM('')
);
#878=(
BOUNDED_CURVE()
B_SPLINE_CURVE(2,(#60659,#60660,#60661),.UNSPECIFIED.,.F.,.F.)
B_SPLINE_CURVE_WITH_KNOTS((3,3),(0.271548216895914,0.277734227531901),
 .UNSPECIFIED.)
CURVE()
GEOMETRIC_REPRESENTATION_ITEM()
RATIONAL_B_SPLINE_CURVE((1.13348223894612,1.13389822901347,1.13426390111354))
REPRESENTATION_ITEM('')
);
#879=(
BOUNDED_CURVE()
B_SPLINE_CURVE(2,(#60665,#60666,#60667),.UNSPECIFIED.,.F.,.F.)
B_SPLINE_CURVE_WITH_KNOTS((3,3),(0.367644516946562,0.373830527582532),
 .UNSPECIFIED.)
CURVE()
GEOMETRIC_REPRESENTATION_ITEM()
RATIONAL_B_SPLINE_CURVE((1.13426390111304,1.13389822901297,1.13348223894563))
REPRESENTATION_ITEM('')
);
#880=(
BOUNDED_CURVE()
B_SPLINE_CURVE(2,(#60671,#60672,#60673),.UNSPECIFIED.,.F.,.F.)
B_SPLINE_CURVE_WITH_KNOTS((3,3),(0.27154821689591,0.277734227531895),
 .UNSPECIFIED.)
CURVE()
GEOMETRIC_REPRESENTATION_ITEM()
RATIONAL_B_SPLINE_CURVE((1.13348223894613,1.13389822901348,1.13426390111355))
REPRESENTATION_ITEM('')
);
#881=(
BOUNDED_CURVE()
B_SPLINE_CURVE(2,(#60677,#60678,#60679),.UNSPECIFIED.,.F.,.F.)
B_SPLINE_CURVE_WITH_KNOTS((3,3),(0.367644516946554,0.373830527582529),
 .UNSPECIFIED.)
CURVE()
GEOMETRIC_REPRESENTATION_ITEM()
RATIONAL_B_SPLINE_CURVE((1.13426390111305,1.13389822901299,1.13348223894564))
REPRESENTATION_ITEM('')
);
#882=(
BOUNDED_CURVE()
B_SPLINE_CURVE(2,(#60683,#60684,#60685),.UNSPECIFIED.,.F.,.F.)
B_SPLINE_CURVE_WITH_KNOTS((3,3),(0.271548216895907,0.277734227531893),
 .UNSPECIFIED.)
CURVE()
GEOMETRIC_REPRESENTATION_ITEM()
RATIONAL_B_SPLINE_CURVE((1.13348223894611,1.13389822901346,1.13426390111353))
REPRESENTATION_ITEM('')
);
#883=(
BOUNDED_CURVE()
B_SPLINE_CURVE(2,(#60689,#60690,#60691),.UNSPECIFIED.,.F.,.F.)
B_SPLINE_CURVE_WITH_KNOTS((3,3),(0.367644516946562,0.373830527582532),
 .UNSPECIFIED.)
CURVE()
GEOMETRIC_REPRESENTATION_ITEM()
RATIONAL_B_SPLINE_CURVE((1.13426390111302,1.13389822901296,1.13348223894561))
REPRESENTATION_ITEM('')
);
#884=(
BOUNDED_CURVE()
B_SPLINE_CURVE(2,(#60695,#60696,#60697),.UNSPECIFIED.,.F.,.F.)
B_SPLINE_CURVE_WITH_KNOTS((3,3),(0.271548216895914,0.277734227531899),
 .UNSPECIFIED.)
CURVE()
GEOMETRIC_REPRESENTATION_ITEM()
RATIONAL_B_SPLINE_CURVE((1.13348223894609,1.13389822901344,1.13426390111351))
REPRESENTATION_ITEM('')
);
#885=(
BOUNDED_CURVE()
B_SPLINE_CURVE(2,(#60701,#60702,#60703),.UNSPECIFIED.,.F.,.F.)
B_SPLINE_CURVE_WITH_KNOTS((3,3),(0.36764451694656,0.373830527582535),
 .UNSPECIFIED.)
CURVE()
GEOMETRIC_REPRESENTATION_ITEM()
RATIONAL_B_SPLINE_CURVE((1.13426390111302,1.13389822901295,1.1334822389456))
REPRESENTATION_ITEM('')
);
#886=(
BOUNDED_CURVE()
B_SPLINE_CURVE(2,(#60707,#60708,#60709),.UNSPECIFIED.,.F.,.F.)
B_SPLINE_CURVE_WITH_KNOTS((3,3),(0.271548216895908,0.277734227531894),
 .UNSPECIFIED.)
CURVE()
GEOMETRIC_REPRESENTATION_ITEM()
RATIONAL_B_SPLINE_CURVE((1.1334822389461,1.13389822901345,1.13426390111352))
REPRESENTATION_ITEM('')
);
#887=(
BOUNDED_CURVE()
B_SPLINE_CURVE(2,(#60713,#60714,#60715),.UNSPECIFIED.,.F.,.F.)
B_SPLINE_CURVE_WITH_KNOTS((3,3),(0.367644516946558,0.373830527582536),
 .UNSPECIFIED.)
CURVE()
GEOMETRIC_REPRESENTATION_ITEM()
RATIONAL_B_SPLINE_CURVE((1.13426390111302,1.13389822901295,1.13348223894561))
REPRESENTATION_ITEM('')
);
#888=(
BOUNDED_CURVE()
B_SPLINE_CURVE(2,(#60719,#60720,#60721),.UNSPECIFIED.,.F.,.F.)
B_SPLINE_CURVE_WITH_KNOTS((3,3),(0.271548216895914,0.277734227531899),
 .UNSPECIFIED.)
CURVE()
GEOMETRIC_REPRESENTATION_ITEM()
RATIONAL_B_SPLINE_CURVE((1.13348223894613,1.13389822901348,1.13426390111355))
REPRESENTATION_ITEM('')
);
#889=(
BOUNDED_CURVE()
B_SPLINE_CURVE(2,(#60725,#60726,#60727),.UNSPECIFIED.,.F.,.F.)
B_SPLINE_CURVE_WITH_KNOTS((3,3),(0.367644516946564,0.373830527582534),
 .UNSPECIFIED.)
CURVE()
GEOMETRIC_REPRESENTATION_ITEM()
RATIONAL_B_SPLINE_CURVE((1.13426390111303,1.13389822901296,1.13348223894561))
REPRESENTATION_ITEM('')
);
#890=(
BOUNDED_CURVE()
B_SPLINE_CURVE(2,(#60731,#60732,#60733),.UNSPECIFIED.,.F.,.F.)
B_SPLINE_CURVE_WITH_KNOTS((3,3),(0.271548216895916,0.277734227531901),
 .UNSPECIFIED.)
CURVE()
GEOMETRIC_REPRESENTATION_ITEM()
RATIONAL_B_SPLINE_CURVE((1.13348223894614,1.13389822901349,1.13426390111357))
REPRESENTATION_ITEM('')
);
#891=(
BOUNDED_CURVE()
B_SPLINE_CURVE(2,(#60737,#60738,#60739),.UNSPECIFIED.,.F.,.F.)
B_SPLINE_CURVE_WITH_KNOTS((3,3),(0.367644516946554,0.373830527582527),
 .UNSPECIFIED.)
CURVE()
GEOMETRIC_REPRESENTATION_ITEM()
RATIONAL_B_SPLINE_CURVE((1.13426390111312,1.13389822901305,1.13348223894571))
REPRESENTATION_ITEM('')
);
#892=(
BOUNDED_CURVE()
B_SPLINE_CURVE(2,(#60743,#60744,#60745),.UNSPECIFIED.,.F.,.F.)
B_SPLINE_CURVE_WITH_KNOTS((3,3),(0.271548216895913,0.2777342275319),
 .UNSPECIFIED.)
CURVE()
GEOMETRIC_REPRESENTATION_ITEM()
RATIONAL_B_SPLINE_CURVE((1.13348223894615,1.1338982290135,1.13426390111358))
REPRESENTATION_ITEM('')
);
#893=(
BOUNDED_CURVE()
B_SPLINE_CURVE(2,(#60749,#60750,#60751),.UNSPECIFIED.,.F.,.F.)
B_SPLINE_CURVE_WITH_KNOTS((3,3),(0.367644516946564,0.373830527582538),
 .UNSPECIFIED.)
CURVE()
GEOMETRIC_REPRESENTATION_ITEM()
RATIONAL_B_SPLINE_CURVE((1.134263901113,1.13389822901293,1.13348223894559))
REPRESENTATION_ITEM('')
);
#894=(
BOUNDED_CURVE()
B_SPLINE_CURVE(2,(#60755,#60756,#60757),.UNSPECIFIED.,.F.,.F.)
B_SPLINE_CURVE_WITH_KNOTS((3,3),(0.271548216895908,0.277734227531895),
 .UNSPECIFIED.)
CURVE()
GEOMETRIC_REPRESENTATION_ITEM()
RATIONAL_B_SPLINE_CURVE((1.13348223894615,1.1338982290135,1.13426390111358))
REPRESENTATION_ITEM('')
);
#895=(
BOUNDED_CURVE()
B_SPLINE_CURVE(2,(#60761,#60762,#60763),.UNSPECIFIED.,.F.,.F.)
B_SPLINE_CURVE_WITH_KNOTS((3,3),(0.367644516946561,0.373830527582532),
 .UNSPECIFIED.)
CURVE()
GEOMETRIC_REPRESENTATION_ITEM()
RATIONAL_B_SPLINE_CURVE((1.13426390111309,1.13389822901302,1.13348223894568))
REPRESENTATION_ITEM('')
);
#896=(
BOUNDED_CURVE()
B_SPLINE_CURVE(2,(#60767,#60768,#60769),.UNSPECIFIED.,.F.,.F.)
B_SPLINE_CURVE_WITH_KNOTS((3,3),(0.271548216895921,0.277734227531907),
 .UNSPECIFIED.)
CURVE()
GEOMETRIC_REPRESENTATION_ITEM()
RATIONAL_B_SPLINE_CURVE((1.13348223894616,1.13389822901351,1.13426390111358))
REPRESENTATION_ITEM('')
);
#897=(
BOUNDED_CURVE()
B_SPLINE_CURVE(2,(#60773,#60774,#60775),.UNSPECIFIED.,.F.,.F.)
B_SPLINE_CURVE_WITH_KNOTS((3,3),(0.367644516946558,0.373830527582535),
 .UNSPECIFIED.)
CURVE()
GEOMETRIC_REPRESENTATION_ITEM()
RATIONAL_B_SPLINE_CURVE((1.13426390111305,1.13389822901298,1.13348223894564))
REPRESENTATION_ITEM('')
);
#898=(
BOUNDED_CURVE()
B_SPLINE_CURVE(2,(#60779,#60780,#60781),.UNSPECIFIED.,.F.,.F.)
B_SPLINE_CURVE_WITH_KNOTS((3,3),(0.271548216895908,0.27773422753189),
 .UNSPECIFIED.)
CURVE()
GEOMETRIC_REPRESENTATION_ITEM()
RATIONAL_B_SPLINE_CURVE((1.13348223894616,1.13389822901351,1.13426390111359))
REPRESENTATION_ITEM('')
);
#899=(
BOUNDED_CURVE()
B_SPLINE_CURVE(2,(#60785,#60786,#60787),.UNSPECIFIED.,.F.,.F.)
B_SPLINE_CURVE_WITH_KNOTS((3,3),(0.367644516946548,0.373830527582523),
 .UNSPECIFIED.)
CURVE()
GEOMETRIC_REPRESENTATION_ITEM()
RATIONAL_B_SPLINE_CURVE((1.13426390111314,1.13389822901308,1.13348223894573))
REPRESENTATION_ITEM('')
);
#900=(
BOUNDED_CURVE()
B_SPLINE_CURVE(2,(#60791,#60792,#60793),.UNSPECIFIED.,.F.,.F.)
B_SPLINE_CURVE_WITH_KNOTS((3,3),(0.271548216895905,0.277734227531892),
 .UNSPECIFIED.)
CURVE()
GEOMETRIC_REPRESENTATION_ITEM()
RATIONAL_B_SPLINE_CURVE((1.13348223894608,1.13389822901343,1.1342639011135))
REPRESENTATION_ITEM('')
);
#901=(
BOUNDED_CURVE()
B_SPLINE_CURVE(2,(#60797,#60798,#60799),.UNSPECIFIED.,.F.,.F.)
B_SPLINE_CURVE_WITH_KNOTS((3,3),(0.36764451694655,0.373830527582528),
 .UNSPECIFIED.)
CURVE()
GEOMETRIC_REPRESENTATION_ITEM()
RATIONAL_B_SPLINE_CURVE((1.1342639011131,1.13389822901304,1.13348223894569))
REPRESENTATION_ITEM('')
);
#902=(
BOUNDED_CURVE()
B_SPLINE_CURVE(2,(#60803,#60804,#60805),.UNSPECIFIED.,.F.,.F.)
B_SPLINE_CURVE_WITH_KNOTS((3,3),(0.27154821689591,0.277734227531895),
 .UNSPECIFIED.)
CURVE()
GEOMETRIC_REPRESENTATION_ITEM()
RATIONAL_B_SPLINE_CURVE((1.13348223894612,1.13389822901347,1.13426390111354))
REPRESENTATION_ITEM('')
);
#903=(
BOUNDED_CURVE()
B_SPLINE_CURVE(2,(#60809,#60810,#60811),.UNSPECIFIED.,.F.,.F.)
B_SPLINE_CURVE_WITH_KNOTS((3,3),(0.367644516946551,0.373830527582525),
 .UNSPECIFIED.)
CURVE()
GEOMETRIC_REPRESENTATION_ITEM()
RATIONAL_B_SPLINE_CURVE((1.13426390111313,1.13389822901307,1.13348223894572))
REPRESENTATION_ITEM('')
);
#904=(
BOUNDED_CURVE()
B_SPLINE_CURVE(2,(#60815,#60816,#60817),.UNSPECIFIED.,.F.,.F.)
B_SPLINE_CURVE_WITH_KNOTS((3,3),(0.271548216895914,0.277734227531894),
 .UNSPECIFIED.)
CURVE()
GEOMETRIC_REPRESENTATION_ITEM()
RATIONAL_B_SPLINE_CURVE((1.13348223894619,1.13389822901354,1.13426390111361))
REPRESENTATION_ITEM('')
);
#905=(
BOUNDED_CURVE()
B_SPLINE_CURVE(2,(#60821,#60822,#60823),.UNSPECIFIED.,.F.,.F.)
B_SPLINE_CURVE_WITH_KNOTS((3,3),(0.367644516946565,0.373830527582531),
 .UNSPECIFIED.)
CURVE()
GEOMETRIC_REPRESENTATION_ITEM()
RATIONAL_B_SPLINE_CURVE((1.134263901113,1.13389822901293,1.13348223894559))
REPRESENTATION_ITEM('')
);
#906=(
BOUNDED_CURVE()
B_SPLINE_CURVE(2,(#60827,#60828,#60829),.UNSPECIFIED.,.F.,.F.)
B_SPLINE_CURVE_WITH_KNOTS((3,3),(0.271548216895912,0.277734227531896),
 .UNSPECIFIED.)
CURVE()
GEOMETRIC_REPRESENTATION_ITEM()
RATIONAL_B_SPLINE_CURVE((1.13348223894612,1.13389822901347,1.13426390111354))
REPRESENTATION_ITEM('')
);
#907=(
BOUNDED_CURVE()
B_SPLINE_CURVE(2,(#60833,#60834,#60835),.UNSPECIFIED.,.F.,.F.)
B_SPLINE_CURVE_WITH_KNOTS((3,3),(0.367644516946563,0.373830527582537),
 .UNSPECIFIED.)
CURVE()
GEOMETRIC_REPRESENTATION_ITEM()
RATIONAL_B_SPLINE_CURVE((1.13426390111305,1.13389822901298,1.13348223894564))
REPRESENTATION_ITEM('')
);
#908=(
BOUNDED_CURVE()
B_SPLINE_CURVE(2,(#60839,#60840,#60841),.UNSPECIFIED.,.F.,.F.)
B_SPLINE_CURVE_WITH_KNOTS((3,3),(0.271548216895909,0.277734227531891),
 .UNSPECIFIED.)
CURVE()
GEOMETRIC_REPRESENTATION_ITEM()
RATIONAL_B_SPLINE_CURVE((1.13348223894604,1.13389822901339,1.13426390111346))
REPRESENTATION_ITEM('')
);
#909=(
BOUNDED_CURVE()
B_SPLINE_CURVE(2,(#60845,#60846,#60847),.UNSPECIFIED.,.F.,.F.)
B_SPLINE_CURVE_WITH_KNOTS((3,3),(0.367644516946552,0.373830527582532),
 .UNSPECIFIED.)
CURVE()
GEOMETRIC_REPRESENTATION_ITEM()
RATIONAL_B_SPLINE_CURVE((1.13426390111305,1.13389822901299,1.13348223894564))
REPRESENTATION_ITEM('')
);
#910=(
BOUNDED_CURVE()
B_SPLINE_CURVE(2,(#60851,#60852,#60853),.UNSPECIFIED.,.F.,.F.)
B_SPLINE_CURVE_WITH_KNOTS((3,3),(0.271548216895916,0.277734227531902),
 .UNSPECIFIED.)
CURVE()
GEOMETRIC_REPRESENTATION_ITEM()
RATIONAL_B_SPLINE_CURVE((1.13348223894616,1.13389822901351,1.13426390111359))
REPRESENTATION_ITEM('')
);
#911=(
BOUNDED_CURVE()
B_SPLINE_CURVE(2,(#60857,#60858,#60859),.UNSPECIFIED.,.F.,.F.)
B_SPLINE_CURVE_WITH_KNOTS((3,3),(0.367644516946562,0.373830527582535),
 .UNSPECIFIED.)
CURVE()
GEOMETRIC_REPRESENTATION_ITEM()
RATIONAL_B_SPLINE_CURVE((1.13426390111309,1.13389822901302,1.13348223894568))
REPRESENTATION_ITEM('')
);
#912=(
BOUNDED_CURVE()
B_SPLINE_CURVE(2,(#60863,#60864,#60865),.UNSPECIFIED.,.F.,.F.)
B_SPLINE_CURVE_WITH_KNOTS((3,3),(0.271548216895913,0.277734227531904),
 .UNSPECIFIED.)
CURVE()
GEOMETRIC_REPRESENTATION_ITEM()
RATIONAL_B_SPLINE_CURVE((1.13348223894619,1.13389822901354,1.13426390111362))
REPRESENTATION_ITEM('')
);
#913=(
BOUNDED_CURVE()
B_SPLINE_CURVE(2,(#60869,#60870,#60871),.UNSPECIFIED.,.F.,.F.)
B_SPLINE_CURVE_WITH_KNOTS((3,3),(0.36764451694655,0.373830527582524),
 .UNSPECIFIED.)
CURVE()
GEOMETRIC_REPRESENTATION_ITEM()
RATIONAL_B_SPLINE_CURVE((1.13426390111312,1.13389822901305,1.13348223894571))
REPRESENTATION_ITEM('')
);
#914=(
BOUNDED_CURVE()
B_SPLINE_CURVE(2,(#60875,#60876,#60877),.UNSPECIFIED.,.F.,.F.)
B_SPLINE_CURVE_WITH_KNOTS((3,3),(0.271548216895921,0.277734227531899),
 .UNSPECIFIED.)
CURVE()
GEOMETRIC_REPRESENTATION_ITEM()
RATIONAL_B_SPLINE_CURVE((1.13348223894619,1.13389822901354,1.13426390111361))
REPRESENTATION_ITEM('')
);
#915=(
BOUNDED_CURVE()
B_SPLINE_CURVE(2,(#60881,#60882,#60883),.UNSPECIFIED.,.F.,.F.)
B_SPLINE_CURVE_WITH_KNOTS((3,3),(0.367644516946559,0.373830527582526),
 .UNSPECIFIED.)
CURVE()
GEOMETRIC_REPRESENTATION_ITEM()
RATIONAL_B_SPLINE_CURVE((1.1342639011131,1.13389822901303,1.13348223894569))
REPRESENTATION_ITEM('')
);
#916=(
BOUNDED_CURVE()
B_SPLINE_CURVE(2,(#60887,#60888,#60889),.UNSPECIFIED.,.F.,.F.)
B_SPLINE_CURVE_WITH_KNOTS((3,3),(0.271548216895914,0.2777342275319),
 .UNSPECIFIED.)
CURVE()
GEOMETRIC_REPRESENTATION_ITEM()
RATIONAL_B_SPLINE_CURVE((1.13348223894616,1.13389822901351,1.13426390111358))
REPRESENTATION_ITEM('')
);
#917=(
BOUNDED_CURVE()
B_SPLINE_CURVE(2,(#60893,#60894,#60895),.UNSPECIFIED.,.F.,.F.)
B_SPLINE_CURVE_WITH_KNOTS((3,3),(0.367644516946557,0.373830527582536),
 .UNSPECIFIED.)
CURVE()
GEOMETRIC_REPRESENTATION_ITEM()
RATIONAL_B_SPLINE_CURVE((1.13426390111309,1.13389822901303,1.13348223894568))
REPRESENTATION_ITEM('')
);
#918=(
BOUNDED_CURVE()
B_SPLINE_CURVE(2,(#60899,#60900,#60901),.UNSPECIFIED.,.F.,.F.)
B_SPLINE_CURVE_WITH_KNOTS((3,3),(0.271548216895912,0.277734227531897),
 .UNSPECIFIED.)
CURVE()
GEOMETRIC_REPRESENTATION_ITEM()
RATIONAL_B_SPLINE_CURVE((1.13348223894616,1.13389822901351,1.13426390111358))
REPRESENTATION_ITEM('')
);
#919=(
BOUNDED_CURVE()
B_SPLINE_CURVE(2,(#60905,#60906,#60907),.UNSPECIFIED.,.F.,.F.)
B_SPLINE_CURVE_WITH_KNOTS((3,3),(0.367644516946558,0.373830527582532),
 .UNSPECIFIED.)
CURVE()
GEOMETRIC_REPRESENTATION_ITEM()
RATIONAL_B_SPLINE_CURVE((1.13426390111307,1.13389822901301,1.13348223894566))
REPRESENTATION_ITEM('')
);
#920=(
BOUNDED_CURVE()
B_SPLINE_CURVE(2,(#60911,#60912,#60913),.UNSPECIFIED.,.F.,.F.)
B_SPLINE_CURVE_WITH_KNOTS((3,3),(0.271548216895914,0.277734227531905),
 .UNSPECIFIED.)
CURVE()
GEOMETRIC_REPRESENTATION_ITEM()
RATIONAL_B_SPLINE_CURVE((1.13348223894616,1.13389822901351,1.13426390111358))
REPRESENTATION_ITEM('')
);
#921=(
BOUNDED_CURVE()
B_SPLINE_CURVE(2,(#60917,#60918,#60919),.UNSPECIFIED.,.F.,.F.)
B_SPLINE_CURVE_WITH_KNOTS((3,3),(0.367644516946569,0.373830527582539),
 .UNSPECIFIED.)
CURVE()
GEOMETRIC_REPRESENTATION_ITEM()
RATIONAL_B_SPLINE_CURVE((1.13426390111301,1.13389822901295,1.1334822389456))
REPRESENTATION_ITEM('')
);
#922=(
BOUNDED_CURVE()
B_SPLINE_CURVE(2,(#60923,#60924,#60925),.UNSPECIFIED.,.F.,.F.)
B_SPLINE_CURVE_WITH_KNOTS((3,3),(0.271548216895913,0.2777342275319),
 .UNSPECIFIED.)
CURVE()
GEOMETRIC_REPRESENTATION_ITEM()
RATIONAL_B_SPLINE_CURVE((1.13348223894614,1.13389822901349,1.13426390111356))
REPRESENTATION_ITEM('')
);
#923=(
BOUNDED_CURVE()
B_SPLINE_CURVE(2,(#60929,#60930,#60931),.UNSPECIFIED.,.F.,.F.)
B_SPLINE_CURVE_WITH_KNOTS((3,3),(0.367644516946566,0.373830527582539),
 .UNSPECIFIED.)
CURVE()
GEOMETRIC_REPRESENTATION_ITEM()
RATIONAL_B_SPLINE_CURVE((1.13426390111297,1.1338982290129,1.13348223894556))
REPRESENTATION_ITEM('')
);
#924=(
BOUNDED_CURVE()
B_SPLINE_CURVE(2,(#60935,#60936,#60937),.UNSPECIFIED.,.F.,.F.)
B_SPLINE_CURVE_WITH_KNOTS((3,3),(0.271548216895926,0.277734227531904),
 .UNSPECIFIED.)
CURVE()
GEOMETRIC_REPRESENTATION_ITEM()
RATIONAL_B_SPLINE_CURVE((1.13348223894627,1.13389822901362,1.1342639011137))
REPRESENTATION_ITEM('')
);
#925=(
BOUNDED_CURVE()
B_SPLINE_CURVE(2,(#60941,#60942,#60943),.UNSPECIFIED.,.F.,.F.)
B_SPLINE_CURVE_WITH_KNOTS((3,3),(0.367644516946557,0.373830527582532),
 .UNSPECIFIED.)
CURVE()
GEOMETRIC_REPRESENTATION_ITEM()
RATIONAL_B_SPLINE_CURVE((1.13426390111306,1.13389822901299,1.13348223894565))
REPRESENTATION_ITEM('')
);
#926=(
BOUNDED_CURVE()
B_SPLINE_CURVE(2,(#60947,#60948,#60949),.UNSPECIFIED.,.F.,.F.)
B_SPLINE_CURVE_WITH_KNOTS((3,3),(0.271548216895913,0.277734227531899),
 .UNSPECIFIED.)
CURVE()
GEOMETRIC_REPRESENTATION_ITEM()
RATIONAL_B_SPLINE_CURVE((1.13348223894618,1.13389822901353,1.13426390111361))
REPRESENTATION_ITEM('')
);
#927=(
BOUNDED_CURVE()
B_SPLINE_CURVE(2,(#60953,#60954,#60955),.UNSPECIFIED.,.F.,.F.)
B_SPLINE_CURVE_WITH_KNOTS((3,3),(0.367644516946561,0.373830527582535),
 .UNSPECIFIED.)
CURVE()
GEOMETRIC_REPRESENTATION_ITEM()
RATIONAL_B_SPLINE_CURVE((1.13426390111305,1.13389822901298,1.13348223894564))
REPRESENTATION_ITEM('')
);
#928=(
BOUNDED_CURVE()
B_SPLINE_CURVE(2,(#60959,#60960,#60961),.UNSPECIFIED.,.F.,.F.)
B_SPLINE_CURVE_WITH_KNOTS((3,3),(0.271548216895915,0.277734227531905),
 .UNSPECIFIED.)
CURVE()
GEOMETRIC_REPRESENTATION_ITEM()
RATIONAL_B_SPLINE_CURVE((1.13348223894613,1.13389822901348,1.13426390111356))
REPRESENTATION_ITEM('')
);
#929=(
BOUNDED_CURVE()
B_SPLINE_CURVE(2,(#60965,#60966,#60967),.UNSPECIFIED.,.F.,.F.)
B_SPLINE_CURVE_WITH_KNOTS((3,3),(0.367644516946559,0.373830527582528),
 .UNSPECIFIED.)
CURVE()
GEOMETRIC_REPRESENTATION_ITEM()
RATIONAL_B_SPLINE_CURVE((1.13426390111303,1.13389822901297,1.13348223894562))
REPRESENTATION_ITEM('')
);
#930=(
BOUNDED_CURVE()
B_SPLINE_CURVE(2,(#60971,#60972,#60973),.UNSPECIFIED.,.F.,.F.)
B_SPLINE_CURVE_WITH_KNOTS((3,3),(0.271548216895913,0.277734227531899),
 .UNSPECIFIED.)
CURVE()
GEOMETRIC_REPRESENTATION_ITEM()
RATIONAL_B_SPLINE_CURVE((1.13348223894613,1.13389822901348,1.13426390111356))
REPRESENTATION_ITEM('')
);
#931=(
BOUNDED_CURVE()
B_SPLINE_CURVE(2,(#60977,#60978,#60979),.UNSPECIFIED.,.F.,.F.)
B_SPLINE_CURVE_WITH_KNOTS((3,3),(0.367644516946557,0.373830527582533),
 .UNSPECIFIED.)
CURVE()
GEOMETRIC_REPRESENTATION_ITEM()
RATIONAL_B_SPLINE_CURVE((1.13426390111302,1.13389822901296,1.13348223894561))
REPRESENTATION_ITEM('')
);
#932=(
BOUNDED_CURVE()
B_SPLINE_CURVE(2,(#60983,#60984,#60985),.UNSPECIFIED.,.F.,.F.)
B_SPLINE_CURVE_WITH_KNOTS((3,3),(0.271548216895926,0.277734227531906),
 .UNSPECIFIED.)
CURVE()
GEOMETRIC_REPRESENTATION_ITEM()
RATIONAL_B_SPLINE_CURVE((1.13348223894624,1.13389822901359,1.13426390111366))
REPRESENTATION_ITEM('')
);
#933=(
BOUNDED_CURVE()
B_SPLINE_CURVE(2,(#60989,#60990,#60991),.UNSPECIFIED.,.F.,.F.)
B_SPLINE_CURVE_WITH_KNOTS((3,3),(0.367644516946561,0.373830527582536),
 .UNSPECIFIED.)
CURVE()
GEOMETRIC_REPRESENTATION_ITEM()
RATIONAL_B_SPLINE_CURVE((1.13426390111306,1.13389822901299,1.13348223894564))
REPRESENTATION_ITEM('')
);
#934=(
BOUNDED_CURVE()
B_SPLINE_CURVE(2,(#60995,#60996,#60997),.UNSPECIFIED.,.F.,.F.)
B_SPLINE_CURVE_WITH_KNOTS((3,3),(0.271548216895911,0.277734227531901),
 .UNSPECIFIED.)
CURVE()
GEOMETRIC_REPRESENTATION_ITEM()
RATIONAL_B_SPLINE_CURVE((1.13348223894609,1.13389822901344,1.13426390111352))
REPRESENTATION_ITEM('')
);
#935=(
BOUNDED_CURVE()
B_SPLINE_CURVE(2,(#61001,#61002,#61003),.UNSPECIFIED.,.F.,.F.)
B_SPLINE_CURVE_WITH_KNOTS((3,3),(0.367644516946558,0.373830527582533),
 .UNSPECIFIED.)
CURVE()
GEOMETRIC_REPRESENTATION_ITEM()
RATIONAL_B_SPLINE_CURVE((1.1342639011131,1.13389822901303,1.13348223894569))
REPRESENTATION_ITEM('')
);
#936=(
BOUNDED_CURVE()
B_SPLINE_CURVE(2,(#61007,#61008,#61009),.UNSPECIFIED.,.F.,.F.)
B_SPLINE_CURVE_WITH_KNOTS((3,3),(0.271548216895922,0.277734227531909),
 .UNSPECIFIED.)
CURVE()
GEOMETRIC_REPRESENTATION_ITEM()
RATIONAL_B_SPLINE_CURVE((1.13348223894623,1.13389822901358,1.13426390111366))
REPRESENTATION_ITEM('')
);
#937=(
BOUNDED_CURVE()
B_SPLINE_CURVE(2,(#61013,#61014,#61015),.UNSPECIFIED.,.F.,.F.)
B_SPLINE_CURVE_WITH_KNOTS((3,3),(0.367644516946562,0.373830527582538),
 .UNSPECIFIED.)
CURVE()
GEOMETRIC_REPRESENTATION_ITEM()
RATIONAL_B_SPLINE_CURVE((1.13426390111305,1.13389822901298,1.13348223894563))
REPRESENTATION_ITEM('')
);
#938=(
BOUNDED_CURVE()
B_SPLINE_CURVE(2,(#61019,#61020,#61021),.UNSPECIFIED.,.F.,.F.)
B_SPLINE_CURVE_WITH_KNOTS((3,3),(0.271548216895906,0.277734227531898),
 .UNSPECIFIED.)
CURVE()
GEOMETRIC_REPRESENTATION_ITEM()
RATIONAL_B_SPLINE_CURVE((1.13348223894604,1.13389822901339,1.13426390111346))
REPRESENTATION_ITEM('')
);
#939=(
BOUNDED_CURVE()
B_SPLINE_CURVE(2,(#61025,#61026,#61027),.UNSPECIFIED.,.F.,.F.)
B_SPLINE_CURVE_WITH_KNOTS((3,3),(0.367644516946563,0.373830527582537),
 .UNSPECIFIED.)
CURVE()
GEOMETRIC_REPRESENTATION_ITEM()
RATIONAL_B_SPLINE_CURVE((1.134263901113,1.13389822901294,1.13348223894559))
REPRESENTATION_ITEM('')
);
#940=(
BOUNDED_CURVE()
B_SPLINE_CURVE(2,(#61031,#61032,#61033),.UNSPECIFIED.,.F.,.F.)
B_SPLINE_CURVE_WITH_KNOTS((3,3),(0.271548216895914,0.277734227531897),
 .UNSPECIFIED.)
CURVE()
GEOMETRIC_REPRESENTATION_ITEM()
RATIONAL_B_SPLINE_CURVE((1.13348223894613,1.13389822901348,1.13426390111355))
REPRESENTATION_ITEM('')
);
#941=(
BOUNDED_CURVE()
B_SPLINE_CURVE(2,(#61037,#61038,#61039),.UNSPECIFIED.,.F.,.F.)
B_SPLINE_CURVE_WITH_KNOTS((3,3),(0.367644516946558,0.373830527582532),
 .UNSPECIFIED.)
CURVE()
GEOMETRIC_REPRESENTATION_ITEM()
RATIONAL_B_SPLINE_CURVE((1.13426390111307,1.133898229013,1.13348223894566))
REPRESENTATION_ITEM('')
);
#942=(
BOUNDED_CURVE()
B_SPLINE_CURVE(2,(#61043,#61044,#61045),.UNSPECIFIED.,.F.,.F.)
B_SPLINE_CURVE_WITH_KNOTS((3,3),(0.271548216895917,0.277734227531901),
 .UNSPECIFIED.)
CURVE()
GEOMETRIC_REPRESENTATION_ITEM()
RATIONAL_B_SPLINE_CURVE((1.13348223894616,1.1338982290135,1.13426390111358))
REPRESENTATION_ITEM('')
);
#943=(
BOUNDED_CURVE()
B_SPLINE_CURVE(2,(#61049,#61050,#61051),.UNSPECIFIED.,.F.,.F.)
B_SPLINE_CURVE_WITH_KNOTS((3,3),(0.367644516946556,0.37383052758253),
 .UNSPECIFIED.)
CURVE()
GEOMETRIC_REPRESENTATION_ITEM()
RATIONAL_B_SPLINE_CURVE((1.13426390111304,1.13389822901297,1.13348223894563))
REPRESENTATION_ITEM('')
);
#944=(
BOUNDED_CURVE()
B_SPLINE_CURVE(2,(#61055,#61056,#61057),.UNSPECIFIED.,.F.,.F.)
B_SPLINE_CURVE_WITH_KNOTS((3,3),(0.271548216895911,0.277734227531893),
 .UNSPECIFIED.)
CURVE()
GEOMETRIC_REPRESENTATION_ITEM()
RATIONAL_B_SPLINE_CURVE((1.13348223894607,1.13389822901342,1.13426390111349))
REPRESENTATION_ITEM('')
);
#945=(
BOUNDED_CURVE()
B_SPLINE_CURVE(2,(#61061,#61062,#61063),.UNSPECIFIED.,.F.,.F.)
B_SPLINE_CURVE_WITH_KNOTS((3,3),(0.367644516946565,0.373830527582539),
 .UNSPECIFIED.)
CURVE()
GEOMETRIC_REPRESENTATION_ITEM()
RATIONAL_B_SPLINE_CURVE((1.13426390111301,1.13389822901295,1.1334822389456))
REPRESENTATION_ITEM('')
);
#946=(
BOUNDED_CURVE()
B_SPLINE_CURVE(2,(#61067,#61068,#61069),.UNSPECIFIED.,.F.,.F.)
B_SPLINE_CURVE_WITH_KNOTS((3,3),(0.271548216895916,0.277734227531897),
 .UNSPECIFIED.)
CURVE()
GEOMETRIC_REPRESENTATION_ITEM()
RATIONAL_B_SPLINE_CURVE((1.13348223894613,1.13389822901348,1.13426390111355))
REPRESENTATION_ITEM('')
);
#947=(
BOUNDED_CURVE()
B_SPLINE_CURVE(2,(#61073,#61074,#61075),.UNSPECIFIED.,.F.,.F.)
B_SPLINE_CURVE_WITH_KNOTS((3,3),(0.36764451694656,0.373830527582534),
 .UNSPECIFIED.)
CURVE()
GEOMETRIC_REPRESENTATION_ITEM()
RATIONAL_B_SPLINE_CURVE((1.13426390111306,1.13389822901299,1.13348223894564))
REPRESENTATION_ITEM('')
);
#948=(
BOUNDED_CURVE()
B_SPLINE_CURVE(2,(#61079,#61080,#61081),.UNSPECIFIED.,.F.,.F.)
B_SPLINE_CURVE_WITH_KNOTS((3,3),(0.271548216895918,0.277734227531904),
 .UNSPECIFIED.)
CURVE()
GEOMETRIC_REPRESENTATION_ITEM()
RATIONAL_B_SPLINE_CURVE((1.13348223894613,1.13389822901348,1.13426390111355))
REPRESENTATION_ITEM('')
);
#949=(
BOUNDED_CURVE()
B_SPLINE_CURVE(2,(#61085,#61086,#61087),.UNSPECIFIED.,.F.,.F.)
B_SPLINE_CURVE_WITH_KNOTS((3,3),(0.367644516946555,0.373830527582533),
 .UNSPECIFIED.)
CURVE()
GEOMETRIC_REPRESENTATION_ITEM()
RATIONAL_B_SPLINE_CURVE((1.13426390111305,1.13389822901298,1.13348223894564))
REPRESENTATION_ITEM('')
);
#950=(
BOUNDED_CURVE()
B_SPLINE_CURVE(2,(#61091,#61092,#61093),.UNSPECIFIED.,.F.,.F.)
B_SPLINE_CURVE_WITH_KNOTS((3,3),(0.271548216895928,0.277734227531916),
 .UNSPECIFIED.)
CURVE()
GEOMETRIC_REPRESENTATION_ITEM()
RATIONAL_B_SPLINE_CURVE((1.13348223894621,1.13389822901356,1.13426390111363))
REPRESENTATION_ITEM('')
);
#951=(
BOUNDED_CURVE()
B_SPLINE_CURVE(2,(#61097,#61098,#61099),.UNSPECIFIED.,.F.,.F.)
B_SPLINE_CURVE_WITH_KNOTS((3,3),(0.367644516946548,0.373830527582523),
 .UNSPECIFIED.)
CURVE()
GEOMETRIC_REPRESENTATION_ITEM()
RATIONAL_B_SPLINE_CURVE((1.13426390111312,1.13389822901305,1.13348223894571))
REPRESENTATION_ITEM('')
);
#952=(
BOUNDED_CURVE()
B_SPLINE_CURVE(2,(#61103,#61104,#61105),.UNSPECIFIED.,.F.,.F.)
B_SPLINE_CURVE_WITH_KNOTS((3,3),(0.271548216895918,0.277734227531905),
 .UNSPECIFIED.)
CURVE()
GEOMETRIC_REPRESENTATION_ITEM()
RATIONAL_B_SPLINE_CURVE((1.13348223894611,1.13389822901346,1.13426390111354))
REPRESENTATION_ITEM('')
);
#953=(
BOUNDED_CURVE()
B_SPLINE_CURVE(2,(#61109,#61110,#61111),.UNSPECIFIED.,.F.,.F.)
B_SPLINE_CURVE_WITH_KNOTS((3,3),(0.367644516946559,0.373830527582532),
 .UNSPECIFIED.)
CURVE()
GEOMETRIC_REPRESENTATION_ITEM()
RATIONAL_B_SPLINE_CURVE((1.13426390111305,1.13389822901298,1.13348223894564))
REPRESENTATION_ITEM('')
);
#954=(
BOUNDED_CURVE()
B_SPLINE_CURVE(2,(#61115,#61116,#61117),.UNSPECIFIED.,.F.,.F.)
B_SPLINE_CURVE_WITH_KNOTS((3,3),(0.271548216895915,0.277734227531901),
 .UNSPECIFIED.)
CURVE()
GEOMETRIC_REPRESENTATION_ITEM()
RATIONAL_B_SPLINE_CURVE((1.13348223894615,1.1338982290135,1.13426390111357))
REPRESENTATION_ITEM('')
);
#955=(
BOUNDED_CURVE()
B_SPLINE_CURVE(2,(#61121,#61122,#61123),.UNSPECIFIED.,.F.,.F.)
B_SPLINE_CURVE_WITH_KNOTS((3,3),(0.367644516946548,0.373830527582526),
 .UNSPECIFIED.)
CURVE()
GEOMETRIC_REPRESENTATION_ITEM()
RATIONAL_B_SPLINE_CURVE((1.13426390111308,1.13389822901302,1.13348223894567))
REPRESENTATION_ITEM('')
);
#956=(
BOUNDED_CURVE()
B_SPLINE_CURVE(2,(#61127,#61128,#61129),.UNSPECIFIED.,.F.,.F.)
B_SPLINE_CURVE_WITH_KNOTS((3,3),(0.271548216895917,0.277734227531902),
 .UNSPECIFIED.)
CURVE()
GEOMETRIC_REPRESENTATION_ITEM()
RATIONAL_B_SPLINE_CURVE((1.13348223894615,1.1338982290135,1.13426390111358))
REPRESENTATION_ITEM('')
);
#957=(
BOUNDED_CURVE()
B_SPLINE_CURVE(2,(#61133,#61134,#61135),.UNSPECIFIED.,.F.,.F.)
B_SPLINE_CURVE_WITH_KNOTS((3,3),(0.367644516946561,0.373830527582534),
 .UNSPECIFIED.)
CURVE()
GEOMETRIC_REPRESENTATION_ITEM()
RATIONAL_B_SPLINE_CURVE((1.13426390111303,1.13389822901296,1.13348223894562))
REPRESENTATION_ITEM('')
);
#958=(
BOUNDED_CURVE()
B_SPLINE_CURVE(2,(#61139,#61140,#61141),.UNSPECIFIED.,.F.,.F.)
B_SPLINE_CURVE_WITH_KNOTS((3,3),(0.271548216895922,0.277734227531908),
 .UNSPECIFIED.)
CURVE()
GEOMETRIC_REPRESENTATION_ITEM()
RATIONAL_B_SPLINE_CURVE((1.13348223894617,1.13389822901352,1.1342639011136))
REPRESENTATION_ITEM('')
);
#959=(
BOUNDED_CURVE()
B_SPLINE_CURVE(2,(#61145,#61146,#61147),.UNSPECIFIED.,.F.,.F.)
B_SPLINE_CURVE_WITH_KNOTS((3,3),(0.367644516946555,0.373830527582532),
 .UNSPECIFIED.)
CURVE()
GEOMETRIC_REPRESENTATION_ITEM()
RATIONAL_B_SPLINE_CURVE((1.13426390111307,1.133898229013,1.13348223894566))
REPRESENTATION_ITEM('')
);
#960=(
BOUNDED_CURVE()
B_SPLINE_CURVE(2,(#61151,#61152,#61153),.UNSPECIFIED.,.F.,.F.)
B_SPLINE_CURVE_WITH_KNOTS((3,3),(0.27154821689592,0.277734227531907),
 .UNSPECIFIED.)
CURVE()
GEOMETRIC_REPRESENTATION_ITEM()
RATIONAL_B_SPLINE_CURVE((1.13348223894614,1.13389822901349,1.13426390111356))
REPRESENTATION_ITEM('')
);
#961=(
BOUNDED_CURVE()
B_SPLINE_CURVE(2,(#61157,#61158,#61159),.UNSPECIFIED.,.F.,.F.)
B_SPLINE_CURVE_WITH_KNOTS((3,3),(0.367644516946564,0.373830527582538),
 .UNSPECIFIED.)
CURVE()
GEOMETRIC_REPRESENTATION_ITEM()
RATIONAL_B_SPLINE_CURVE((1.13426390111299,1.13389822901292,1.13348223894557))
REPRESENTATION_ITEM('')
);
#962=(
BOUNDED_CURVE()
B_SPLINE_CURVE(2,(#61163,#61164,#61165),.UNSPECIFIED.,.F.,.F.)
B_SPLINE_CURVE_WITH_KNOTS((3,3),(0.271548216895926,0.277734227531912),
 .UNSPECIFIED.)
CURVE()
GEOMETRIC_REPRESENTATION_ITEM()
RATIONAL_B_SPLINE_CURVE((1.13348223894617,1.13389822901352,1.13426390111359))
REPRESENTATION_ITEM('')
);
#963=(
BOUNDED_CURVE()
B_SPLINE_CURVE(2,(#61169,#61170,#61171),.UNSPECIFIED.,.F.,.F.)
B_SPLINE_CURVE_WITH_KNOTS((3,3),(0.367644516946548,0.373830527582525),
 .UNSPECIFIED.)
CURVE()
GEOMETRIC_REPRESENTATION_ITEM()
RATIONAL_B_SPLINE_CURVE((1.13426390111308,1.13389822901301,1.13348223894567))
REPRESENTATION_ITEM('')
);
#964=(
BOUNDED_CURVE()
B_SPLINE_CURVE(2,(#61175,#61176,#61177),.UNSPECIFIED.,.F.,.F.)
B_SPLINE_CURVE_WITH_KNOTS((3,3),(0.271548216895921,0.277734227531907),
 .UNSPECIFIED.)
CURVE()
GEOMETRIC_REPRESENTATION_ITEM()
RATIONAL_B_SPLINE_CURVE((1.13348223894617,1.13389822901352,1.13426390111359))
REPRESENTATION_ITEM('')
);
#965=(
BOUNDED_CURVE()
B_SPLINE_CURVE(2,(#61181,#61182,#61183),.UNSPECIFIED.,.F.,.F.)
B_SPLINE_CURVE_WITH_KNOTS((3,3),(0.367644516946557,0.373830527582527),
 .UNSPECIFIED.)
CURVE()
GEOMETRIC_REPRESENTATION_ITEM()
RATIONAL_B_SPLINE_CURVE((1.1342639011131,1.13389822901303,1.13348223894569))
REPRESENTATION_ITEM('')
);
#966=(
BOUNDED_CURVE()
B_SPLINE_CURVE(2,(#61186,#61187,#61188),.UNSPECIFIED.,.F.,.F.)
B_SPLINE_CURVE_WITH_KNOTS((3,3),(0.271548216895922,0.277734227531908),
 .UNSPECIFIED.)
CURVE()
GEOMETRIC_REPRESENTATION_ITEM()
RATIONAL_B_SPLINE_CURVE((1.13348223894615,1.1338982290135,1.13426390111358))
REPRESENTATION_ITEM('')
);
#967=(
BOUNDED_CURVE()
B_SPLINE_CURVE(2,(#61190,#61191,#61192),.UNSPECIFIED.,.F.,.F.)
B_SPLINE_CURVE_WITH_KNOTS((3,3),(0.367644516946556,0.373830527582529),
 .UNSPECIFIED.)
CURVE()
GEOMETRIC_REPRESENTATION_ITEM()
RATIONAL_B_SPLINE_CURVE((1.13426390111308,1.13389822901301,1.13348223894567))
REPRESENTATION_ITEM('')
);
#968=(
BOUNDED_CURVE()
B_SPLINE_CURVE(2,(#61195,#61196,#61197),.UNSPECIFIED.,.F.,.F.)
B_SPLINE_CURVE_WITH_KNOTS((3,3),(0.271548216895921,0.277734227531909),
 .UNSPECIFIED.)
CURVE()
GEOMETRIC_REPRESENTATION_ITEM()
RATIONAL_B_SPLINE_CURVE((1.13348223894619,1.13389822901354,1.13426390111361))
REPRESENTATION_ITEM('')
);
#969=(
BOUNDED_CURVE()
B_SPLINE_CURVE(2,(#61199,#61200,#61201),.UNSPECIFIED.,.F.,.F.)
B_SPLINE_CURVE_WITH_KNOTS((3,3),(0.36764451694656,0.37383052758253),
 .UNSPECIFIED.)
CURVE()
GEOMETRIC_REPRESENTATION_ITEM()
RATIONAL_B_SPLINE_CURVE((1.13426390111303,1.13389822901296,1.13348223894562))
REPRESENTATION_ITEM('')
);
#970=(
BOUNDED_CURVE()
B_SPLINE_CURVE(2,(#61204,#61205,#61206),.UNSPECIFIED.,.F.,.F.)
B_SPLINE_CURVE_WITH_KNOTS((3,3),(0.271548216895921,0.277734227531907),
 .UNSPECIFIED.)
CURVE()
GEOMETRIC_REPRESENTATION_ITEM()
RATIONAL_B_SPLINE_CURVE((1.13348223894618,1.13389822901353,1.1342639011136))
REPRESENTATION_ITEM('')
);
#971=(
BOUNDED_CURVE()
B_SPLINE_CURVE(2,(#61208,#61209,#61210),.UNSPECIFIED.,.F.,.F.)
B_SPLINE_CURVE_WITH_KNOTS((3,3),(0.367644516946553,0.373830527582534),
 .UNSPECIFIED.)
CURVE()
GEOMETRIC_REPRESENTATION_ITEM()
RATIONAL_B_SPLINE_CURVE((1.13426390111306,1.13389822901299,1.13348223894565))
REPRESENTATION_ITEM('')
);
#972=(
BOUNDED_CURVE()
B_SPLINE_CURVE(2,(#61213,#61214,#61215),.UNSPECIFIED.,.F.,.F.)
B_SPLINE_CURVE_WITH_KNOTS((3,3),(0.271548216895916,0.277734227531903),
 .UNSPECIFIED.)
CURVE()
GEOMETRIC_REPRESENTATION_ITEM()
RATIONAL_B_SPLINE_CURVE((1.13348223894615,1.1338982290135,1.13426390111357))
REPRESENTATION_ITEM('')
);
#973=(
BOUNDED_CURVE()
B_SPLINE_CURVE(2,(#61217,#61218,#61219),.UNSPECIFIED.,.F.,.F.)
B_SPLINE_CURVE_WITH_KNOTS((3,3),(0.367644516946558,0.373830527582532),
 .UNSPECIFIED.)
CURVE()
GEOMETRIC_REPRESENTATION_ITEM()
RATIONAL_B_SPLINE_CURVE((1.13426390111307,1.13389822901301,1.13348223894566))
REPRESENTATION_ITEM('')
);
#974=(
BOUNDED_CURVE()
B_SPLINE_CURVE(2,(#61222,#61223,#61224),.UNSPECIFIED.,.F.,.F.)
B_SPLINE_CURVE_WITH_KNOTS((3,3),(0.271548216895911,0.277734227531895),
 .UNSPECIFIED.)
CURVE()
GEOMETRIC_REPRESENTATION_ITEM()
RATIONAL_B_SPLINE_CURVE((1.13348223894606,1.13389822901341,1.13426390111348))
REPRESENTATION_ITEM('')
);
#975=(
BOUNDED_CURVE()
B_SPLINE_CURVE(2,(#61226,#61227,#61228),.UNSPECIFIED.,.F.,.F.)
B_SPLINE_CURVE_WITH_KNOTS((3,3),(0.367644516946553,0.373830527582531),
 .UNSPECIFIED.)
CURVE()
GEOMETRIC_REPRESENTATION_ITEM()
RATIONAL_B_SPLINE_CURVE((1.13426390111307,1.133898229013,1.13348223894566))
REPRESENTATION_ITEM('')
);
#976=(
BOUNDED_CURVE()
B_SPLINE_CURVE(2,(#61231,#61232,#61233),.UNSPECIFIED.,.F.,.F.)
B_SPLINE_CURVE_WITH_KNOTS((3,3),(0.271548216895918,0.277734227531903),
 .UNSPECIFIED.)
CURVE()
GEOMETRIC_REPRESENTATION_ITEM()
RATIONAL_B_SPLINE_CURVE((1.13348223894611,1.13389822901346,1.13426390111353))
REPRESENTATION_ITEM('')
);
#977=(
BOUNDED_CURVE()
B_SPLINE_CURVE(2,(#61235,#61236,#61237),.UNSPECIFIED.,.F.,.F.)
B_SPLINE_CURVE_WITH_KNOTS((3,3),(0.367644516946551,0.373830527582526),
 .UNSPECIFIED.)
CURVE()
GEOMETRIC_REPRESENTATION_ITEM()
RATIONAL_B_SPLINE_CURVE((1.1342639011131,1.13389822901304,1.13348223894569))
REPRESENTATION_ITEM('')
);
#978=(
BOUNDED_CURVE()
B_SPLINE_CURVE(2,(#61240,#61241,#61242),.UNSPECIFIED.,.F.,.F.)
B_SPLINE_CURVE_WITH_KNOTS((3,3),(0.271548216895922,0.277734227531909),
 .UNSPECIFIED.)
CURVE()
GEOMETRIC_REPRESENTATION_ITEM()
RATIONAL_B_SPLINE_CURVE((1.13348223894615,1.1338982290135,1.13426390111357))
REPRESENTATION_ITEM('')
);
#979=(
BOUNDED_CURVE()
B_SPLINE_CURVE(2,(#61244,#61245,#61246),.UNSPECIFIED.,.F.,.F.)
B_SPLINE_CURVE_WITH_KNOTS((3,3),(0.36764451694656,0.373830527582534),
 .UNSPECIFIED.)
CURVE()
GEOMETRIC_REPRESENTATION_ITEM()
RATIONAL_B_SPLINE_CURVE((1.13426390111304,1.13389822901297,1.13348223894563))
REPRESENTATION_ITEM('')
);
#980=(
BOUNDED_CURVE()
B_SPLINE_CURVE(2,(#61249,#61250,#61251),.UNSPECIFIED.,.F.,.F.)
B_SPLINE_CURVE_WITH_KNOTS((3,3),(0.271548216895917,0.277734227531904),
 .UNSPECIFIED.)
CURVE()
GEOMETRIC_REPRESENTATION_ITEM()
RATIONAL_B_SPLINE_CURVE((1.13348223894616,1.13389822901351,1.13426390111359))
REPRESENTATION_ITEM('')
);
#981=(
BOUNDED_CURVE()
B_SPLINE_CURVE(2,(#61253,#61254,#61255),.UNSPECIFIED.,.F.,.F.)
B_SPLINE_CURVE_WITH_KNOTS((3,3),(0.367644516946562,0.373830527582537),
 .UNSPECIFIED.)
CURVE()
GEOMETRIC_REPRESENTATION_ITEM()
RATIONAL_B_SPLINE_CURVE((1.13426390111298,1.13389822901291,1.13348223894556))
REPRESENTATION_ITEM('')
);
#982=(
BOUNDED_CURVE()
B_SPLINE_CURVE(2,(#61258,#61259,#61260),.UNSPECIFIED.,.F.,.F.)
B_SPLINE_CURVE_WITH_KNOTS((3,3),(0.271548216895925,0.277734227531911),
 .UNSPECIFIED.)
CURVE()
GEOMETRIC_REPRESENTATION_ITEM()
RATIONAL_B_SPLINE_CURVE((1.13348223894616,1.13389822901351,1.13426390111359))
REPRESENTATION_ITEM('')
);
#983=(
BOUNDED_CURVE()
B_SPLINE_CURVE(2,(#61262,#61263,#61264),.UNSPECIFIED.,.F.,.F.)
B_SPLINE_CURVE_WITH_KNOTS((3,3),(0.367644516946555,0.373830527582529),
 .UNSPECIFIED.)
CURVE()
GEOMETRIC_REPRESENTATION_ITEM()
RATIONAL_B_SPLINE_CURVE((1.13426390111312,1.13389822901305,1.13348223894571))
REPRESENTATION_ITEM('')
);
#984=(
BOUNDED_CURVE()
B_SPLINE_CURVE(2,(#61267,#61268,#61269),.UNSPECIFIED.,.F.,.F.)
B_SPLINE_CURVE_WITH_KNOTS((3,3),(0.271548216895925,0.277734227531912),
 .UNSPECIFIED.)
CURVE()
GEOMETRIC_REPRESENTATION_ITEM()
RATIONAL_B_SPLINE_CURVE((1.13348223894618,1.13389822901353,1.1342639011136))
REPRESENTATION_ITEM('')
);
#985=(
BOUNDED_CURVE()
B_SPLINE_CURVE(2,(#61271,#61272,#61273),.UNSPECIFIED.,.F.,.F.)
B_SPLINE_CURVE_WITH_KNOTS((3,3),(0.367644516946557,0.373830527582532),
 .UNSPECIFIED.)
CURVE()
GEOMETRIC_REPRESENTATION_ITEM()
RATIONAL_B_SPLINE_CURVE((1.13426390111306,1.13389822901299,1.13348223894564))
REPRESENTATION_ITEM('')
);
#986=(
BOUNDED_CURVE()
B_SPLINE_CURVE(2,(#61276,#61277,#61278),.UNSPECIFIED.,.F.,.F.)
B_SPLINE_CURVE_WITH_KNOTS((3,3),(0.271548216895908,0.277734227531892),
 .UNSPECIFIED.)
CURVE()
GEOMETRIC_REPRESENTATION_ITEM()
RATIONAL_B_SPLINE_CURVE((1.13348223894609,1.13389822901344,1.13426390111352))
REPRESENTATION_ITEM('')
);
#987=(
BOUNDED_CURVE()
B_SPLINE_CURVE(2,(#61280,#61281,#61282),.UNSPECIFIED.,.F.,.F.)
B_SPLINE_CURVE_WITH_KNOTS((3,3),(0.367644516946557,0.373830527582522),
 .UNSPECIFIED.)
CURVE()
GEOMETRIC_REPRESENTATION_ITEM()
RATIONAL_B_SPLINE_CURVE((1.13426390111309,1.13389822901302,1.13348223894568))
REPRESENTATION_ITEM('')
);
#988=(
BOUNDED_CURVE()
B_SPLINE_CURVE(2,(#61285,#61286,#61287),.UNSPECIFIED.,.F.,.F.)
B_SPLINE_CURVE_WITH_KNOTS((3,3),(0.271548216895913,0.277734227531902),
 .UNSPECIFIED.)
CURVE()
GEOMETRIC_REPRESENTATION_ITEM()
RATIONAL_B_SPLINE_CURVE((1.1334822389461,1.13389822901345,1.13426390111352))
REPRESENTATION_ITEM('')
);
#989=(
BOUNDED_CURVE()
B_SPLINE_CURVE(2,(#61289,#61290,#61291),.UNSPECIFIED.,.F.,.F.)
B_SPLINE_CURVE_WITH_KNOTS((3,3),(0.367644516946559,0.373830527582539),
 .UNSPECIFIED.)
CURVE()
GEOMETRIC_REPRESENTATION_ITEM()
RATIONAL_B_SPLINE_CURVE((1.13426390111296,1.13389822901289,1.13348223894555))
REPRESENTATION_ITEM('')
);
#990=(
BOUNDED_CURVE()
B_SPLINE_CURVE(2,(#61294,#61295,#61296),.UNSPECIFIED.,.F.,.F.)
B_SPLINE_CURVE_WITH_KNOTS((3,3),(0.271548216895926,0.277734227531913),
 .UNSPECIFIED.)
CURVE()
GEOMETRIC_REPRESENTATION_ITEM()
RATIONAL_B_SPLINE_CURVE((1.13348223894622,1.13389822901357,1.13426390111365))
REPRESENTATION_ITEM('')
);
#991=(
BOUNDED_CURVE()
B_SPLINE_CURVE(2,(#61298,#61299,#61300),.UNSPECIFIED.,.F.,.F.)
B_SPLINE_CURVE_WITH_KNOTS((3,3),(0.36764451694656,0.373830527582534),
 .UNSPECIFIED.)
CURVE()
GEOMETRIC_REPRESENTATION_ITEM()
RATIONAL_B_SPLINE_CURVE((1.13426390111298,1.13389822901291,1.13348223894557))
REPRESENTATION_ITEM('')
);
#992=(
BOUNDED_CURVE()
B_SPLINE_CURVE(2,(#61303,#61304,#61305),.UNSPECIFIED.,.F.,.F.)
B_SPLINE_CURVE_WITH_KNOTS((3,3),(0.271548216895926,0.277734227531909),
 .UNSPECIFIED.)
CURVE()
GEOMETRIC_REPRESENTATION_ITEM()
RATIONAL_B_SPLINE_CURVE((1.13348223894617,1.13389822901352,1.13426390111359))
REPRESENTATION_ITEM('')
);
#993=(
BOUNDED_CURVE()
B_SPLINE_CURVE(2,(#61307,#61308,#61309),.UNSPECIFIED.,.F.,.F.)
B_SPLINE_CURVE_WITH_KNOTS((3,3),(0.367644516946566,0.373830527582539),
 .UNSPECIFIED.)
CURVE()
GEOMETRIC_REPRESENTATION_ITEM()
RATIONAL_B_SPLINE_CURVE((1.13426390111296,1.13389822901289,1.13348223894555))
REPRESENTATION_ITEM('')
);
#994=(
BOUNDED_CURVE()
B_SPLINE_CURVE(2,(#61312,#61313,#61314),.UNSPECIFIED.,.F.,.F.)
B_SPLINE_CURVE_WITH_KNOTS((3,3),(0.271548216895918,0.277734227531904),
 .UNSPECIFIED.)
CURVE()
GEOMETRIC_REPRESENTATION_ITEM()
RATIONAL_B_SPLINE_CURVE((1.13348223894611,1.13389822901346,1.13426390111353))
REPRESENTATION_ITEM('')
);
#995=(
BOUNDED_CURVE()
B_SPLINE_CURVE(2,(#61316,#61317,#61318),.UNSPECIFIED.,.F.,.F.)
B_SPLINE_CURVE_WITH_KNOTS((3,3),(0.367644516946555,0.373830527582529),
 .UNSPECIFIED.)
CURVE()
GEOMETRIC_REPRESENTATION_ITEM()
RATIONAL_B_SPLINE_CURVE((1.13426390111303,1.13389822901296,1.13348223894562))
REPRESENTATION_ITEM('')
);
#996=(
BOUNDED_CURVE()
B_SPLINE_CURVE(2,(#61322,#61323,#61324),.UNSPECIFIED.,.F.,.F.)
B_SPLINE_CURVE_WITH_KNOTS((3,3),(0.271548216895927,0.277734227531913),
 .UNSPECIFIED.)
CURVE()
GEOMETRIC_REPRESENTATION_ITEM()
RATIONAL_B_SPLINE_CURVE((1.13348223894624,1.13389822901359,1.13426390111366))
REPRESENTATION_ITEM('')
);
#997=(
BOUNDED_CURVE()
B_SPLINE_CURVE(2,(#61328,#61329,#61330),.UNSPECIFIED.,.F.,.F.)
B_SPLINE_CURVE_WITH_KNOTS((3,3),(0.367644516946557,0.373830527582527),
 .UNSPECIFIED.)
CURVE()
GEOMETRIC_REPRESENTATION_ITEM()
RATIONAL_B_SPLINE_CURVE((1.1342639011131,1.13389822901303,1.13348223894569))
REPRESENTATION_ITEM('')
);
#998=(
BOUNDED_CURVE()
B_SPLINE_CURVE(2,(#61334,#61335,#61336),.UNSPECIFIED.,.F.,.F.)
B_SPLINE_CURVE_WITH_KNOTS((3,3),(0.27154821689592,0.277734227531904),
 .UNSPECIFIED.)
CURVE()
GEOMETRIC_REPRESENTATION_ITEM()
RATIONAL_B_SPLINE_CURVE((1.13348223894613,1.13389822901348,1.13426390111355))
REPRESENTATION_ITEM('')
);
#999=(
BOUNDED_CURVE()
B_SPLINE_CURVE(2,(#61340,#61341,#61342),.UNSPECIFIED.,.F.,.F.)
B_SPLINE_CURVE_WITH_KNOTS((3,3),(0.367644516946566,0.373830527582538),
 .UNSPECIFIED.)
CURVE()
GEOMETRIC_REPRESENTATION_ITEM()
RATIONAL_B_SPLINE_CURVE((1.13426390111301,1.13389822901294,1.1334822389456))
REPRESENTATION_ITEM('')
);
#1000=(
BOUNDED_CURVE()
B_SPLINE_CURVE(2,(#61346,#61347,#61348),.UNSPECIFIED.,.F.,.F.)
B_SPLINE_CURVE_WITH_KNOTS((3,3),(0.27154821689592,0.277734227531902),
 .UNSPECIFIED.)
CURVE()
GEOMETRIC_REPRESENTATION_ITEM()
RATIONAL_B_SPLINE_CURVE((1.1334822389461,1.13389822901344,1.13426390111352))
REPRESENTATION_ITEM('')
);
#1001=(
BOUNDED_CURVE()
B_SPLINE_CURVE(2,(#61352,#61353,#61354),.UNSPECIFIED.,.F.,.F.)
B_SPLINE_CURVE_WITH_KNOTS((3,3),(0.367644516946558,0.373830527582536),
 .UNSPECIFIED.)
CURVE()
GEOMETRIC_REPRESENTATION_ITEM()
RATIONAL_B_SPLINE_CURVE((1.13426390111303,1.13389822901296,1.13348223894562))
REPRESENTATION_ITEM('')
);
#1002=(
BOUNDED_CURVE()
B_SPLINE_CURVE(2,(#61358,#61359,#61360),.UNSPECIFIED.,.F.,.F.)
B_SPLINE_CURVE_WITH_KNOTS((3,3),(0.271548216895916,0.277734227531903),
 .UNSPECIFIED.)
CURVE()
GEOMETRIC_REPRESENTATION_ITEM()
RATIONAL_B_SPLINE_CURVE((1.13348223894608,1.13389822901343,1.1342639011135))
REPRESENTATION_ITEM('')
);
#1003=(
BOUNDED_CURVE()
B_SPLINE_CURVE(2,(#61364,#61365,#61366),.UNSPECIFIED.,.F.,.F.)
B_SPLINE_CURVE_WITH_KNOTS((3,3),(0.367644516946558,0.373830527582538),
 .UNSPECIFIED.)
CURVE()
GEOMETRIC_REPRESENTATION_ITEM()
RATIONAL_B_SPLINE_CURVE((1.13426390111299,1.13389822901292,1.13348223894558))
REPRESENTATION_ITEM('')
);
#1004=(
BOUNDED_CURVE()
B_SPLINE_CURVE(2,(#61370,#61371,#61372),.UNSPECIFIED.,.F.,.F.)
B_SPLINE_CURVE_WITH_KNOTS((3,3),(0.271548216895918,0.277734227531905),
 .UNSPECIFIED.)
CURVE()
GEOMETRIC_REPRESENTATION_ITEM()
RATIONAL_B_SPLINE_CURVE((1.13348223894618,1.13389822901353,1.1342639011136))
REPRESENTATION_ITEM('')
);
#1005=(
BOUNDED_CURVE()
B_SPLINE_CURVE(2,(#61376,#61377,#61378),.UNSPECIFIED.,.F.,.F.)
B_SPLINE_CURVE_WITH_KNOTS((3,3),(0.367644516946549,0.373830527582523),
 .UNSPECIFIED.)
CURVE()
GEOMETRIC_REPRESENTATION_ITEM()
RATIONAL_B_SPLINE_CURVE((1.13426390111313,1.13389822901306,1.13348223894572))
REPRESENTATION_ITEM('')
);
#1006=(
BOUNDED_CURVE()
B_SPLINE_CURVE(2,(#61382,#61383,#61384),.UNSPECIFIED.,.F.,.F.)
B_SPLINE_CURVE_WITH_KNOTS((3,3),(0.271548216895918,0.277734227531904),
 .UNSPECIFIED.)
CURVE()
GEOMETRIC_REPRESENTATION_ITEM()
RATIONAL_B_SPLINE_CURVE((1.13348223894607,1.13389822901342,1.1342639011135))
REPRESENTATION_ITEM('')
);
#1007=(
BOUNDED_CURVE()
B_SPLINE_CURVE(2,(#61388,#61389,#61390),.UNSPECIFIED.,.F.,.F.)
B_SPLINE_CURVE_WITH_KNOTS((3,3),(0.367644516946553,0.373830527582525),
 .UNSPECIFIED.)
CURVE()
GEOMETRIC_REPRESENTATION_ITEM()
RATIONAL_B_SPLINE_CURVE((1.13426390111306,1.133898229013,1.13348223894565))
REPRESENTATION_ITEM('')
);
#1008=(
BOUNDED_CURVE()
B_SPLINE_CURVE(2,(#61394,#61395,#61396),.UNSPECIFIED.,.F.,.F.)
B_SPLINE_CURVE_WITH_KNOTS((3,3),(0.271548216895918,0.277734227531897),
 .UNSPECIFIED.)
CURVE()
GEOMETRIC_REPRESENTATION_ITEM()
RATIONAL_B_SPLINE_CURVE((1.13348223894613,1.13389822901348,1.13426390111355))
REPRESENTATION_ITEM('')
);
#1009=(
BOUNDED_CURVE()
B_SPLINE_CURVE(2,(#61400,#61401,#61402),.UNSPECIFIED.,.F.,.F.)
B_SPLINE_CURVE_WITH_KNOTS((3,3),(0.367644516946551,0.373830527582524),
 .UNSPECIFIED.)
CURVE()
GEOMETRIC_REPRESENTATION_ITEM()
RATIONAL_B_SPLINE_CURVE((1.13426390111309,1.13389822901302,1.13348223894568))
REPRESENTATION_ITEM('')
);
#1010=(
BOUNDED_CURVE()
B_SPLINE_CURVE(2,(#61406,#61407,#61408),.UNSPECIFIED.,.F.,.F.)
B_SPLINE_CURVE_WITH_KNOTS((3,3),(0.271548216895914,0.2777342275319),
 .UNSPECIFIED.)
CURVE()
GEOMETRIC_REPRESENTATION_ITEM()
RATIONAL_B_SPLINE_CURVE((1.13348223894608,1.13389822901343,1.13426390111351))
REPRESENTATION_ITEM('')
);
#1011=(
BOUNDED_CURVE()
B_SPLINE_CURVE(2,(#61412,#61413,#61414),.UNSPECIFIED.,.F.,.F.)
B_SPLINE_CURVE_WITH_KNOTS((3,3),(0.367644516946559,0.373830527582536),
 .UNSPECIFIED.)
CURVE()
GEOMETRIC_REPRESENTATION_ITEM()
RATIONAL_B_SPLINE_CURVE((1.13426390111305,1.13389822901298,1.13348223894564))
REPRESENTATION_ITEM('')
);
#1012=(
BOUNDED_CURVE()
B_SPLINE_CURVE(2,(#61418,#61419,#61420),.UNSPECIFIED.,.F.,.F.)
B_SPLINE_CURVE_WITH_KNOTS((3,3),(0.27154821689591,0.277734227531898),
 .UNSPECIFIED.)
CURVE()
GEOMETRIC_REPRESENTATION_ITEM()
RATIONAL_B_SPLINE_CURVE((1.13348223894607,1.13389822901342,1.1342639011135))
REPRESENTATION_ITEM('')
);
#1013=(
BOUNDED_CURVE()
B_SPLINE_CURVE(2,(#61424,#61425,#61426),.UNSPECIFIED.,.F.,.F.)
B_SPLINE_CURVE_WITH_KNOTS((3,3),(0.367644516946559,0.373830527582532),
 .UNSPECIFIED.)
CURVE()
GEOMETRIC_REPRESENTATION_ITEM()
RATIONAL_B_SPLINE_CURVE((1.13426390111307,1.133898229013,1.13348223894566))
REPRESENTATION_ITEM('')
);
#1014=(
BOUNDED_CURVE()
B_SPLINE_CURVE(2,(#61430,#61431,#61432),.UNSPECIFIED.,.F.,.F.)
B_SPLINE_CURVE_WITH_KNOTS((3,3),(0.271548216895924,0.277734227531905),
 .UNSPECIFIED.)
CURVE()
GEOMETRIC_REPRESENTATION_ITEM()
RATIONAL_B_SPLINE_CURVE((1.13348223894618,1.13389822901353,1.1342639011136))
REPRESENTATION_ITEM('')
);
#1015=(
BOUNDED_CURVE()
B_SPLINE_CURVE(2,(#61436,#61437,#61438),.UNSPECIFIED.,.F.,.F.)
B_SPLINE_CURVE_WITH_KNOTS((3,3),(0.367644516946555,0.373830527582531),
 .UNSPECIFIED.)
CURVE()
GEOMETRIC_REPRESENTATION_ITEM()
RATIONAL_B_SPLINE_CURVE((1.134263901113,1.13389822901293,1.13348223894559))
REPRESENTATION_ITEM('')
);
#1016=(
BOUNDED_CURVE()
B_SPLINE_CURVE(2,(#61442,#61443,#61444),.UNSPECIFIED.,.F.,.F.)
B_SPLINE_CURVE_WITH_KNOTS((3,3),(0.271548216895916,0.277734227531902),
 .UNSPECIFIED.)
CURVE()
GEOMETRIC_REPRESENTATION_ITEM()
RATIONAL_B_SPLINE_CURVE((1.13348223894612,1.13389822901347,1.13426390111355))
REPRESENTATION_ITEM('')
);
#1017=(
BOUNDED_CURVE()
B_SPLINE_CURVE(2,(#61448,#61449,#61450),.UNSPECIFIED.,.F.,.F.)
B_SPLINE_CURVE_WITH_KNOTS((3,3),(0.36764451694656,0.373830527582534),
 .UNSPECIFIED.)
CURVE()
GEOMETRIC_REPRESENTATION_ITEM()
RATIONAL_B_SPLINE_CURVE((1.13426390111302,1.13389822901296,1.13348223894561))
REPRESENTATION_ITEM('')
);
#1018=(
BOUNDED_CURVE()
B_SPLINE_CURVE(2,(#61454,#61455,#61456),.UNSPECIFIED.,.F.,.F.)
B_SPLINE_CURVE_WITH_KNOTS((3,3),(0.271548216895913,0.277734227531896),
 .UNSPECIFIED.)
CURVE()
GEOMETRIC_REPRESENTATION_ITEM()
RATIONAL_B_SPLINE_CURVE((1.13348223894608,1.13389822901343,1.1342639011135))
REPRESENTATION_ITEM('')
);
#1019=(
BOUNDED_CURVE()
B_SPLINE_CURVE(2,(#61460,#61461,#61462),.UNSPECIFIED.,.F.,.F.)
B_SPLINE_CURVE_WITH_KNOTS((3,3),(0.367644516946558,0.373830527582535),
 .UNSPECIFIED.)
CURVE()
GEOMETRIC_REPRESENTATION_ITEM()
RATIONAL_B_SPLINE_CURVE((1.13426390111305,1.13389822901298,1.13348223894563))
REPRESENTATION_ITEM('')
);
#1020=(
BOUNDED_CURVE()
B_SPLINE_CURVE(2,(#61466,#61467,#61468),.UNSPECIFIED.,.F.,.F.)
B_SPLINE_CURVE_WITH_KNOTS((3,3),(0.271548216895911,0.277734227531902),
 .UNSPECIFIED.)
CURVE()
GEOMETRIC_REPRESENTATION_ITEM()
RATIONAL_B_SPLINE_CURVE((1.13348223894613,1.13389822901348,1.13426390111355))
REPRESENTATION_ITEM('')
);
#1021=(
BOUNDED_CURVE()
B_SPLINE_CURVE(2,(#61472,#61473,#61474),.UNSPECIFIED.,.F.,.F.)
B_SPLINE_CURVE_WITH_KNOTS((3,3),(0.367644516946552,0.373830527582527),
 .UNSPECIFIED.)
CURVE()
GEOMETRIC_REPRESENTATION_ITEM()
RATIONAL_B_SPLINE_CURVE((1.13426390111308,1.13389822901301,1.13348223894567))
REPRESENTATION_ITEM('')
);
#1022=(
BOUNDED_CURVE()
B_SPLINE_CURVE(2,(#61478,#61479,#61480),.UNSPECIFIED.,.F.,.F.)
B_SPLINE_CURVE_WITH_KNOTS((3,3),(0.271548216895913,0.277734227531896),
 .UNSPECIFIED.)
CURVE()
GEOMETRIC_REPRESENTATION_ITEM()
RATIONAL_B_SPLINE_CURVE((1.13348223894609,1.13389822901344,1.13426390111351))
REPRESENTATION_ITEM('')
);
#1023=(
BOUNDED_CURVE()
B_SPLINE_CURVE(2,(#61484,#61485,#61486),.UNSPECIFIED.,.F.,.F.)
B_SPLINE_CURVE_WITH_KNOTS((3,3),(0.367644516946554,0.373830527582527),
 .UNSPECIFIED.)
CURVE()
GEOMETRIC_REPRESENTATION_ITEM()
RATIONAL_B_SPLINE_CURVE((1.13426390111307,1.13389822901301,1.13348223894566))
REPRESENTATION_ITEM('')
);
#1024=(
BOUNDED_CURVE()
B_SPLINE_CURVE(2,(#61490,#61491,#61492),.UNSPECIFIED.,.F.,.F.)
B_SPLINE_CURVE_WITH_KNOTS((3,3),(0.271548216895912,0.277734227531901),
 .UNSPECIFIED.)
CURVE()
GEOMETRIC_REPRESENTATION_ITEM()
RATIONAL_B_SPLINE_CURVE((1.13348223894619,1.13389822901354,1.13426390111361))
REPRESENTATION_ITEM('')
);
#1025=(
BOUNDED_CURVE()
B_SPLINE_CURVE(2,(#61496,#61497,#61498),.UNSPECIFIED.,.F.,.F.)
B_SPLINE_CURVE_WITH_KNOTS((3,3),(0.367644516946552,0.373830527582526),
 .UNSPECIFIED.)
CURVE()
GEOMETRIC_REPRESENTATION_ITEM()
RATIONAL_B_SPLINE_CURVE((1.13426390111306,1.13389822901299,1.13348223894565))
REPRESENTATION_ITEM('')
);
#1026=(
BOUNDED_CURVE()
B_SPLINE_CURVE(2,(#61502,#61503,#61504),.UNSPECIFIED.,.F.,.F.)
B_SPLINE_CURVE_WITH_KNOTS((3,3),(0.271548216895908,0.277734227531896),
 .UNSPECIFIED.)
CURVE()
GEOMETRIC_REPRESENTATION_ITEM()
RATIONAL_B_SPLINE_CURVE((1.13348223894609,1.13389822901344,1.13426390111351))
REPRESENTATION_ITEM('')
);
#1027=(
BOUNDED_CURVE()
B_SPLINE_CURVE(2,(#61508,#61509,#61510),.UNSPECIFIED.,.F.,.F.)
B_SPLINE_CURVE_WITH_KNOTS((3,3),(0.367644516946558,0.373830527582532),
 .UNSPECIFIED.)
CURVE()
GEOMETRIC_REPRESENTATION_ITEM()
RATIONAL_B_SPLINE_CURVE((1.13426390111305,1.13389822901298,1.13348223894564))
REPRESENTATION_ITEM('')
);
#1028=(
BOUNDED_CURVE()
B_SPLINE_CURVE(2,(#61514,#61515,#61516),.UNSPECIFIED.,.F.,.F.)
B_SPLINE_CURVE_WITH_KNOTS((3,3),(0.271548216895918,0.27773422753191),
 .UNSPECIFIED.)
CURVE()
GEOMETRIC_REPRESENTATION_ITEM()
RATIONAL_B_SPLINE_CURVE((1.1334822389462,1.13389822901355,1.13426390111362))
REPRESENTATION_ITEM('')
);
#1029=(
BOUNDED_CURVE()
B_SPLINE_CURVE(2,(#61520,#61521,#61522),.UNSPECIFIED.,.F.,.F.)
B_SPLINE_CURVE_WITH_KNOTS((3,3),(0.367644516946559,0.373830527582532),
 .UNSPECIFIED.)
CURVE()
GEOMETRIC_REPRESENTATION_ITEM()
RATIONAL_B_SPLINE_CURVE((1.13426390111305,1.13389822901299,1.13348223894564))
REPRESENTATION_ITEM('')
);
#1030=(
BOUNDED_CURVE()
B_SPLINE_CURVE(2,(#61526,#61527,#61528),.UNSPECIFIED.,.F.,.F.)
B_SPLINE_CURVE_WITH_KNOTS((3,3),(0.271548216895917,0.277734227531899),
 .UNSPECIFIED.)
CURVE()
GEOMETRIC_REPRESENTATION_ITEM()
RATIONAL_B_SPLINE_CURVE((1.13348223894612,1.13389822901347,1.13426390111355))
REPRESENTATION_ITEM('')
);
#1031=(
BOUNDED_CURVE()
B_SPLINE_CURVE(2,(#61532,#61533,#61534),.UNSPECIFIED.,.F.,.F.)
B_SPLINE_CURVE_WITH_KNOTS((3,3),(0.367644516946562,0.373830527582533),
 .UNSPECIFIED.)
CURVE()
GEOMETRIC_REPRESENTATION_ITEM()
RATIONAL_B_SPLINE_CURVE((1.13426390111306,1.13389822901299,1.13348223894564))
REPRESENTATION_ITEM('')
);
#1032=(
BOUNDED_CURVE()
B_SPLINE_CURVE(2,(#61538,#61539,#61540),.UNSPECIFIED.,.F.,.F.)
B_SPLINE_CURVE_WITH_KNOTS((3,3),(0.271548216895905,0.277734227531891),
 .UNSPECIFIED.)
CURVE()
GEOMETRIC_REPRESENTATION_ITEM()
RATIONAL_B_SPLINE_CURVE((1.13348223894609,1.13389822901344,1.13426390111351))
REPRESENTATION_ITEM('')
);
#1033=(
BOUNDED_CURVE()
B_SPLINE_CURVE(2,(#61544,#61545,#61546),.UNSPECIFIED.,.F.,.F.)
B_SPLINE_CURVE_WITH_KNOTS((3,3),(0.367644516946557,0.373830527582533),
 .UNSPECIFIED.)
CURVE()
GEOMETRIC_REPRESENTATION_ITEM()
RATIONAL_B_SPLINE_CURVE((1.13426390111305,1.13389822901299,1.13348223894564))
REPRESENTATION_ITEM('')
);
#1034=(
BOUNDED_CURVE()
B_SPLINE_CURVE(2,(#61550,#61551,#61552),.UNSPECIFIED.,.F.,.F.)
B_SPLINE_CURVE_WITH_KNOTS((3,3),(0.271548216895918,0.277734227531906),
 .UNSPECIFIED.)
CURVE()
GEOMETRIC_REPRESENTATION_ITEM()
RATIONAL_B_SPLINE_CURVE((1.13348223894616,1.13389822901351,1.13426390111358))
REPRESENTATION_ITEM('')
);
#1035=(
BOUNDED_CURVE()
B_SPLINE_CURVE(2,(#61574,#61575,#61576),.UNSPECIFIED.,.F.,.F.)
B_SPLINE_CURVE_WITH_KNOTS((3,3),(0.376641898803529,0.382940702095941),
 .UNSPECIFIED.)
CURVE()
GEOMETRIC_REPRESENTATION_ITEM()
RATIONAL_B_SPLINE_CURVE((1.12071541658433,1.1202411994692,1.11971735964528))
REPRESENTATION_ITEM('')
);
#1036=(
BOUNDED_CURVE()
B_SPLINE_CURVE(2,(#61580,#61581,#61582),.UNSPECIFIED.,.F.,.F.)
B_SPLINE_CURVE_WITH_KNOTS((3,3),(0.249954652430657,0.25625345571807),
 .UNSPECIFIED.)
CURVE()
GEOMETRIC_REPRESENTATION_ITEM()
RATIONAL_B_SPLINE_CURVE((1.1197173596462,1.12024119946966,1.12071541658442))
REPRESENTATION_ITEM('')
);
#1037=(
BOUNDED_CURVE()
B_SPLINE_CURVE(2,(#61586,#61587,#61588),.UNSPECIFIED.,.F.,.F.)
B_SPLINE_CURVE_WITH_KNOTS((3,3),(0.376641898803524,0.382940702095934),
 .UNSPECIFIED.)
CURVE()
GEOMETRIC_REPRESENTATION_ITEM()
RATIONAL_B_SPLINE_CURVE((1.12071541658448,1.12024119946934,1.11971735964542))
REPRESENTATION_ITEM('')
);
#1038=(
BOUNDED_CURVE()
B_SPLINE_CURVE(2,(#61592,#61593,#61594),.UNSPECIFIED.,.F.,.F.)
B_SPLINE_CURVE_WITH_KNOTS((3,3),(0.249954652430655,0.256253455718069),
 .UNSPECIFIED.)
CURVE()
GEOMETRIC_REPRESENTATION_ITEM()
RATIONAL_B_SPLINE_CURVE((1.11971735964613,1.1202411994696,1.12071541658435))
REPRESENTATION_ITEM('')
);
#1039=(
BOUNDED_CURVE()
B_SPLINE_CURVE(2,(#61598,#61599,#61600),.UNSPECIFIED.,.F.,.F.)
B_SPLINE_CURVE_WITH_KNOTS((3,3),(0.376641898803532,0.382940702095944),
 .UNSPECIFIED.)
CURVE()
GEOMETRIC_REPRESENTATION_ITEM()
RATIONAL_B_SPLINE_CURVE((1.12071541658434,1.12024119946921,1.11971735964529))
REPRESENTATION_ITEM('')
);
#1040=(
BOUNDED_CURVE()
B_SPLINE_CURVE(2,(#61604,#61605,#61606),.UNSPECIFIED.,.F.,.F.)
B_SPLINE_CURVE_WITH_KNOTS((3,3),(0.249954652430645,0.256253455718059),
 .UNSPECIFIED.)
CURVE()
GEOMETRIC_REPRESENTATION_ITEM()
RATIONAL_B_SPLINE_CURVE((1.11971735964598,1.12024119946945,1.1207154165842))
REPRESENTATION_ITEM('')
);
#1041=(
BOUNDED_CURVE()
B_SPLINE_CURVE(2,(#61610,#61611,#61612),.UNSPECIFIED.,.F.,.F.)
B_SPLINE_CURVE_WITH_KNOTS((3,3),(0.376641898803521,0.382940702095933),
 .UNSPECIFIED.)
CURVE()
GEOMETRIC_REPRESENTATION_ITEM()
RATIONAL_B_SPLINE_CURVE((1.1207154165845,1.12024119946936,1.11971735964544))
REPRESENTATION_ITEM('')
);
#1042=(
BOUNDED_CURVE()
B_SPLINE_CURVE(2,(#61616,#61617,#61618),.UNSPECIFIED.,.F.,.F.)
B_SPLINE_CURVE_WITH_KNOTS((3,3),(0.249954652430661,0.256253455718076),
 .UNSPECIFIED.)
CURVE()
GEOMETRIC_REPRESENTATION_ITEM()
RATIONAL_B_SPLINE_CURVE((1.1197173596463,1.12024119946977,1.12071541658453))
REPRESENTATION_ITEM('')
);
#1043=(
BOUNDED_CURVE()
B_SPLINE_CURVE(2,(#61622,#61623,#61624),.UNSPECIFIED.,.F.,.F.)
B_SPLINE_CURVE_WITH_KNOTS((3,3),(0.376641898803535,0.382940702095943),
 .UNSPECIFIED.)
CURVE()
GEOMETRIC_REPRESENTATION_ITEM()
RATIONAL_B_SPLINE_CURVE((1.12071541658437,1.12024119946923,1.11971735964532))
REPRESENTATION_ITEM('')
);
#1044=(
BOUNDED_CURVE()
B_SPLINE_CURVE(2,(#61628,#61629,#61630),.UNSPECIFIED.,.F.,.F.)
B_SPLINE_CURVE_WITH_KNOTS((3,3),(0.249954652430645,0.256253455718058),
 .UNSPECIFIED.)
CURVE()
GEOMETRIC_REPRESENTATION_ITEM()
RATIONAL_B_SPLINE_CURVE((1.11971735964609,1.12024119946955,1.12071541658431))
REPRESENTATION_ITEM('')
);
#1045=(
BOUNDED_CURVE()
B_SPLINE_CURVE(2,(#61634,#61635,#61636),.UNSPECIFIED.,.F.,.F.)
B_SPLINE_CURVE_WITH_KNOTS((3,3),(0.376641898803531,0.382940702095942),
 .UNSPECIFIED.)
CURVE()
GEOMETRIC_REPRESENTATION_ITEM()
RATIONAL_B_SPLINE_CURVE((1.12071541658437,1.12024119946923,1.11971735964532))
REPRESENTATION_ITEM('')
);
#1046=(
BOUNDED_CURVE()
B_SPLINE_CURVE(2,(#61640,#61641,#61642),.UNSPECIFIED.,.F.,.F.)
B_SPLINE_CURVE_WITH_KNOTS((3,3),(0.249954652430646,0.256253455718059),
 .UNSPECIFIED.)
CURVE()
GEOMETRIC_REPRESENTATION_ITEM()
RATIONAL_B_SPLINE_CURVE((1.11971735964605,1.12024119946951,1.12071541658427))
REPRESENTATION_ITEM('')
);
#1047=(
BOUNDED_CURVE()
B_SPLINE_CURVE(2,(#61646,#61647,#61648),.UNSPECIFIED.,.F.,.F.)
B_SPLINE_CURVE_WITH_KNOTS((3,3),(0.376641898803521,0.382940702095931),
 .UNSPECIFIED.)
CURVE()
GEOMETRIC_REPRESENTATION_ITEM()
RATIONAL_B_SPLINE_CURVE((1.12071541658451,1.12024119946938,1.11971735964546))
REPRESENTATION_ITEM('')
);
#1048=(
BOUNDED_CURVE()
B_SPLINE_CURVE(2,(#61652,#61653,#61654),.UNSPECIFIED.,.F.,.F.)
B_SPLINE_CURVE_WITH_KNOTS((3,3),(0.249954652430639,0.256253455718052),
 .UNSPECIFIED.)
CURVE()
GEOMETRIC_REPRESENTATION_ITEM()
RATIONAL_B_SPLINE_CURVE((1.11971735964601,1.12024119946948,1.12071541658424))
REPRESENTATION_ITEM('')
);
#1049=(
BOUNDED_CURVE()
B_SPLINE_CURVE(2,(#61658,#61659,#61660),.UNSPECIFIED.,.F.,.F.)
B_SPLINE_CURVE_WITH_KNOTS((3,3),(0.376641898803533,0.382940702095945),
 .UNSPECIFIED.)
CURVE()
GEOMETRIC_REPRESENTATION_ITEM()
RATIONAL_B_SPLINE_CURVE((1.12071541658434,1.1202411994692,1.11971735964528))
REPRESENTATION_ITEM('')
);
#1050=(
BOUNDED_CURVE()
B_SPLINE_CURVE(2,(#61664,#61665,#61666),.UNSPECIFIED.,.F.,.F.)
B_SPLINE_CURVE_WITH_KNOTS((3,3),(0.249954652430659,0.256253455718072),
 .UNSPECIFIED.)
CURVE()
GEOMETRIC_REPRESENTATION_ITEM()
RATIONAL_B_SPLINE_CURVE((1.11971735964624,1.12024119946971,1.12071541658447))
REPRESENTATION_ITEM('')
);
#1051=(
BOUNDED_CURVE()
B_SPLINE_CURVE(2,(#61670,#61671,#61672),.UNSPECIFIED.,.F.,.F.)
B_SPLINE_CURVE_WITH_KNOTS((3,3),(0.376641898803529,0.382940702095948),
 .UNSPECIFIED.)
CURVE()
GEOMETRIC_REPRESENTATION_ITEM()
RATIONAL_B_SPLINE_CURVE((1.12071541658446,1.12024119946932,1.1197173596454))
REPRESENTATION_ITEM('')
);
#1052=(
BOUNDED_CURVE()
B_SPLINE_CURVE(2,(#61676,#61677,#61678),.UNSPECIFIED.,.F.,.F.)
B_SPLINE_CURVE_WITH_KNOTS((3,3),(0.249954652430643,0.256253455718057),
 .UNSPECIFIED.)
CURVE()
GEOMETRIC_REPRESENTATION_ITEM()
RATIONAL_B_SPLINE_CURVE((1.11971735964609,1.12024119946956,1.12071541658432))
REPRESENTATION_ITEM('')
);
#1053=(
BOUNDED_CURVE()
B_SPLINE_CURVE(2,(#61682,#61683,#61684),.UNSPECIFIED.,.F.,.F.)
B_SPLINE_CURVE_WITH_KNOTS((3,3),(0.376641898803523,0.382940702095941),
 .UNSPECIFIED.)
CURVE()
GEOMETRIC_REPRESENTATION_ITEM()
RATIONAL_B_SPLINE_CURVE((1.12071541658451,1.12024119946937,1.11971735964545))
REPRESENTATION_ITEM('')
);
#1054=(
BOUNDED_CURVE()
B_SPLINE_CURVE(2,(#61688,#61689,#61690),.UNSPECIFIED.,.F.,.F.)
B_SPLINE_CURVE_WITH_KNOTS((3,3),(0.249954652430644,0.256253455718058),
 .UNSPECIFIED.)
CURVE()
GEOMETRIC_REPRESENTATION_ITEM()
RATIONAL_B_SPLINE_CURVE((1.11971735964615,1.12024119946961,1.12071541658437))
REPRESENTATION_ITEM('')
);
#1055=(
BOUNDED_CURVE()
B_SPLINE_CURVE(2,(#61694,#61695,#61696),.UNSPECIFIED.,.F.,.F.)
B_SPLINE_CURVE_WITH_KNOTS((3,3),(0.376641898803536,0.382940702095946),
 .UNSPECIFIED.)
CURVE()
GEOMETRIC_REPRESENTATION_ITEM()
RATIONAL_B_SPLINE_CURVE((1.12071541658451,1.12024119946938,1.11971735964546))
REPRESENTATION_ITEM('')
);
#1056=(
BOUNDED_CURVE()
B_SPLINE_CURVE(2,(#61700,#61701,#61702),.UNSPECIFIED.,.F.,.F.)
B_SPLINE_CURVE_WITH_KNOTS((3,3),(0.24995465243065,0.256253455718062),
 .UNSPECIFIED.)
CURVE()
GEOMETRIC_REPRESENTATION_ITEM()
RATIONAL_B_SPLINE_CURVE((1.11971735964599,1.12024119946946,1.12071541658421))
REPRESENTATION_ITEM('')
);
#1057=(
BOUNDED_CURVE()
B_SPLINE_CURVE(2,(#61706,#61707,#61708),.UNSPECIFIED.,.F.,.F.)
B_SPLINE_CURVE_WITH_KNOTS((3,3),(0.376641898803523,0.38294070209593),
 .UNSPECIFIED.)
CURVE()
GEOMETRIC_REPRESENTATION_ITEM()
RATIONAL_B_SPLINE_CURVE((1.1207154165845,1.12024119946936,1.11971735964544))
REPRESENTATION_ITEM('')
);
#1058=(
BOUNDED_CURVE()
B_SPLINE_CURVE(2,(#61712,#61713,#61714),.UNSPECIFIED.,.F.,.F.)
B_SPLINE_CURVE_WITH_KNOTS((3,3),(0.249954652430653,0.256253455718064),
 .UNSPECIFIED.)
CURVE()
GEOMETRIC_REPRESENTATION_ITEM()
RATIONAL_B_SPLINE_CURVE((1.11971735964611,1.12024119946957,1.12071541658433))
REPRESENTATION_ITEM('')
);
#1059=(
BOUNDED_CURVE()
B_SPLINE_CURVE(2,(#61718,#61719,#61720),.UNSPECIFIED.,.F.,.F.)
B_SPLINE_CURVE_WITH_KNOTS((3,3),(0.376641898803521,0.382940702095931),
 .UNSPECIFIED.)
CURVE()
GEOMETRIC_REPRESENTATION_ITEM()
RATIONAL_B_SPLINE_CURVE((1.12071541658461,1.12024119946947,1.11971735964555))
REPRESENTATION_ITEM('')
);
#1060=(
BOUNDED_CURVE()
B_SPLINE_CURVE(2,(#61724,#61725,#61726),.UNSPECIFIED.,.F.,.F.)
B_SPLINE_CURVE_WITH_KNOTS((3,3),(0.249954652430661,0.256253455718072),
 .UNSPECIFIED.)
CURVE()
GEOMETRIC_REPRESENTATION_ITEM()
RATIONAL_B_SPLINE_CURVE((1.11971735964623,1.1202411994697,1.12071541658446))
REPRESENTATION_ITEM('')
);
#1061=(
BOUNDED_CURVE()
B_SPLINE_CURVE(2,(#61730,#61731,#61732),.UNSPECIFIED.,.F.,.F.)
B_SPLINE_CURVE_WITH_KNOTS((3,3),(0.376641898803537,0.382940702095947),
 .UNSPECIFIED.)
CURVE()
GEOMETRIC_REPRESENTATION_ITEM()
RATIONAL_B_SPLINE_CURVE((1.1207154165845,1.12024119946936,1.11971735964544))
REPRESENTATION_ITEM('')
);
#1062=(
BOUNDED_CURVE()
B_SPLINE_CURVE(2,(#61736,#61737,#61738),.UNSPECIFIED.,.F.,.F.)
B_SPLINE_CURVE_WITH_KNOTS((3,3),(0.249954652430645,0.256253455718056),
 .UNSPECIFIED.)
CURVE()
GEOMETRIC_REPRESENTATION_ITEM()
RATIONAL_B_SPLINE_CURVE((1.11971735964613,1.1202411994696,1.12071541658435))
REPRESENTATION_ITEM('')
);
#1063=(
BOUNDED_CURVE()
B_SPLINE_CURVE(2,(#61742,#61743,#61744),.UNSPECIFIED.,.F.,.F.)
B_SPLINE_CURVE_WITH_KNOTS((3,3),(0.376641898803536,0.382940702095954),
 .UNSPECIFIED.)
CURVE()
GEOMETRIC_REPRESENTATION_ITEM()
RATIONAL_B_SPLINE_CURVE((1.12071541658435,1.12024119946922,1.1197173596453))
REPRESENTATION_ITEM('')
);
#1064=(
BOUNDED_CURVE()
B_SPLINE_CURVE(2,(#61748,#61749,#61750),.UNSPECIFIED.,.F.,.F.)
B_SPLINE_CURVE_WITH_KNOTS((3,3),(0.249954652430663,0.256253455718072),
 .UNSPECIFIED.)
CURVE()
GEOMETRIC_REPRESENTATION_ITEM()
RATIONAL_B_SPLINE_CURVE((1.11971735964633,1.1202411994698,1.12071541658456))
REPRESENTATION_ITEM('')
);
#1065=(
BOUNDED_CURVE()
B_SPLINE_CURVE(2,(#61754,#61755,#61756),.UNSPECIFIED.,.F.,.F.)
B_SPLINE_CURVE_WITH_KNOTS((3,3),(0.376641898803512,0.382940702095922),
 .UNSPECIFIED.)
CURVE()
GEOMETRIC_REPRESENTATION_ITEM()
RATIONAL_B_SPLINE_CURVE((1.12071541658461,1.12024119946947,1.11971735964555))
REPRESENTATION_ITEM('')
);
#1066=(
BOUNDED_CURVE()
B_SPLINE_CURVE(2,(#61760,#61761,#61762),.UNSPECIFIED.,.F.,.F.)
B_SPLINE_CURVE_WITH_KNOTS((3,3),(0.249954652430648,0.256253455718062),
 .UNSPECIFIED.)
CURVE()
GEOMETRIC_REPRESENTATION_ITEM()
RATIONAL_B_SPLINE_CURVE((1.11971735964605,1.12024119946951,1.12071541658427))
REPRESENTATION_ITEM('')
);
#1067=(
BOUNDED_CURVE()
B_SPLINE_CURVE(2,(#61766,#61767,#61768),.UNSPECIFIED.,.F.,.F.)
B_SPLINE_CURVE_WITH_KNOTS((3,3),(0.376641898803527,0.382940702095944),
 .UNSPECIFIED.)
CURVE()
GEOMETRIC_REPRESENTATION_ITEM()
RATIONAL_B_SPLINE_CURVE((1.12071541658444,1.12024119946931,1.11971735964539))
REPRESENTATION_ITEM('')
);
#1068=(
BOUNDED_CURVE()
B_SPLINE_CURVE(2,(#61772,#61773,#61774),.UNSPECIFIED.,.F.,.F.)
B_SPLINE_CURVE_WITH_KNOTS((3,3),(0.24995465243065,0.256253455718066),
 .UNSPECIFIED.)
CURVE()
GEOMETRIC_REPRESENTATION_ITEM()
RATIONAL_B_SPLINE_CURVE((1.11971735964612,1.12024119946958,1.12071541658434))
REPRESENTATION_ITEM('')
);
#1069=(
BOUNDED_CURVE()
B_SPLINE_CURVE(2,(#61778,#61779,#61780),.UNSPECIFIED.,.F.,.F.)
B_SPLINE_CURVE_WITH_KNOTS((3,3),(0.37664189880352,0.382940702095936),
 .UNSPECIFIED.)
CURVE()
GEOMETRIC_REPRESENTATION_ITEM()
RATIONAL_B_SPLINE_CURVE((1.12071541658452,1.12024119946938,1.11971735964546))
REPRESENTATION_ITEM('')
);
#1070=(
BOUNDED_CURVE()
B_SPLINE_CURVE(2,(#61784,#61785,#61786),.UNSPECIFIED.,.F.,.F.)
B_SPLINE_CURVE_WITH_KNOTS((3,3),(0.249954652430664,0.25625345571808),
 .UNSPECIFIED.)
CURVE()
GEOMETRIC_REPRESENTATION_ITEM()
RATIONAL_B_SPLINE_CURVE((1.11971735964628,1.12024119946975,1.12071541658451))
REPRESENTATION_ITEM('')
);
#1071=(
BOUNDED_CURVE()
B_SPLINE_CURVE(2,(#61790,#61791,#61792),.UNSPECIFIED.,.F.,.F.)
B_SPLINE_CURVE_WITH_KNOTS((3,3),(0.376641898803518,0.382940702095937),
 .UNSPECIFIED.)
CURVE()
GEOMETRIC_REPRESENTATION_ITEM()
RATIONAL_B_SPLINE_CURVE((1.12071541658454,1.12024119946941,1.11971735964549))
REPRESENTATION_ITEM('')
);
#1072=(
BOUNDED_CURVE()
B_SPLINE_CURVE(2,(#61796,#61797,#61798),.UNSPECIFIED.,.F.,.F.)
B_SPLINE_CURVE_WITH_KNOTS((3,3),(0.249954652430639,0.256253455718056),
 .UNSPECIFIED.)
CURVE()
GEOMETRIC_REPRESENTATION_ITEM()
RATIONAL_B_SPLINE_CURVE((1.11971735964609,1.12024119946956,1.12071541658432))
REPRESENTATION_ITEM('')
);
#1073=(
BOUNDED_CURVE()
B_SPLINE_CURVE(2,(#61802,#61803,#61804),.UNSPECIFIED.,.F.,.F.)
B_SPLINE_CURVE_WITH_KNOTS((3,3),(0.376641898803522,0.382940702095936),
 .UNSPECIFIED.)
CURVE()
GEOMETRIC_REPRESENTATION_ITEM()
RATIONAL_B_SPLINE_CURVE((1.12071541658447,1.12024119946934,1.11971735964542))
REPRESENTATION_ITEM('')
);
#1074=(
BOUNDED_CURVE()
B_SPLINE_CURVE(2,(#61808,#61809,#61810),.UNSPECIFIED.,.F.,.F.)
B_SPLINE_CURVE_WITH_KNOTS((3,3),(0.249954652430657,0.256253455718066),
 .UNSPECIFIED.)
CURVE()
GEOMETRIC_REPRESENTATION_ITEM()
RATIONAL_B_SPLINE_CURVE((1.11971735964622,1.12024119946968,1.12071541658444))
REPRESENTATION_ITEM('')
);
#1075=(
BOUNDED_CURVE()
B_SPLINE_CURVE(2,(#61814,#61815,#61816),.UNSPECIFIED.,.F.,.F.)
B_SPLINE_CURVE_WITH_KNOTS((3,3),(0.376641898803533,0.38294070209594),
 .UNSPECIFIED.)
CURVE()
GEOMETRIC_REPRESENTATION_ITEM()
RATIONAL_B_SPLINE_CURVE((1.12071541658433,1.1202411994692,1.11971735964528))
REPRESENTATION_ITEM('')
);
#1076=(
BOUNDED_CURVE()
B_SPLINE_CURVE(2,(#61820,#61821,#61822),.UNSPECIFIED.,.F.,.F.)
B_SPLINE_CURVE_WITH_KNOTS((3,3),(0.249954652430642,0.256253455718055),
 .UNSPECIFIED.)
CURVE()
GEOMETRIC_REPRESENTATION_ITEM()
RATIONAL_B_SPLINE_CURVE((1.11971735964602,1.12024119946948,1.12071541658424))
REPRESENTATION_ITEM('')
);
#1077=(
BOUNDED_CURVE()
B_SPLINE_CURVE(2,(#61826,#61827,#61828),.UNSPECIFIED.,.F.,.F.)
B_SPLINE_CURVE_WITH_KNOTS((3,3),(0.376641898803547,0.382940702095962),
 .UNSPECIFIED.)
CURVE()
GEOMETRIC_REPRESENTATION_ITEM()
RATIONAL_B_SPLINE_CURVE((1.12071541658418,1.12024119946904,1.11971735964512))
REPRESENTATION_ITEM('')
);
#1078=(
BOUNDED_CURVE()
B_SPLINE_CURVE(2,(#61832,#61833,#61834),.UNSPECIFIED.,.F.,.F.)
B_SPLINE_CURVE_WITH_KNOTS((3,3),(0.249954652430658,0.256253455718078),
 .UNSPECIFIED.)
CURVE()
GEOMETRIC_REPRESENTATION_ITEM()
RATIONAL_B_SPLINE_CURVE((1.1197173596463,1.12024119946977,1.12071541658453))
REPRESENTATION_ITEM('')
);
#1079=(
BOUNDED_CURVE()
B_SPLINE_CURVE(2,(#61838,#61839,#61840),.UNSPECIFIED.,.F.,.F.)
B_SPLINE_CURVE_WITH_KNOTS((3,3),(0.376641898803522,0.382940702095938),
 .UNSPECIFIED.)
CURVE()
GEOMETRIC_REPRESENTATION_ITEM()
RATIONAL_B_SPLINE_CURVE((1.12071541658451,1.12024119946937,1.11971735964545))
REPRESENTATION_ITEM('')
);
#1080=(
BOUNDED_CURVE()
B_SPLINE_CURVE(2,(#61844,#61845,#61846),.UNSPECIFIED.,.F.,.F.)
B_SPLINE_CURVE_WITH_KNOTS((3,3),(0.249954652430655,0.25625345571807),
 .UNSPECIFIED.)
CURVE()
GEOMETRIC_REPRESENTATION_ITEM()
RATIONAL_B_SPLINE_CURVE((1.11971735964625,1.12024119946971,1.12071541658447))
REPRESENTATION_ITEM('')
);
#1081=(
BOUNDED_CURVE()
B_SPLINE_CURVE(2,(#61850,#61851,#61852),.UNSPECIFIED.,.F.,.F.)
B_SPLINE_CURVE_WITH_KNOTS((3,3),(0.376641898803531,0.382940702095945),
 .UNSPECIFIED.)
CURVE()
GEOMETRIC_REPRESENTATION_ITEM()
RATIONAL_B_SPLINE_CURVE((1.12071541658432,1.12024119946919,1.11971735964527))
REPRESENTATION_ITEM('')
);
#1082=(
BOUNDED_CURVE()
B_SPLINE_CURVE(2,(#61856,#61857,#61858),.UNSPECIFIED.,.F.,.F.)
B_SPLINE_CURVE_WITH_KNOTS((3,3),(0.249954652430637,0.256253455718055),
 .UNSPECIFIED.)
CURVE()
GEOMETRIC_REPRESENTATION_ITEM()
RATIONAL_B_SPLINE_CURVE((1.11971735964599,1.12024119946945,1.12071541658421))
REPRESENTATION_ITEM('')
);
#1083=(
BOUNDED_CURVE()
B_SPLINE_CURVE(2,(#61862,#61863,#61864),.UNSPECIFIED.,.F.,.F.)
B_SPLINE_CURVE_WITH_KNOTS((3,3),(0.376641898803544,0.382940702095957),
 .UNSPECIFIED.)
CURVE()
GEOMETRIC_REPRESENTATION_ITEM()
RATIONAL_B_SPLINE_CURVE((1.12071541658422,1.12024119946908,1.11971735964516))
REPRESENTATION_ITEM('')
);
#1084=(
BOUNDED_CURVE()
B_SPLINE_CURVE(2,(#61868,#61869,#61870),.UNSPECIFIED.,.F.,.F.)
B_SPLINE_CURVE_WITH_KNOTS((3,3),(0.249954652430653,0.256253455718062),
 .UNSPECIFIED.)
CURVE()
GEOMETRIC_REPRESENTATION_ITEM()
RATIONAL_B_SPLINE_CURVE((1.11971735964616,1.12024119946962,1.12071541658438))
REPRESENTATION_ITEM('')
);
#1085=(
BOUNDED_CURVE()
B_SPLINE_CURVE(2,(#61874,#61875,#61876),.UNSPECIFIED.,.F.,.F.)
B_SPLINE_CURVE_WITH_KNOTS((3,3),(0.376641898803539,0.38294070209595),
 .UNSPECIFIED.)
CURVE()
GEOMETRIC_REPRESENTATION_ITEM()
RATIONAL_B_SPLINE_CURVE((1.12071541658449,1.12024119946935,1.11971735964543))
REPRESENTATION_ITEM('')
);
#1086=(
BOUNDED_CURVE()
B_SPLINE_CURVE(2,(#61880,#61881,#61882),.UNSPECIFIED.,.F.,.F.)
B_SPLINE_CURVE_WITH_KNOTS((3,3),(0.249954652430653,0.256253455718071),
 .UNSPECIFIED.)
CURVE()
GEOMETRIC_REPRESENTATION_ITEM()
RATIONAL_B_SPLINE_CURVE((1.11971735964627,1.12024119946973,1.12071541658449))
REPRESENTATION_ITEM('')
);
#1087=(
BOUNDED_CURVE()
B_SPLINE_CURVE(2,(#61886,#61887,#61888),.UNSPECIFIED.,.F.,.F.)
B_SPLINE_CURVE_WITH_KNOTS((3,3),(0.376641898803533,0.382940702095944),
 .UNSPECIFIED.)
CURVE()
GEOMETRIC_REPRESENTATION_ITEM()
RATIONAL_B_SPLINE_CURVE((1.12071541658435,1.12024119946922,1.1197173596453))
REPRESENTATION_ITEM('')
);
#1088=(
BOUNDED_CURVE()
B_SPLINE_CURVE(2,(#61892,#61893,#61894),.UNSPECIFIED.,.F.,.F.)
B_SPLINE_CURVE_WITH_KNOTS((3,3),(0.249954652430647,0.256253455718059),
 .UNSPECIFIED.)
CURVE()
GEOMETRIC_REPRESENTATION_ITEM()
RATIONAL_B_SPLINE_CURVE((1.11971735964614,1.12024119946961,1.12071541658437))
REPRESENTATION_ITEM('')
);
#1089=(
BOUNDED_CURVE()
B_SPLINE_CURVE(2,(#61898,#61899,#61900),.UNSPECIFIED.,.F.,.F.)
B_SPLINE_CURVE_WITH_KNOTS((3,3),(0.376641898803539,0.382940702095955),
 .UNSPECIFIED.)
CURVE()
GEOMETRIC_REPRESENTATION_ITEM()
RATIONAL_B_SPLINE_CURVE((1.12071541658434,1.1202411994692,1.11971735964528))
REPRESENTATION_ITEM('')
);
#1090=(
BOUNDED_CURVE()
B_SPLINE_CURVE(2,(#61904,#61905,#61906),.UNSPECIFIED.,.F.,.F.)
B_SPLINE_CURVE_WITH_KNOTS((3,3),(0.249954652430656,0.256253455718067),
 .UNSPECIFIED.)
CURVE()
GEOMETRIC_REPRESENTATION_ITEM()
RATIONAL_B_SPLINE_CURVE((1.11971735964622,1.12024119946969,1.12071541658444))
REPRESENTATION_ITEM('')
);
#1091=(
BOUNDED_CURVE()
B_SPLINE_CURVE(2,(#61910,#61911,#61912),.UNSPECIFIED.,.F.,.F.)
B_SPLINE_CURVE_WITH_KNOTS((3,3),(0.376641898803524,0.382940702095936),
 .UNSPECIFIED.)
CURVE()
GEOMETRIC_REPRESENTATION_ITEM()
RATIONAL_B_SPLINE_CURVE((1.12071541658457,1.12024119946943,1.11971735964551))
REPRESENTATION_ITEM('')
);
#1092=(
BOUNDED_CURVE()
B_SPLINE_CURVE(2,(#61916,#61917,#61918),.UNSPECIFIED.,.F.,.F.)
B_SPLINE_CURVE_WITH_KNOTS((3,3),(0.249954652430651,0.256253455718065),
 .UNSPECIFIED.)
CURVE()
GEOMETRIC_REPRESENTATION_ITEM()
RATIONAL_B_SPLINE_CURVE((1.11971735964615,1.12024119946961,1.12071541658437))
REPRESENTATION_ITEM('')
);
#1093=(
BOUNDED_CURVE()
B_SPLINE_CURVE(2,(#61922,#61923,#61924),.UNSPECIFIED.,.F.,.F.)
B_SPLINE_CURVE_WITH_KNOTS((3,3),(0.376641898803518,0.382940702095931),
 .UNSPECIFIED.)
CURVE()
GEOMETRIC_REPRESENTATION_ITEM()
RATIONAL_B_SPLINE_CURVE((1.12071541658449,1.12024119946936,1.11971735964544))
REPRESENTATION_ITEM('')
);
#1094=(
BOUNDED_CURVE()
B_SPLINE_CURVE(2,(#61928,#61929,#61930),.UNSPECIFIED.,.F.,.F.)
B_SPLINE_CURVE_WITH_KNOTS((3,3),(0.249954652430648,0.256253455718058),
 .UNSPECIFIED.)
CURVE()
GEOMETRIC_REPRESENTATION_ITEM()
RATIONAL_B_SPLINE_CURVE((1.11971735964614,1.1202411994696,1.12071541658436))
REPRESENTATION_ITEM('')
);
#1095=(
BOUNDED_CURVE()
B_SPLINE_CURVE(2,(#61934,#61935,#61936),.UNSPECIFIED.,.F.,.F.)
B_SPLINE_CURVE_WITH_KNOTS((3,3),(0.376641898803531,0.382940702095945),
 .UNSPECIFIED.)
CURVE()
GEOMETRIC_REPRESENTATION_ITEM()
RATIONAL_B_SPLINE_CURVE((1.12071541658451,1.12024119946937,1.11971735964545))
REPRESENTATION_ITEM('')
);
#1096=(
BOUNDED_CURVE()
B_SPLINE_CURVE(2,(#61940,#61941,#61942),.UNSPECIFIED.,.F.,.F.)
B_SPLINE_CURVE_WITH_KNOTS((3,3),(0.249954652430648,0.256253455718067),
 .UNSPECIFIED.)
CURVE()
GEOMETRIC_REPRESENTATION_ITEM()
RATIONAL_B_SPLINE_CURVE((1.11971735964618,1.12024119946964,1.1207154165844))
REPRESENTATION_ITEM('')
);
#1097=(
BOUNDED_CURVE()
B_SPLINE_CURVE(2,(#61946,#61947,#61948),.UNSPECIFIED.,.F.,.F.)
B_SPLINE_CURVE_WITH_KNOTS((3,3),(0.376641898803536,0.382940702095949),
 .UNSPECIFIED.)
CURVE()
GEOMETRIC_REPRESENTATION_ITEM()
RATIONAL_B_SPLINE_CURVE((1.12071541658431,1.12024119946918,1.11971735964526))
REPRESENTATION_ITEM('')
);
#1098=(
BOUNDED_CURVE()
B_SPLINE_CURVE(2,(#61952,#61953,#61954),.UNSPECIFIED.,.F.,.F.)
B_SPLINE_CURVE_WITH_KNOTS((3,3),(0.249954652430665,0.256253455718077),
 .UNSPECIFIED.)
CURVE()
GEOMETRIC_REPRESENTATION_ITEM()
RATIONAL_B_SPLINE_CURVE((1.11971735964631,1.12024119946977,1.12071541658453))
REPRESENTATION_ITEM('')
);
#1099=(
BOUNDED_CURVE()
B_SPLINE_CURVE(2,(#61958,#61959,#61960),.UNSPECIFIED.,.F.,.F.)
B_SPLINE_CURVE_WITH_KNOTS((3,3),(0.376641898803534,0.382940702095945),
 .UNSPECIFIED.)
CURVE()
GEOMETRIC_REPRESENTATION_ITEM()
RATIONAL_B_SPLINE_CURVE((1.12071541658427,1.12024119946914,1.11971735964522))
REPRESENTATION_ITEM('')
);
#1100=(
BOUNDED_CURVE()
B_SPLINE_CURVE(2,(#61964,#61965,#61966),.UNSPECIFIED.,.F.,.F.)
B_SPLINE_CURVE_WITH_KNOTS((3,3),(0.249954652430654,0.256253455718069),
 .UNSPECIFIED.)
CURVE()
GEOMETRIC_REPRESENTATION_ITEM()
RATIONAL_B_SPLINE_CURVE((1.11971735964621,1.12024119946968,1.12071541658444))
REPRESENTATION_ITEM('')
);
#1101=(
BOUNDED_CURVE()
B_SPLINE_CURVE(2,(#61970,#61971,#61972),.UNSPECIFIED.,.F.,.F.)
B_SPLINE_CURVE_WITH_KNOTS((3,3),(0.376641898803532,0.382940702095944),
 .UNSPECIFIED.)
CURVE()
GEOMETRIC_REPRESENTATION_ITEM()
RATIONAL_B_SPLINE_CURVE((1.12071541658432,1.12024119946919,1.11971735964527))
REPRESENTATION_ITEM('')
);
#1102=(
BOUNDED_CURVE()
B_SPLINE_CURVE(2,(#61976,#61977,#61978),.UNSPECIFIED.,.F.,.F.)
B_SPLINE_CURVE_WITH_KNOTS((3,3),(0.249954652430654,0.256253455718072),
 .UNSPECIFIED.)
CURVE()
GEOMETRIC_REPRESENTATION_ITEM()
RATIONAL_B_SPLINE_CURVE((1.11971735964625,1.12024119946971,1.12071541658447))
REPRESENTATION_ITEM('')
);
#1103=(
BOUNDED_CURVE()
B_SPLINE_CURVE(2,(#61982,#61983,#61984),.UNSPECIFIED.,.F.,.F.)
B_SPLINE_CURVE_WITH_KNOTS((3,3),(0.376641898803539,0.382940702095952),
 .UNSPECIFIED.)
CURVE()
GEOMETRIC_REPRESENTATION_ITEM()
RATIONAL_B_SPLINE_CURVE((1.1207154165844,1.12024119946926,1.11971735964534))
REPRESENTATION_ITEM('')
);
#1104=(
BOUNDED_CURVE()
B_SPLINE_CURVE(2,(#61988,#61989,#61990),.UNSPECIFIED.,.F.,.F.)
B_SPLINE_CURVE_WITH_KNOTS((3,3),(0.249954652430648,0.256253455718062),
 .UNSPECIFIED.)
CURVE()
GEOMETRIC_REPRESENTATION_ITEM()
RATIONAL_B_SPLINE_CURVE((1.11971735964618,1.12024119946965,1.12071541658441))
REPRESENTATION_ITEM('')
);
#1105=(
BOUNDED_CURVE()
B_SPLINE_CURVE(2,(#61994,#61995,#61996),.UNSPECIFIED.,.F.,.F.)
B_SPLINE_CURVE_WITH_KNOTS((3,3),(0.376641898803519,0.382940702095932),
 .UNSPECIFIED.)
CURVE()
GEOMETRIC_REPRESENTATION_ITEM()
RATIONAL_B_SPLINE_CURVE((1.12071541658452,1.12024119946938,1.11971735964546))
REPRESENTATION_ITEM('')
);
#1106=(
BOUNDED_CURVE()
B_SPLINE_CURVE(2,(#62000,#62001,#62002),.UNSPECIFIED.,.F.,.F.)
B_SPLINE_CURVE_WITH_KNOTS((3,3),(0.249954652430659,0.256253455718071),
 .UNSPECIFIED.)
CURVE()
GEOMETRIC_REPRESENTATION_ITEM()
RATIONAL_B_SPLINE_CURVE((1.11971735964627,1.12024119946974,1.1207154165845))
REPRESENTATION_ITEM('')
);
#1107=(
BOUNDED_CURVE()
B_SPLINE_CURVE(2,(#62006,#62007,#62008),.UNSPECIFIED.,.F.,.F.)
B_SPLINE_CURVE_WITH_KNOTS((3,3),(0.376641898803527,0.382940702095942),
 .UNSPECIFIED.)
CURVE()
GEOMETRIC_REPRESENTATION_ITEM()
RATIONAL_B_SPLINE_CURVE((1.12071541658453,1.1202411994694,1.11971735964547))
REPRESENTATION_ITEM('')
);
#1108=(
BOUNDED_CURVE()
B_SPLINE_CURVE(2,(#62012,#62013,#62014),.UNSPECIFIED.,.F.,.F.)
B_SPLINE_CURVE_WITH_KNOTS((3,3),(0.249954652430662,0.256253455718075),
 .UNSPECIFIED.)
CURVE()
GEOMETRIC_REPRESENTATION_ITEM()
RATIONAL_B_SPLINE_CURVE((1.11971735964629,1.12024119946976,1.12071541658452))
REPRESENTATION_ITEM('')
);
#1109=(
BOUNDED_CURVE()
B_SPLINE_CURVE(2,(#62018,#62019,#62020),.UNSPECIFIED.,.F.,.F.)
B_SPLINE_CURVE_WITH_KNOTS((3,3),(0.376641898803543,0.382940702095954),
 .UNSPECIFIED.)
CURVE()
GEOMETRIC_REPRESENTATION_ITEM()
RATIONAL_B_SPLINE_CURVE((1.12071541658423,1.1202411994691,1.11971735964518))
REPRESENTATION_ITEM('')
);
#1110=(
BOUNDED_CURVE()
B_SPLINE_CURVE(2,(#62024,#62025,#62026),.UNSPECIFIED.,.F.,.F.)
B_SPLINE_CURVE_WITH_KNOTS((3,3),(0.249954652430648,0.256253455718061),
 .UNSPECIFIED.)
CURVE()
GEOMETRIC_REPRESENTATION_ITEM()
RATIONAL_B_SPLINE_CURVE((1.11971735964609,1.12024119946956,1.12071541658431))
REPRESENTATION_ITEM('')
);
#1111=(
BOUNDED_CURVE()
B_SPLINE_CURVE(2,(#62030,#62031,#62032),.UNSPECIFIED.,.F.,.F.)
B_SPLINE_CURVE_WITH_KNOTS((3,3),(0.376641898803529,0.382940702095943),
 .UNSPECIFIED.)
CURVE()
GEOMETRIC_REPRESENTATION_ITEM()
RATIONAL_B_SPLINE_CURVE((1.12071541658438,1.12024119946925,1.11971735964533))
REPRESENTATION_ITEM('')
);
#1112=(
BOUNDED_CURVE()
B_SPLINE_CURVE(2,(#62036,#62037,#62038),.UNSPECIFIED.,.F.,.F.)
B_SPLINE_CURVE_WITH_KNOTS((3,3),(0.249954652430657,0.256253455718069),
 .UNSPECIFIED.)
CURVE()
GEOMETRIC_REPRESENTATION_ITEM()
RATIONAL_B_SPLINE_CURVE((1.11971735964625,1.12024119946971,1.12071541658447))
REPRESENTATION_ITEM('')
);
#1113=(
BOUNDED_CURVE()
B_SPLINE_CURVE(2,(#62042,#62043,#62044),.UNSPECIFIED.,.F.,.F.)
B_SPLINE_CURVE_WITH_KNOTS((3,3),(0.376641898803529,0.382940702095941),
 .UNSPECIFIED.)
CURVE()
GEOMETRIC_REPRESENTATION_ITEM()
RATIONAL_B_SPLINE_CURVE((1.12071541658439,1.12024119946925,1.11971735964533))
REPRESENTATION_ITEM('')
);
#1114=(
BOUNDED_CURVE()
B_SPLINE_CURVE(2,(#62048,#62049,#62050),.UNSPECIFIED.,.F.,.F.)
B_SPLINE_CURVE_WITH_KNOTS((3,3),(0.24995465243065,0.256253455718062),
 .UNSPECIFIED.)
CURVE()
GEOMETRIC_REPRESENTATION_ITEM()
RATIONAL_B_SPLINE_CURVE((1.11971735964607,1.12024119946954,1.12071541658429))
REPRESENTATION_ITEM('')
);
#1115=(
BOUNDED_CURVE()
B_SPLINE_CURVE(2,(#62054,#62055,#62056),.UNSPECIFIED.,.F.,.F.)
B_SPLINE_CURVE_WITH_KNOTS((3,3),(0.376641898803544,0.382940702095955),
 .UNSPECIFIED.)
CURVE()
GEOMETRIC_REPRESENTATION_ITEM()
RATIONAL_B_SPLINE_CURVE((1.12071541658421,1.12024119946907,1.11971735964515))
REPRESENTATION_ITEM('')
);
#1116=(
BOUNDED_CURVE()
B_SPLINE_CURVE(2,(#62060,#62061,#62062),.UNSPECIFIED.,.F.,.F.)
B_SPLINE_CURVE_WITH_KNOTS((3,3),(0.249954652430658,0.256253455718075),
 .UNSPECIFIED.)
CURVE()
GEOMETRIC_REPRESENTATION_ITEM()
RATIONAL_B_SPLINE_CURVE((1.11971735964629,1.12024119946976,1.12071541658452))
REPRESENTATION_ITEM('')
);
#1117=(
BOUNDED_CURVE()
B_SPLINE_CURVE(2,(#62066,#62067,#62068),.UNSPECIFIED.,.F.,.F.)
B_SPLINE_CURVE_WITH_KNOTS((3,3),(0.376641898803543,0.382940702095958),
 .UNSPECIFIED.)
CURVE()
GEOMETRIC_REPRESENTATION_ITEM()
RATIONAL_B_SPLINE_CURVE((1.12071541658432,1.12024119946919,1.11971735964527))
REPRESENTATION_ITEM('')
);
#1118=(
BOUNDED_CURVE()
B_SPLINE_CURVE(2,(#62072,#62073,#62074),.UNSPECIFIED.,.F.,.F.)
B_SPLINE_CURVE_WITH_KNOTS((3,3),(0.249954652430663,0.256253455718076),
 .UNSPECIFIED.)
CURVE()
GEOMETRIC_REPRESENTATION_ITEM()
RATIONAL_B_SPLINE_CURVE((1.11971735964633,1.12024119946979,1.12071541658455))
REPRESENTATION_ITEM('')
);
#1119=(
BOUNDED_CURVE()
B_SPLINE_CURVE(2,(#62078,#62079,#62080),.UNSPECIFIED.,.F.,.F.)
B_SPLINE_CURVE_WITH_KNOTS((3,3),(0.37664189880352,0.382940702095933),
 .UNSPECIFIED.)
CURVE()
GEOMETRIC_REPRESENTATION_ITEM()
RATIONAL_B_SPLINE_CURVE((1.1207154165845,1.12024119946936,1.11971735964544))
REPRESENTATION_ITEM('')
);
#1120=(
BOUNDED_CURVE()
B_SPLINE_CURVE(2,(#62084,#62085,#62086),.UNSPECIFIED.,.F.,.F.)
B_SPLINE_CURVE_WITH_KNOTS((3,3),(0.249954652430661,0.256253455718074),
 .UNSPECIFIED.)
CURVE()
GEOMETRIC_REPRESENTATION_ITEM()
RATIONAL_B_SPLINE_CURVE((1.11971735964627,1.12024119946973,1.12071541658449))
REPRESENTATION_ITEM('')
);
#1121=(
BOUNDED_CURVE()
B_SPLINE_CURVE(2,(#62090,#62091,#62092),.UNSPECIFIED.,.F.,.F.)
B_SPLINE_CURVE_WITH_KNOTS((3,3),(0.376641898803524,0.382940702095942),
 .UNSPECIFIED.)
CURVE()
GEOMETRIC_REPRESENTATION_ITEM()
RATIONAL_B_SPLINE_CURVE((1.12071541658449,1.12024119946935,1.11971735964543))
REPRESENTATION_ITEM('')
);
#1122=(
BOUNDED_CURVE()
B_SPLINE_CURVE(2,(#62096,#62097,#62098),.UNSPECIFIED.,.F.,.F.)
B_SPLINE_CURVE_WITH_KNOTS((3,3),(0.249954652430645,0.256253455718058),
 .UNSPECIFIED.)
CURVE()
GEOMETRIC_REPRESENTATION_ITEM()
RATIONAL_B_SPLINE_CURVE((1.11971735964602,1.12024119946949,1.12071541658425))
REPRESENTATION_ITEM('')
);
#1123=(
BOUNDED_CURVE()
B_SPLINE_CURVE(2,(#62102,#62103,#62104),.UNSPECIFIED.,.F.,.F.)
B_SPLINE_CURVE_WITH_KNOTS((3,3),(0.376641898803526,0.382940702095943),
 .UNSPECIFIED.)
CURVE()
GEOMETRIC_REPRESENTATION_ITEM()
RATIONAL_B_SPLINE_CURVE((1.12071541658447,1.12024119946934,1.11971735964542))
REPRESENTATION_ITEM('')
);
#1124=(
BOUNDED_CURVE()
B_SPLINE_CURVE(2,(#62108,#62109,#62110),.UNSPECIFIED.,.F.,.F.)
B_SPLINE_CURVE_WITH_KNOTS((3,3),(0.249954652430656,0.25625345571807),
 .UNSPECIFIED.)
CURVE()
GEOMETRIC_REPRESENTATION_ITEM()
RATIONAL_B_SPLINE_CURVE((1.11971735964623,1.12024119946969,1.12071541658445))
REPRESENTATION_ITEM('')
);
#1125=(
BOUNDED_CURVE()
B_SPLINE_CURVE(2,(#62114,#62115,#62116),.UNSPECIFIED.,.F.,.F.)
B_SPLINE_CURVE_WITH_KNOTS((3,3),(0.376641898803539,0.382940702095953),
 .UNSPECIFIED.)
CURVE()
GEOMETRIC_REPRESENTATION_ITEM()
RATIONAL_B_SPLINE_CURVE((1.12071541658437,1.12024119946923,1.11971735964531))
REPRESENTATION_ITEM('')
);
#1126=(
BOUNDED_CURVE()
B_SPLINE_CURVE(2,(#62120,#62121,#62122),.UNSPECIFIED.,.F.,.F.)
B_SPLINE_CURVE_WITH_KNOTS((3,3),(0.249954652430661,0.256253455718075),
 .UNSPECIFIED.)
CURVE()
GEOMETRIC_REPRESENTATION_ITEM()
RATIONAL_B_SPLINE_CURVE((1.11971735964628,1.12024119946974,1.1207154165845))
REPRESENTATION_ITEM('')
);
#1127=(
BOUNDED_CURVE()
B_SPLINE_CURVE(2,(#62126,#62127,#62128),.UNSPECIFIED.,.F.,.F.)
B_SPLINE_CURVE_WITH_KNOTS((3,3),(0.376641898803538,0.382940702095948),
 .UNSPECIFIED.)
CURVE()
GEOMETRIC_REPRESENTATION_ITEM()
RATIONAL_B_SPLINE_CURVE((1.12071541658433,1.1202411994692,1.11971735964528))
REPRESENTATION_ITEM('')
);
#1128=(
BOUNDED_CURVE()
B_SPLINE_CURVE(2,(#62132,#62133,#62134),.UNSPECIFIED.,.F.,.F.)
B_SPLINE_CURVE_WITH_KNOTS((3,3),(0.249954652430662,0.256253455718076),
 .UNSPECIFIED.)
CURVE()
GEOMETRIC_REPRESENTATION_ITEM()
RATIONAL_B_SPLINE_CURVE((1.11971735964622,1.12024119946968,1.12071541658444))
REPRESENTATION_ITEM('')
);
#1129=(
BOUNDED_CURVE()
B_SPLINE_CURVE(2,(#62138,#62139,#62140),.UNSPECIFIED.,.F.,.F.)
B_SPLINE_CURVE_WITH_KNOTS((3,3),(0.37664189880352,0.382940702095935),
 .UNSPECIFIED.)
CURVE()
GEOMETRIC_REPRESENTATION_ITEM()
RATIONAL_B_SPLINE_CURVE((1.12071541658454,1.12024119946941,1.11971735964549))
REPRESENTATION_ITEM('')
);
#1130=(
BOUNDED_CURVE()
B_SPLINE_CURVE(2,(#62144,#62145,#62146),.UNSPECIFIED.,.F.,.F.)
B_SPLINE_CURVE_WITH_KNOTS((3,3),(0.24995465243066,0.256253455718075),
 .UNSPECIFIED.)
CURVE()
GEOMETRIC_REPRESENTATION_ITEM()
RATIONAL_B_SPLINE_CURVE((1.1197173596463,1.12024119946976,1.12071541658452))
REPRESENTATION_ITEM('')
);
#1131=(
BOUNDED_CURVE()
B_SPLINE_CURVE(2,(#62150,#62151,#62152),.UNSPECIFIED.,.F.,.F.)
B_SPLINE_CURVE_WITH_KNOTS((3,3),(0.376641898803523,0.382940702095934),
 .UNSPECIFIED.)
CURVE()
GEOMETRIC_REPRESENTATION_ITEM()
RATIONAL_B_SPLINE_CURVE((1.12071541658448,1.12024119946934,1.11971735964542))
REPRESENTATION_ITEM('')
);
#1132=(
BOUNDED_CURVE()
B_SPLINE_CURVE(2,(#62156,#62157,#62158),.UNSPECIFIED.,.F.,.F.)
B_SPLINE_CURVE_WITH_KNOTS((3,3),(0.249954652430663,0.256253455718077),
 .UNSPECIFIED.)
CURVE()
GEOMETRIC_REPRESENTATION_ITEM()
RATIONAL_B_SPLINE_CURVE((1.11971735964627,1.12024119946973,1.12071541658449))
REPRESENTATION_ITEM('')
);
#1133=(
BOUNDED_CURVE()
B_SPLINE_CURVE(2,(#62162,#62163,#62164),.UNSPECIFIED.,.F.,.F.)
B_SPLINE_CURVE_WITH_KNOTS((3,3),(0.376641898803548,0.382940702095957),
 .UNSPECIFIED.)
CURVE()
GEOMETRIC_REPRESENTATION_ITEM()
RATIONAL_B_SPLINE_CURVE((1.12071541658418,1.12024119946905,1.11971735964513))
REPRESENTATION_ITEM('')
);
#1134=(
BOUNDED_CURVE()
B_SPLINE_CURVE(2,(#62168,#62169,#62170),.UNSPECIFIED.,.F.,.F.)
B_SPLINE_CURVE_WITH_KNOTS((3,3),(0.249954652430651,0.256253455718065),
 .UNSPECIFIED.)
CURVE()
GEOMETRIC_REPRESENTATION_ITEM()
RATIONAL_B_SPLINE_CURVE((1.1197173596461,1.12024119946956,1.12071541658432))
REPRESENTATION_ITEM('')
);
#1135=(
BOUNDED_CURVE()
B_SPLINE_CURVE(2,(#62174,#62175,#62176),.UNSPECIFIED.,.F.,.F.)
B_SPLINE_CURVE_WITH_KNOTS((3,3),(0.376641898803522,0.382940702095932),
 .UNSPECIFIED.)
CURVE()
GEOMETRIC_REPRESENTATION_ITEM()
RATIONAL_B_SPLINE_CURVE((1.12071541658448,1.12024119946934,1.11971735964542))
REPRESENTATION_ITEM('')
);
#1136=(
BOUNDED_CURVE()
B_SPLINE_CURVE(2,(#62180,#62181,#62182),.UNSPECIFIED.,.F.,.F.)
B_SPLINE_CURVE_WITH_KNOTS((3,3),(0.249954652430654,0.256253455718068),
 .UNSPECIFIED.)
CURVE()
GEOMETRIC_REPRESENTATION_ITEM()
RATIONAL_B_SPLINE_CURVE((1.11971735964629,1.12024119946976,1.12071541658452))
REPRESENTATION_ITEM('')
);
#1137=(
BOUNDED_CURVE()
B_SPLINE_CURVE(2,(#62186,#62187,#62188),.UNSPECIFIED.,.F.,.F.)
B_SPLINE_CURVE_WITH_KNOTS((3,3),(0.376641898803521,0.382940702095935),
 .UNSPECIFIED.)
CURVE()
GEOMETRIC_REPRESENTATION_ITEM()
RATIONAL_B_SPLINE_CURVE((1.12071541658442,1.12024119946928,1.11971735964536))
REPRESENTATION_ITEM('')
);
#1138=(
BOUNDED_CURVE()
B_SPLINE_CURVE(2,(#62192,#62193,#62194),.UNSPECIFIED.,.F.,.F.)
B_SPLINE_CURVE_WITH_KNOTS((3,3),(0.24995465243066,0.256253455718076),
 .UNSPECIFIED.)
CURVE()
GEOMETRIC_REPRESENTATION_ITEM()
RATIONAL_B_SPLINE_CURVE((1.11971735964628,1.12024119946975,1.12071541658451))
REPRESENTATION_ITEM('')
);
#1139=(
BOUNDED_CURVE()
B_SPLINE_CURVE(2,(#62198,#62199,#62200),.UNSPECIFIED.,.F.,.F.)
B_SPLINE_CURVE_WITH_KNOTS((3,3),(0.37664189880352,0.382940702095931),
 .UNSPECIFIED.)
CURVE()
GEOMETRIC_REPRESENTATION_ITEM()
RATIONAL_B_SPLINE_CURVE((1.12071541658452,1.12024119946938,1.11971735964546))
REPRESENTATION_ITEM('')
);
#1140=(
BOUNDED_CURVE()
B_SPLINE_CURVE(2,(#62204,#62205,#62206),.UNSPECIFIED.,.F.,.F.)
B_SPLINE_CURVE_WITH_KNOTS((3,3),(0.249954652430663,0.25625345571808),
 .UNSPECIFIED.)
CURVE()
GEOMETRIC_REPRESENTATION_ITEM()
RATIONAL_B_SPLINE_CURVE((1.11971735964629,1.12024119946975,1.12071541658451))
REPRESENTATION_ITEM('')
);
#1141=(
BOUNDED_CURVE()
B_SPLINE_CURVE(2,(#62210,#62211,#62212),.UNSPECIFIED.,.F.,.F.)
B_SPLINE_CURVE_WITH_KNOTS((3,3),(0.376641898803514,0.382940702095925),
 .UNSPECIFIED.)
CURVE()
GEOMETRIC_REPRESENTATION_ITEM()
RATIONAL_B_SPLINE_CURVE((1.12071541658449,1.12024119946936,1.11971735964544))
REPRESENTATION_ITEM('')
);
#1142=(
BOUNDED_CURVE()
B_SPLINE_CURVE(2,(#62216,#62217,#62218),.UNSPECIFIED.,.F.,.F.)
B_SPLINE_CURVE_WITH_KNOTS((3,3),(0.249954652430668,0.25625345571808),
 .UNSPECIFIED.)
CURVE()
GEOMETRIC_REPRESENTATION_ITEM()
RATIONAL_B_SPLINE_CURVE((1.11971735964628,1.12024119946974,1.1207154165845))
REPRESENTATION_ITEM('')
);
#1143=(
BOUNDED_CURVE()
B_SPLINE_CURVE(2,(#62222,#62223,#62224),.UNSPECIFIED.,.F.,.F.)
B_SPLINE_CURVE_WITH_KNOTS((3,3),(0.376641898803516,0.382940702095925),
 .UNSPECIFIED.)
CURVE()
GEOMETRIC_REPRESENTATION_ITEM()
RATIONAL_B_SPLINE_CURVE((1.1207154165845,1.12024119946936,1.11971735964544))
REPRESENTATION_ITEM('')
);
#1144=(
BOUNDED_CURVE()
B_SPLINE_CURVE(2,(#62228,#62229,#62230),.UNSPECIFIED.,.F.,.F.)
B_SPLINE_CURVE_WITH_KNOTS((3,3),(0.24995465243065,0.256253455718064),
 .UNSPECIFIED.)
CURVE()
GEOMETRIC_REPRESENTATION_ITEM()
RATIONAL_B_SPLINE_CURVE((1.11971735964608,1.12024119946955,1.1207154165843))
REPRESENTATION_ITEM('')
);
#1145=(
BOUNDED_CURVE()
B_SPLINE_CURVE(2,(#62234,#62235,#62236),.UNSPECIFIED.,.F.,.F.)
B_SPLINE_CURVE_WITH_KNOTS((3,3),(0.376641898803537,0.382940702095953),
 .UNSPECIFIED.)
CURVE()
GEOMETRIC_REPRESENTATION_ITEM()
RATIONAL_B_SPLINE_CURVE((1.12071541658421,1.12024119946908,1.11971735964516))
REPRESENTATION_ITEM('')
);
#1146=(
BOUNDED_CURVE()
B_SPLINE_CURVE(2,(#62240,#62241,#62242),.UNSPECIFIED.,.F.,.F.)
B_SPLINE_CURVE_WITH_KNOTS((3,3),(0.249954652430652,0.256253455718068),
 .UNSPECIFIED.)
CURVE()
GEOMETRIC_REPRESENTATION_ITEM()
RATIONAL_B_SPLINE_CURVE((1.11971735964626,1.12024119946972,1.12071541658448))
REPRESENTATION_ITEM('')
);
#1147=(
BOUNDED_CURVE()
B_SPLINE_CURVE(2,(#62246,#62247,#62248),.UNSPECIFIED.,.F.,.F.)
B_SPLINE_CURVE_WITH_KNOTS((3,3),(0.376641898803534,0.382940702095941),
 .UNSPECIFIED.)
CURVE()
GEOMETRIC_REPRESENTATION_ITEM()
RATIONAL_B_SPLINE_CURVE((1.12071541658423,1.1202411994691,1.11971735964518))
REPRESENTATION_ITEM('')
);
#1148=(
BOUNDED_CURVE()
B_SPLINE_CURVE(2,(#62252,#62253,#62254),.UNSPECIFIED.,.F.,.F.)
B_SPLINE_CURVE_WITH_KNOTS((3,3),(0.249954652430639,0.256253455718054),
 .UNSPECIFIED.)
CURVE()
GEOMETRIC_REPRESENTATION_ITEM()
RATIONAL_B_SPLINE_CURVE((1.11971735964598,1.12024119946944,1.1207154165842))
REPRESENTATION_ITEM('')
);
#1149=(
BOUNDED_CURVE()
B_SPLINE_CURVE(2,(#62258,#62259,#62260),.UNSPECIFIED.,.F.,.F.)
B_SPLINE_CURVE_WITH_KNOTS((3,3),(0.376641898803521,0.382940702095926),
 .UNSPECIFIED.)
CURVE()
GEOMETRIC_REPRESENTATION_ITEM()
RATIONAL_B_SPLINE_CURVE((1.12071541658441,1.12024119946928,1.11971735964536))
REPRESENTATION_ITEM('')
);
#1150=(
BOUNDED_CURVE()
B_SPLINE_CURVE(2,(#62264,#62265,#62266),.UNSPECIFIED.,.F.,.F.)
B_SPLINE_CURVE_WITH_KNOTS((3,3),(0.249954652430644,0.256253455718059),
 .UNSPECIFIED.)
CURVE()
GEOMETRIC_REPRESENTATION_ITEM()
RATIONAL_B_SPLINE_CURVE((1.11971735964605,1.12024119946951,1.12071541658427))
REPRESENTATION_ITEM('')
);
#1151=(
BOUNDED_CURVE()
B_SPLINE_CURVE(2,(#62270,#62271,#62272),.UNSPECIFIED.,.F.,.F.)
B_SPLINE_CURVE_WITH_KNOTS((3,3),(0.376641898803522,0.382940702095933),
 .UNSPECIFIED.)
CURVE()
GEOMETRIC_REPRESENTATION_ITEM()
RATIONAL_B_SPLINE_CURVE((1.12071541658452,1.12024119946939,1.11971735964547))
REPRESENTATION_ITEM('')
);
#1152=(
BOUNDED_CURVE()
B_SPLINE_CURVE(2,(#62276,#62277,#62278),.UNSPECIFIED.,.F.,.F.)
B_SPLINE_CURVE_WITH_KNOTS((3,3),(0.249954652430652,0.256253455718069),
 .UNSPECIFIED.)
CURVE()
GEOMETRIC_REPRESENTATION_ITEM()
RATIONAL_B_SPLINE_CURVE((1.11971735964616,1.12024119946962,1.12071541658438))
REPRESENTATION_ITEM('')
);
#1153=(
BOUNDED_CURVE()
B_SPLINE_CURVE(2,(#62282,#62283,#62284),.UNSPECIFIED.,.F.,.F.)
B_SPLINE_CURVE_WITH_KNOTS((3,3),(0.376641898803538,0.38294070209595),
 .UNSPECIFIED.)
CURVE()
GEOMETRIC_REPRESENTATION_ITEM()
RATIONAL_B_SPLINE_CURVE((1.12071541658426,1.12024119946913,1.11971735964521))
REPRESENTATION_ITEM('')
);
#1154=(
BOUNDED_CURVE()
B_SPLINE_CURVE(2,(#62287,#62288,#62289),.UNSPECIFIED.,.F.,.F.)
B_SPLINE_CURVE_WITH_KNOTS((3,3),(0.249954652430655,0.256253455718073),
 .UNSPECIFIED.)
CURVE()
GEOMETRIC_REPRESENTATION_ITEM()
RATIONAL_B_SPLINE_CURVE((1.11971735964623,1.1202411994697,1.12071541658446))
REPRESENTATION_ITEM('')
);
#1155=(
BOUNDED_CURVE()
B_SPLINE_CURVE(2,(#62291,#62292,#62293),.UNSPECIFIED.,.F.,.F.)
B_SPLINE_CURVE_WITH_KNOTS((3,3),(0.376641898803523,0.38294070209594),
 .UNSPECIFIED.)
CURVE()
GEOMETRIC_REPRESENTATION_ITEM()
RATIONAL_B_SPLINE_CURVE((1.12071541658441,1.12024119946928,1.11971735964536))
REPRESENTATION_ITEM('')
);
#1156=(
BOUNDED_CURVE()
B_SPLINE_CURVE(2,(#62296,#62297,#62298),.UNSPECIFIED.,.F.,.F.)
B_SPLINE_CURVE_WITH_KNOTS((3,3),(0.249954652430659,0.256253455718073),
 .UNSPECIFIED.)
CURVE()
GEOMETRIC_REPRESENTATION_ITEM()
RATIONAL_B_SPLINE_CURVE((1.11971735964623,1.12024119946969,1.12071541658445))
REPRESENTATION_ITEM('')
);
#1157=(
BOUNDED_CURVE()
B_SPLINE_CURVE(2,(#62300,#62301,#62302),.UNSPECIFIED.,.F.,.F.)
B_SPLINE_CURVE_WITH_KNOTS((3,3),(0.376641898803521,0.382940702095929),
 .UNSPECIFIED.)
CURVE()
GEOMETRIC_REPRESENTATION_ITEM()
RATIONAL_B_SPLINE_CURVE((1.12071541658454,1.1202411994694,1.11971735964548))
REPRESENTATION_ITEM('')
);
#1158=(
BOUNDED_CURVE()
B_SPLINE_CURVE(2,(#62305,#62306,#62307),.UNSPECIFIED.,.F.,.F.)
B_SPLINE_CURVE_WITH_KNOTS((3,3),(0.249954652430646,0.256253455718056),
 .UNSPECIFIED.)
CURVE()
GEOMETRIC_REPRESENTATION_ITEM()
RATIONAL_B_SPLINE_CURVE((1.11971735964596,1.12024119946942,1.12071541658418))
REPRESENTATION_ITEM('')
);
#1159=(
BOUNDED_CURVE()
B_SPLINE_CURVE(2,(#62309,#62310,#62311),.UNSPECIFIED.,.F.,.F.)
B_SPLINE_CURVE_WITH_KNOTS((3,3),(0.376641898803528,0.382940702095943),
 .UNSPECIFIED.)
CURVE()
GEOMETRIC_REPRESENTATION_ITEM()
RATIONAL_B_SPLINE_CURVE((1.12071541658433,1.1202411994692,1.11971735964528))
REPRESENTATION_ITEM('')
);
#1160=(
BOUNDED_CURVE()
B_SPLINE_CURVE(2,(#62314,#62315,#62316),.UNSPECIFIED.,.F.,.F.)
B_SPLINE_CURVE_WITH_KNOTS((3,3),(0.24995465243066,0.256253455718077),
 .UNSPECIFIED.)
CURVE()
GEOMETRIC_REPRESENTATION_ITEM()
RATIONAL_B_SPLINE_CURVE((1.11971735964636,1.12024119946983,1.12071541658459))
REPRESENTATION_ITEM('')
);
#1161=(
BOUNDED_CURVE()
B_SPLINE_CURVE(2,(#62318,#62319,#62320),.UNSPECIFIED.,.F.,.F.)
B_SPLINE_CURVE_WITH_KNOTS((3,3),(0.376641898803527,0.382940702095942),
 .UNSPECIFIED.)
CURVE()
GEOMETRIC_REPRESENTATION_ITEM()
RATIONAL_B_SPLINE_CURVE((1.12071541658443,1.12024119946929,1.11971735964537))
REPRESENTATION_ITEM('')
);
#1162=(
BOUNDED_CURVE()
B_SPLINE_CURVE(2,(#62323,#62324,#62325),.UNSPECIFIED.,.F.,.F.)
B_SPLINE_CURVE_WITH_KNOTS((3,3),(0.249954652430663,0.256253455718073),
 .UNSPECIFIED.)
CURVE()
GEOMETRIC_REPRESENTATION_ITEM()
RATIONAL_B_SPLINE_CURVE((1.11971735964622,1.12024119946969,1.12071541658445))
REPRESENTATION_ITEM('')
);
#1163=(
BOUNDED_CURVE()
B_SPLINE_CURVE(2,(#62327,#62328,#62329),.UNSPECIFIED.,.F.,.F.)
B_SPLINE_CURVE_WITH_KNOTS((3,3),(0.376641898803534,0.382940702095947),
 .UNSPECIFIED.)
CURVE()
GEOMETRIC_REPRESENTATION_ITEM()
RATIONAL_B_SPLINE_CURVE((1.12071541658425,1.12024119946912,1.1197173596452))
REPRESENTATION_ITEM('')
);
#1164=(
BOUNDED_CURVE()
B_SPLINE_CURVE(2,(#62332,#62333,#62334),.UNSPECIFIED.,.F.,.F.)
B_SPLINE_CURVE_WITH_KNOTS((3,3),(0.249954652430658,0.256253455718067),
 .UNSPECIFIED.)
CURVE()
GEOMETRIC_REPRESENTATION_ITEM()
RATIONAL_B_SPLINE_CURVE((1.1197173596462,1.12024119946966,1.12071541658442))
REPRESENTATION_ITEM('')
);
#1165=(
BOUNDED_CURVE()
B_SPLINE_CURVE(2,(#62336,#62337,#62338),.UNSPECIFIED.,.F.,.F.)
B_SPLINE_CURVE_WITH_KNOTS((3,3),(0.376641898803512,0.382940702095926),
 .UNSPECIFIED.)
CURVE()
GEOMETRIC_REPRESENTATION_ITEM()
RATIONAL_B_SPLINE_CURVE((1.12071541658454,1.12024119946941,1.11971735964549))
REPRESENTATION_ITEM('')
);
#1166=(
BOUNDED_CURVE()
B_SPLINE_CURVE(2,(#62341,#62342,#62343),.UNSPECIFIED.,.F.,.F.)
B_SPLINE_CURVE_WITH_KNOTS((3,3),(0.249954652430648,0.256253455718064),
 .UNSPECIFIED.)
CURVE()
GEOMETRIC_REPRESENTATION_ITEM()
RATIONAL_B_SPLINE_CURVE((1.11971735964605,1.12024119946951,1.12071541658427))
REPRESENTATION_ITEM('')
);
#1167=(
BOUNDED_CURVE()
B_SPLINE_CURVE(2,(#62345,#62346,#62347),.UNSPECIFIED.,.F.,.F.)
B_SPLINE_CURVE_WITH_KNOTS((3,3),(0.37664189880353,0.382940702095945),
 .UNSPECIFIED.)
CURVE()
GEOMETRIC_REPRESENTATION_ITEM()
RATIONAL_B_SPLINE_CURVE((1.12071541658432,1.12024119946919,1.11971735964527))
REPRESENTATION_ITEM('')
);
#1168=(
BOUNDED_CURVE()
B_SPLINE_CURVE(2,(#62350,#62351,#62352),.UNSPECIFIED.,.F.,.F.)
B_SPLINE_CURVE_WITH_KNOTS((3,3),(0.24995465243065,0.256253455718062),
 .UNSPECIFIED.)
CURVE()
GEOMETRIC_REPRESENTATION_ITEM()
RATIONAL_B_SPLINE_CURVE((1.1197173596462,1.12024119946966,1.12071541658442))
REPRESENTATION_ITEM('')
);
#1169=(
BOUNDED_CURVE()
B_SPLINE_CURVE(2,(#62354,#62355,#62356),.UNSPECIFIED.,.F.,.F.)
B_SPLINE_CURVE_WITH_KNOTS((3,3),(0.376641898803514,0.382940702095926),
 .UNSPECIFIED.)
CURVE()
GEOMETRIC_REPRESENTATION_ITEM()
RATIONAL_B_SPLINE_CURVE((1.12071541658458,1.12024119946944,1.11971735964552))
REPRESENTATION_ITEM('')
);
#1170=(
BOUNDED_CURVE()
B_SPLINE_CURVE(2,(#62359,#62360,#62361),.UNSPECIFIED.,.F.,.F.)
B_SPLINE_CURVE_WITH_KNOTS((3,3),(0.249954652430654,0.256253455718075),
 .UNSPECIFIED.)
CURVE()
GEOMETRIC_REPRESENTATION_ITEM()
RATIONAL_B_SPLINE_CURVE((1.11971735964632,1.12024119946978,1.12071541658454))
REPRESENTATION_ITEM('')
);
#1171=(
BOUNDED_CURVE()
B_SPLINE_CURVE(2,(#62363,#62364,#62365),.UNSPECIFIED.,.F.,.F.)
B_SPLINE_CURVE_WITH_KNOTS((3,3),(0.376641898803524,0.382940702095939),
 .UNSPECIFIED.)
CURVE()
GEOMETRIC_REPRESENTATION_ITEM()
RATIONAL_B_SPLINE_CURVE((1.12071541658443,1.1202411994693,1.11971735964538))
REPRESENTATION_ITEM('')
);
#1172=(
BOUNDED_CURVE()
B_SPLINE_CURVE(2,(#62368,#62369,#62370),.UNSPECIFIED.,.F.,.F.)
B_SPLINE_CURVE_WITH_KNOTS((3,3),(0.249954652430651,0.256253455718065),
 .UNSPECIFIED.)
CURVE()
GEOMETRIC_REPRESENTATION_ITEM()
RATIONAL_B_SPLINE_CURVE((1.11971735964614,1.12024119946961,1.12071541658437))
REPRESENTATION_ITEM('')
);
#1173=(
BOUNDED_CURVE()
B_SPLINE_CURVE(2,(#62372,#62373,#62374),.UNSPECIFIED.,.F.,.F.)
B_SPLINE_CURVE_WITH_KNOTS((3,3),(0.376641898803524,0.382940702095937),
 .UNSPECIFIED.)
CURVE()
GEOMETRIC_REPRESENTATION_ITEM()
RATIONAL_B_SPLINE_CURVE((1.12071541658443,1.1202411994693,1.11971735964538))
REPRESENTATION_ITEM('')
);
#1174=(
BOUNDED_CURVE()
B_SPLINE_CURVE(2,(#62377,#62378,#62379),.UNSPECIFIED.,.F.,.F.)
B_SPLINE_CURVE_WITH_KNOTS((3,3),(0.24995465243066,0.256253455718078),
 .UNSPECIFIED.)
CURVE()
GEOMETRIC_REPRESENTATION_ITEM()
RATIONAL_B_SPLINE_CURVE((1.11971735964625,1.12024119946971,1.12071541658447))
REPRESENTATION_ITEM('')
);
#1175=(
BOUNDED_CURVE()
B_SPLINE_CURVE(2,(#62381,#62382,#62383),.UNSPECIFIED.,.F.,.F.)
B_SPLINE_CURVE_WITH_KNOTS((3,3),(0.376641898803522,0.382940702095931),
 .UNSPECIFIED.)
CURVE()
GEOMETRIC_REPRESENTATION_ITEM()
RATIONAL_B_SPLINE_CURVE((1.1207154165845,1.12024119946936,1.11971735964544))
REPRESENTATION_ITEM('')
);
#1176=(
BOUNDED_CURVE()
B_SPLINE_CURVE(2,(#62386,#62387,#62388),.UNSPECIFIED.,.F.,.F.)
B_SPLINE_CURVE_WITH_KNOTS((3,3),(0.249954652430652,0.256253455718071),
 .UNSPECIFIED.)
CURVE()
GEOMETRIC_REPRESENTATION_ITEM()
RATIONAL_B_SPLINE_CURVE((1.11971735964614,1.12024119946961,1.12071541658437))
REPRESENTATION_ITEM('')
);
#1177=(
BOUNDED_CURVE()
B_SPLINE_CURVE(2,(#62390,#62391,#62392),.UNSPECIFIED.,.F.,.F.)
B_SPLINE_CURVE_WITH_KNOTS((3,3),(0.376641898803528,0.382940702095942),
 .UNSPECIFIED.)
CURVE()
GEOMETRIC_REPRESENTATION_ITEM()
RATIONAL_B_SPLINE_CURVE((1.12071541658436,1.12024119946922,1.1197173596453))
REPRESENTATION_ITEM('')
);
#1178=(
BOUNDED_CURVE()
B_SPLINE_CURVE(2,(#62395,#62396,#62397),.UNSPECIFIED.,.F.,.F.)
B_SPLINE_CURVE_WITH_KNOTS((3,3),(0.249954652430651,0.256253455718071),
 .UNSPECIFIED.)
CURVE()
GEOMETRIC_REPRESENTATION_ITEM()
RATIONAL_B_SPLINE_CURVE((1.11971735964609,1.12024119946955,1.12071541658431))
REPRESENTATION_ITEM('')
);
#1179=(
BOUNDED_CURVE()
B_SPLINE_CURVE(2,(#62399,#62400,#62401),.UNSPECIFIED.,.F.,.F.)
B_SPLINE_CURVE_WITH_KNOTS((3,3),(0.376641898803537,0.382940702095949),
 .UNSPECIFIED.)
CURVE()
GEOMETRIC_REPRESENTATION_ITEM()
RATIONAL_B_SPLINE_CURVE((1.12071541658424,1.1202411994691,1.11971735964519))
REPRESENTATION_ITEM('')
);
#1180=(
BOUNDED_CURVE()
B_SPLINE_CURVE(2,(#62404,#62405,#62406),.UNSPECIFIED.,.F.,.F.)
B_SPLINE_CURVE_WITH_KNOTS((3,3),(0.249954652430663,0.256253455718077),
 .UNSPECIFIED.)
CURVE()
GEOMETRIC_REPRESENTATION_ITEM()
RATIONAL_B_SPLINE_CURVE((1.11971735964627,1.12024119946974,1.1207154165845))
REPRESENTATION_ITEM('')
);
#1181=(
BOUNDED_CURVE()
B_SPLINE_CURVE(2,(#62408,#62409,#62410),.UNSPECIFIED.,.F.,.F.)
B_SPLINE_CURVE_WITH_KNOTS((3,3),(0.376641898803535,0.382940702095948),
 .UNSPECIFIED.)
CURVE()
GEOMETRIC_REPRESENTATION_ITEM()
RATIONAL_B_SPLINE_CURVE((1.12071541658433,1.1202411994692,1.11971735964528))
REPRESENTATION_ITEM('')
);
#1182=(
BOUNDED_CURVE()
B_SPLINE_CURVE(2,(#62413,#62414,#62415),.UNSPECIFIED.,.F.,.F.)
B_SPLINE_CURVE_WITH_KNOTS((3,3),(0.249954652430657,0.256253455718068),
 .UNSPECIFIED.)
CURVE()
GEOMETRIC_REPRESENTATION_ITEM()
RATIONAL_B_SPLINE_CURVE((1.11971735964623,1.1202411994697,1.12071541658445))
REPRESENTATION_ITEM('')
);
#1183=(
BOUNDED_CURVE()
B_SPLINE_CURVE(2,(#62417,#62418,#62419),.UNSPECIFIED.,.F.,.F.)
B_SPLINE_CURVE_WITH_KNOTS((3,3),(0.376641898803534,0.382940702095946),
 .UNSPECIFIED.)
CURVE()
GEOMETRIC_REPRESENTATION_ITEM()
RATIONAL_B_SPLINE_CURVE((1.12071541658428,1.12024119946915,1.11971735964523))
REPRESENTATION_ITEM('')
);
#1184=(
BOUNDED_CURVE()
B_SPLINE_CURVE(2,(#62423,#62424,#62425),.UNSPECIFIED.,.F.,.F.)
B_SPLINE_CURVE_WITH_KNOTS((3,3),(0.249954652430652,0.256253455718065),
 .UNSPECIFIED.)
CURVE()
GEOMETRIC_REPRESENTATION_ITEM()
RATIONAL_B_SPLINE_CURVE((1.11971735964615,1.12024119946961,1.12071541658437))
REPRESENTATION_ITEM('')
);
#1185=(
BOUNDED_CURVE()
B_SPLINE_CURVE(2,(#62429,#62430,#62431),.UNSPECIFIED.,.F.,.F.)
B_SPLINE_CURVE_WITH_KNOTS((3,3),(0.376641898803528,0.38294070209594),
 .UNSPECIFIED.)
CURVE()
GEOMETRIC_REPRESENTATION_ITEM()
RATIONAL_B_SPLINE_CURVE((1.12071541658438,1.12024119946925,1.11971735964533))
REPRESENTATION_ITEM('')
);
#1186=(
BOUNDED_CURVE()
B_SPLINE_CURVE(2,(#62435,#62436,#62437),.UNSPECIFIED.,.F.,.F.)
B_SPLINE_CURVE_WITH_KNOTS((3,3),(0.249954652430646,0.256253455718057),
 .UNSPECIFIED.)
CURVE()
GEOMETRIC_REPRESENTATION_ITEM()
RATIONAL_B_SPLINE_CURVE((1.11971735964604,1.12024119946951,1.12071541658426))
REPRESENTATION_ITEM('')
);
#1187=(
BOUNDED_CURVE()
B_SPLINE_CURVE(2,(#62441,#62442,#62443),.UNSPECIFIED.,.F.,.F.)
B_SPLINE_CURVE_WITH_KNOTS((3,3),(0.376641898803525,0.382940702095939),
 .UNSPECIFIED.)
CURVE()
GEOMETRIC_REPRESENTATION_ITEM()
RATIONAL_B_SPLINE_CURVE((1.12071541658443,1.1202411994693,1.11971735964538))
REPRESENTATION_ITEM('')
);
#1188=(
BOUNDED_CURVE()
B_SPLINE_CURVE(2,(#62447,#62448,#62449),.UNSPECIFIED.,.F.,.F.)
B_SPLINE_CURVE_WITH_KNOTS((3,3),(0.249954652430639,0.256253455718051),
 .UNSPECIFIED.)
CURVE()
GEOMETRIC_REPRESENTATION_ITEM()
RATIONAL_B_SPLINE_CURVE((1.11971735964598,1.12024119946945,1.1207154165842))
REPRESENTATION_ITEM('')
);
#1189=(
BOUNDED_CURVE()
B_SPLINE_CURVE(2,(#62453,#62454,#62455),.UNSPECIFIED.,.F.,.F.)
B_SPLINE_CURVE_WITH_KNOTS((3,3),(0.376641898803521,0.382940702095934),
 .UNSPECIFIED.)
CURVE()
GEOMETRIC_REPRESENTATION_ITEM()
RATIONAL_B_SPLINE_CURVE((1.12071541658441,1.12024119946928,1.11971735964536))
REPRESENTATION_ITEM('')
);
#1190=(
BOUNDED_CURVE()
B_SPLINE_CURVE(2,(#62459,#62460,#62461),.UNSPECIFIED.,.F.,.F.)
B_SPLINE_CURVE_WITH_KNOTS((3,3),(0.249954652430652,0.256253455718065),
 .UNSPECIFIED.)
CURVE()
GEOMETRIC_REPRESENTATION_ITEM()
RATIONAL_B_SPLINE_CURVE((1.11971735964616,1.12024119946962,1.12071541658438))
REPRESENTATION_ITEM('')
);
#1191=(
BOUNDED_CURVE()
B_SPLINE_CURVE(2,(#62465,#62466,#62467),.UNSPECIFIED.,.F.,.F.)
B_SPLINE_CURVE_WITH_KNOTS((3,3),(0.376641898803544,0.382940702095957),
 .UNSPECIFIED.)
CURVE()
GEOMETRIC_REPRESENTATION_ITEM()
RATIONAL_B_SPLINE_CURVE((1.12071541658424,1.1202411994691,1.11971735964518))
REPRESENTATION_ITEM('')
);
#1192=(
BOUNDED_CURVE()
B_SPLINE_CURVE(2,(#62471,#62472,#62473),.UNSPECIFIED.,.F.,.F.)
B_SPLINE_CURVE_WITH_KNOTS((3,3),(0.249954652430643,0.256253455718053),
 .UNSPECIFIED.)
CURVE()
GEOMETRIC_REPRESENTATION_ITEM()
RATIONAL_B_SPLINE_CURVE((1.11971735964601,1.12024119946947,1.12071541658423))
REPRESENTATION_ITEM('')
);
#1193=(
BOUNDED_CURVE()
B_SPLINE_CURVE(2,(#62477,#62478,#62479),.UNSPECIFIED.,.F.,.F.)
B_SPLINE_CURVE_WITH_KNOTS((3,3),(0.376641898803543,0.382940702095953),
 .UNSPECIFIED.)
CURVE()
GEOMETRIC_REPRESENTATION_ITEM()
RATIONAL_B_SPLINE_CURVE((1.12071541658425,1.12024119946911,1.1197173596452))
REPRESENTATION_ITEM('')
);
#1194=(
BOUNDED_CURVE()
B_SPLINE_CURVE(2,(#62483,#62484,#62485),.UNSPECIFIED.,.F.,.F.)
B_SPLINE_CURVE_WITH_KNOTS((3,3),(0.249954652430649,0.256253455718062),
 .UNSPECIFIED.)
CURVE()
GEOMETRIC_REPRESENTATION_ITEM()
RATIONAL_B_SPLINE_CURVE((1.11971735964607,1.12024119946954,1.12071541658429))
REPRESENTATION_ITEM('')
);
#1195=(
BOUNDED_CURVE()
B_SPLINE_CURVE(2,(#70283,#70284,#70285),.UNSPECIFIED.,.F.,.F.)
B_SPLINE_CURVE_WITH_KNOTS((3,3),(-0.375752880509706,-0.25773139970398),
 .UNSPECIFIED.)
CURVE()
GEOMETRIC_REPRESENTATION_ITEM()
RATIONAL_B_SPLINE_CURVE((1.41147367097488,1.52065153937885,1.52065153937885))
REPRESENTATION_ITEM('')
);
#1196=(
BOUNDED_CURVE()
B_SPLINE_CURVE(2,(#70287,#70288,#70289),.UNSPECIFIED.,.F.,.F.)
B_SPLINE_CURVE_WITH_KNOTS((3,3),(-0.375752880509709,-0.139709918898254),
 .UNSPECIFIED.)
CURVE()
GEOMETRIC_REPRESENTATION_ITEM()
RATIONAL_B_SPLINE_CURVE((1.41147367097488,1.62982940778282,1.41147367097488))
REPRESENTATION_ITEM('')
);
#1197=(
BOUNDED_CURVE()
B_SPLINE_CURVE(2,(#70291,#70292,#70293),.UNSPECIFIED.,.F.,.F.)
B_SPLINE_CURVE_WITH_KNOTS((3,3),(-0.375752880509709,-0.139709918898254),
 .UNSPECIFIED.)
CURVE()
GEOMETRIC_REPRESENTATION_ITEM()
RATIONAL_B_SPLINE_CURVE((1.41147367097488,1.62982940778282,1.41147367097488))
REPRESENTATION_ITEM('')
);
#1198=(
BOUNDED_CURVE()
B_SPLINE_CURVE(2,(#70295,#70296,#70297),.UNSPECIFIED.,.F.,.F.)
B_SPLINE_CURVE_WITH_KNOTS((3,3),(-0.375752880509708,-0.139709918898254),
 .UNSPECIFIED.)
CURVE()
GEOMETRIC_REPRESENTATION_ITEM()
RATIONAL_B_SPLINE_CURVE((1.41147367097487,1.62982940778281,1.41147367097487))
REPRESENTATION_ITEM('')
);
#1199=(
BOUNDED_CURVE()
B_SPLINE_CURVE(2,(#70299,#70300,#70301),.UNSPECIFIED.,.F.,.F.)
B_SPLINE_CURVE_WITH_KNOTS((3,3),(-0.375752880509709,-0.139709918898253),
 .UNSPECIFIED.)
CURVE()
GEOMETRIC_REPRESENTATION_ITEM()
RATIONAL_B_SPLINE_CURVE((1.41147367097488,1.62982940778282,1.41147367097488))
REPRESENTATION_ITEM('')
);
#1200=(
BOUNDED_CURVE()
B_SPLINE_CURVE(2,(#70303,#70304,#70305),.UNSPECIFIED.,.F.,.F.)
B_SPLINE_CURVE_WITH_KNOTS((3,3),(-0.375752880509709,-0.139709918898254),
 .UNSPECIFIED.)
CURVE()
GEOMETRIC_REPRESENTATION_ITEM()
RATIONAL_B_SPLINE_CURVE((1.41147367097488,1.62982940778282,1.41147367097488))
REPRESENTATION_ITEM('')
);
#1201=(
BOUNDED_CURVE()
B_SPLINE_CURVE(2,(#70306,#70307,#70308),.UNSPECIFIED.,.F.,.F.)
B_SPLINE_CURVE_WITH_KNOTS((3,3),(-0.25773139970398,-0.139709918898256),
 .UNSPECIFIED.)
CURVE()
GEOMETRIC_REPRESENTATION_ITEM()
RATIONAL_B_SPLINE_CURVE((1.52065153937885,1.52065153937885,1.41147367097488))
REPRESENTATION_ITEM('')
);
#1202=(
BOUNDED_CURVE()
B_SPLINE_CURVE(2,(#70330,#70331,#70332),.UNSPECIFIED.,.F.,.F.)
B_SPLINE_CURVE_WITH_KNOTS((3,3),(0.367644516946548,0.373830527582523),
 .UNSPECIFIED.)
CURVE()
GEOMETRIC_REPRESENTATION_ITEM()
RATIONAL_B_SPLINE_CURVE((1.13426390111316,1.13389822901309,1.13348223894575))
REPRESENTATION_ITEM('')
);
#1203=(
BOUNDED_CURVE()
B_SPLINE_CURVE(2,(#70336,#70337,#70338),.UNSPECIFIED.,.F.,.F.)
B_SPLINE_CURVE_WITH_KNOTS((3,3),(0.271548216895916,0.277734227531904),
 .UNSPECIFIED.)
CURVE()
GEOMETRIC_REPRESENTATION_ITEM()
RATIONAL_B_SPLINE_CURVE((1.13348223894615,1.1338982290135,1.13426390111357))
REPRESENTATION_ITEM('')
);
#1204=(
BOUNDED_CURVE()
B_SPLINE_CURVE(2,(#70342,#70343,#70344),.UNSPECIFIED.,.F.,.F.)
B_SPLINE_CURVE_WITH_KNOTS((3,3),(0.36764451694656,0.373830527582529),
 .UNSPECIFIED.)
CURVE()
GEOMETRIC_REPRESENTATION_ITEM()
RATIONAL_B_SPLINE_CURVE((1.13426390111306,1.13389822901299,1.13348223894565))
REPRESENTATION_ITEM('')
);
#1205=(
BOUNDED_CURVE()
B_SPLINE_CURVE(2,(#70348,#70349,#70350),.UNSPECIFIED.,.F.,.F.)
B_SPLINE_CURVE_WITH_KNOTS((3,3),(0.271548216895914,0.277734227531901),
 .UNSPECIFIED.)
CURVE()
GEOMETRIC_REPRESENTATION_ITEM()
RATIONAL_B_SPLINE_CURVE((1.13348223894612,1.13389822901347,1.13426390111354))
REPRESENTATION_ITEM('')
);
#1206=(
BOUNDED_CURVE()
B_SPLINE_CURVE(2,(#70354,#70355,#70356),.UNSPECIFIED.,.F.,.F.)
B_SPLINE_CURVE_WITH_KNOTS((3,3),(0.367644516946562,0.373830527582532),
 .UNSPECIFIED.)
CURVE()
GEOMETRIC_REPRESENTATION_ITEM()
RATIONAL_B_SPLINE_CURVE((1.13426390111304,1.13389822901297,1.13348223894563))
REPRESENTATION_ITEM('')
);
#1207=(
BOUNDED_CURVE()
B_SPLINE_CURVE(2,(#70360,#70361,#70362),.UNSPECIFIED.,.F.,.F.)
B_SPLINE_CURVE_WITH_KNOTS((3,3),(0.27154821689591,0.277734227531895),
 .UNSPECIFIED.)
CURVE()
GEOMETRIC_REPRESENTATION_ITEM()
RATIONAL_B_SPLINE_CURVE((1.13348223894613,1.13389822901348,1.13426390111355))
REPRESENTATION_ITEM('')
);
#1208=(
BOUNDED_CURVE()
B_SPLINE_CURVE(2,(#70366,#70367,#70368),.UNSPECIFIED.,.F.,.F.)
B_SPLINE_CURVE_WITH_KNOTS((3,3),(0.367644516946554,0.373830527582529),
 .UNSPECIFIED.)
CURVE()
GEOMETRIC_REPRESENTATION_ITEM()
RATIONAL_B_SPLINE_CURVE((1.13426390111305,1.13389822901299,1.13348223894564))
REPRESENTATION_ITEM('')
);
#1209=(
BOUNDED_CURVE()
B_SPLINE_CURVE(2,(#70372,#70373,#70374),.UNSPECIFIED.,.F.,.F.)
B_SPLINE_CURVE_WITH_KNOTS((3,3),(0.271548216895907,0.277734227531893),
 .UNSPECIFIED.)
CURVE()
GEOMETRIC_REPRESENTATION_ITEM()
RATIONAL_B_SPLINE_CURVE((1.13348223894611,1.13389822901346,1.13426390111353))
REPRESENTATION_ITEM('')
);
#1210=(
BOUNDED_CURVE()
B_SPLINE_CURVE(2,(#70378,#70379,#70380),.UNSPECIFIED.,.F.,.F.)
B_SPLINE_CURVE_WITH_KNOTS((3,3),(0.367644516946562,0.373830527582532),
 .UNSPECIFIED.)
CURVE()
GEOMETRIC_REPRESENTATION_ITEM()
RATIONAL_B_SPLINE_CURVE((1.13426390111302,1.13389822901296,1.13348223894561))
REPRESENTATION_ITEM('')
);
#1211=(
BOUNDED_CURVE()
B_SPLINE_CURVE(2,(#70384,#70385,#70386),.UNSPECIFIED.,.F.,.F.)
B_SPLINE_CURVE_WITH_KNOTS((3,3),(0.271548216895914,0.277734227531899),
 .UNSPECIFIED.)
CURVE()
GEOMETRIC_REPRESENTATION_ITEM()
RATIONAL_B_SPLINE_CURVE((1.13348223894609,1.13389822901344,1.13426390111351))
REPRESENTATION_ITEM('')
);
#1212=(
BOUNDED_CURVE()
B_SPLINE_CURVE(2,(#70390,#70391,#70392),.UNSPECIFIED.,.F.,.F.)
B_SPLINE_CURVE_WITH_KNOTS((3,3),(0.36764451694656,0.373830527582535),
 .UNSPECIFIED.)
CURVE()
GEOMETRIC_REPRESENTATION_ITEM()
RATIONAL_B_SPLINE_CURVE((1.13426390111302,1.13389822901295,1.1334822389456))
REPRESENTATION_ITEM('')
);
#1213=(
BOUNDED_CURVE()
B_SPLINE_CURVE(2,(#70396,#70397,#70398),.UNSPECIFIED.,.F.,.F.)
B_SPLINE_CURVE_WITH_KNOTS((3,3),(0.271548216895908,0.277734227531894),
 .UNSPECIFIED.)
CURVE()
GEOMETRIC_REPRESENTATION_ITEM()
RATIONAL_B_SPLINE_CURVE((1.1334822389461,1.13389822901345,1.13426390111352))
REPRESENTATION_ITEM('')
);
#1214=(
BOUNDED_CURVE()
B_SPLINE_CURVE(2,(#70402,#70403,#70404),.UNSPECIFIED.,.F.,.F.)
B_SPLINE_CURVE_WITH_KNOTS((3,3),(0.367644516946558,0.373830527582536),
 .UNSPECIFIED.)
CURVE()
GEOMETRIC_REPRESENTATION_ITEM()
RATIONAL_B_SPLINE_CURVE((1.13426390111302,1.13389822901295,1.13348223894561))
REPRESENTATION_ITEM('')
);
#1215=(
BOUNDED_CURVE()
B_SPLINE_CURVE(2,(#70408,#70409,#70410),.UNSPECIFIED.,.F.,.F.)
B_SPLINE_CURVE_WITH_KNOTS((3,3),(0.271548216895914,0.277734227531899),
 .UNSPECIFIED.)
CURVE()
GEOMETRIC_REPRESENTATION_ITEM()
RATIONAL_B_SPLINE_CURVE((1.13348223894613,1.13389822901348,1.13426390111355))
REPRESENTATION_ITEM('')
);
#1216=(
BOUNDED_CURVE()
B_SPLINE_CURVE(2,(#70414,#70415,#70416),.UNSPECIFIED.,.F.,.F.)
B_SPLINE_CURVE_WITH_KNOTS((3,3),(0.367644516946564,0.373830527582534),
 .UNSPECIFIED.)
CURVE()
GEOMETRIC_REPRESENTATION_ITEM()
RATIONAL_B_SPLINE_CURVE((1.13426390111303,1.13389822901296,1.13348223894561))
REPRESENTATION_ITEM('')
);
#1217=(
BOUNDED_CURVE()
B_SPLINE_CURVE(2,(#70420,#70421,#70422),.UNSPECIFIED.,.F.,.F.)
B_SPLINE_CURVE_WITH_KNOTS((3,3),(0.271548216895916,0.277734227531901),
 .UNSPECIFIED.)
CURVE()
GEOMETRIC_REPRESENTATION_ITEM()
RATIONAL_B_SPLINE_CURVE((1.13348223894614,1.13389822901349,1.13426390111357))
REPRESENTATION_ITEM('')
);
#1218=(
BOUNDED_CURVE()
B_SPLINE_CURVE(2,(#70426,#70427,#70428),.UNSPECIFIED.,.F.,.F.)
B_SPLINE_CURVE_WITH_KNOTS((3,3),(0.367644516946554,0.373830527582527),
 .UNSPECIFIED.)
CURVE()
GEOMETRIC_REPRESENTATION_ITEM()
RATIONAL_B_SPLINE_CURVE((1.13426390111312,1.13389822901305,1.13348223894571))
REPRESENTATION_ITEM('')
);
#1219=(
BOUNDED_CURVE()
B_SPLINE_CURVE(2,(#70432,#70433,#70434),.UNSPECIFIED.,.F.,.F.)
B_SPLINE_CURVE_WITH_KNOTS((3,3),(0.271548216895913,0.2777342275319),
 .UNSPECIFIED.)
CURVE()
GEOMETRIC_REPRESENTATION_ITEM()
RATIONAL_B_SPLINE_CURVE((1.13348223894615,1.1338982290135,1.13426390111358))
REPRESENTATION_ITEM('')
);
#1220=(
BOUNDED_CURVE()
B_SPLINE_CURVE(2,(#70438,#70439,#70440),.UNSPECIFIED.,.F.,.F.)
B_SPLINE_CURVE_WITH_KNOTS((3,3),(0.367644516946564,0.373830527582538),
 .UNSPECIFIED.)
CURVE()
GEOMETRIC_REPRESENTATION_ITEM()
RATIONAL_B_SPLINE_CURVE((1.134263901113,1.13389822901293,1.13348223894559))
REPRESENTATION_ITEM('')
);
#1221=(
BOUNDED_CURVE()
B_SPLINE_CURVE(2,(#70444,#70445,#70446),.UNSPECIFIED.,.F.,.F.)
B_SPLINE_CURVE_WITH_KNOTS((3,3),(0.271548216895908,0.277734227531895),
 .UNSPECIFIED.)
CURVE()
GEOMETRIC_REPRESENTATION_ITEM()
RATIONAL_B_SPLINE_CURVE((1.13348223894615,1.1338982290135,1.13426390111358))
REPRESENTATION_ITEM('')
);
#1222=(
BOUNDED_CURVE()
B_SPLINE_CURVE(2,(#70450,#70451,#70452),.UNSPECIFIED.,.F.,.F.)
B_SPLINE_CURVE_WITH_KNOTS((3,3),(0.367644516946561,0.373830527582532),
 .UNSPECIFIED.)
CURVE()
GEOMETRIC_REPRESENTATION_ITEM()
RATIONAL_B_SPLINE_CURVE((1.13426390111309,1.13389822901302,1.13348223894568))
REPRESENTATION_ITEM('')
);
#1223=(
BOUNDED_CURVE()
B_SPLINE_CURVE(2,(#70456,#70457,#70458),.UNSPECIFIED.,.F.,.F.)
B_SPLINE_CURVE_WITH_KNOTS((3,3),(0.271548216895921,0.277734227531907),
 .UNSPECIFIED.)
CURVE()
GEOMETRIC_REPRESENTATION_ITEM()
RATIONAL_B_SPLINE_CURVE((1.13348223894616,1.13389822901351,1.13426390111358))
REPRESENTATION_ITEM('')
);
#1224=(
BOUNDED_CURVE()
B_SPLINE_CURVE(2,(#70462,#70463,#70464),.UNSPECIFIED.,.F.,.F.)
B_SPLINE_CURVE_WITH_KNOTS((3,3),(0.367644516946558,0.373830527582535),
 .UNSPECIFIED.)
CURVE()
GEOMETRIC_REPRESENTATION_ITEM()
RATIONAL_B_SPLINE_CURVE((1.13426390111305,1.13389822901298,1.13348223894564))
REPRESENTATION_ITEM('')
);
#1225=(
BOUNDED_CURVE()
B_SPLINE_CURVE(2,(#70468,#70469,#70470),.UNSPECIFIED.,.F.,.F.)
B_SPLINE_CURVE_WITH_KNOTS((3,3),(0.271548216895908,0.27773422753189),
 .UNSPECIFIED.)
CURVE()
GEOMETRIC_REPRESENTATION_ITEM()
RATIONAL_B_SPLINE_CURVE((1.13348223894616,1.13389822901351,1.13426390111359))
REPRESENTATION_ITEM('')
);
#1226=(
BOUNDED_CURVE()
B_SPLINE_CURVE(2,(#70474,#70475,#70476),.UNSPECIFIED.,.F.,.F.)
B_SPLINE_CURVE_WITH_KNOTS((3,3),(0.367644516946548,0.373830527582523),
 .UNSPECIFIED.)
CURVE()
GEOMETRIC_REPRESENTATION_ITEM()
RATIONAL_B_SPLINE_CURVE((1.13426390111314,1.13389822901308,1.13348223894573))
REPRESENTATION_ITEM('')
);
#1227=(
BOUNDED_CURVE()
B_SPLINE_CURVE(2,(#70480,#70481,#70482),.UNSPECIFIED.,.F.,.F.)
B_SPLINE_CURVE_WITH_KNOTS((3,3),(0.271548216895905,0.277734227531892),
 .UNSPECIFIED.)
CURVE()
GEOMETRIC_REPRESENTATION_ITEM()
RATIONAL_B_SPLINE_CURVE((1.13348223894608,1.13389822901343,1.1342639011135))
REPRESENTATION_ITEM('')
);
#1228=(
BOUNDED_CURVE()
B_SPLINE_CURVE(2,(#70486,#70487,#70488),.UNSPECIFIED.,.F.,.F.)
B_SPLINE_CURVE_WITH_KNOTS((3,3),(0.36764451694655,0.373830527582528),
 .UNSPECIFIED.)
CURVE()
GEOMETRIC_REPRESENTATION_ITEM()
RATIONAL_B_SPLINE_CURVE((1.1342639011131,1.13389822901304,1.13348223894569))
REPRESENTATION_ITEM('')
);
#1229=(
BOUNDED_CURVE()
B_SPLINE_CURVE(2,(#70492,#70493,#70494),.UNSPECIFIED.,.F.,.F.)
B_SPLINE_CURVE_WITH_KNOTS((3,3),(0.27154821689591,0.277734227531895),
 .UNSPECIFIED.)
CURVE()
GEOMETRIC_REPRESENTATION_ITEM()
RATIONAL_B_SPLINE_CURVE((1.13348223894612,1.13389822901347,1.13426390111354))
REPRESENTATION_ITEM('')
);
#1230=(
BOUNDED_CURVE()
B_SPLINE_CURVE(2,(#70498,#70499,#70500),.UNSPECIFIED.,.F.,.F.)
B_SPLINE_CURVE_WITH_KNOTS((3,3),(0.367644516946551,0.373830527582525),
 .UNSPECIFIED.)
CURVE()
GEOMETRIC_REPRESENTATION_ITEM()
RATIONAL_B_SPLINE_CURVE((1.13426390111313,1.13389822901307,1.13348223894572))
REPRESENTATION_ITEM('')
);
#1231=(
BOUNDED_CURVE()
B_SPLINE_CURVE(2,(#70504,#70505,#70506),.UNSPECIFIED.,.F.,.F.)
B_SPLINE_CURVE_WITH_KNOTS((3,3),(0.271548216895914,0.277734227531894),
 .UNSPECIFIED.)
CURVE()
GEOMETRIC_REPRESENTATION_ITEM()
RATIONAL_B_SPLINE_CURVE((1.13348223894619,1.13389822901354,1.13426390111361))
REPRESENTATION_ITEM('')
);
#1232=(
BOUNDED_CURVE()
B_SPLINE_CURVE(2,(#70510,#70511,#70512),.UNSPECIFIED.,.F.,.F.)
B_SPLINE_CURVE_WITH_KNOTS((3,3),(0.367644516946565,0.373830527582531),
 .UNSPECIFIED.)
CURVE()
GEOMETRIC_REPRESENTATION_ITEM()
RATIONAL_B_SPLINE_CURVE((1.134263901113,1.13389822901293,1.13348223894559))
REPRESENTATION_ITEM('')
);
#1233=(
BOUNDED_CURVE()
B_SPLINE_CURVE(2,(#70516,#70517,#70518),.UNSPECIFIED.,.F.,.F.)
B_SPLINE_CURVE_WITH_KNOTS((3,3),(0.271548216895912,0.277734227531896),
 .UNSPECIFIED.)
CURVE()
GEOMETRIC_REPRESENTATION_ITEM()
RATIONAL_B_SPLINE_CURVE((1.13348223894612,1.13389822901347,1.13426390111354))
REPRESENTATION_ITEM('')
);
#1234=(
BOUNDED_CURVE()
B_SPLINE_CURVE(2,(#70522,#70523,#70524),.UNSPECIFIED.,.F.,.F.)
B_SPLINE_CURVE_WITH_KNOTS((3,3),(0.367644516946563,0.373830527582537),
 .UNSPECIFIED.)
CURVE()
GEOMETRIC_REPRESENTATION_ITEM()
RATIONAL_B_SPLINE_CURVE((1.13426390111305,1.13389822901298,1.13348223894564))
REPRESENTATION_ITEM('')
);
#1235=(
BOUNDED_CURVE()
B_SPLINE_CURVE(2,(#70528,#70529,#70530),.UNSPECIFIED.,.F.,.F.)
B_SPLINE_CURVE_WITH_KNOTS((3,3),(0.271548216895909,0.277734227531891),
 .UNSPECIFIED.)
CURVE()
GEOMETRIC_REPRESENTATION_ITEM()
RATIONAL_B_SPLINE_CURVE((1.13348223894604,1.13389822901339,1.13426390111346))
REPRESENTATION_ITEM('')
);
#1236=(
BOUNDED_CURVE()
B_SPLINE_CURVE(2,(#70534,#70535,#70536),.UNSPECIFIED.,.F.,.F.)
B_SPLINE_CURVE_WITH_KNOTS((3,3),(0.367644516946552,0.373830527582532),
 .UNSPECIFIED.)
CURVE()
GEOMETRIC_REPRESENTATION_ITEM()
RATIONAL_B_SPLINE_CURVE((1.13426390111305,1.13389822901299,1.13348223894564))
REPRESENTATION_ITEM('')
);
#1237=(
BOUNDED_CURVE()
B_SPLINE_CURVE(2,(#70540,#70541,#70542),.UNSPECIFIED.,.F.,.F.)
B_SPLINE_CURVE_WITH_KNOTS((3,3),(0.271548216895916,0.277734227531902),
 .UNSPECIFIED.)
CURVE()
GEOMETRIC_REPRESENTATION_ITEM()
RATIONAL_B_SPLINE_CURVE((1.13348223894616,1.13389822901351,1.13426390111359))
REPRESENTATION_ITEM('')
);
#1238=(
BOUNDED_CURVE()
B_SPLINE_CURVE(2,(#70546,#70547,#70548),.UNSPECIFIED.,.F.,.F.)
B_SPLINE_CURVE_WITH_KNOTS((3,3),(0.367644516946562,0.373830527582535),
 .UNSPECIFIED.)
CURVE()
GEOMETRIC_REPRESENTATION_ITEM()
RATIONAL_B_SPLINE_CURVE((1.13426390111309,1.13389822901302,1.13348223894568))
REPRESENTATION_ITEM('')
);
#1239=(
BOUNDED_CURVE()
B_SPLINE_CURVE(2,(#70552,#70553,#70554),.UNSPECIFIED.,.F.,.F.)
B_SPLINE_CURVE_WITH_KNOTS((3,3),(0.271548216895913,0.277734227531904),
 .UNSPECIFIED.)
CURVE()
GEOMETRIC_REPRESENTATION_ITEM()
RATIONAL_B_SPLINE_CURVE((1.13348223894619,1.13389822901354,1.13426390111362))
REPRESENTATION_ITEM('')
);
#1240=(
BOUNDED_CURVE()
B_SPLINE_CURVE(2,(#70558,#70559,#70560),.UNSPECIFIED.,.F.,.F.)
B_SPLINE_CURVE_WITH_KNOTS((3,3),(0.36764451694655,0.373830527582524),
 .UNSPECIFIED.)
CURVE()
GEOMETRIC_REPRESENTATION_ITEM()
RATIONAL_B_SPLINE_CURVE((1.13426390111312,1.13389822901305,1.13348223894571))
REPRESENTATION_ITEM('')
);
#1241=(
BOUNDED_CURVE()
B_SPLINE_CURVE(2,(#70564,#70565,#70566),.UNSPECIFIED.,.F.,.F.)
B_SPLINE_CURVE_WITH_KNOTS((3,3),(0.271548216895921,0.277734227531899),
 .UNSPECIFIED.)
CURVE()
GEOMETRIC_REPRESENTATION_ITEM()
RATIONAL_B_SPLINE_CURVE((1.13348223894619,1.13389822901354,1.13426390111361))
REPRESENTATION_ITEM('')
);
#1242=(
BOUNDED_CURVE()
B_SPLINE_CURVE(2,(#70570,#70571,#70572),.UNSPECIFIED.,.F.,.F.)
B_SPLINE_CURVE_WITH_KNOTS((3,3),(0.367644516946559,0.373830527582526),
 .UNSPECIFIED.)
CURVE()
GEOMETRIC_REPRESENTATION_ITEM()
RATIONAL_B_SPLINE_CURVE((1.1342639011131,1.13389822901303,1.13348223894569))
REPRESENTATION_ITEM('')
);
#1243=(
BOUNDED_CURVE()
B_SPLINE_CURVE(2,(#70576,#70577,#70578),.UNSPECIFIED.,.F.,.F.)
B_SPLINE_CURVE_WITH_KNOTS((3,3),(0.271548216895914,0.2777342275319),
 .UNSPECIFIED.)
CURVE()
GEOMETRIC_REPRESENTATION_ITEM()
RATIONAL_B_SPLINE_CURVE((1.13348223894616,1.13389822901351,1.13426390111358))
REPRESENTATION_ITEM('')
);
#1244=(
BOUNDED_CURVE()
B_SPLINE_CURVE(2,(#70582,#70583,#70584),.UNSPECIFIED.,.F.,.F.)
B_SPLINE_CURVE_WITH_KNOTS((3,3),(0.367644516946557,0.373830527582536),
 .UNSPECIFIED.)
CURVE()
GEOMETRIC_REPRESENTATION_ITEM()
RATIONAL_B_SPLINE_CURVE((1.13426390111309,1.13389822901303,1.13348223894568))
REPRESENTATION_ITEM('')
);
#1245=(
BOUNDED_CURVE()
B_SPLINE_CURVE(2,(#70588,#70589,#70590),.UNSPECIFIED.,.F.,.F.)
B_SPLINE_CURVE_WITH_KNOTS((3,3),(0.271548216895912,0.277734227531897),
 .UNSPECIFIED.)
CURVE()
GEOMETRIC_REPRESENTATION_ITEM()
RATIONAL_B_SPLINE_CURVE((1.13348223894616,1.13389822901351,1.13426390111358))
REPRESENTATION_ITEM('')
);
#1246=(
BOUNDED_CURVE()
B_SPLINE_CURVE(2,(#70594,#70595,#70596),.UNSPECIFIED.,.F.,.F.)
B_SPLINE_CURVE_WITH_KNOTS((3,3),(0.367644516946558,0.373830527582532),
 .UNSPECIFIED.)
CURVE()
GEOMETRIC_REPRESENTATION_ITEM()
RATIONAL_B_SPLINE_CURVE((1.13426390111307,1.13389822901301,1.13348223894566))
REPRESENTATION_ITEM('')
);
#1247=(
BOUNDED_CURVE()
B_SPLINE_CURVE(2,(#70600,#70601,#70602),.UNSPECIFIED.,.F.,.F.)
B_SPLINE_CURVE_WITH_KNOTS((3,3),(0.271548216895914,0.277734227531905),
 .UNSPECIFIED.)
CURVE()
GEOMETRIC_REPRESENTATION_ITEM()
RATIONAL_B_SPLINE_CURVE((1.13348223894616,1.13389822901351,1.13426390111358))
REPRESENTATION_ITEM('')
);
#1248=(
BOUNDED_CURVE()
B_SPLINE_CURVE(2,(#70606,#70607,#70608),.UNSPECIFIED.,.F.,.F.)
B_SPLINE_CURVE_WITH_KNOTS((3,3),(0.367644516946569,0.373830527582539),
 .UNSPECIFIED.)
CURVE()
GEOMETRIC_REPRESENTATION_ITEM()
RATIONAL_B_SPLINE_CURVE((1.13426390111301,1.13389822901295,1.1334822389456))
REPRESENTATION_ITEM('')
);
#1249=(
BOUNDED_CURVE()
B_SPLINE_CURVE(2,(#70612,#70613,#70614),.UNSPECIFIED.,.F.,.F.)
B_SPLINE_CURVE_WITH_KNOTS((3,3),(0.271548216895913,0.2777342275319),
 .UNSPECIFIED.)
CURVE()
GEOMETRIC_REPRESENTATION_ITEM()
RATIONAL_B_SPLINE_CURVE((1.13348223894614,1.13389822901349,1.13426390111356))
REPRESENTATION_ITEM('')
);
#1250=(
BOUNDED_CURVE()
B_SPLINE_CURVE(2,(#70618,#70619,#70620),.UNSPECIFIED.,.F.,.F.)
B_SPLINE_CURVE_WITH_KNOTS((3,3),(0.367644516946566,0.373830527582539),
 .UNSPECIFIED.)
CURVE()
GEOMETRIC_REPRESENTATION_ITEM()
RATIONAL_B_SPLINE_CURVE((1.13426390111297,1.1338982290129,1.13348223894556))
REPRESENTATION_ITEM('')
);
#1251=(
BOUNDED_CURVE()
B_SPLINE_CURVE(2,(#70624,#70625,#70626),.UNSPECIFIED.,.F.,.F.)
B_SPLINE_CURVE_WITH_KNOTS((3,3),(0.271548216895926,0.277734227531904),
 .UNSPECIFIED.)
CURVE()
GEOMETRIC_REPRESENTATION_ITEM()
RATIONAL_B_SPLINE_CURVE((1.13348223894627,1.13389822901362,1.1342639011137))
REPRESENTATION_ITEM('')
);
#1252=(
BOUNDED_CURVE()
B_SPLINE_CURVE(2,(#70630,#70631,#70632),.UNSPECIFIED.,.F.,.F.)
B_SPLINE_CURVE_WITH_KNOTS((3,3),(0.367644516946557,0.373830527582532),
 .UNSPECIFIED.)
CURVE()
GEOMETRIC_REPRESENTATION_ITEM()
RATIONAL_B_SPLINE_CURVE((1.13426390111306,1.13389822901299,1.13348223894565))
REPRESENTATION_ITEM('')
);
#1253=(
BOUNDED_CURVE()
B_SPLINE_CURVE(2,(#70636,#70637,#70638),.UNSPECIFIED.,.F.,.F.)
B_SPLINE_CURVE_WITH_KNOTS((3,3),(0.271548216895913,0.277734227531899),
 .UNSPECIFIED.)
CURVE()
GEOMETRIC_REPRESENTATION_ITEM()
RATIONAL_B_SPLINE_CURVE((1.13348223894618,1.13389822901353,1.13426390111361))
REPRESENTATION_ITEM('')
);
#1254=(
BOUNDED_CURVE()
B_SPLINE_CURVE(2,(#70642,#70643,#70644),.UNSPECIFIED.,.F.,.F.)
B_SPLINE_CURVE_WITH_KNOTS((3,3),(0.367644516946561,0.373830527582535),
 .UNSPECIFIED.)
CURVE()
GEOMETRIC_REPRESENTATION_ITEM()
RATIONAL_B_SPLINE_CURVE((1.13426390111305,1.13389822901298,1.13348223894564))
REPRESENTATION_ITEM('')
);
#1255=(
BOUNDED_CURVE()
B_SPLINE_CURVE(2,(#70648,#70649,#70650),.UNSPECIFIED.,.F.,.F.)
B_SPLINE_CURVE_WITH_KNOTS((3,3),(0.271548216895915,0.277734227531905),
 .UNSPECIFIED.)
CURVE()
GEOMETRIC_REPRESENTATION_ITEM()
RATIONAL_B_SPLINE_CURVE((1.13348223894613,1.13389822901348,1.13426390111356))
REPRESENTATION_ITEM('')
);
#1256=(
BOUNDED_CURVE()
B_SPLINE_CURVE(2,(#70654,#70655,#70656),.UNSPECIFIED.,.F.,.F.)
B_SPLINE_CURVE_WITH_KNOTS((3,3),(0.367644516946559,0.373830527582528),
 .UNSPECIFIED.)
CURVE()
GEOMETRIC_REPRESENTATION_ITEM()
RATIONAL_B_SPLINE_CURVE((1.13426390111303,1.13389822901297,1.13348223894562))
REPRESENTATION_ITEM('')
);
#1257=(
BOUNDED_CURVE()
B_SPLINE_CURVE(2,(#70660,#70661,#70662),.UNSPECIFIED.,.F.,.F.)
B_SPLINE_CURVE_WITH_KNOTS((3,3),(0.271548216895913,0.277734227531899),
 .UNSPECIFIED.)
CURVE()
GEOMETRIC_REPRESENTATION_ITEM()
RATIONAL_B_SPLINE_CURVE((1.13348223894613,1.13389822901348,1.13426390111356))
REPRESENTATION_ITEM('')
);
#1258=(
BOUNDED_CURVE()
B_SPLINE_CURVE(2,(#70666,#70667,#70668),.UNSPECIFIED.,.F.,.F.)
B_SPLINE_CURVE_WITH_KNOTS((3,3),(0.367644516946557,0.373830527582533),
 .UNSPECIFIED.)
CURVE()
GEOMETRIC_REPRESENTATION_ITEM()
RATIONAL_B_SPLINE_CURVE((1.13426390111302,1.13389822901296,1.13348223894561))
REPRESENTATION_ITEM('')
);
#1259=(
BOUNDED_CURVE()
B_SPLINE_CURVE(2,(#70672,#70673,#70674),.UNSPECIFIED.,.F.,.F.)
B_SPLINE_CURVE_WITH_KNOTS((3,3),(0.271548216895926,0.277734227531906),
 .UNSPECIFIED.)
CURVE()
GEOMETRIC_REPRESENTATION_ITEM()
RATIONAL_B_SPLINE_CURVE((1.13348223894624,1.13389822901359,1.13426390111366))
REPRESENTATION_ITEM('')
);
#1260=(
BOUNDED_CURVE()
B_SPLINE_CURVE(2,(#70678,#70679,#70680),.UNSPECIFIED.,.F.,.F.)
B_SPLINE_CURVE_WITH_KNOTS((3,3),(0.367644516946561,0.373830527582536),
 .UNSPECIFIED.)
CURVE()
GEOMETRIC_REPRESENTATION_ITEM()
RATIONAL_B_SPLINE_CURVE((1.13426390111306,1.13389822901299,1.13348223894564))
REPRESENTATION_ITEM('')
);
#1261=(
BOUNDED_CURVE()
B_SPLINE_CURVE(2,(#70684,#70685,#70686),.UNSPECIFIED.,.F.,.F.)
B_SPLINE_CURVE_WITH_KNOTS((3,3),(0.271548216895911,0.277734227531901),
 .UNSPECIFIED.)
CURVE()
GEOMETRIC_REPRESENTATION_ITEM()
RATIONAL_B_SPLINE_CURVE((1.13348223894609,1.13389822901344,1.13426390111352))
REPRESENTATION_ITEM('')
);
#1262=(
BOUNDED_CURVE()
B_SPLINE_CURVE(2,(#70690,#70691,#70692),.UNSPECIFIED.,.F.,.F.)
B_SPLINE_CURVE_WITH_KNOTS((3,3),(0.367644516946558,0.373830527582533),
 .UNSPECIFIED.)
CURVE()
GEOMETRIC_REPRESENTATION_ITEM()
RATIONAL_B_SPLINE_CURVE((1.1342639011131,1.13389822901303,1.13348223894569))
REPRESENTATION_ITEM('')
);
#1263=(
BOUNDED_CURVE()
B_SPLINE_CURVE(2,(#70696,#70697,#70698),.UNSPECIFIED.,.F.,.F.)
B_SPLINE_CURVE_WITH_KNOTS((3,3),(0.271548216895922,0.277734227531909),
 .UNSPECIFIED.)
CURVE()
GEOMETRIC_REPRESENTATION_ITEM()
RATIONAL_B_SPLINE_CURVE((1.13348223894623,1.13389822901358,1.13426390111366))
REPRESENTATION_ITEM('')
);
#1264=(
BOUNDED_CURVE()
B_SPLINE_CURVE(2,(#70702,#70703,#70704),.UNSPECIFIED.,.F.,.F.)
B_SPLINE_CURVE_WITH_KNOTS((3,3),(0.367644516946562,0.373830527582538),
 .UNSPECIFIED.)
CURVE()
GEOMETRIC_REPRESENTATION_ITEM()
RATIONAL_B_SPLINE_CURVE((1.13426390111305,1.13389822901298,1.13348223894563))
REPRESENTATION_ITEM('')
);
#1265=(
BOUNDED_CURVE()
B_SPLINE_CURVE(2,(#70708,#70709,#70710),.UNSPECIFIED.,.F.,.F.)
B_SPLINE_CURVE_WITH_KNOTS((3,3),(0.271548216895906,0.277734227531898),
 .UNSPECIFIED.)
CURVE()
GEOMETRIC_REPRESENTATION_ITEM()
RATIONAL_B_SPLINE_CURVE((1.13348223894604,1.13389822901339,1.13426390111346))
REPRESENTATION_ITEM('')
);
#1266=(
BOUNDED_CURVE()
B_SPLINE_CURVE(2,(#70714,#70715,#70716),.UNSPECIFIED.,.F.,.F.)
B_SPLINE_CURVE_WITH_KNOTS((3,3),(0.367644516946563,0.373830527582537),
 .UNSPECIFIED.)
CURVE()
GEOMETRIC_REPRESENTATION_ITEM()
RATIONAL_B_SPLINE_CURVE((1.134263901113,1.13389822901294,1.13348223894559))
REPRESENTATION_ITEM('')
);
#1267=(
BOUNDED_CURVE()
B_SPLINE_CURVE(2,(#70720,#70721,#70722),.UNSPECIFIED.,.F.,.F.)
B_SPLINE_CURVE_WITH_KNOTS((3,3),(0.271548216895914,0.277734227531897),
 .UNSPECIFIED.)
CURVE()
GEOMETRIC_REPRESENTATION_ITEM()
RATIONAL_B_SPLINE_CURVE((1.13348223894613,1.13389822901348,1.13426390111355))
REPRESENTATION_ITEM('')
);
#1268=(
BOUNDED_CURVE()
B_SPLINE_CURVE(2,(#70726,#70727,#70728),.UNSPECIFIED.,.F.,.F.)
B_SPLINE_CURVE_WITH_KNOTS((3,3),(0.367644516946558,0.373830527582532),
 .UNSPECIFIED.)
CURVE()
GEOMETRIC_REPRESENTATION_ITEM()
RATIONAL_B_SPLINE_CURVE((1.13426390111307,1.133898229013,1.13348223894566))
REPRESENTATION_ITEM('')
);
#1269=(
BOUNDED_CURVE()
B_SPLINE_CURVE(2,(#70732,#70733,#70734),.UNSPECIFIED.,.F.,.F.)
B_SPLINE_CURVE_WITH_KNOTS((3,3),(0.271548216895917,0.277734227531901),
 .UNSPECIFIED.)
CURVE()
GEOMETRIC_REPRESENTATION_ITEM()
RATIONAL_B_SPLINE_CURVE((1.13348223894616,1.1338982290135,1.13426390111358))
REPRESENTATION_ITEM('')
);
#1270=(
BOUNDED_CURVE()
B_SPLINE_CURVE(2,(#70738,#70739,#70740),.UNSPECIFIED.,.F.,.F.)
B_SPLINE_CURVE_WITH_KNOTS((3,3),(0.367644516946556,0.37383052758253),
 .UNSPECIFIED.)
CURVE()
GEOMETRIC_REPRESENTATION_ITEM()
RATIONAL_B_SPLINE_CURVE((1.13426390111304,1.13389822901297,1.13348223894563))
REPRESENTATION_ITEM('')
);
#1271=(
BOUNDED_CURVE()
B_SPLINE_CURVE(2,(#70744,#70745,#70746),.UNSPECIFIED.,.F.,.F.)
B_SPLINE_CURVE_WITH_KNOTS((3,3),(0.271548216895911,0.277734227531893),
 .UNSPECIFIED.)
CURVE()
GEOMETRIC_REPRESENTATION_ITEM()
RATIONAL_B_SPLINE_CURVE((1.13348223894607,1.13389822901342,1.13426390111349))
REPRESENTATION_ITEM('')
);
#1272=(
BOUNDED_CURVE()
B_SPLINE_CURVE(2,(#70750,#70751,#70752),.UNSPECIFIED.,.F.,.F.)
B_SPLINE_CURVE_WITH_KNOTS((3,3),(0.367644516946565,0.373830527582539),
 .UNSPECIFIED.)
CURVE()
GEOMETRIC_REPRESENTATION_ITEM()
RATIONAL_B_SPLINE_CURVE((1.13426390111301,1.13389822901295,1.1334822389456))
REPRESENTATION_ITEM('')
);
#1273=(
BOUNDED_CURVE()
B_SPLINE_CURVE(2,(#70756,#70757,#70758),.UNSPECIFIED.,.F.,.F.)
B_SPLINE_CURVE_WITH_KNOTS((3,3),(0.271548216895916,0.277734227531897),
 .UNSPECIFIED.)
CURVE()
GEOMETRIC_REPRESENTATION_ITEM()
RATIONAL_B_SPLINE_CURVE((1.13348223894613,1.13389822901348,1.13426390111355))
REPRESENTATION_ITEM('')
);
#1274=(
BOUNDED_CURVE()
B_SPLINE_CURVE(2,(#70762,#70763,#70764),.UNSPECIFIED.,.F.,.F.)
B_SPLINE_CURVE_WITH_KNOTS((3,3),(0.36764451694656,0.373830527582534),
 .UNSPECIFIED.)
CURVE()
GEOMETRIC_REPRESENTATION_ITEM()
RATIONAL_B_SPLINE_CURVE((1.13426390111306,1.13389822901299,1.13348223894564))
REPRESENTATION_ITEM('')
);
#1275=(
BOUNDED_CURVE()
B_SPLINE_CURVE(2,(#70768,#70769,#70770),.UNSPECIFIED.,.F.,.F.)
B_SPLINE_CURVE_WITH_KNOTS((3,3),(0.271548216895918,0.277734227531904),
 .UNSPECIFIED.)
CURVE()
GEOMETRIC_REPRESENTATION_ITEM()
RATIONAL_B_SPLINE_CURVE((1.13348223894613,1.13389822901348,1.13426390111355))
REPRESENTATION_ITEM('')
);
#1276=(
BOUNDED_CURVE()
B_SPLINE_CURVE(2,(#70774,#70775,#70776),.UNSPECIFIED.,.F.,.F.)
B_SPLINE_CURVE_WITH_KNOTS((3,3),(0.367644516946555,0.373830527582533),
 .UNSPECIFIED.)
CURVE()
GEOMETRIC_REPRESENTATION_ITEM()
RATIONAL_B_SPLINE_CURVE((1.13426390111305,1.13389822901298,1.13348223894564))
REPRESENTATION_ITEM('')
);
#1277=(
BOUNDED_CURVE()
B_SPLINE_CURVE(2,(#70780,#70781,#70782),.UNSPECIFIED.,.F.,.F.)
B_SPLINE_CURVE_WITH_KNOTS((3,3),(0.271548216895928,0.277734227531916),
 .UNSPECIFIED.)
CURVE()
GEOMETRIC_REPRESENTATION_ITEM()
RATIONAL_B_SPLINE_CURVE((1.13348223894621,1.13389822901356,1.13426390111363))
REPRESENTATION_ITEM('')
);
#1278=(
BOUNDED_CURVE()
B_SPLINE_CURVE(2,(#70786,#70787,#70788),.UNSPECIFIED.,.F.,.F.)
B_SPLINE_CURVE_WITH_KNOTS((3,3),(0.367644516946548,0.373830527582523),
 .UNSPECIFIED.)
CURVE()
GEOMETRIC_REPRESENTATION_ITEM()
RATIONAL_B_SPLINE_CURVE((1.13426390111312,1.13389822901305,1.13348223894571))
REPRESENTATION_ITEM('')
);
#1279=(
BOUNDED_CURVE()
B_SPLINE_CURVE(2,(#70792,#70793,#70794),.UNSPECIFIED.,.F.,.F.)
B_SPLINE_CURVE_WITH_KNOTS((3,3),(0.271548216895918,0.277734227531905),
 .UNSPECIFIED.)
CURVE()
GEOMETRIC_REPRESENTATION_ITEM()
RATIONAL_B_SPLINE_CURVE((1.13348223894611,1.13389822901346,1.13426390111354))
REPRESENTATION_ITEM('')
);
#1280=(
BOUNDED_CURVE()
B_SPLINE_CURVE(2,(#70798,#70799,#70800),.UNSPECIFIED.,.F.,.F.)
B_SPLINE_CURVE_WITH_KNOTS((3,3),(0.367644516946559,0.373830527582532),
 .UNSPECIFIED.)
CURVE()
GEOMETRIC_REPRESENTATION_ITEM()
RATIONAL_B_SPLINE_CURVE((1.13426390111305,1.13389822901298,1.13348223894564))
REPRESENTATION_ITEM('')
);
#1281=(
BOUNDED_CURVE()
B_SPLINE_CURVE(2,(#70804,#70805,#70806),.UNSPECIFIED.,.F.,.F.)
B_SPLINE_CURVE_WITH_KNOTS((3,3),(0.271548216895915,0.277734227531901),
 .UNSPECIFIED.)
CURVE()
GEOMETRIC_REPRESENTATION_ITEM()
RATIONAL_B_SPLINE_CURVE((1.13348223894615,1.1338982290135,1.13426390111357))
REPRESENTATION_ITEM('')
);
#1282=(
BOUNDED_CURVE()
B_SPLINE_CURVE(2,(#70810,#70811,#70812),.UNSPECIFIED.,.F.,.F.)
B_SPLINE_CURVE_WITH_KNOTS((3,3),(0.367644516946548,0.373830527582526),
 .UNSPECIFIED.)
CURVE()
GEOMETRIC_REPRESENTATION_ITEM()
RATIONAL_B_SPLINE_CURVE((1.13426390111308,1.13389822901302,1.13348223894567))
REPRESENTATION_ITEM('')
);
#1283=(
BOUNDED_CURVE()
B_SPLINE_CURVE(2,(#70816,#70817,#70818),.UNSPECIFIED.,.F.,.F.)
B_SPLINE_CURVE_WITH_KNOTS((3,3),(0.271548216895917,0.277734227531902),
 .UNSPECIFIED.)
CURVE()
GEOMETRIC_REPRESENTATION_ITEM()
RATIONAL_B_SPLINE_CURVE((1.13348223894615,1.1338982290135,1.13426390111358))
REPRESENTATION_ITEM('')
);
#1284=(
BOUNDED_CURVE()
B_SPLINE_CURVE(2,(#70822,#70823,#70824),.UNSPECIFIED.,.F.,.F.)
B_SPLINE_CURVE_WITH_KNOTS((3,3),(0.367644516946561,0.373830527582534),
 .UNSPECIFIED.)
CURVE()
GEOMETRIC_REPRESENTATION_ITEM()
RATIONAL_B_SPLINE_CURVE((1.13426390111303,1.13389822901296,1.13348223894562))
REPRESENTATION_ITEM('')
);
#1285=(
BOUNDED_CURVE()
B_SPLINE_CURVE(2,(#70828,#70829,#70830),.UNSPECIFIED.,.F.,.F.)
B_SPLINE_CURVE_WITH_KNOTS((3,3),(0.271548216895922,0.277734227531908),
 .UNSPECIFIED.)
CURVE()
GEOMETRIC_REPRESENTATION_ITEM()
RATIONAL_B_SPLINE_CURVE((1.13348223894617,1.13389822901352,1.1342639011136))
REPRESENTATION_ITEM('')
);
#1286=(
BOUNDED_CURVE()
B_SPLINE_CURVE(2,(#70834,#70835,#70836),.UNSPECIFIED.,.F.,.F.)
B_SPLINE_CURVE_WITH_KNOTS((3,3),(0.367644516946555,0.373830527582532),
 .UNSPECIFIED.)
CURVE()
GEOMETRIC_REPRESENTATION_ITEM()
RATIONAL_B_SPLINE_CURVE((1.13426390111307,1.133898229013,1.13348223894566))
REPRESENTATION_ITEM('')
);
#1287=(
BOUNDED_CURVE()
B_SPLINE_CURVE(2,(#70840,#70841,#70842),.UNSPECIFIED.,.F.,.F.)
B_SPLINE_CURVE_WITH_KNOTS((3,3),(0.27154821689592,0.277734227531907),
 .UNSPECIFIED.)
CURVE()
GEOMETRIC_REPRESENTATION_ITEM()
RATIONAL_B_SPLINE_CURVE((1.13348223894614,1.13389822901349,1.13426390111356))
REPRESENTATION_ITEM('')
);
#1288=(
BOUNDED_CURVE()
B_SPLINE_CURVE(2,(#70846,#70847,#70848),.UNSPECIFIED.,.F.,.F.)
B_SPLINE_CURVE_WITH_KNOTS((3,3),(0.367644516946564,0.373830527582538),
 .UNSPECIFIED.)
CURVE()
GEOMETRIC_REPRESENTATION_ITEM()
RATIONAL_B_SPLINE_CURVE((1.13426390111299,1.13389822901292,1.13348223894557))
REPRESENTATION_ITEM('')
);
#1289=(
BOUNDED_CURVE()
B_SPLINE_CURVE(2,(#70852,#70853,#70854),.UNSPECIFIED.,.F.,.F.)
B_SPLINE_CURVE_WITH_KNOTS((3,3),(0.271548216895926,0.277734227531912),
 .UNSPECIFIED.)
CURVE()
GEOMETRIC_REPRESENTATION_ITEM()
RATIONAL_B_SPLINE_CURVE((1.13348223894617,1.13389822901352,1.13426390111359))
REPRESENTATION_ITEM('')
);
#1290=(
BOUNDED_CURVE()
B_SPLINE_CURVE(2,(#70858,#70859,#70860),.UNSPECIFIED.,.F.,.F.)
B_SPLINE_CURVE_WITH_KNOTS((3,3),(0.367644516946548,0.373830527582525),
 .UNSPECIFIED.)
CURVE()
GEOMETRIC_REPRESENTATION_ITEM()
RATIONAL_B_SPLINE_CURVE((1.13426390111308,1.13389822901301,1.13348223894567))
REPRESENTATION_ITEM('')
);
#1291=(
BOUNDED_CURVE()
B_SPLINE_CURVE(2,(#70864,#70865,#70866),.UNSPECIFIED.,.F.,.F.)
B_SPLINE_CURVE_WITH_KNOTS((3,3),(0.271548216895921,0.277734227531907),
 .UNSPECIFIED.)
CURVE()
GEOMETRIC_REPRESENTATION_ITEM()
RATIONAL_B_SPLINE_CURVE((1.13348223894617,1.13389822901352,1.13426390111359))
REPRESENTATION_ITEM('')
);
#1292=(
BOUNDED_CURVE()
B_SPLINE_CURVE(2,(#70870,#70871,#70872),.UNSPECIFIED.,.F.,.F.)
B_SPLINE_CURVE_WITH_KNOTS((3,3),(0.367644516946557,0.373830527582527),
 .UNSPECIFIED.)
CURVE()
GEOMETRIC_REPRESENTATION_ITEM()
RATIONAL_B_SPLINE_CURVE((1.1342639011131,1.13389822901303,1.13348223894569))
REPRESENTATION_ITEM('')
);
#1293=(
BOUNDED_CURVE()
B_SPLINE_CURVE(2,(#70875,#70876,#70877),.UNSPECIFIED.,.F.,.F.)
B_SPLINE_CURVE_WITH_KNOTS((3,3),(0.271548216895922,0.277734227531908),
 .UNSPECIFIED.)
CURVE()
GEOMETRIC_REPRESENTATION_ITEM()
RATIONAL_B_SPLINE_CURVE((1.13348223894615,1.1338982290135,1.13426390111358))
REPRESENTATION_ITEM('')
);
#1294=(
BOUNDED_CURVE()
B_SPLINE_CURVE(2,(#70879,#70880,#70881),.UNSPECIFIED.,.F.,.F.)
B_SPLINE_CURVE_WITH_KNOTS((3,3),(0.367644516946556,0.373830527582529),
 .UNSPECIFIED.)
CURVE()
GEOMETRIC_REPRESENTATION_ITEM()
RATIONAL_B_SPLINE_CURVE((1.13426390111308,1.13389822901301,1.13348223894567))
REPRESENTATION_ITEM('')
);
#1295=(
BOUNDED_CURVE()
B_SPLINE_CURVE(2,(#70884,#70885,#70886),.UNSPECIFIED.,.F.,.F.)
B_SPLINE_CURVE_WITH_KNOTS((3,3),(0.271548216895921,0.277734227531909),
 .UNSPECIFIED.)
CURVE()
GEOMETRIC_REPRESENTATION_ITEM()
RATIONAL_B_SPLINE_CURVE((1.13348223894619,1.13389822901354,1.13426390111361))
REPRESENTATION_ITEM('')
);
#1296=(
BOUNDED_CURVE()
B_SPLINE_CURVE(2,(#70888,#70889,#70890),.UNSPECIFIED.,.F.,.F.)
B_SPLINE_CURVE_WITH_KNOTS((3,3),(0.36764451694656,0.37383052758253),
 .UNSPECIFIED.)
CURVE()
GEOMETRIC_REPRESENTATION_ITEM()
RATIONAL_B_SPLINE_CURVE((1.13426390111303,1.13389822901296,1.13348223894562))
REPRESENTATION_ITEM('')
);
#1297=(
BOUNDED_CURVE()
B_SPLINE_CURVE(2,(#70893,#70894,#70895),.UNSPECIFIED.,.F.,.F.)
B_SPLINE_CURVE_WITH_KNOTS((3,3),(0.271548216895921,0.277734227531907),
 .UNSPECIFIED.)
CURVE()
GEOMETRIC_REPRESENTATION_ITEM()
RATIONAL_B_SPLINE_CURVE((1.13348223894618,1.13389822901353,1.1342639011136))
REPRESENTATION_ITEM('')
);
#1298=(
BOUNDED_CURVE()
B_SPLINE_CURVE(2,(#70897,#70898,#70899),.UNSPECIFIED.,.F.,.F.)
B_SPLINE_CURVE_WITH_KNOTS((3,3),(0.367644516946553,0.373830527582534),
 .UNSPECIFIED.)
CURVE()
GEOMETRIC_REPRESENTATION_ITEM()
RATIONAL_B_SPLINE_CURVE((1.13426390111306,1.13389822901299,1.13348223894565))
REPRESENTATION_ITEM('')
);
#1299=(
BOUNDED_CURVE()
B_SPLINE_CURVE(2,(#70902,#70903,#70904),.UNSPECIFIED.,.F.,.F.)
B_SPLINE_CURVE_WITH_KNOTS((3,3),(0.271548216895916,0.277734227531903),
 .UNSPECIFIED.)
CURVE()
GEOMETRIC_REPRESENTATION_ITEM()
RATIONAL_B_SPLINE_CURVE((1.13348223894615,1.1338982290135,1.13426390111357))
REPRESENTATION_ITEM('')
);
#1300=(
BOUNDED_CURVE()
B_SPLINE_CURVE(2,(#70906,#70907,#70908),.UNSPECIFIED.,.F.,.F.)
B_SPLINE_CURVE_WITH_KNOTS((3,3),(0.367644516946558,0.373830527582532),
 .UNSPECIFIED.)
CURVE()
GEOMETRIC_REPRESENTATION_ITEM()
RATIONAL_B_SPLINE_CURVE((1.13426390111307,1.13389822901301,1.13348223894566))
REPRESENTATION_ITEM('')
);
#1301=(
BOUNDED_CURVE()
B_SPLINE_CURVE(2,(#70911,#70912,#70913),.UNSPECIFIED.,.F.,.F.)
B_SPLINE_CURVE_WITH_KNOTS((3,3),(0.271548216895911,0.277734227531895),
 .UNSPECIFIED.)
CURVE()
GEOMETRIC_REPRESENTATION_ITEM()
RATIONAL_B_SPLINE_CURVE((1.13348223894606,1.13389822901341,1.13426390111348))
REPRESENTATION_ITEM('')
);
#1302=(
BOUNDED_CURVE()
B_SPLINE_CURVE(2,(#70915,#70916,#70917),.UNSPECIFIED.,.F.,.F.)
B_SPLINE_CURVE_WITH_KNOTS((3,3),(0.367644516946553,0.373830527582531),
 .UNSPECIFIED.)
CURVE()
GEOMETRIC_REPRESENTATION_ITEM()
RATIONAL_B_SPLINE_CURVE((1.13426390111307,1.133898229013,1.13348223894566))
REPRESENTATION_ITEM('')
);
#1303=(
BOUNDED_CURVE()
B_SPLINE_CURVE(2,(#70920,#70921,#70922),.UNSPECIFIED.,.F.,.F.)
B_SPLINE_CURVE_WITH_KNOTS((3,3),(0.271548216895918,0.277734227531903),
 .UNSPECIFIED.)
CURVE()
GEOMETRIC_REPRESENTATION_ITEM()
RATIONAL_B_SPLINE_CURVE((1.13348223894611,1.13389822901346,1.13426390111353))
REPRESENTATION_ITEM('')
);
#1304=(
BOUNDED_CURVE()
B_SPLINE_CURVE(2,(#70924,#70925,#70926),.UNSPECIFIED.,.F.,.F.)
B_SPLINE_CURVE_WITH_KNOTS((3,3),(0.367644516946551,0.373830527582526),
 .UNSPECIFIED.)
CURVE()
GEOMETRIC_REPRESENTATION_ITEM()
RATIONAL_B_SPLINE_CURVE((1.1342639011131,1.13389822901304,1.13348223894569))
REPRESENTATION_ITEM('')
);
#1305=(
BOUNDED_CURVE()
B_SPLINE_CURVE(2,(#70929,#70930,#70931),.UNSPECIFIED.,.F.,.F.)
B_SPLINE_CURVE_WITH_KNOTS((3,3),(0.271548216895922,0.277734227531909),
 .UNSPECIFIED.)
CURVE()
GEOMETRIC_REPRESENTATION_ITEM()
RATIONAL_B_SPLINE_CURVE((1.13348223894615,1.1338982290135,1.13426390111357))
REPRESENTATION_ITEM('')
);
#1306=(
BOUNDED_CURVE()
B_SPLINE_CURVE(2,(#70933,#70934,#70935),.UNSPECIFIED.,.F.,.F.)
B_SPLINE_CURVE_WITH_KNOTS((3,3),(0.36764451694656,0.373830527582534),
 .UNSPECIFIED.)
CURVE()
GEOMETRIC_REPRESENTATION_ITEM()
RATIONAL_B_SPLINE_CURVE((1.13426390111304,1.13389822901297,1.13348223894563))
REPRESENTATION_ITEM('')
);
#1307=(
BOUNDED_CURVE()
B_SPLINE_CURVE(2,(#70938,#70939,#70940),.UNSPECIFIED.,.F.,.F.)
B_SPLINE_CURVE_WITH_KNOTS((3,3),(0.271548216895917,0.277734227531904),
 .UNSPECIFIED.)
CURVE()
GEOMETRIC_REPRESENTATION_ITEM()
RATIONAL_B_SPLINE_CURVE((1.13348223894616,1.13389822901351,1.13426390111359))
REPRESENTATION_ITEM('')
);
#1308=(
BOUNDED_CURVE()
B_SPLINE_CURVE(2,(#70942,#70943,#70944),.UNSPECIFIED.,.F.,.F.)
B_SPLINE_CURVE_WITH_KNOTS((3,3),(0.367644516946562,0.373830527582537),
 .UNSPECIFIED.)
CURVE()
GEOMETRIC_REPRESENTATION_ITEM()
RATIONAL_B_SPLINE_CURVE((1.13426390111298,1.13389822901291,1.13348223894556))
REPRESENTATION_ITEM('')
);
#1309=(
BOUNDED_CURVE()
B_SPLINE_CURVE(2,(#70947,#70948,#70949),.UNSPECIFIED.,.F.,.F.)
B_SPLINE_CURVE_WITH_KNOTS((3,3),(0.271548216895925,0.277734227531911),
 .UNSPECIFIED.)
CURVE()
GEOMETRIC_REPRESENTATION_ITEM()
RATIONAL_B_SPLINE_CURVE((1.13348223894616,1.13389822901351,1.13426390111359))
REPRESENTATION_ITEM('')
);
#1310=(
BOUNDED_CURVE()
B_SPLINE_CURVE(2,(#70951,#70952,#70953),.UNSPECIFIED.,.F.,.F.)
B_SPLINE_CURVE_WITH_KNOTS((3,3),(0.367644516946555,0.373830527582529),
 .UNSPECIFIED.)
CURVE()
GEOMETRIC_REPRESENTATION_ITEM()
RATIONAL_B_SPLINE_CURVE((1.13426390111312,1.13389822901305,1.13348223894571))
REPRESENTATION_ITEM('')
);
#1311=(
BOUNDED_CURVE()
B_SPLINE_CURVE(2,(#70956,#70957,#70958),.UNSPECIFIED.,.F.,.F.)
B_SPLINE_CURVE_WITH_KNOTS((3,3),(0.271548216895925,0.277734227531912),
 .UNSPECIFIED.)
CURVE()
GEOMETRIC_REPRESENTATION_ITEM()
RATIONAL_B_SPLINE_CURVE((1.13348223894618,1.13389822901353,1.1342639011136))
REPRESENTATION_ITEM('')
);
#1312=(
BOUNDED_CURVE()
B_SPLINE_CURVE(2,(#70960,#70961,#70962),.UNSPECIFIED.,.F.,.F.)
B_SPLINE_CURVE_WITH_KNOTS((3,3),(0.367644516946557,0.373830527582532),
 .UNSPECIFIED.)
CURVE()
GEOMETRIC_REPRESENTATION_ITEM()
RATIONAL_B_SPLINE_CURVE((1.13426390111306,1.13389822901299,1.13348223894564))
REPRESENTATION_ITEM('')
);
#1313=(
BOUNDED_CURVE()
B_SPLINE_CURVE(2,(#70965,#70966,#70967),.UNSPECIFIED.,.F.,.F.)
B_SPLINE_CURVE_WITH_KNOTS((3,3),(0.271548216895908,0.277734227531892),
 .UNSPECIFIED.)
CURVE()
GEOMETRIC_REPRESENTATION_ITEM()
RATIONAL_B_SPLINE_CURVE((1.13348223894609,1.13389822901344,1.13426390111352))
REPRESENTATION_ITEM('')
);
#1314=(
BOUNDED_CURVE()
B_SPLINE_CURVE(2,(#70969,#70970,#70971),.UNSPECIFIED.,.F.,.F.)
B_SPLINE_CURVE_WITH_KNOTS((3,3),(0.367644516946557,0.373830527582522),
 .UNSPECIFIED.)
CURVE()
GEOMETRIC_REPRESENTATION_ITEM()
RATIONAL_B_SPLINE_CURVE((1.13426390111309,1.13389822901302,1.13348223894568))
REPRESENTATION_ITEM('')
);
#1315=(
BOUNDED_CURVE()
B_SPLINE_CURVE(2,(#70974,#70975,#70976),.UNSPECIFIED.,.F.,.F.)
B_SPLINE_CURVE_WITH_KNOTS((3,3),(0.271548216895913,0.277734227531902),
 .UNSPECIFIED.)
CURVE()
GEOMETRIC_REPRESENTATION_ITEM()
RATIONAL_B_SPLINE_CURVE((1.1334822389461,1.13389822901345,1.13426390111352))
REPRESENTATION_ITEM('')
);
#1316=(
BOUNDED_CURVE()
B_SPLINE_CURVE(2,(#70978,#70979,#70980),.UNSPECIFIED.,.F.,.F.)
B_SPLINE_CURVE_WITH_KNOTS((3,3),(0.367644516946559,0.373830527582539),
 .UNSPECIFIED.)
CURVE()
GEOMETRIC_REPRESENTATION_ITEM()
RATIONAL_B_SPLINE_CURVE((1.13426390111296,1.13389822901289,1.13348223894555))
REPRESENTATION_ITEM('')
);
#1317=(
BOUNDED_CURVE()
B_SPLINE_CURVE(2,(#70983,#70984,#70985),.UNSPECIFIED.,.F.,.F.)
B_SPLINE_CURVE_WITH_KNOTS((3,3),(0.271548216895926,0.277734227531913),
 .UNSPECIFIED.)
CURVE()
GEOMETRIC_REPRESENTATION_ITEM()
RATIONAL_B_SPLINE_CURVE((1.13348223894622,1.13389822901357,1.13426390111365))
REPRESENTATION_ITEM('')
);
#1318=(
BOUNDED_CURVE()
B_SPLINE_CURVE(2,(#70987,#70988,#70989),.UNSPECIFIED.,.F.,.F.)
B_SPLINE_CURVE_WITH_KNOTS((3,3),(0.36764451694656,0.373830527582534),
 .UNSPECIFIED.)
CURVE()
GEOMETRIC_REPRESENTATION_ITEM()
RATIONAL_B_SPLINE_CURVE((1.13426390111298,1.13389822901291,1.13348223894557))
REPRESENTATION_ITEM('')
);
#1319=(
BOUNDED_CURVE()
B_SPLINE_CURVE(2,(#70992,#70993,#70994),.UNSPECIFIED.,.F.,.F.)
B_SPLINE_CURVE_WITH_KNOTS((3,3),(0.271548216895926,0.277734227531909),
 .UNSPECIFIED.)
CURVE()
GEOMETRIC_REPRESENTATION_ITEM()
RATIONAL_B_SPLINE_CURVE((1.13348223894617,1.13389822901352,1.13426390111359))
REPRESENTATION_ITEM('')
);
#1320=(
BOUNDED_CURVE()
B_SPLINE_CURVE(2,(#70996,#70997,#70998),.UNSPECIFIED.,.F.,.F.)
B_SPLINE_CURVE_WITH_KNOTS((3,3),(0.367644516946566,0.373830527582539),
 .UNSPECIFIED.)
CURVE()
GEOMETRIC_REPRESENTATION_ITEM()
RATIONAL_B_SPLINE_CURVE((1.13426390111296,1.13389822901289,1.13348223894555))
REPRESENTATION_ITEM('')
);
#1321=(
BOUNDED_CURVE()
B_SPLINE_CURVE(2,(#71001,#71002,#71003),.UNSPECIFIED.,.F.,.F.)
B_SPLINE_CURVE_WITH_KNOTS((3,3),(0.271548216895918,0.277734227531904),
 .UNSPECIFIED.)
CURVE()
GEOMETRIC_REPRESENTATION_ITEM()
RATIONAL_B_SPLINE_CURVE((1.13348223894611,1.13389822901346,1.13426390111353))
REPRESENTATION_ITEM('')
);
#1322=(
BOUNDED_CURVE()
B_SPLINE_CURVE(2,(#71005,#71006,#71007),.UNSPECIFIED.,.F.,.F.)
B_SPLINE_CURVE_WITH_KNOTS((3,3),(0.367644516946555,0.373830527582529),
 .UNSPECIFIED.)
CURVE()
GEOMETRIC_REPRESENTATION_ITEM()
RATIONAL_B_SPLINE_CURVE((1.13426390111303,1.13389822901296,1.13348223894562))
REPRESENTATION_ITEM('')
);
#1323=(
BOUNDED_CURVE()
B_SPLINE_CURVE(2,(#71011,#71012,#71013),.UNSPECIFIED.,.F.,.F.)
B_SPLINE_CURVE_WITH_KNOTS((3,3),(0.271548216895927,0.277734227531913),
 .UNSPECIFIED.)
CURVE()
GEOMETRIC_REPRESENTATION_ITEM()
RATIONAL_B_SPLINE_CURVE((1.13348223894624,1.13389822901359,1.13426390111366))
REPRESENTATION_ITEM('')
);
#1324=(
BOUNDED_CURVE()
B_SPLINE_CURVE(2,(#71017,#71018,#71019),.UNSPECIFIED.,.F.,.F.)
B_SPLINE_CURVE_WITH_KNOTS((3,3),(0.367644516946557,0.373830527582527),
 .UNSPECIFIED.)
CURVE()
GEOMETRIC_REPRESENTATION_ITEM()
RATIONAL_B_SPLINE_CURVE((1.1342639011131,1.13389822901303,1.13348223894569))
REPRESENTATION_ITEM('')
);
#1325=(
BOUNDED_CURVE()
B_SPLINE_CURVE(2,(#71023,#71024,#71025),.UNSPECIFIED.,.F.,.F.)
B_SPLINE_CURVE_WITH_KNOTS((3,3),(0.27154821689592,0.277734227531904),
 .UNSPECIFIED.)
CURVE()
GEOMETRIC_REPRESENTATION_ITEM()
RATIONAL_B_SPLINE_CURVE((1.13348223894613,1.13389822901348,1.13426390111355))
REPRESENTATION_ITEM('')
);
#1326=(
BOUNDED_CURVE()
B_SPLINE_CURVE(2,(#71029,#71030,#71031),.UNSPECIFIED.,.F.,.F.)
B_SPLINE_CURVE_WITH_KNOTS((3,3),(0.367644516946566,0.373830527582538),
 .UNSPECIFIED.)
CURVE()
GEOMETRIC_REPRESENTATION_ITEM()
RATIONAL_B_SPLINE_CURVE((1.13426390111301,1.13389822901294,1.1334822389456))
REPRESENTATION_ITEM('')
);
#1327=(
BOUNDED_CURVE()
B_SPLINE_CURVE(2,(#71035,#71036,#71037),.UNSPECIFIED.,.F.,.F.)
B_SPLINE_CURVE_WITH_KNOTS((3,3),(0.27154821689592,0.277734227531902),
 .UNSPECIFIED.)
CURVE()
GEOMETRIC_REPRESENTATION_ITEM()
RATIONAL_B_SPLINE_CURVE((1.1334822389461,1.13389822901344,1.13426390111352))
REPRESENTATION_ITEM('')
);
#1328=(
BOUNDED_CURVE()
B_SPLINE_CURVE(2,(#71041,#71042,#71043),.UNSPECIFIED.,.F.,.F.)
B_SPLINE_CURVE_WITH_KNOTS((3,3),(0.367644516946558,0.373830527582536),
 .UNSPECIFIED.)
CURVE()
GEOMETRIC_REPRESENTATION_ITEM()
RATIONAL_B_SPLINE_CURVE((1.13426390111303,1.13389822901296,1.13348223894562))
REPRESENTATION_ITEM('')
);
#1329=(
BOUNDED_CURVE()
B_SPLINE_CURVE(2,(#71047,#71048,#71049),.UNSPECIFIED.,.F.,.F.)
B_SPLINE_CURVE_WITH_KNOTS((3,3),(0.271548216895916,0.277734227531903),
 .UNSPECIFIED.)
CURVE()
GEOMETRIC_REPRESENTATION_ITEM()
RATIONAL_B_SPLINE_CURVE((1.13348223894608,1.13389822901343,1.1342639011135))
REPRESENTATION_ITEM('')
);
#1330=(
BOUNDED_CURVE()
B_SPLINE_CURVE(2,(#71053,#71054,#71055),.UNSPECIFIED.,.F.,.F.)
B_SPLINE_CURVE_WITH_KNOTS((3,3),(0.367644516946558,0.373830527582538),
 .UNSPECIFIED.)
CURVE()
GEOMETRIC_REPRESENTATION_ITEM()
RATIONAL_B_SPLINE_CURVE((1.13426390111299,1.13389822901292,1.13348223894558))
REPRESENTATION_ITEM('')
);
#1331=(
BOUNDED_CURVE()
B_SPLINE_CURVE(2,(#71059,#71060,#71061),.UNSPECIFIED.,.F.,.F.)
B_SPLINE_CURVE_WITH_KNOTS((3,3),(0.271548216895918,0.277734227531905),
 .UNSPECIFIED.)
CURVE()
GEOMETRIC_REPRESENTATION_ITEM()
RATIONAL_B_SPLINE_CURVE((1.13348223894618,1.13389822901353,1.1342639011136))
REPRESENTATION_ITEM('')
);
#1332=(
BOUNDED_CURVE()
B_SPLINE_CURVE(2,(#71065,#71066,#71067),.UNSPECIFIED.,.F.,.F.)
B_SPLINE_CURVE_WITH_KNOTS((3,3),(0.367644516946549,0.373830527582523),
 .UNSPECIFIED.)
CURVE()
GEOMETRIC_REPRESENTATION_ITEM()
RATIONAL_B_SPLINE_CURVE((1.13426390111313,1.13389822901306,1.13348223894572))
REPRESENTATION_ITEM('')
);
#1333=(
BOUNDED_CURVE()
B_SPLINE_CURVE(2,(#71071,#71072,#71073),.UNSPECIFIED.,.F.,.F.)
B_SPLINE_CURVE_WITH_KNOTS((3,3),(0.271548216895918,0.277734227531904),
 .UNSPECIFIED.)
CURVE()
GEOMETRIC_REPRESENTATION_ITEM()
RATIONAL_B_SPLINE_CURVE((1.13348223894607,1.13389822901342,1.1342639011135))
REPRESENTATION_ITEM('')
);
#1334=(
BOUNDED_CURVE()
B_SPLINE_CURVE(2,(#71077,#71078,#71079),.UNSPECIFIED.,.F.,.F.)
B_SPLINE_CURVE_WITH_KNOTS((3,3),(0.367644516946553,0.373830527582525),
 .UNSPECIFIED.)
CURVE()
GEOMETRIC_REPRESENTATION_ITEM()
RATIONAL_B_SPLINE_CURVE((1.13426390111306,1.133898229013,1.13348223894565))
REPRESENTATION_ITEM('')
);
#1335=(
BOUNDED_CURVE()
B_SPLINE_CURVE(2,(#71083,#71084,#71085),.UNSPECIFIED.,.F.,.F.)
B_SPLINE_CURVE_WITH_KNOTS((3,3),(0.271548216895918,0.277734227531897),
 .UNSPECIFIED.)
CURVE()
GEOMETRIC_REPRESENTATION_ITEM()
RATIONAL_B_SPLINE_CURVE((1.13348223894613,1.13389822901348,1.13426390111355))
REPRESENTATION_ITEM('')
);
#1336=(
BOUNDED_CURVE()
B_SPLINE_CURVE(2,(#71089,#71090,#71091),.UNSPECIFIED.,.F.,.F.)
B_SPLINE_CURVE_WITH_KNOTS((3,3),(0.367644516946551,0.373830527582524),
 .UNSPECIFIED.)
CURVE()
GEOMETRIC_REPRESENTATION_ITEM()
RATIONAL_B_SPLINE_CURVE((1.13426390111309,1.13389822901302,1.13348223894568))
REPRESENTATION_ITEM('')
);
#1337=(
BOUNDED_CURVE()
B_SPLINE_CURVE(2,(#71095,#71096,#71097),.UNSPECIFIED.,.F.,.F.)
B_SPLINE_CURVE_WITH_KNOTS((3,3),(0.271548216895914,0.2777342275319),
 .UNSPECIFIED.)
CURVE()
GEOMETRIC_REPRESENTATION_ITEM()
RATIONAL_B_SPLINE_CURVE((1.13348223894608,1.13389822901343,1.13426390111351))
REPRESENTATION_ITEM('')
);
#1338=(
BOUNDED_CURVE()
B_SPLINE_CURVE(2,(#71101,#71102,#71103),.UNSPECIFIED.,.F.,.F.)
B_SPLINE_CURVE_WITH_KNOTS((3,3),(0.367644516946559,0.373830527582536),
 .UNSPECIFIED.)
CURVE()
GEOMETRIC_REPRESENTATION_ITEM()
RATIONAL_B_SPLINE_CURVE((1.13426390111305,1.13389822901298,1.13348223894564))
REPRESENTATION_ITEM('')
);
#1339=(
BOUNDED_CURVE()
B_SPLINE_CURVE(2,(#71107,#71108,#71109),.UNSPECIFIED.,.F.,.F.)
B_SPLINE_CURVE_WITH_KNOTS((3,3),(0.27154821689591,0.277734227531898),
 .UNSPECIFIED.)
CURVE()
GEOMETRIC_REPRESENTATION_ITEM()
RATIONAL_B_SPLINE_CURVE((1.13348223894607,1.13389822901342,1.1342639011135))
REPRESENTATION_ITEM('')
);
#1340=(
BOUNDED_CURVE()
B_SPLINE_CURVE(2,(#71113,#71114,#71115),.UNSPECIFIED.,.F.,.F.)
B_SPLINE_CURVE_WITH_KNOTS((3,3),(0.367644516946559,0.373830527582532),
 .UNSPECIFIED.)
CURVE()
GEOMETRIC_REPRESENTATION_ITEM()
RATIONAL_B_SPLINE_CURVE((1.13426390111307,1.133898229013,1.13348223894566))
REPRESENTATION_ITEM('')
);
#1341=(
BOUNDED_CURVE()
B_SPLINE_CURVE(2,(#71119,#71120,#71121),.UNSPECIFIED.,.F.,.F.)
B_SPLINE_CURVE_WITH_KNOTS((3,3),(0.271548216895924,0.277734227531905),
 .UNSPECIFIED.)
CURVE()
GEOMETRIC_REPRESENTATION_ITEM()
RATIONAL_B_SPLINE_CURVE((1.13348223894618,1.13389822901353,1.1342639011136))
REPRESENTATION_ITEM('')
);
#1342=(
BOUNDED_CURVE()
B_SPLINE_CURVE(2,(#71125,#71126,#71127),.UNSPECIFIED.,.F.,.F.)
B_SPLINE_CURVE_WITH_KNOTS((3,3),(0.367644516946555,0.373830527582531),
 .UNSPECIFIED.)
CURVE()
GEOMETRIC_REPRESENTATION_ITEM()
RATIONAL_B_SPLINE_CURVE((1.134263901113,1.13389822901293,1.13348223894559))
REPRESENTATION_ITEM('')
);
#1343=(
BOUNDED_CURVE()
B_SPLINE_CURVE(2,(#71131,#71132,#71133),.UNSPECIFIED.,.F.,.F.)
B_SPLINE_CURVE_WITH_KNOTS((3,3),(0.271548216895916,0.277734227531902),
 .UNSPECIFIED.)
CURVE()
GEOMETRIC_REPRESENTATION_ITEM()
RATIONAL_B_SPLINE_CURVE((1.13348223894612,1.13389822901347,1.13426390111355))
REPRESENTATION_ITEM('')
);
#1344=(
BOUNDED_CURVE()
B_SPLINE_CURVE(2,(#71137,#71138,#71139),.UNSPECIFIED.,.F.,.F.)
B_SPLINE_CURVE_WITH_KNOTS((3,3),(0.36764451694656,0.373830527582534),
 .UNSPECIFIED.)
CURVE()
GEOMETRIC_REPRESENTATION_ITEM()
RATIONAL_B_SPLINE_CURVE((1.13426390111302,1.13389822901296,1.13348223894561))
REPRESENTATION_ITEM('')
);
#1345=(
BOUNDED_CURVE()
B_SPLINE_CURVE(2,(#71143,#71144,#71145),.UNSPECIFIED.,.F.,.F.)
B_SPLINE_CURVE_WITH_KNOTS((3,3),(0.271548216895913,0.277734227531896),
 .UNSPECIFIED.)
CURVE()
GEOMETRIC_REPRESENTATION_ITEM()
RATIONAL_B_SPLINE_CURVE((1.13348223894608,1.13389822901343,1.1342639011135))
REPRESENTATION_ITEM('')
);
#1346=(
BOUNDED_CURVE()
B_SPLINE_CURVE(2,(#71149,#71150,#71151),.UNSPECIFIED.,.F.,.F.)
B_SPLINE_CURVE_WITH_KNOTS((3,3),(0.367644516946558,0.373830527582535),
 .UNSPECIFIED.)
CURVE()
GEOMETRIC_REPRESENTATION_ITEM()
RATIONAL_B_SPLINE_CURVE((1.13426390111305,1.13389822901298,1.13348223894563))
REPRESENTATION_ITEM('')
);
#1347=(
BOUNDED_CURVE()
B_SPLINE_CURVE(2,(#71155,#71156,#71157),.UNSPECIFIED.,.F.,.F.)
B_SPLINE_CURVE_WITH_KNOTS((3,3),(0.271548216895911,0.277734227531902),
 .UNSPECIFIED.)
CURVE()
GEOMETRIC_REPRESENTATION_ITEM()
RATIONAL_B_SPLINE_CURVE((1.13348223894613,1.13389822901348,1.13426390111355))
REPRESENTATION_ITEM('')
);
#1348=(
BOUNDED_CURVE()
B_SPLINE_CURVE(2,(#71161,#71162,#71163),.UNSPECIFIED.,.F.,.F.)
B_SPLINE_CURVE_WITH_KNOTS((3,3),(0.367644516946552,0.373830527582527),
 .UNSPECIFIED.)
CURVE()
GEOMETRIC_REPRESENTATION_ITEM()
RATIONAL_B_SPLINE_CURVE((1.13426390111308,1.13389822901301,1.13348223894567))
REPRESENTATION_ITEM('')
);
#1349=(
BOUNDED_CURVE()
B_SPLINE_CURVE(2,(#71167,#71168,#71169),.UNSPECIFIED.,.F.,.F.)
B_SPLINE_CURVE_WITH_KNOTS((3,3),(0.271548216895913,0.277734227531896),
 .UNSPECIFIED.)
CURVE()
GEOMETRIC_REPRESENTATION_ITEM()
RATIONAL_B_SPLINE_CURVE((1.13348223894609,1.13389822901344,1.13426390111351))
REPRESENTATION_ITEM('')
);
#1350=(
BOUNDED_CURVE()
B_SPLINE_CURVE(2,(#71173,#71174,#71175),.UNSPECIFIED.,.F.,.F.)
B_SPLINE_CURVE_WITH_KNOTS((3,3),(0.367644516946554,0.373830527582527),
 .UNSPECIFIED.)
CURVE()
GEOMETRIC_REPRESENTATION_ITEM()
RATIONAL_B_SPLINE_CURVE((1.13426390111307,1.13389822901301,1.13348223894566))
REPRESENTATION_ITEM('')
);
#1351=(
BOUNDED_CURVE()
B_SPLINE_CURVE(2,(#71179,#71180,#71181),.UNSPECIFIED.,.F.,.F.)
B_SPLINE_CURVE_WITH_KNOTS((3,3),(0.271548216895912,0.277734227531901),
 .UNSPECIFIED.)
CURVE()
GEOMETRIC_REPRESENTATION_ITEM()
RATIONAL_B_SPLINE_CURVE((1.13348223894619,1.13389822901354,1.13426390111361))
REPRESENTATION_ITEM('')
);
#1352=(
BOUNDED_CURVE()
B_SPLINE_CURVE(2,(#71185,#71186,#71187),.UNSPECIFIED.,.F.,.F.)
B_SPLINE_CURVE_WITH_KNOTS((3,3),(0.367644516946552,0.373830527582526),
 .UNSPECIFIED.)
CURVE()
GEOMETRIC_REPRESENTATION_ITEM()
RATIONAL_B_SPLINE_CURVE((1.13426390111306,1.13389822901299,1.13348223894565))
REPRESENTATION_ITEM('')
);
#1353=(
BOUNDED_CURVE()
B_SPLINE_CURVE(2,(#71191,#71192,#71193),.UNSPECIFIED.,.F.,.F.)
B_SPLINE_CURVE_WITH_KNOTS((3,3),(0.271548216895908,0.277734227531896),
 .UNSPECIFIED.)
CURVE()
GEOMETRIC_REPRESENTATION_ITEM()
RATIONAL_B_SPLINE_CURVE((1.13348223894609,1.13389822901344,1.13426390111351))
REPRESENTATION_ITEM('')
);
#1354=(
BOUNDED_CURVE()
B_SPLINE_CURVE(2,(#71197,#71198,#71199),.UNSPECIFIED.,.F.,.F.)
B_SPLINE_CURVE_WITH_KNOTS((3,3),(0.367644516946558,0.373830527582532),
 .UNSPECIFIED.)
CURVE()
GEOMETRIC_REPRESENTATION_ITEM()
RATIONAL_B_SPLINE_CURVE((1.13426390111305,1.13389822901298,1.13348223894564))
REPRESENTATION_ITEM('')
);
#1355=(
BOUNDED_CURVE()
B_SPLINE_CURVE(2,(#71203,#71204,#71205),.UNSPECIFIED.,.F.,.F.)
B_SPLINE_CURVE_WITH_KNOTS((3,3),(0.271548216895918,0.27773422753191),
 .UNSPECIFIED.)
CURVE()
GEOMETRIC_REPRESENTATION_ITEM()
RATIONAL_B_SPLINE_CURVE((1.1334822389462,1.13389822901355,1.13426390111362))
REPRESENTATION_ITEM('')
);
#1356=(
BOUNDED_CURVE()
B_SPLINE_CURVE(2,(#71209,#71210,#71211),.UNSPECIFIED.,.F.,.F.)
B_SPLINE_CURVE_WITH_KNOTS((3,3),(0.367644516946559,0.373830527582532),
 .UNSPECIFIED.)
CURVE()
GEOMETRIC_REPRESENTATION_ITEM()
RATIONAL_B_SPLINE_CURVE((1.13426390111305,1.13389822901299,1.13348223894564))
REPRESENTATION_ITEM('')
);
#1357=(
BOUNDED_CURVE()
B_SPLINE_CURVE(2,(#71215,#71216,#71217),.UNSPECIFIED.,.F.,.F.)
B_SPLINE_CURVE_WITH_KNOTS((3,3),(0.271548216895917,0.277734227531899),
 .UNSPECIFIED.)
CURVE()
GEOMETRIC_REPRESENTATION_ITEM()
RATIONAL_B_SPLINE_CURVE((1.13348223894612,1.13389822901347,1.13426390111355))
REPRESENTATION_ITEM('')
);
#1358=(
BOUNDED_CURVE()
B_SPLINE_CURVE(2,(#71221,#71222,#71223),.UNSPECIFIED.,.F.,.F.)
B_SPLINE_CURVE_WITH_KNOTS((3,3),(0.367644516946562,0.373830527582533),
 .UNSPECIFIED.)
CURVE()
GEOMETRIC_REPRESENTATION_ITEM()
RATIONAL_B_SPLINE_CURVE((1.13426390111306,1.13389822901299,1.13348223894564))
REPRESENTATION_ITEM('')
);
#1359=(
BOUNDED_CURVE()
B_SPLINE_CURVE(2,(#71227,#71228,#71229),.UNSPECIFIED.,.F.,.F.)
B_SPLINE_CURVE_WITH_KNOTS((3,3),(0.271548216895905,0.277734227531891),
 .UNSPECIFIED.)
CURVE()
GEOMETRIC_REPRESENTATION_ITEM()
RATIONAL_B_SPLINE_CURVE((1.13348223894609,1.13389822901344,1.13426390111351))
REPRESENTATION_ITEM('')
);
#1360=(
BOUNDED_CURVE()
B_SPLINE_CURVE(2,(#71233,#71234,#71235),.UNSPECIFIED.,.F.,.F.)
B_SPLINE_CURVE_WITH_KNOTS((3,3),(0.367644516946557,0.373830527582533),
 .UNSPECIFIED.)
CURVE()
GEOMETRIC_REPRESENTATION_ITEM()
RATIONAL_B_SPLINE_CURVE((1.13426390111305,1.13389822901299,1.13348223894564))
REPRESENTATION_ITEM('')
);
#1361=(
BOUNDED_CURVE()
B_SPLINE_CURVE(2,(#71239,#71240,#71241),.UNSPECIFIED.,.F.,.F.)
B_SPLINE_CURVE_WITH_KNOTS((3,3),(0.271548216895918,0.277734227531906),
 .UNSPECIFIED.)
CURVE()
GEOMETRIC_REPRESENTATION_ITEM()
RATIONAL_B_SPLINE_CURVE((1.13348223894616,1.13389822901351,1.13426390111358))
REPRESENTATION_ITEM('')
);
#1362=(
BOUNDED_CURVE()
B_SPLINE_CURVE(2,(#71263,#71264,#71265),.UNSPECIFIED.,.F.,.F.)
B_SPLINE_CURVE_WITH_KNOTS((3,3),(0.376641898803529,0.382940702095941),
 .UNSPECIFIED.)
CURVE()
GEOMETRIC_REPRESENTATION_ITEM()
RATIONAL_B_SPLINE_CURVE((1.12071541658433,1.1202411994692,1.11971735964528))
REPRESENTATION_ITEM('')
);
#1363=(
BOUNDED_CURVE()
B_SPLINE_CURVE(2,(#71269,#71270,#71271),.UNSPECIFIED.,.F.,.F.)
B_SPLINE_CURVE_WITH_KNOTS((3,3),(0.249954652430657,0.25625345571807),
 .UNSPECIFIED.)
CURVE()
GEOMETRIC_REPRESENTATION_ITEM()
RATIONAL_B_SPLINE_CURVE((1.1197173596462,1.12024119946966,1.12071541658442))
REPRESENTATION_ITEM('')
);
#1364=(
BOUNDED_CURVE()
B_SPLINE_CURVE(2,(#71275,#71276,#71277),.UNSPECIFIED.,.F.,.F.)
B_SPLINE_CURVE_WITH_KNOTS((3,3),(0.376641898803524,0.382940702095934),
 .UNSPECIFIED.)
CURVE()
GEOMETRIC_REPRESENTATION_ITEM()
RATIONAL_B_SPLINE_CURVE((1.12071541658448,1.12024119946934,1.11971735964542))
REPRESENTATION_ITEM('')
);
#1365=(
BOUNDED_CURVE()
B_SPLINE_CURVE(2,(#71281,#71282,#71283),.UNSPECIFIED.,.F.,.F.)
B_SPLINE_CURVE_WITH_KNOTS((3,3),(0.249954652430655,0.256253455718069),
 .UNSPECIFIED.)
CURVE()
GEOMETRIC_REPRESENTATION_ITEM()
RATIONAL_B_SPLINE_CURVE((1.11971735964613,1.1202411994696,1.12071541658435))
REPRESENTATION_ITEM('')
);
#1366=(
BOUNDED_CURVE()
B_SPLINE_CURVE(2,(#71287,#71288,#71289),.UNSPECIFIED.,.F.,.F.)
B_SPLINE_CURVE_WITH_KNOTS((3,3),(0.376641898803532,0.382940702095944),
 .UNSPECIFIED.)
CURVE()
GEOMETRIC_REPRESENTATION_ITEM()
RATIONAL_B_SPLINE_CURVE((1.12071541658434,1.12024119946921,1.11971735964529))
REPRESENTATION_ITEM('')
);
#1367=(
BOUNDED_CURVE()
B_SPLINE_CURVE(2,(#71293,#71294,#71295),.UNSPECIFIED.,.F.,.F.)
B_SPLINE_CURVE_WITH_KNOTS((3,3),(0.249954652430645,0.256253455718059),
 .UNSPECIFIED.)
CURVE()
GEOMETRIC_REPRESENTATION_ITEM()
RATIONAL_B_SPLINE_CURVE((1.11971735964598,1.12024119946945,1.1207154165842))
REPRESENTATION_ITEM('')
);
#1368=(
BOUNDED_CURVE()
B_SPLINE_CURVE(2,(#71299,#71300,#71301),.UNSPECIFIED.,.F.,.F.)
B_SPLINE_CURVE_WITH_KNOTS((3,3),(0.376641898803521,0.382940702095933),
 .UNSPECIFIED.)
CURVE()
GEOMETRIC_REPRESENTATION_ITEM()
RATIONAL_B_SPLINE_CURVE((1.1207154165845,1.12024119946936,1.11971735964544))
REPRESENTATION_ITEM('')
);
#1369=(
BOUNDED_CURVE()
B_SPLINE_CURVE(2,(#71305,#71306,#71307),.UNSPECIFIED.,.F.,.F.)
B_SPLINE_CURVE_WITH_KNOTS((3,3),(0.249954652430661,0.256253455718076),
 .UNSPECIFIED.)
CURVE()
GEOMETRIC_REPRESENTATION_ITEM()
RATIONAL_B_SPLINE_CURVE((1.1197173596463,1.12024119946977,1.12071541658453))
REPRESENTATION_ITEM('')
);
#1370=(
BOUNDED_CURVE()
B_SPLINE_CURVE(2,(#71311,#71312,#71313),.UNSPECIFIED.,.F.,.F.)
B_SPLINE_CURVE_WITH_KNOTS((3,3),(0.376641898803535,0.382940702095943),
 .UNSPECIFIED.)
CURVE()
GEOMETRIC_REPRESENTATION_ITEM()
RATIONAL_B_SPLINE_CURVE((1.12071541658437,1.12024119946923,1.11971735964532))
REPRESENTATION_ITEM('')
);
#1371=(
BOUNDED_CURVE()
B_SPLINE_CURVE(2,(#71317,#71318,#71319),.UNSPECIFIED.,.F.,.F.)
B_SPLINE_CURVE_WITH_KNOTS((3,3),(0.249954652430645,0.256253455718058),
 .UNSPECIFIED.)
CURVE()
GEOMETRIC_REPRESENTATION_ITEM()
RATIONAL_B_SPLINE_CURVE((1.11971735964609,1.12024119946955,1.12071541658431))
REPRESENTATION_ITEM('')
);
#1372=(
BOUNDED_CURVE()
B_SPLINE_CURVE(2,(#71323,#71324,#71325),.UNSPECIFIED.,.F.,.F.)
B_SPLINE_CURVE_WITH_KNOTS((3,3),(0.376641898803531,0.382940702095942),
 .UNSPECIFIED.)
CURVE()
GEOMETRIC_REPRESENTATION_ITEM()
RATIONAL_B_SPLINE_CURVE((1.12071541658437,1.12024119946923,1.11971735964532))
REPRESENTATION_ITEM('')
);
#1373=(
BOUNDED_CURVE()
B_SPLINE_CURVE(2,(#71329,#71330,#71331),.UNSPECIFIED.,.F.,.F.)
B_SPLINE_CURVE_WITH_KNOTS((3,3),(0.249954652430646,0.256253455718059),
 .UNSPECIFIED.)
CURVE()
GEOMETRIC_REPRESENTATION_ITEM()
RATIONAL_B_SPLINE_CURVE((1.11971735964605,1.12024119946951,1.12071541658427))
REPRESENTATION_ITEM('')
);
#1374=(
BOUNDED_CURVE()
B_SPLINE_CURVE(2,(#71335,#71336,#71337),.UNSPECIFIED.,.F.,.F.)
B_SPLINE_CURVE_WITH_KNOTS((3,3),(0.376641898803521,0.382940702095931),
 .UNSPECIFIED.)
CURVE()
GEOMETRIC_REPRESENTATION_ITEM()
RATIONAL_B_SPLINE_CURVE((1.12071541658451,1.12024119946938,1.11971735964546))
REPRESENTATION_ITEM('')
);
#1375=(
BOUNDED_CURVE()
B_SPLINE_CURVE(2,(#71341,#71342,#71343),.UNSPECIFIED.,.F.,.F.)
B_SPLINE_CURVE_WITH_KNOTS((3,3),(0.249954652430639,0.256253455718052),
 .UNSPECIFIED.)
CURVE()
GEOMETRIC_REPRESENTATION_ITEM()
RATIONAL_B_SPLINE_CURVE((1.11971735964601,1.12024119946948,1.12071541658424))
REPRESENTATION_ITEM('')
);
#1376=(
BOUNDED_CURVE()
B_SPLINE_CURVE(2,(#71347,#71348,#71349),.UNSPECIFIED.,.F.,.F.)
B_SPLINE_CURVE_WITH_KNOTS((3,3),(0.376641898803533,0.382940702095945),
 .UNSPECIFIED.)
CURVE()
GEOMETRIC_REPRESENTATION_ITEM()
RATIONAL_B_SPLINE_CURVE((1.12071541658434,1.1202411994692,1.11971735964528))
REPRESENTATION_ITEM('')
);
#1377=(
BOUNDED_CURVE()
B_SPLINE_CURVE(2,(#71353,#71354,#71355),.UNSPECIFIED.,.F.,.F.)
B_SPLINE_CURVE_WITH_KNOTS((3,3),(0.249954652430659,0.256253455718072),
 .UNSPECIFIED.)
CURVE()
GEOMETRIC_REPRESENTATION_ITEM()
RATIONAL_B_SPLINE_CURVE((1.11971735964624,1.12024119946971,1.12071541658447))
REPRESENTATION_ITEM('')
);
#1378=(
BOUNDED_CURVE()
B_SPLINE_CURVE(2,(#71359,#71360,#71361),.UNSPECIFIED.,.F.,.F.)
B_SPLINE_CURVE_WITH_KNOTS((3,3),(0.376641898803529,0.382940702095948),
 .UNSPECIFIED.)
CURVE()
GEOMETRIC_REPRESENTATION_ITEM()
RATIONAL_B_SPLINE_CURVE((1.12071541658446,1.12024119946932,1.1197173596454))
REPRESENTATION_ITEM('')
);
#1379=(
BOUNDED_CURVE()
B_SPLINE_CURVE(2,(#71365,#71366,#71367),.UNSPECIFIED.,.F.,.F.)
B_SPLINE_CURVE_WITH_KNOTS((3,3),(0.249954652430643,0.256253455718057),
 .UNSPECIFIED.)
CURVE()
GEOMETRIC_REPRESENTATION_ITEM()
RATIONAL_B_SPLINE_CURVE((1.11971735964609,1.12024119946956,1.12071541658432))
REPRESENTATION_ITEM('')
);
#1380=(
BOUNDED_CURVE()
B_SPLINE_CURVE(2,(#71371,#71372,#71373),.UNSPECIFIED.,.F.,.F.)
B_SPLINE_CURVE_WITH_KNOTS((3,3),(0.376641898803523,0.382940702095941),
 .UNSPECIFIED.)
CURVE()
GEOMETRIC_REPRESENTATION_ITEM()
RATIONAL_B_SPLINE_CURVE((1.12071541658451,1.12024119946937,1.11971735964545))
REPRESENTATION_ITEM('')
);
#1381=(
BOUNDED_CURVE()
B_SPLINE_CURVE(2,(#71377,#71378,#71379),.UNSPECIFIED.,.F.,.F.)
B_SPLINE_CURVE_WITH_KNOTS((3,3),(0.249954652430644,0.256253455718058),
 .UNSPECIFIED.)
CURVE()
GEOMETRIC_REPRESENTATION_ITEM()
RATIONAL_B_SPLINE_CURVE((1.11971735964615,1.12024119946961,1.12071541658437))
REPRESENTATION_ITEM('')
);
#1382=(
BOUNDED_CURVE()
B_SPLINE_CURVE(2,(#71383,#71384,#71385),.UNSPECIFIED.,.F.,.F.)
B_SPLINE_CURVE_WITH_KNOTS((3,3),(0.376641898803536,0.382940702095946),
 .UNSPECIFIED.)
CURVE()
GEOMETRIC_REPRESENTATION_ITEM()
RATIONAL_B_SPLINE_CURVE((1.12071541658451,1.12024119946938,1.11971735964546))
REPRESENTATION_ITEM('')
);
#1383=(
BOUNDED_CURVE()
B_SPLINE_CURVE(2,(#71389,#71390,#71391),.UNSPECIFIED.,.F.,.F.)
B_SPLINE_CURVE_WITH_KNOTS((3,3),(0.24995465243065,0.256253455718062),
 .UNSPECIFIED.)
CURVE()
GEOMETRIC_REPRESENTATION_ITEM()
RATIONAL_B_SPLINE_CURVE((1.11971735964599,1.12024119946946,1.12071541658421))
REPRESENTATION_ITEM('')
);
#1384=(
BOUNDED_CURVE()
B_SPLINE_CURVE(2,(#71395,#71396,#71397),.UNSPECIFIED.,.F.,.F.)
B_SPLINE_CURVE_WITH_KNOTS((3,3),(0.376641898803523,0.38294070209593),
 .UNSPECIFIED.)
CURVE()
GEOMETRIC_REPRESENTATION_ITEM()
RATIONAL_B_SPLINE_CURVE((1.1207154165845,1.12024119946936,1.11971735964544))
REPRESENTATION_ITEM('')
);
#1385=(
BOUNDED_CURVE()
B_SPLINE_CURVE(2,(#71401,#71402,#71403),.UNSPECIFIED.,.F.,.F.)
B_SPLINE_CURVE_WITH_KNOTS((3,3),(0.249954652430653,0.256253455718064),
 .UNSPECIFIED.)
CURVE()
GEOMETRIC_REPRESENTATION_ITEM()
RATIONAL_B_SPLINE_CURVE((1.11971735964611,1.12024119946957,1.12071541658433))
REPRESENTATION_ITEM('')
);
#1386=(
BOUNDED_CURVE()
B_SPLINE_CURVE(2,(#71407,#71408,#71409),.UNSPECIFIED.,.F.,.F.)
B_SPLINE_CURVE_WITH_KNOTS((3,3),(0.376641898803521,0.382940702095931),
 .UNSPECIFIED.)
CURVE()
GEOMETRIC_REPRESENTATION_ITEM()
RATIONAL_B_SPLINE_CURVE((1.12071541658461,1.12024119946947,1.11971735964555))
REPRESENTATION_ITEM('')
);
#1387=(
BOUNDED_CURVE()
B_SPLINE_CURVE(2,(#71413,#71414,#71415),.UNSPECIFIED.,.F.,.F.)
B_SPLINE_CURVE_WITH_KNOTS((3,3),(0.249954652430661,0.256253455718072),
 .UNSPECIFIED.)
CURVE()
GEOMETRIC_REPRESENTATION_ITEM()
RATIONAL_B_SPLINE_CURVE((1.11971735964623,1.1202411994697,1.12071541658446))
REPRESENTATION_ITEM('')
);
#1388=(
BOUNDED_CURVE()
B_SPLINE_CURVE(2,(#71419,#71420,#71421),.UNSPECIFIED.,.F.,.F.)
B_SPLINE_CURVE_WITH_KNOTS((3,3),(0.376641898803537,0.382940702095947),
 .UNSPECIFIED.)
CURVE()
GEOMETRIC_REPRESENTATION_ITEM()
RATIONAL_B_SPLINE_CURVE((1.1207154165845,1.12024119946936,1.11971735964544))
REPRESENTATION_ITEM('')
);
#1389=(
BOUNDED_CURVE()
B_SPLINE_CURVE(2,(#71425,#71426,#71427),.UNSPECIFIED.,.F.,.F.)
B_SPLINE_CURVE_WITH_KNOTS((3,3),(0.249954652430645,0.256253455718056),
 .UNSPECIFIED.)
CURVE()
GEOMETRIC_REPRESENTATION_ITEM()
RATIONAL_B_SPLINE_CURVE((1.11971735964613,1.1202411994696,1.12071541658435))
REPRESENTATION_ITEM('')
);
#1390=(
BOUNDED_CURVE()
B_SPLINE_CURVE(2,(#71431,#71432,#71433),.UNSPECIFIED.,.F.,.F.)
B_SPLINE_CURVE_WITH_KNOTS((3,3),(0.376641898803536,0.382940702095954),
 .UNSPECIFIED.)
CURVE()
GEOMETRIC_REPRESENTATION_ITEM()
RATIONAL_B_SPLINE_CURVE((1.12071541658435,1.12024119946922,1.1197173596453))
REPRESENTATION_ITEM('')
);
#1391=(
BOUNDED_CURVE()
B_SPLINE_CURVE(2,(#71437,#71438,#71439),.UNSPECIFIED.,.F.,.F.)
B_SPLINE_CURVE_WITH_KNOTS((3,3),(0.249954652430663,0.256253455718072),
 .UNSPECIFIED.)
CURVE()
GEOMETRIC_REPRESENTATION_ITEM()
RATIONAL_B_SPLINE_CURVE((1.11971735964633,1.1202411994698,1.12071541658456))
REPRESENTATION_ITEM('')
);
#1392=(
BOUNDED_CURVE()
B_SPLINE_CURVE(2,(#71443,#71444,#71445),.UNSPECIFIED.,.F.,.F.)
B_SPLINE_CURVE_WITH_KNOTS((3,3),(0.376641898803512,0.382940702095922),
 .UNSPECIFIED.)
CURVE()
GEOMETRIC_REPRESENTATION_ITEM()
RATIONAL_B_SPLINE_CURVE((1.12071541658461,1.12024119946947,1.11971735964555))
REPRESENTATION_ITEM('')
);
#1393=(
BOUNDED_CURVE()
B_SPLINE_CURVE(2,(#71449,#71450,#71451),.UNSPECIFIED.,.F.,.F.)
B_SPLINE_CURVE_WITH_KNOTS((3,3),(0.249954652430648,0.256253455718062),
 .UNSPECIFIED.)
CURVE()
GEOMETRIC_REPRESENTATION_ITEM()
RATIONAL_B_SPLINE_CURVE((1.11971735964605,1.12024119946951,1.12071541658427))
REPRESENTATION_ITEM('')
);
#1394=(
BOUNDED_CURVE()
B_SPLINE_CURVE(2,(#71455,#71456,#71457),.UNSPECIFIED.,.F.,.F.)
B_SPLINE_CURVE_WITH_KNOTS((3,3),(0.376641898803527,0.382940702095944),
 .UNSPECIFIED.)
CURVE()
GEOMETRIC_REPRESENTATION_ITEM()
RATIONAL_B_SPLINE_CURVE((1.12071541658444,1.12024119946931,1.11971735964539))
REPRESENTATION_ITEM('')
);
#1395=(
BOUNDED_CURVE()
B_SPLINE_CURVE(2,(#71461,#71462,#71463),.UNSPECIFIED.,.F.,.F.)
B_SPLINE_CURVE_WITH_KNOTS((3,3),(0.24995465243065,0.256253455718066),
 .UNSPECIFIED.)
CURVE()
GEOMETRIC_REPRESENTATION_ITEM()
RATIONAL_B_SPLINE_CURVE((1.11971735964612,1.12024119946958,1.12071541658434))
REPRESENTATION_ITEM('')
);
#1396=(
BOUNDED_CURVE()
B_SPLINE_CURVE(2,(#71467,#71468,#71469),.UNSPECIFIED.,.F.,.F.)
B_SPLINE_CURVE_WITH_KNOTS((3,3),(0.37664189880352,0.382940702095936),
 .UNSPECIFIED.)
CURVE()
GEOMETRIC_REPRESENTATION_ITEM()
RATIONAL_B_SPLINE_CURVE((1.12071541658452,1.12024119946938,1.11971735964546))
REPRESENTATION_ITEM('')
);
#1397=(
BOUNDED_CURVE()
B_SPLINE_CURVE(2,(#71473,#71474,#71475),.UNSPECIFIED.,.F.,.F.)
B_SPLINE_CURVE_WITH_KNOTS((3,3),(0.249954652430664,0.25625345571808),
 .UNSPECIFIED.)
CURVE()
GEOMETRIC_REPRESENTATION_ITEM()
RATIONAL_B_SPLINE_CURVE((1.11971735964628,1.12024119946975,1.12071541658451))
REPRESENTATION_ITEM('')
);
#1398=(
BOUNDED_CURVE()
B_SPLINE_CURVE(2,(#71479,#71480,#71481),.UNSPECIFIED.,.F.,.F.)
B_SPLINE_CURVE_WITH_KNOTS((3,3),(0.376641898803518,0.382940702095937),
 .UNSPECIFIED.)
CURVE()
GEOMETRIC_REPRESENTATION_ITEM()
RATIONAL_B_SPLINE_CURVE((1.12071541658454,1.12024119946941,1.11971735964549))
REPRESENTATION_ITEM('')
);
#1399=(
BOUNDED_CURVE()
B_SPLINE_CURVE(2,(#71485,#71486,#71487),.UNSPECIFIED.,.F.,.F.)
B_SPLINE_CURVE_WITH_KNOTS((3,3),(0.249954652430639,0.256253455718056),
 .UNSPECIFIED.)
CURVE()
GEOMETRIC_REPRESENTATION_ITEM()
RATIONAL_B_SPLINE_CURVE((1.11971735964609,1.12024119946956,1.12071541658432))
REPRESENTATION_ITEM('')
);
#1400=(
BOUNDED_CURVE()
B_SPLINE_CURVE(2,(#71491,#71492,#71493),.UNSPECIFIED.,.F.,.F.)
B_SPLINE_CURVE_WITH_KNOTS((3,3),(0.376641898803522,0.382940702095936),
 .UNSPECIFIED.)
CURVE()
GEOMETRIC_REPRESENTATION_ITEM()
RATIONAL_B_SPLINE_CURVE((1.12071541658447,1.12024119946934,1.11971735964542))
REPRESENTATION_ITEM('')
);
#1401=(
BOUNDED_CURVE()
B_SPLINE_CURVE(2,(#71497,#71498,#71499),.UNSPECIFIED.,.F.,.F.)
B_SPLINE_CURVE_WITH_KNOTS((3,3),(0.249954652430657,0.256253455718066),
 .UNSPECIFIED.)
CURVE()
GEOMETRIC_REPRESENTATION_ITEM()
RATIONAL_B_SPLINE_CURVE((1.11971735964622,1.12024119946968,1.12071541658444))
REPRESENTATION_ITEM('')
);
#1402=(
BOUNDED_CURVE()
B_SPLINE_CURVE(2,(#71503,#71504,#71505),.UNSPECIFIED.,.F.,.F.)
B_SPLINE_CURVE_WITH_KNOTS((3,3),(0.376641898803533,0.38294070209594),
 .UNSPECIFIED.)
CURVE()
GEOMETRIC_REPRESENTATION_ITEM()
RATIONAL_B_SPLINE_CURVE((1.12071541658433,1.1202411994692,1.11971735964528))
REPRESENTATION_ITEM('')
);
#1403=(
BOUNDED_CURVE()
B_SPLINE_CURVE(2,(#71509,#71510,#71511),.UNSPECIFIED.,.F.,.F.)
B_SPLINE_CURVE_WITH_KNOTS((3,3),(0.249954652430642,0.256253455718055),
 .UNSPECIFIED.)
CURVE()
GEOMETRIC_REPRESENTATION_ITEM()
RATIONAL_B_SPLINE_CURVE((1.11971735964602,1.12024119946948,1.12071541658424))
REPRESENTATION_ITEM('')
);
#1404=(
BOUNDED_CURVE()
B_SPLINE_CURVE(2,(#71515,#71516,#71517),.UNSPECIFIED.,.F.,.F.)
B_SPLINE_CURVE_WITH_KNOTS((3,3),(0.376641898803547,0.382940702095962),
 .UNSPECIFIED.)
CURVE()
GEOMETRIC_REPRESENTATION_ITEM()
RATIONAL_B_SPLINE_CURVE((1.12071541658418,1.12024119946904,1.11971735964512))
REPRESENTATION_ITEM('')
);
#1405=(
BOUNDED_CURVE()
B_SPLINE_CURVE(2,(#71521,#71522,#71523),.UNSPECIFIED.,.F.,.F.)
B_SPLINE_CURVE_WITH_KNOTS((3,3),(0.249954652430658,0.256253455718078),
 .UNSPECIFIED.)
CURVE()
GEOMETRIC_REPRESENTATION_ITEM()
RATIONAL_B_SPLINE_CURVE((1.1197173596463,1.12024119946977,1.12071541658453))
REPRESENTATION_ITEM('')
);
#1406=(
BOUNDED_CURVE()
B_SPLINE_CURVE(2,(#71527,#71528,#71529),.UNSPECIFIED.,.F.,.F.)
B_SPLINE_CURVE_WITH_KNOTS((3,3),(0.376641898803522,0.382940702095938),
 .UNSPECIFIED.)
CURVE()
GEOMETRIC_REPRESENTATION_ITEM()
RATIONAL_B_SPLINE_CURVE((1.12071541658451,1.12024119946937,1.11971735964545))
REPRESENTATION_ITEM('')
);
#1407=(
BOUNDED_CURVE()
B_SPLINE_CURVE(2,(#71533,#71534,#71535),.UNSPECIFIED.,.F.,.F.)
B_SPLINE_CURVE_WITH_KNOTS((3,3),(0.249954652430655,0.25625345571807),
 .UNSPECIFIED.)
CURVE()
GEOMETRIC_REPRESENTATION_ITEM()
RATIONAL_B_SPLINE_CURVE((1.11971735964625,1.12024119946971,1.12071541658447))
REPRESENTATION_ITEM('')
);
#1408=(
BOUNDED_CURVE()
B_SPLINE_CURVE(2,(#71539,#71540,#71541),.UNSPECIFIED.,.F.,.F.)
B_SPLINE_CURVE_WITH_KNOTS((3,3),(0.376641898803531,0.382940702095945),
 .UNSPECIFIED.)
CURVE()
GEOMETRIC_REPRESENTATION_ITEM()
RATIONAL_B_SPLINE_CURVE((1.12071541658432,1.12024119946919,1.11971735964527))
REPRESENTATION_ITEM('')
);
#1409=(
BOUNDED_CURVE()
B_SPLINE_CURVE(2,(#71545,#71546,#71547),.UNSPECIFIED.,.F.,.F.)
B_SPLINE_CURVE_WITH_KNOTS((3,3),(0.249954652430637,0.256253455718055),
 .UNSPECIFIED.)
CURVE()
GEOMETRIC_REPRESENTATION_ITEM()
RATIONAL_B_SPLINE_CURVE((1.11971735964599,1.12024119946945,1.12071541658421))
REPRESENTATION_ITEM('')
);
#1410=(
BOUNDED_CURVE()
B_SPLINE_CURVE(2,(#71551,#71552,#71553),.UNSPECIFIED.,.F.,.F.)
B_SPLINE_CURVE_WITH_KNOTS((3,3),(0.376641898803544,0.382940702095957),
 .UNSPECIFIED.)
CURVE()
GEOMETRIC_REPRESENTATION_ITEM()
RATIONAL_B_SPLINE_CURVE((1.12071541658422,1.12024119946908,1.11971735964516))
REPRESENTATION_ITEM('')
);
#1411=(
BOUNDED_CURVE()
B_SPLINE_CURVE(2,(#71557,#71558,#71559),.UNSPECIFIED.,.F.,.F.)
B_SPLINE_CURVE_WITH_KNOTS((3,3),(0.249954652430653,0.256253455718062),
 .UNSPECIFIED.)
CURVE()
GEOMETRIC_REPRESENTATION_ITEM()
RATIONAL_B_SPLINE_CURVE((1.11971735964616,1.12024119946962,1.12071541658438))
REPRESENTATION_ITEM('')
);
#1412=(
BOUNDED_CURVE()
B_SPLINE_CURVE(2,(#71563,#71564,#71565),.UNSPECIFIED.,.F.,.F.)
B_SPLINE_CURVE_WITH_KNOTS((3,3),(0.376641898803539,0.38294070209595),
 .UNSPECIFIED.)
CURVE()
GEOMETRIC_REPRESENTATION_ITEM()
RATIONAL_B_SPLINE_CURVE((1.12071541658449,1.12024119946935,1.11971735964543))
REPRESENTATION_ITEM('')
);
#1413=(
BOUNDED_CURVE()
B_SPLINE_CURVE(2,(#71569,#71570,#71571),.UNSPECIFIED.,.F.,.F.)
B_SPLINE_CURVE_WITH_KNOTS((3,3),(0.249954652430653,0.256253455718071),
 .UNSPECIFIED.)
CURVE()
GEOMETRIC_REPRESENTATION_ITEM()
RATIONAL_B_SPLINE_CURVE((1.11971735964627,1.12024119946973,1.12071541658449))
REPRESENTATION_ITEM('')
);
#1414=(
BOUNDED_CURVE()
B_SPLINE_CURVE(2,(#71575,#71576,#71577),.UNSPECIFIED.,.F.,.F.)
B_SPLINE_CURVE_WITH_KNOTS((3,3),(0.376641898803533,0.382940702095944),
 .UNSPECIFIED.)
CURVE()
GEOMETRIC_REPRESENTATION_ITEM()
RATIONAL_B_SPLINE_CURVE((1.12071541658435,1.12024119946922,1.1197173596453))
REPRESENTATION_ITEM('')
);
#1415=(
BOUNDED_CURVE()
B_SPLINE_CURVE(2,(#71581,#71582,#71583),.UNSPECIFIED.,.F.,.F.)
B_SPLINE_CURVE_WITH_KNOTS((3,3),(0.249954652430647,0.256253455718059),
 .UNSPECIFIED.)
CURVE()
GEOMETRIC_REPRESENTATION_ITEM()
RATIONAL_B_SPLINE_CURVE((1.11971735964614,1.12024119946961,1.12071541658437))
REPRESENTATION_ITEM('')
);
#1416=(
BOUNDED_CURVE()
B_SPLINE_CURVE(2,(#71587,#71588,#71589),.UNSPECIFIED.,.F.,.F.)
B_SPLINE_CURVE_WITH_KNOTS((3,3),(0.376641898803539,0.382940702095955),
 .UNSPECIFIED.)
CURVE()
GEOMETRIC_REPRESENTATION_ITEM()
RATIONAL_B_SPLINE_CURVE((1.12071541658434,1.1202411994692,1.11971735964528))
REPRESENTATION_ITEM('')
);
#1417=(
BOUNDED_CURVE()
B_SPLINE_CURVE(2,(#71593,#71594,#71595),.UNSPECIFIED.,.F.,.F.)
B_SPLINE_CURVE_WITH_KNOTS((3,3),(0.249954652430656,0.256253455718067),
 .UNSPECIFIED.)
CURVE()
GEOMETRIC_REPRESENTATION_ITEM()
RATIONAL_B_SPLINE_CURVE((1.11971735964622,1.12024119946969,1.12071541658444))
REPRESENTATION_ITEM('')
);
#1418=(
BOUNDED_CURVE()
B_SPLINE_CURVE(2,(#71599,#71600,#71601),.UNSPECIFIED.,.F.,.F.)
B_SPLINE_CURVE_WITH_KNOTS((3,3),(0.376641898803524,0.382940702095936),
 .UNSPECIFIED.)
CURVE()
GEOMETRIC_REPRESENTATION_ITEM()
RATIONAL_B_SPLINE_CURVE((1.12071541658457,1.12024119946943,1.11971735964551))
REPRESENTATION_ITEM('')
);
#1419=(
BOUNDED_CURVE()
B_SPLINE_CURVE(2,(#71605,#71606,#71607),.UNSPECIFIED.,.F.,.F.)
B_SPLINE_CURVE_WITH_KNOTS((3,3),(0.249954652430651,0.256253455718065),
 .UNSPECIFIED.)
CURVE()
GEOMETRIC_REPRESENTATION_ITEM()
RATIONAL_B_SPLINE_CURVE((1.11971735964615,1.12024119946961,1.12071541658437))
REPRESENTATION_ITEM('')
);
#1420=(
BOUNDED_CURVE()
B_SPLINE_CURVE(2,(#71611,#71612,#71613),.UNSPECIFIED.,.F.,.F.)
B_SPLINE_CURVE_WITH_KNOTS((3,3),(0.376641898803518,0.382940702095931),
 .UNSPECIFIED.)
CURVE()
GEOMETRIC_REPRESENTATION_ITEM()
RATIONAL_B_SPLINE_CURVE((1.12071541658449,1.12024119946936,1.11971735964544))
REPRESENTATION_ITEM('')
);
#1421=(
BOUNDED_CURVE()
B_SPLINE_CURVE(2,(#71617,#71618,#71619),.UNSPECIFIED.,.F.,.F.)
B_SPLINE_CURVE_WITH_KNOTS((3,3),(0.249954652430648,0.256253455718058),
 .UNSPECIFIED.)
CURVE()
GEOMETRIC_REPRESENTATION_ITEM()
RATIONAL_B_SPLINE_CURVE((1.11971735964614,1.1202411994696,1.12071541658436))
REPRESENTATION_ITEM('')
);
#1422=(
BOUNDED_CURVE()
B_SPLINE_CURVE(2,(#71623,#71624,#71625),.UNSPECIFIED.,.F.,.F.)
B_SPLINE_CURVE_WITH_KNOTS((3,3),(0.376641898803531,0.382940702095945),
 .UNSPECIFIED.)
CURVE()
GEOMETRIC_REPRESENTATION_ITEM()
RATIONAL_B_SPLINE_CURVE((1.12071541658451,1.12024119946937,1.11971735964545))
REPRESENTATION_ITEM('')
);
#1423=(
BOUNDED_CURVE()
B_SPLINE_CURVE(2,(#71629,#71630,#71631),.UNSPECIFIED.,.F.,.F.)
B_SPLINE_CURVE_WITH_KNOTS((3,3),(0.249954652430648,0.256253455718067),
 .UNSPECIFIED.)
CURVE()
GEOMETRIC_REPRESENTATION_ITEM()
RATIONAL_B_SPLINE_CURVE((1.11971735964618,1.12024119946964,1.1207154165844))
REPRESENTATION_ITEM('')
);
#1424=(
BOUNDED_CURVE()
B_SPLINE_CURVE(2,(#71635,#71636,#71637),.UNSPECIFIED.,.F.,.F.)
B_SPLINE_CURVE_WITH_KNOTS((3,3),(0.376641898803536,0.382940702095949),
 .UNSPECIFIED.)
CURVE()
GEOMETRIC_REPRESENTATION_ITEM()
RATIONAL_B_SPLINE_CURVE((1.12071541658431,1.12024119946918,1.11971735964526))
REPRESENTATION_ITEM('')
);
#1425=(
BOUNDED_CURVE()
B_SPLINE_CURVE(2,(#71641,#71642,#71643),.UNSPECIFIED.,.F.,.F.)
B_SPLINE_CURVE_WITH_KNOTS((3,3),(0.249954652430665,0.256253455718077),
 .UNSPECIFIED.)
CURVE()
GEOMETRIC_REPRESENTATION_ITEM()
RATIONAL_B_SPLINE_CURVE((1.11971735964631,1.12024119946977,1.12071541658453))
REPRESENTATION_ITEM('')
);
#1426=(
BOUNDED_CURVE()
B_SPLINE_CURVE(2,(#71647,#71648,#71649),.UNSPECIFIED.,.F.,.F.)
B_SPLINE_CURVE_WITH_KNOTS((3,3),(0.376641898803534,0.382940702095945),
 .UNSPECIFIED.)
CURVE()
GEOMETRIC_REPRESENTATION_ITEM()
RATIONAL_B_SPLINE_CURVE((1.12071541658427,1.12024119946914,1.11971735964522))
REPRESENTATION_ITEM('')
);
#1427=(
BOUNDED_CURVE()
B_SPLINE_CURVE(2,(#71653,#71654,#71655),.UNSPECIFIED.,.F.,.F.)
B_SPLINE_CURVE_WITH_KNOTS((3,3),(0.249954652430654,0.256253455718069),
 .UNSPECIFIED.)
CURVE()
GEOMETRIC_REPRESENTATION_ITEM()
RATIONAL_B_SPLINE_CURVE((1.11971735964621,1.12024119946968,1.12071541658444))
REPRESENTATION_ITEM('')
);
#1428=(
BOUNDED_CURVE()
B_SPLINE_CURVE(2,(#71659,#71660,#71661),.UNSPECIFIED.,.F.,.F.)
B_SPLINE_CURVE_WITH_KNOTS((3,3),(0.376641898803532,0.382940702095944),
 .UNSPECIFIED.)
CURVE()
GEOMETRIC_REPRESENTATION_ITEM()
RATIONAL_B_SPLINE_CURVE((1.12071541658432,1.12024119946919,1.11971735964527))
REPRESENTATION_ITEM('')
);
#1429=(
BOUNDED_CURVE()
B_SPLINE_CURVE(2,(#71665,#71666,#71667),.UNSPECIFIED.,.F.,.F.)
B_SPLINE_CURVE_WITH_KNOTS((3,3),(0.249954652430654,0.256253455718072),
 .UNSPECIFIED.)
CURVE()
GEOMETRIC_REPRESENTATION_ITEM()
RATIONAL_B_SPLINE_CURVE((1.11971735964625,1.12024119946971,1.12071541658447))
REPRESENTATION_ITEM('')
);
#1430=(
BOUNDED_CURVE()
B_SPLINE_CURVE(2,(#71671,#71672,#71673),.UNSPECIFIED.,.F.,.F.)
B_SPLINE_CURVE_WITH_KNOTS((3,3),(0.376641898803539,0.382940702095952),
 .UNSPECIFIED.)
CURVE()
GEOMETRIC_REPRESENTATION_ITEM()
RATIONAL_B_SPLINE_CURVE((1.1207154165844,1.12024119946926,1.11971735964534))
REPRESENTATION_ITEM('')
);
#1431=(
BOUNDED_CURVE()
B_SPLINE_CURVE(2,(#71677,#71678,#71679),.UNSPECIFIED.,.F.,.F.)
B_SPLINE_CURVE_WITH_KNOTS((3,3),(0.249954652430648,0.256253455718062),
 .UNSPECIFIED.)
CURVE()
GEOMETRIC_REPRESENTATION_ITEM()
RATIONAL_B_SPLINE_CURVE((1.11971735964618,1.12024119946965,1.12071541658441))
REPRESENTATION_ITEM('')
);
#1432=(
BOUNDED_CURVE()
B_SPLINE_CURVE(2,(#71683,#71684,#71685),.UNSPECIFIED.,.F.,.F.)
B_SPLINE_CURVE_WITH_KNOTS((3,3),(0.376641898803519,0.382940702095932),
 .UNSPECIFIED.)
CURVE()
GEOMETRIC_REPRESENTATION_ITEM()
RATIONAL_B_SPLINE_CURVE((1.12071541658452,1.12024119946938,1.11971735964546))
REPRESENTATION_ITEM('')
);
#1433=(
BOUNDED_CURVE()
B_SPLINE_CURVE(2,(#71689,#71690,#71691),.UNSPECIFIED.,.F.,.F.)
B_SPLINE_CURVE_WITH_KNOTS((3,3),(0.249954652430659,0.256253455718071),
 .UNSPECIFIED.)
CURVE()
GEOMETRIC_REPRESENTATION_ITEM()
RATIONAL_B_SPLINE_CURVE((1.11971735964627,1.12024119946974,1.1207154165845))
REPRESENTATION_ITEM('')
);
#1434=(
BOUNDED_CURVE()
B_SPLINE_CURVE(2,(#71695,#71696,#71697),.UNSPECIFIED.,.F.,.F.)
B_SPLINE_CURVE_WITH_KNOTS((3,3),(0.376641898803527,0.382940702095942),
 .UNSPECIFIED.)
CURVE()
GEOMETRIC_REPRESENTATION_ITEM()
RATIONAL_B_SPLINE_CURVE((1.12071541658453,1.1202411994694,1.11971735964547))
REPRESENTATION_ITEM('')
);
#1435=(
BOUNDED_CURVE()
B_SPLINE_CURVE(2,(#71701,#71702,#71703),.UNSPECIFIED.,.F.,.F.)
B_SPLINE_CURVE_WITH_KNOTS((3,3),(0.249954652430662,0.256253455718075),
 .UNSPECIFIED.)
CURVE()
GEOMETRIC_REPRESENTATION_ITEM()
RATIONAL_B_SPLINE_CURVE((1.11971735964629,1.12024119946976,1.12071541658452))
REPRESENTATION_ITEM('')
);
#1436=(
BOUNDED_CURVE()
B_SPLINE_CURVE(2,(#71707,#71708,#71709),.UNSPECIFIED.,.F.,.F.)
B_SPLINE_CURVE_WITH_KNOTS((3,3),(0.376641898803543,0.382940702095954),
 .UNSPECIFIED.)
CURVE()
GEOMETRIC_REPRESENTATION_ITEM()
RATIONAL_B_SPLINE_CURVE((1.12071541658423,1.1202411994691,1.11971735964518))
REPRESENTATION_ITEM('')
);
#1437=(
BOUNDED_CURVE()
B_SPLINE_CURVE(2,(#71713,#71714,#71715),.UNSPECIFIED.,.F.,.F.)
B_SPLINE_CURVE_WITH_KNOTS((3,3),(0.249954652430648,0.256253455718061),
 .UNSPECIFIED.)
CURVE()
GEOMETRIC_REPRESENTATION_ITEM()
RATIONAL_B_SPLINE_CURVE((1.11971735964609,1.12024119946956,1.12071541658431))
REPRESENTATION_ITEM('')
);
#1438=(
BOUNDED_CURVE()
B_SPLINE_CURVE(2,(#71719,#71720,#71721),.UNSPECIFIED.,.F.,.F.)
B_SPLINE_CURVE_WITH_KNOTS((3,3),(0.376641898803529,0.382940702095943),
 .UNSPECIFIED.)
CURVE()
GEOMETRIC_REPRESENTATION_ITEM()
RATIONAL_B_SPLINE_CURVE((1.12071541658438,1.12024119946925,1.11971735964533))
REPRESENTATION_ITEM('')
);
#1439=(
BOUNDED_CURVE()
B_SPLINE_CURVE(2,(#71725,#71726,#71727),.UNSPECIFIED.,.F.,.F.)
B_SPLINE_CURVE_WITH_KNOTS((3,3),(0.249954652430657,0.256253455718069),
 .UNSPECIFIED.)
CURVE()
GEOMETRIC_REPRESENTATION_ITEM()
RATIONAL_B_SPLINE_CURVE((1.11971735964625,1.12024119946971,1.12071541658447))
REPRESENTATION_ITEM('')
);
#1440=(
BOUNDED_CURVE()
B_SPLINE_CURVE(2,(#71731,#71732,#71733),.UNSPECIFIED.,.F.,.F.)
B_SPLINE_CURVE_WITH_KNOTS((3,3),(0.376641898803529,0.382940702095941),
 .UNSPECIFIED.)
CURVE()
GEOMETRIC_REPRESENTATION_ITEM()
RATIONAL_B_SPLINE_CURVE((1.12071541658439,1.12024119946925,1.11971735964533))
REPRESENTATION_ITEM('')
);
#1441=(
BOUNDED_CURVE()
B_SPLINE_CURVE(2,(#71737,#71738,#71739),.UNSPECIFIED.,.F.,.F.)
B_SPLINE_CURVE_WITH_KNOTS((3,3),(0.24995465243065,0.256253455718062),
 .UNSPECIFIED.)
CURVE()
GEOMETRIC_REPRESENTATION_ITEM()
RATIONAL_B_SPLINE_CURVE((1.11971735964607,1.12024119946954,1.12071541658429))
REPRESENTATION_ITEM('')
);
#1442=(
BOUNDED_CURVE()
B_SPLINE_CURVE(2,(#71743,#71744,#71745),.UNSPECIFIED.,.F.,.F.)
B_SPLINE_CURVE_WITH_KNOTS((3,3),(0.376641898803544,0.382940702095955),
 .UNSPECIFIED.)
CURVE()
GEOMETRIC_REPRESENTATION_ITEM()
RATIONAL_B_SPLINE_CURVE((1.12071541658421,1.12024119946907,1.11971735964515))
REPRESENTATION_ITEM('')
);
#1443=(
BOUNDED_CURVE()
B_SPLINE_CURVE(2,(#71749,#71750,#71751),.UNSPECIFIED.,.F.,.F.)
B_SPLINE_CURVE_WITH_KNOTS((3,3),(0.249954652430658,0.256253455718075),
 .UNSPECIFIED.)
CURVE()
GEOMETRIC_REPRESENTATION_ITEM()
RATIONAL_B_SPLINE_CURVE((1.11971735964629,1.12024119946976,1.12071541658452))
REPRESENTATION_ITEM('')
);
#1444=(
BOUNDED_CURVE()
B_SPLINE_CURVE(2,(#71755,#71756,#71757),.UNSPECIFIED.,.F.,.F.)
B_SPLINE_CURVE_WITH_KNOTS((3,3),(0.376641898803543,0.382940702095958),
 .UNSPECIFIED.)
CURVE()
GEOMETRIC_REPRESENTATION_ITEM()
RATIONAL_B_SPLINE_CURVE((1.12071541658432,1.12024119946919,1.11971735964527))
REPRESENTATION_ITEM('')
);
#1445=(
BOUNDED_CURVE()
B_SPLINE_CURVE(2,(#71761,#71762,#71763),.UNSPECIFIED.,.F.,.F.)
B_SPLINE_CURVE_WITH_KNOTS((3,3),(0.249954652430663,0.256253455718076),
 .UNSPECIFIED.)
CURVE()
GEOMETRIC_REPRESENTATION_ITEM()
RATIONAL_B_SPLINE_CURVE((1.11971735964633,1.12024119946979,1.12071541658455))
REPRESENTATION_ITEM('')
);
#1446=(
BOUNDED_CURVE()
B_SPLINE_CURVE(2,(#71767,#71768,#71769),.UNSPECIFIED.,.F.,.F.)
B_SPLINE_CURVE_WITH_KNOTS((3,3),(0.37664189880352,0.382940702095933),
 .UNSPECIFIED.)
CURVE()
GEOMETRIC_REPRESENTATION_ITEM()
RATIONAL_B_SPLINE_CURVE((1.1207154165845,1.12024119946936,1.11971735964544))
REPRESENTATION_ITEM('')
);
#1447=(
BOUNDED_CURVE()
B_SPLINE_CURVE(2,(#71773,#71774,#71775),.UNSPECIFIED.,.F.,.F.)
B_SPLINE_CURVE_WITH_KNOTS((3,3),(0.249954652430661,0.256253455718074),
 .UNSPECIFIED.)
CURVE()
GEOMETRIC_REPRESENTATION_ITEM()
RATIONAL_B_SPLINE_CURVE((1.11971735964627,1.12024119946973,1.12071541658449))
REPRESENTATION_ITEM('')
);
#1448=(
BOUNDED_CURVE()
B_SPLINE_CURVE(2,(#71779,#71780,#71781),.UNSPECIFIED.,.F.,.F.)
B_SPLINE_CURVE_WITH_KNOTS((3,3),(0.376641898803524,0.382940702095942),
 .UNSPECIFIED.)
CURVE()
GEOMETRIC_REPRESENTATION_ITEM()
RATIONAL_B_SPLINE_CURVE((1.12071541658449,1.12024119946935,1.11971735964543))
REPRESENTATION_ITEM('')
);
#1449=(
BOUNDED_CURVE()
B_SPLINE_CURVE(2,(#71785,#71786,#71787),.UNSPECIFIED.,.F.,.F.)
B_SPLINE_CURVE_WITH_KNOTS((3,3),(0.249954652430645,0.256253455718058),
 .UNSPECIFIED.)
CURVE()
GEOMETRIC_REPRESENTATION_ITEM()
RATIONAL_B_SPLINE_CURVE((1.11971735964602,1.12024119946949,1.12071541658425))
REPRESENTATION_ITEM('')
);
#1450=(
BOUNDED_CURVE()
B_SPLINE_CURVE(2,(#71791,#71792,#71793),.UNSPECIFIED.,.F.,.F.)
B_SPLINE_CURVE_WITH_KNOTS((3,3),(0.376641898803526,0.382940702095943),
 .UNSPECIFIED.)
CURVE()
GEOMETRIC_REPRESENTATION_ITEM()
RATIONAL_B_SPLINE_CURVE((1.12071541658447,1.12024119946934,1.11971735964542))
REPRESENTATION_ITEM('')
);
#1451=(
BOUNDED_CURVE()
B_SPLINE_CURVE(2,(#71797,#71798,#71799),.UNSPECIFIED.,.F.,.F.)
B_SPLINE_CURVE_WITH_KNOTS((3,3),(0.249954652430656,0.25625345571807),
 .UNSPECIFIED.)
CURVE()
GEOMETRIC_REPRESENTATION_ITEM()
RATIONAL_B_SPLINE_CURVE((1.11971735964623,1.12024119946969,1.12071541658445))
REPRESENTATION_ITEM('')
);
#1452=(
BOUNDED_CURVE()
B_SPLINE_CURVE(2,(#71803,#71804,#71805),.UNSPECIFIED.,.F.,.F.)
B_SPLINE_CURVE_WITH_KNOTS((3,3),(0.376641898803539,0.382940702095953),
 .UNSPECIFIED.)
CURVE()
GEOMETRIC_REPRESENTATION_ITEM()
RATIONAL_B_SPLINE_CURVE((1.12071541658437,1.12024119946923,1.11971735964531))
REPRESENTATION_ITEM('')
);
#1453=(
BOUNDED_CURVE()
B_SPLINE_CURVE(2,(#71809,#71810,#71811),.UNSPECIFIED.,.F.,.F.)
B_SPLINE_CURVE_WITH_KNOTS((3,3),(0.249954652430661,0.256253455718075),
 .UNSPECIFIED.)
CURVE()
GEOMETRIC_REPRESENTATION_ITEM()
RATIONAL_B_SPLINE_CURVE((1.11971735964628,1.12024119946974,1.1207154165845))
REPRESENTATION_ITEM('')
);
#1454=(
BOUNDED_CURVE()
B_SPLINE_CURVE(2,(#71815,#71816,#71817),.UNSPECIFIED.,.F.,.F.)
B_SPLINE_CURVE_WITH_KNOTS((3,3),(0.376641898803538,0.382940702095948),
 .UNSPECIFIED.)
CURVE()
GEOMETRIC_REPRESENTATION_ITEM()
RATIONAL_B_SPLINE_CURVE((1.12071541658433,1.1202411994692,1.11971735964528))
REPRESENTATION_ITEM('')
);
#1455=(
BOUNDED_CURVE()
B_SPLINE_CURVE(2,(#71821,#71822,#71823),.UNSPECIFIED.,.F.,.F.)
B_SPLINE_CURVE_WITH_KNOTS((3,3),(0.249954652430662,0.256253455718076),
 .UNSPECIFIED.)
CURVE()
GEOMETRIC_REPRESENTATION_ITEM()
RATIONAL_B_SPLINE_CURVE((1.11971735964622,1.12024119946968,1.12071541658444))
REPRESENTATION_ITEM('')
);
#1456=(
BOUNDED_CURVE()
B_SPLINE_CURVE(2,(#71827,#71828,#71829),.UNSPECIFIED.,.F.,.F.)
B_SPLINE_CURVE_WITH_KNOTS((3,3),(0.37664189880352,0.382940702095935),
 .UNSPECIFIED.)
CURVE()
GEOMETRIC_REPRESENTATION_ITEM()
RATIONAL_B_SPLINE_CURVE((1.12071541658454,1.12024119946941,1.11971735964549))
REPRESENTATION_ITEM('')
);
#1457=(
BOUNDED_CURVE()
B_SPLINE_CURVE(2,(#71833,#71834,#71835),.UNSPECIFIED.,.F.,.F.)
B_SPLINE_CURVE_WITH_KNOTS((3,3),(0.24995465243066,0.256253455718075),
 .UNSPECIFIED.)
CURVE()
GEOMETRIC_REPRESENTATION_ITEM()
RATIONAL_B_SPLINE_CURVE((1.1197173596463,1.12024119946976,1.12071541658452))
REPRESENTATION_ITEM('')
);
#1458=(
BOUNDED_CURVE()
B_SPLINE_CURVE(2,(#71839,#71840,#71841),.UNSPECIFIED.,.F.,.F.)
B_SPLINE_CURVE_WITH_KNOTS((3,3),(0.376641898803523,0.382940702095934),
 .UNSPECIFIED.)
CURVE()
GEOMETRIC_REPRESENTATION_ITEM()
RATIONAL_B_SPLINE_CURVE((1.12071541658448,1.12024119946934,1.11971735964542))
REPRESENTATION_ITEM('')
);
#1459=(
BOUNDED_CURVE()
B_SPLINE_CURVE(2,(#71845,#71846,#71847),.UNSPECIFIED.,.F.,.F.)
B_SPLINE_CURVE_WITH_KNOTS((3,3),(0.249954652430663,0.256253455718077),
 .UNSPECIFIED.)
CURVE()
GEOMETRIC_REPRESENTATION_ITEM()
RATIONAL_B_SPLINE_CURVE((1.11971735964627,1.12024119946973,1.12071541658449))
REPRESENTATION_ITEM('')
);
#1460=(
BOUNDED_CURVE()
B_SPLINE_CURVE(2,(#71851,#71852,#71853),.UNSPECIFIED.,.F.,.F.)
B_SPLINE_CURVE_WITH_KNOTS((3,3),(0.376641898803548,0.382940702095957),
 .UNSPECIFIED.)
CURVE()
GEOMETRIC_REPRESENTATION_ITEM()
RATIONAL_B_SPLINE_CURVE((1.12071541658418,1.12024119946905,1.11971735964513))
REPRESENTATION_ITEM('')
);
#1461=(
BOUNDED_CURVE()
B_SPLINE_CURVE(2,(#71857,#71858,#71859),.UNSPECIFIED.,.F.,.F.)
B_SPLINE_CURVE_WITH_KNOTS((3,3),(0.249954652430651,0.256253455718065),
 .UNSPECIFIED.)
CURVE()
GEOMETRIC_REPRESENTATION_ITEM()
RATIONAL_B_SPLINE_CURVE((1.1197173596461,1.12024119946956,1.12071541658432))
REPRESENTATION_ITEM('')
);
#1462=(
BOUNDED_CURVE()
B_SPLINE_CURVE(2,(#71863,#71864,#71865),.UNSPECIFIED.,.F.,.F.)
B_SPLINE_CURVE_WITH_KNOTS((3,3),(0.376641898803522,0.382940702095932),
 .UNSPECIFIED.)
CURVE()
GEOMETRIC_REPRESENTATION_ITEM()
RATIONAL_B_SPLINE_CURVE((1.12071541658448,1.12024119946934,1.11971735964542))
REPRESENTATION_ITEM('')
);
#1463=(
BOUNDED_CURVE()
B_SPLINE_CURVE(2,(#71869,#71870,#71871),.UNSPECIFIED.,.F.,.F.)
B_SPLINE_CURVE_WITH_KNOTS((3,3),(0.249954652430654,0.256253455718068),
 .UNSPECIFIED.)
CURVE()
GEOMETRIC_REPRESENTATION_ITEM()
RATIONAL_B_SPLINE_CURVE((1.11971735964629,1.12024119946976,1.12071541658452))
REPRESENTATION_ITEM('')
);
#1464=(
BOUNDED_CURVE()
B_SPLINE_CURVE(2,(#71875,#71876,#71877),.UNSPECIFIED.,.F.,.F.)
B_SPLINE_CURVE_WITH_KNOTS((3,3),(0.376641898803521,0.382940702095935),
 .UNSPECIFIED.)
CURVE()
GEOMETRIC_REPRESENTATION_ITEM()
RATIONAL_B_SPLINE_CURVE((1.12071541658442,1.12024119946928,1.11971735964536))
REPRESENTATION_ITEM('')
);
#1465=(
BOUNDED_CURVE()
B_SPLINE_CURVE(2,(#71881,#71882,#71883),.UNSPECIFIED.,.F.,.F.)
B_SPLINE_CURVE_WITH_KNOTS((3,3),(0.24995465243066,0.256253455718076),
 .UNSPECIFIED.)
CURVE()
GEOMETRIC_REPRESENTATION_ITEM()
RATIONAL_B_SPLINE_CURVE((1.11971735964628,1.12024119946975,1.12071541658451))
REPRESENTATION_ITEM('')
);
#1466=(
BOUNDED_CURVE()
B_SPLINE_CURVE(2,(#71887,#71888,#71889),.UNSPECIFIED.,.F.,.F.)
B_SPLINE_CURVE_WITH_KNOTS((3,3),(0.37664189880352,0.382940702095931),
 .UNSPECIFIED.)
CURVE()
GEOMETRIC_REPRESENTATION_ITEM()
RATIONAL_B_SPLINE_CURVE((1.12071541658452,1.12024119946938,1.11971735964546))
REPRESENTATION_ITEM('')
);
#1467=(
BOUNDED_CURVE()
B_SPLINE_CURVE(2,(#71893,#71894,#71895),.UNSPECIFIED.,.F.,.F.)
B_SPLINE_CURVE_WITH_KNOTS((3,3),(0.249954652430663,0.25625345571808),
 .UNSPECIFIED.)
CURVE()
GEOMETRIC_REPRESENTATION_ITEM()
RATIONAL_B_SPLINE_CURVE((1.11971735964629,1.12024119946975,1.12071541658451))
REPRESENTATION_ITEM('')
);
#1468=(
BOUNDED_CURVE()
B_SPLINE_CURVE(2,(#71899,#71900,#71901),.UNSPECIFIED.,.F.,.F.)
B_SPLINE_CURVE_WITH_KNOTS((3,3),(0.376641898803514,0.382940702095925),
 .UNSPECIFIED.)
CURVE()
GEOMETRIC_REPRESENTATION_ITEM()
RATIONAL_B_SPLINE_CURVE((1.12071541658449,1.12024119946936,1.11971735964544))
REPRESENTATION_ITEM('')
);
#1469=(
BOUNDED_CURVE()
B_SPLINE_CURVE(2,(#71905,#71906,#71907),.UNSPECIFIED.,.F.,.F.)
B_SPLINE_CURVE_WITH_KNOTS((3,3),(0.249954652430668,0.25625345571808),
 .UNSPECIFIED.)
CURVE()
GEOMETRIC_REPRESENTATION_ITEM()
RATIONAL_B_SPLINE_CURVE((1.11971735964628,1.12024119946974,1.1207154165845))
REPRESENTATION_ITEM('')
);
#1470=(
BOUNDED_CURVE()
B_SPLINE_CURVE(2,(#71911,#71912,#71913),.UNSPECIFIED.,.F.,.F.)
B_SPLINE_CURVE_WITH_KNOTS((3,3),(0.376641898803516,0.382940702095925),
 .UNSPECIFIED.)
CURVE()
GEOMETRIC_REPRESENTATION_ITEM()
RATIONAL_B_SPLINE_CURVE((1.1207154165845,1.12024119946936,1.11971735964544))
REPRESENTATION_ITEM('')
);
#1471=(
BOUNDED_CURVE()
B_SPLINE_CURVE(2,(#71917,#71918,#71919),.UNSPECIFIED.,.F.,.F.)
B_SPLINE_CURVE_WITH_KNOTS((3,3),(0.24995465243065,0.256253455718064),
 .UNSPECIFIED.)
CURVE()
GEOMETRIC_REPRESENTATION_ITEM()
RATIONAL_B_SPLINE_CURVE((1.11971735964608,1.12024119946955,1.1207154165843))
REPRESENTATION_ITEM('')
);
#1472=(
BOUNDED_CURVE()
B_SPLINE_CURVE(2,(#71923,#71924,#71925),.UNSPECIFIED.,.F.,.F.)
B_SPLINE_CURVE_WITH_KNOTS((3,3),(0.376641898803537,0.382940702095953),
 .UNSPECIFIED.)
CURVE()
GEOMETRIC_REPRESENTATION_ITEM()
RATIONAL_B_SPLINE_CURVE((1.12071541658421,1.12024119946908,1.11971735964516))
REPRESENTATION_ITEM('')
);
#1473=(
BOUNDED_CURVE()
B_SPLINE_CURVE(2,(#71929,#71930,#71931),.UNSPECIFIED.,.F.,.F.)
B_SPLINE_CURVE_WITH_KNOTS((3,3),(0.249954652430652,0.256253455718068),
 .UNSPECIFIED.)
CURVE()
GEOMETRIC_REPRESENTATION_ITEM()
RATIONAL_B_SPLINE_CURVE((1.11971735964626,1.12024119946972,1.12071541658448))
REPRESENTATION_ITEM('')
);
#1474=(
BOUNDED_CURVE()
B_SPLINE_CURVE(2,(#71935,#71936,#71937),.UNSPECIFIED.,.F.,.F.)
B_SPLINE_CURVE_WITH_KNOTS((3,3),(0.376641898803534,0.382940702095941),
 .UNSPECIFIED.)
CURVE()
GEOMETRIC_REPRESENTATION_ITEM()
RATIONAL_B_SPLINE_CURVE((1.12071541658423,1.1202411994691,1.11971735964518))
REPRESENTATION_ITEM('')
);
#1475=(
BOUNDED_CURVE()
B_SPLINE_CURVE(2,(#71941,#71942,#71943),.UNSPECIFIED.,.F.,.F.)
B_SPLINE_CURVE_WITH_KNOTS((3,3),(0.249954652430639,0.256253455718054),
 .UNSPECIFIED.)
CURVE()
GEOMETRIC_REPRESENTATION_ITEM()
RATIONAL_B_SPLINE_CURVE((1.11971735964598,1.12024119946944,1.1207154165842))
REPRESENTATION_ITEM('')
);
#1476=(
BOUNDED_CURVE()
B_SPLINE_CURVE(2,(#71947,#71948,#71949),.UNSPECIFIED.,.F.,.F.)
B_SPLINE_CURVE_WITH_KNOTS((3,3),(0.376641898803521,0.382940702095926),
 .UNSPECIFIED.)
CURVE()
GEOMETRIC_REPRESENTATION_ITEM()
RATIONAL_B_SPLINE_CURVE((1.12071541658441,1.12024119946928,1.11971735964536))
REPRESENTATION_ITEM('')
);
#1477=(
BOUNDED_CURVE()
B_SPLINE_CURVE(2,(#71953,#71954,#71955),.UNSPECIFIED.,.F.,.F.)
B_SPLINE_CURVE_WITH_KNOTS((3,3),(0.249954652430644,0.256253455718059),
 .UNSPECIFIED.)
CURVE()
GEOMETRIC_REPRESENTATION_ITEM()
RATIONAL_B_SPLINE_CURVE((1.11971735964605,1.12024119946951,1.12071541658427))
REPRESENTATION_ITEM('')
);
#1478=(
BOUNDED_CURVE()
B_SPLINE_CURVE(2,(#71959,#71960,#71961),.UNSPECIFIED.,.F.,.F.)
B_SPLINE_CURVE_WITH_KNOTS((3,3),(0.376641898803522,0.382940702095933),
 .UNSPECIFIED.)
CURVE()
GEOMETRIC_REPRESENTATION_ITEM()
RATIONAL_B_SPLINE_CURVE((1.12071541658452,1.12024119946939,1.11971735964547))
REPRESENTATION_ITEM('')
);
#1479=(
BOUNDED_CURVE()
B_SPLINE_CURVE(2,(#71965,#71966,#71967),.UNSPECIFIED.,.F.,.F.)
B_SPLINE_CURVE_WITH_KNOTS((3,3),(0.249954652430652,0.256253455718069),
 .UNSPECIFIED.)
CURVE()
GEOMETRIC_REPRESENTATION_ITEM()
RATIONAL_B_SPLINE_CURVE((1.11971735964616,1.12024119946962,1.12071541658438))
REPRESENTATION_ITEM('')
);
#1480=(
BOUNDED_CURVE()
B_SPLINE_CURVE(2,(#71971,#71972,#71973),.UNSPECIFIED.,.F.,.F.)
B_SPLINE_CURVE_WITH_KNOTS((3,3),(0.376641898803538,0.38294070209595),
 .UNSPECIFIED.)
CURVE()
GEOMETRIC_REPRESENTATION_ITEM()
RATIONAL_B_SPLINE_CURVE((1.12071541658426,1.12024119946913,1.11971735964521))
REPRESENTATION_ITEM('')
);
#1481=(
BOUNDED_CURVE()
B_SPLINE_CURVE(2,(#71976,#71977,#71978),.UNSPECIFIED.,.F.,.F.)
B_SPLINE_CURVE_WITH_KNOTS((3,3),(0.249954652430655,0.256253455718073),
 .UNSPECIFIED.)
CURVE()
GEOMETRIC_REPRESENTATION_ITEM()
RATIONAL_B_SPLINE_CURVE((1.11971735964623,1.1202411994697,1.12071541658446))
REPRESENTATION_ITEM('')
);
#1482=(
BOUNDED_CURVE()
B_SPLINE_CURVE(2,(#71980,#71981,#71982),.UNSPECIFIED.,.F.,.F.)
B_SPLINE_CURVE_WITH_KNOTS((3,3),(0.376641898803523,0.38294070209594),
 .UNSPECIFIED.)
CURVE()
GEOMETRIC_REPRESENTATION_ITEM()
RATIONAL_B_SPLINE_CURVE((1.12071541658441,1.12024119946928,1.11971735964536))
REPRESENTATION_ITEM('')
);
#1483=(
BOUNDED_CURVE()
B_SPLINE_CURVE(2,(#71985,#71986,#71987),.UNSPECIFIED.,.F.,.F.)
B_SPLINE_CURVE_WITH_KNOTS((3,3),(0.249954652430659,0.256253455718073),
 .UNSPECIFIED.)
CURVE()
GEOMETRIC_REPRESENTATION_ITEM()
RATIONAL_B_SPLINE_CURVE((1.11971735964623,1.12024119946969,1.12071541658445))
REPRESENTATION_ITEM('')
);
#1484=(
BOUNDED_CURVE()
B_SPLINE_CURVE(2,(#71989,#71990,#71991),.UNSPECIFIED.,.F.,.F.)
B_SPLINE_CURVE_WITH_KNOTS((3,3),(0.376641898803521,0.382940702095929),
 .UNSPECIFIED.)
CURVE()
GEOMETRIC_REPRESENTATION_ITEM()
RATIONAL_B_SPLINE_CURVE((1.12071541658454,1.1202411994694,1.11971735964548))
REPRESENTATION_ITEM('')
);
#1485=(
BOUNDED_CURVE()
B_SPLINE_CURVE(2,(#71994,#71995,#71996),.UNSPECIFIED.,.F.,.F.)
B_SPLINE_CURVE_WITH_KNOTS((3,3),(0.249954652430646,0.256253455718056),
 .UNSPECIFIED.)
CURVE()
GEOMETRIC_REPRESENTATION_ITEM()
RATIONAL_B_SPLINE_CURVE((1.11971735964596,1.12024119946942,1.12071541658418))
REPRESENTATION_ITEM('')
);
#1486=(
BOUNDED_CURVE()
B_SPLINE_CURVE(2,(#71998,#71999,#72000),.UNSPECIFIED.,.F.,.F.)
B_SPLINE_CURVE_WITH_KNOTS((3,3),(0.376641898803528,0.382940702095943),
 .UNSPECIFIED.)
CURVE()
GEOMETRIC_REPRESENTATION_ITEM()
RATIONAL_B_SPLINE_CURVE((1.12071541658433,1.1202411994692,1.11971735964528))
REPRESENTATION_ITEM('')
);
#1487=(
BOUNDED_CURVE()
B_SPLINE_CURVE(2,(#72003,#72004,#72005),.UNSPECIFIED.,.F.,.F.)
B_SPLINE_CURVE_WITH_KNOTS((3,3),(0.24995465243066,0.256253455718077),
 .UNSPECIFIED.)
CURVE()
GEOMETRIC_REPRESENTATION_ITEM()
RATIONAL_B_SPLINE_CURVE((1.11971735964636,1.12024119946983,1.12071541658459))
REPRESENTATION_ITEM('')
);
#1488=(
BOUNDED_CURVE()
B_SPLINE_CURVE(2,(#72007,#72008,#72009),.UNSPECIFIED.,.F.,.F.)
B_SPLINE_CURVE_WITH_KNOTS((3,3),(0.376641898803527,0.382940702095942),
 .UNSPECIFIED.)
CURVE()
GEOMETRIC_REPRESENTATION_ITEM()
RATIONAL_B_SPLINE_CURVE((1.12071541658443,1.12024119946929,1.11971735964537))
REPRESENTATION_ITEM('')
);
#1489=(
BOUNDED_CURVE()
B_SPLINE_CURVE(2,(#72012,#72013,#72014),.UNSPECIFIED.,.F.,.F.)
B_SPLINE_CURVE_WITH_KNOTS((3,3),(0.249954652430663,0.256253455718073),
 .UNSPECIFIED.)
CURVE()
GEOMETRIC_REPRESENTATION_ITEM()
RATIONAL_B_SPLINE_CURVE((1.11971735964622,1.12024119946969,1.12071541658445))
REPRESENTATION_ITEM('')
);
#1490=(
BOUNDED_CURVE()
B_SPLINE_CURVE(2,(#72016,#72017,#72018),.UNSPECIFIED.,.F.,.F.)
B_SPLINE_CURVE_WITH_KNOTS((3,3),(0.376641898803534,0.382940702095947),
 .UNSPECIFIED.)
CURVE()
GEOMETRIC_REPRESENTATION_ITEM()
RATIONAL_B_SPLINE_CURVE((1.12071541658425,1.12024119946912,1.1197173596452))
REPRESENTATION_ITEM('')
);
#1491=(
BOUNDED_CURVE()
B_SPLINE_CURVE(2,(#72021,#72022,#72023),.UNSPECIFIED.,.F.,.F.)
B_SPLINE_CURVE_WITH_KNOTS((3,3),(0.249954652430658,0.256253455718067),
 .UNSPECIFIED.)
CURVE()
GEOMETRIC_REPRESENTATION_ITEM()
RATIONAL_B_SPLINE_CURVE((1.1197173596462,1.12024119946966,1.12071541658442))
REPRESENTATION_ITEM('')
);
#1492=(
BOUNDED_CURVE()
B_SPLINE_CURVE(2,(#72025,#72026,#72027),.UNSPECIFIED.,.F.,.F.)
B_SPLINE_CURVE_WITH_KNOTS((3,3),(0.376641898803512,0.382940702095926),
 .UNSPECIFIED.)
CURVE()
GEOMETRIC_REPRESENTATION_ITEM()
RATIONAL_B_SPLINE_CURVE((1.12071541658454,1.12024119946941,1.11971735964549))
REPRESENTATION_ITEM('')
);
#1493=(
BOUNDED_CURVE()
B_SPLINE_CURVE(2,(#72030,#72031,#72032),.UNSPECIFIED.,.F.,.F.)
B_SPLINE_CURVE_WITH_KNOTS((3,3),(0.249954652430648,0.256253455718064),
 .UNSPECIFIED.)
CURVE()
GEOMETRIC_REPRESENTATION_ITEM()
RATIONAL_B_SPLINE_CURVE((1.11971735964605,1.12024119946951,1.12071541658427))
REPRESENTATION_ITEM('')
);
#1494=(
BOUNDED_CURVE()
B_SPLINE_CURVE(2,(#72034,#72035,#72036),.UNSPECIFIED.,.F.,.F.)
B_SPLINE_CURVE_WITH_KNOTS((3,3),(0.37664189880353,0.382940702095945),
 .UNSPECIFIED.)
CURVE()
GEOMETRIC_REPRESENTATION_ITEM()
RATIONAL_B_SPLINE_CURVE((1.12071541658432,1.12024119946919,1.11971735964527))
REPRESENTATION_ITEM('')
);
#1495=(
BOUNDED_CURVE()
B_SPLINE_CURVE(2,(#72039,#72040,#72041),.UNSPECIFIED.,.F.,.F.)
B_SPLINE_CURVE_WITH_KNOTS((3,3),(0.24995465243065,0.256253455718062),
 .UNSPECIFIED.)
CURVE()
GEOMETRIC_REPRESENTATION_ITEM()
RATIONAL_B_SPLINE_CURVE((1.1197173596462,1.12024119946966,1.12071541658442))
REPRESENTATION_ITEM('')
);
#1496=(
BOUNDED_CURVE()
B_SPLINE_CURVE(2,(#72043,#72044,#72045),.UNSPECIFIED.,.F.,.F.)
B_SPLINE_CURVE_WITH_KNOTS((3,3),(0.376641898803514,0.382940702095926),
 .UNSPECIFIED.)
CURVE()
GEOMETRIC_REPRESENTATION_ITEM()
RATIONAL_B_SPLINE_CURVE((1.12071541658458,1.12024119946944,1.11971735964552))
REPRESENTATION_ITEM('')
);
#1497=(
BOUNDED_CURVE()
B_SPLINE_CURVE(2,(#72048,#72049,#72050),.UNSPECIFIED.,.F.,.F.)
B_SPLINE_CURVE_WITH_KNOTS((3,3),(0.249954652430654,0.256253455718075),
 .UNSPECIFIED.)
CURVE()
GEOMETRIC_REPRESENTATION_ITEM()
RATIONAL_B_SPLINE_CURVE((1.11971735964632,1.12024119946978,1.12071541658454))
REPRESENTATION_ITEM('')
);
#1498=(
BOUNDED_CURVE()
B_SPLINE_CURVE(2,(#72052,#72053,#72054),.UNSPECIFIED.,.F.,.F.)
B_SPLINE_CURVE_WITH_KNOTS((3,3),(0.376641898803524,0.382940702095939),
 .UNSPECIFIED.)
CURVE()
GEOMETRIC_REPRESENTATION_ITEM()
RATIONAL_B_SPLINE_CURVE((1.12071541658443,1.1202411994693,1.11971735964538))
REPRESENTATION_ITEM('')
);
#1499=(
BOUNDED_CURVE()
B_SPLINE_CURVE(2,(#72057,#72058,#72059),.UNSPECIFIED.,.F.,.F.)
B_SPLINE_CURVE_WITH_KNOTS((3,3),(0.249954652430651,0.256253455718065),
 .UNSPECIFIED.)
CURVE()
GEOMETRIC_REPRESENTATION_ITEM()
RATIONAL_B_SPLINE_CURVE((1.11971735964614,1.12024119946961,1.12071541658437))
REPRESENTATION_ITEM('')
);
#1500=(
BOUNDED_CURVE()
B_SPLINE_CURVE(2,(#72061,#72062,#72063),.UNSPECIFIED.,.F.,.F.)
B_SPLINE_CURVE_WITH_KNOTS((3,3),(0.376641898803524,0.382940702095937),
 .UNSPECIFIED.)
CURVE()
GEOMETRIC_REPRESENTATION_ITEM()
RATIONAL_B_SPLINE_CURVE((1.12071541658443,1.1202411994693,1.11971735964538))
REPRESENTATION_ITEM('')
);
#1501=(
BOUNDED_CURVE()
B_SPLINE_CURVE(2,(#72066,#72067,#72068),.UNSPECIFIED.,.F.,.F.)
B_SPLINE_CURVE_WITH_KNOTS((3,3),(0.24995465243066,0.256253455718078),
 .UNSPECIFIED.)
CURVE()
GEOMETRIC_REPRESENTATION_ITEM()
RATIONAL_B_SPLINE_CURVE((1.11971735964625,1.12024119946971,1.12071541658447))
REPRESENTATION_ITEM('')
);
#1502=(
BOUNDED_CURVE()
B_SPLINE_CURVE(2,(#72070,#72071,#72072),.UNSPECIFIED.,.F.,.F.)
B_SPLINE_CURVE_WITH_KNOTS((3,3),(0.376641898803522,0.382940702095931),
 .UNSPECIFIED.)
CURVE()
GEOMETRIC_REPRESENTATION_ITEM()
RATIONAL_B_SPLINE_CURVE((1.1207154165845,1.12024119946936,1.11971735964544))
REPRESENTATION_ITEM('')
);
#1503=(
BOUNDED_CURVE()
B_SPLINE_CURVE(2,(#72075,#72076,#72077),.UNSPECIFIED.,.F.,.F.)
B_SPLINE_CURVE_WITH_KNOTS((3,3),(0.249954652430652,0.256253455718071),
 .UNSPECIFIED.)
CURVE()
GEOMETRIC_REPRESENTATION_ITEM()
RATIONAL_B_SPLINE_CURVE((1.11971735964614,1.12024119946961,1.12071541658437))
REPRESENTATION_ITEM('')
);
#1504=(
BOUNDED_CURVE()
B_SPLINE_CURVE(2,(#72079,#72080,#72081),.UNSPECIFIED.,.F.,.F.)
B_SPLINE_CURVE_WITH_KNOTS((3,3),(0.376641898803528,0.382940702095942),
 .UNSPECIFIED.)
CURVE()
GEOMETRIC_REPRESENTATION_ITEM()
RATIONAL_B_SPLINE_CURVE((1.12071541658436,1.12024119946922,1.1197173596453))
REPRESENTATION_ITEM('')
);
#1505=(
BOUNDED_CURVE()
B_SPLINE_CURVE(2,(#72084,#72085,#72086),.UNSPECIFIED.,.F.,.F.)
B_SPLINE_CURVE_WITH_KNOTS((3,3),(0.249954652430651,0.256253455718071),
 .UNSPECIFIED.)
CURVE()
GEOMETRIC_REPRESENTATION_ITEM()
RATIONAL_B_SPLINE_CURVE((1.11971735964609,1.12024119946955,1.12071541658431))
REPRESENTATION_ITEM('')
);
#1506=(
BOUNDED_CURVE()
B_SPLINE_CURVE(2,(#72088,#72089,#72090),.UNSPECIFIED.,.F.,.F.)
B_SPLINE_CURVE_WITH_KNOTS((3,3),(0.376641898803537,0.382940702095949),
 .UNSPECIFIED.)
CURVE()
GEOMETRIC_REPRESENTATION_ITEM()
RATIONAL_B_SPLINE_CURVE((1.12071541658424,1.1202411994691,1.11971735964519))
REPRESENTATION_ITEM('')
);
#1507=(
BOUNDED_CURVE()
B_SPLINE_CURVE(2,(#72093,#72094,#72095),.UNSPECIFIED.,.F.,.F.)
B_SPLINE_CURVE_WITH_KNOTS((3,3),(0.249954652430663,0.256253455718077),
 .UNSPECIFIED.)
CURVE()
GEOMETRIC_REPRESENTATION_ITEM()
RATIONAL_B_SPLINE_CURVE((1.11971735964627,1.12024119946974,1.1207154165845))
REPRESENTATION_ITEM('')
);
#1508=(
BOUNDED_CURVE()
B_SPLINE_CURVE(2,(#72097,#72098,#72099),.UNSPECIFIED.,.F.,.F.)
B_SPLINE_CURVE_WITH_KNOTS((3,3),(0.376641898803535,0.382940702095948),
 .UNSPECIFIED.)
CURVE()
GEOMETRIC_REPRESENTATION_ITEM()
RATIONAL_B_SPLINE_CURVE((1.12071541658433,1.1202411994692,1.11971735964528))
REPRESENTATION_ITEM('')
);
#1509=(
BOUNDED_CURVE()
B_SPLINE_CURVE(2,(#72102,#72103,#72104),.UNSPECIFIED.,.F.,.F.)
B_SPLINE_CURVE_WITH_KNOTS((3,3),(0.249954652430657,0.256253455718068),
 .UNSPECIFIED.)
CURVE()
GEOMETRIC_REPRESENTATION_ITEM()
RATIONAL_B_SPLINE_CURVE((1.11971735964623,1.1202411994697,1.12071541658445))
REPRESENTATION_ITEM('')
);
#1510=(
BOUNDED_CURVE()
B_SPLINE_CURVE(2,(#72106,#72107,#72108),.UNSPECIFIED.,.F.,.F.)
B_SPLINE_CURVE_WITH_KNOTS((3,3),(0.376641898803534,0.382940702095946),
 .UNSPECIFIED.)
CURVE()
GEOMETRIC_REPRESENTATION_ITEM()
RATIONAL_B_SPLINE_CURVE((1.12071541658428,1.12024119946915,1.11971735964523))
REPRESENTATION_ITEM('')
);
#1511=(
BOUNDED_CURVE()
B_SPLINE_CURVE(2,(#72112,#72113,#72114),.UNSPECIFIED.,.F.,.F.)
B_SPLINE_CURVE_WITH_KNOTS((3,3),(0.249954652430652,0.256253455718065),
 .UNSPECIFIED.)
CURVE()
GEOMETRIC_REPRESENTATION_ITEM()
RATIONAL_B_SPLINE_CURVE((1.11971735964615,1.12024119946961,1.12071541658437))
REPRESENTATION_ITEM('')
);
#1512=(
BOUNDED_CURVE()
B_SPLINE_CURVE(2,(#72118,#72119,#72120),.UNSPECIFIED.,.F.,.F.)
B_SPLINE_CURVE_WITH_KNOTS((3,3),(0.376641898803528,0.38294070209594),
 .UNSPECIFIED.)
CURVE()
GEOMETRIC_REPRESENTATION_ITEM()
RATIONAL_B_SPLINE_CURVE((1.12071541658438,1.12024119946925,1.11971735964533))
REPRESENTATION_ITEM('')
);
#1513=(
BOUNDED_CURVE()
B_SPLINE_CURVE(2,(#72124,#72125,#72126),.UNSPECIFIED.,.F.,.F.)
B_SPLINE_CURVE_WITH_KNOTS((3,3),(0.249954652430646,0.256253455718057),
 .UNSPECIFIED.)
CURVE()
GEOMETRIC_REPRESENTATION_ITEM()
RATIONAL_B_SPLINE_CURVE((1.11971735964604,1.12024119946951,1.12071541658426))
REPRESENTATION_ITEM('')
);
#1514=(
BOUNDED_CURVE()
B_SPLINE_CURVE(2,(#72130,#72131,#72132),.UNSPECIFIED.,.F.,.F.)
B_SPLINE_CURVE_WITH_KNOTS((3,3),(0.376641898803525,0.382940702095939),
 .UNSPECIFIED.)
CURVE()
GEOMETRIC_REPRESENTATION_ITEM()
RATIONAL_B_SPLINE_CURVE((1.12071541658443,1.1202411994693,1.11971735964538))
REPRESENTATION_ITEM('')
);
#1515=(
BOUNDED_CURVE()
B_SPLINE_CURVE(2,(#72136,#72137,#72138),.UNSPECIFIED.,.F.,.F.)
B_SPLINE_CURVE_WITH_KNOTS((3,3),(0.249954652430639,0.256253455718051),
 .UNSPECIFIED.)
CURVE()
GEOMETRIC_REPRESENTATION_ITEM()
RATIONAL_B_SPLINE_CURVE((1.11971735964598,1.12024119946945,1.1207154165842))
REPRESENTATION_ITEM('')
);
#1516=(
BOUNDED_CURVE()
B_SPLINE_CURVE(2,(#72142,#72143,#72144),.UNSPECIFIED.,.F.,.F.)
B_SPLINE_CURVE_WITH_KNOTS((3,3),(0.376641898803521,0.382940702095934),
 .UNSPECIFIED.)
CURVE()
GEOMETRIC_REPRESENTATION_ITEM()
RATIONAL_B_SPLINE_CURVE((1.12071541658441,1.12024119946928,1.11971735964536))
REPRESENTATION_ITEM('')
);
#1517=(
BOUNDED_CURVE()
B_SPLINE_CURVE(2,(#72148,#72149,#72150),.UNSPECIFIED.,.F.,.F.)
B_SPLINE_CURVE_WITH_KNOTS((3,3),(0.249954652430652,0.256253455718065),
 .UNSPECIFIED.)
CURVE()
GEOMETRIC_REPRESENTATION_ITEM()
RATIONAL_B_SPLINE_CURVE((1.11971735964616,1.12024119946962,1.12071541658438))
REPRESENTATION_ITEM('')
);
#1518=(
BOUNDED_CURVE()
B_SPLINE_CURVE(2,(#72154,#72155,#72156),.UNSPECIFIED.,.F.,.F.)
B_SPLINE_CURVE_WITH_KNOTS((3,3),(0.376641898803544,0.382940702095957),
 .UNSPECIFIED.)
CURVE()
GEOMETRIC_REPRESENTATION_ITEM()
RATIONAL_B_SPLINE_CURVE((1.12071541658424,1.1202411994691,1.11971735964518))
REPRESENTATION_ITEM('')
);
#1519=(
BOUNDED_CURVE()
B_SPLINE_CURVE(2,(#72160,#72161,#72162),.UNSPECIFIED.,.F.,.F.)
B_SPLINE_CURVE_WITH_KNOTS((3,3),(0.249954652430643,0.256253455718053),
 .UNSPECIFIED.)
CURVE()
GEOMETRIC_REPRESENTATION_ITEM()
RATIONAL_B_SPLINE_CURVE((1.11971735964601,1.12024119946947,1.12071541658423))
REPRESENTATION_ITEM('')
);
#1520=(
BOUNDED_CURVE()
B_SPLINE_CURVE(2,(#72166,#72167,#72168),.UNSPECIFIED.,.F.,.F.)
B_SPLINE_CURVE_WITH_KNOTS((3,3),(0.376641898803543,0.382940702095953),
 .UNSPECIFIED.)
CURVE()
GEOMETRIC_REPRESENTATION_ITEM()
RATIONAL_B_SPLINE_CURVE((1.12071541658425,1.12024119946911,1.1197173596452))
REPRESENTATION_ITEM('')
);
#1521=(
BOUNDED_CURVE()
B_SPLINE_CURVE(2,(#72172,#72173,#72174),.UNSPECIFIED.,.F.,.F.)
B_SPLINE_CURVE_WITH_KNOTS((3,3),(0.249954652430649,0.256253455718062),
 .UNSPECIFIED.)
CURVE()
GEOMETRIC_REPRESENTATION_ITEM()
RATIONAL_B_SPLINE_CURVE((1.11971735964607,1.12024119946954,1.12071541658429))
REPRESENTATION_ITEM('')
);
#1522=ELLIPSE('',#32268,0.0195162536838815,0.0137573643715162);
#1523=ELLIPSE('',#32269,0.0195162536830269,0.0137573643713391);
#1524=ELLIPSE('',#32271,0.0195162536835621,0.0137573643714695);
#1525=ELLIPSE('',#32272,0.019516253683001,0.0137573643713521);
#1526=ELLIPSE('',#32274,0.0195162536836977,0.0137573643714721);
#1527=ELLIPSE('',#32275,0.0195162536830636,0.0137573643713535);
#1528=ELLIPSE('',#32277,0.0195162536837443,0.0137573643714943);
#1529=ELLIPSE('',#32278,0.0195162536831223,0.0137573643713688);
#1530=ELLIPSE('',#32280,0.019516253683803,0.013757364371504);
#1531=ELLIPSE('',#32281,0.0195162536829111,0.0137573643713217);
#1532=ELLIPSE('',#32283,0.0195162536837688,0.0137573643714986);
#1533=ELLIPSE('',#32284,0.0195162536830749,0.0137573643713556);
#1534=ELLIPSE('',#32286,0.0195162536837257,0.0137573643714922);
#1535=ELLIPSE('',#32287,0.0195162536830703,0.0137573643713494);
#1536=ELLIPSE('',#32289,0.0195162536838104,0.013757364371505);
#1537=ELLIPSE('',#32290,0.0195162536830614,0.0137573643713493);
#1538=ELLIPSE('',#32292,0.0195162536837473,0.0137573643714877);
#1539=ELLIPSE('',#32293,0.0195162536830537,0.0137573643713548);
#1540=ELLIPSE('',#32295,0.0195162536838422,0.0137573643715182);
#1541=ELLIPSE('',#32296,0.0195162536831755,0.0137573643713807);
#1542=ELLIPSE('',#32298,0.0195162536837639,0.0137573643714952);
#1543=ELLIPSE('',#32299,0.0195162536830792,0.0137573643713542);
#1544=ELLIPSE('',#32301,0.0195162536835653,0.0137573643714501);
#1545=ELLIPSE('',#32302,0.0195162536831025,0.0137573643713567);
#1546=ELLIPSE('',#32304,0.0195162536835776,0.0137573643714587);
#1547=ELLIPSE('',#32305,0.0195162536828947,0.01375736437132);
#1548=ELLIPSE('',#32307,0.0195162536837483,0.0137573643714995);
#1549=ELLIPSE('',#32308,0.0195162536831204,0.0137573643713664);
#1550=ELLIPSE('',#32310,0.0195162536835793,0.0137573643714601);
#1551=ELLIPSE('',#32311,0.0195162536830448,0.0137573643713492);
#1552=ELLIPSE('',#32320,0.0195034997306777,0.013754915723726);
#1553=ELLIPSE('',#32322,0.0195030685020683,0.0137548403891227);
#1554=ELLIPSE('',#32324,0.0195027524929284,0.0137547851848027);
#1555=ELLIPSE('',#32326,0.0195025132809572,0.0137547433941177);
#1556=ELLIPSE('',#32328,0.0195023280193677,0.0137547110253133);
#1557=ELLIPSE('',#32330,0.0195021823053853,0.0137546855626127);
#1558=ELLIPSE('',#32332,0.0195020666474465,0.0137546653482711);
#1559=ELLIPSE('',#32334,0.0195019745733047,0.0137546492518586);
#1560=ELLIPSE('',#32336,0.0195019015620118,0.0137546364836367);
#1561=ELLIPSE('',#32338,0.0195018443987318,0.0137546264818649);
#1562=ELLIPSE('',#32340,0.0195018007910573,0.0137546188457545);
#1563=ELLIPSE('',#32342,0.0195017691158091,0.0137546132912077);
#1564=ELLIPSE('',#32344,0.0195017482624769,0.0137546096234092);
#1565=ELLIPSE('',#32346,0.0195017375337946,0.0137546077193674);
#1566=ELLIPSE('',#32348,0.0195017365885567,0.0137546075177427);
#1567=ELLIPSE('',#32350,0.0195017454175912,0.0137546090143427);
#1568=ELLIPSE('',#32352,0.0195017643506138,0.0137546122627749);
#1569=ELLIPSE('',#32354,0.0195017941005044,0.0137546173811011);
#1570=ELLIPSE('',#32356,0.0195018358641676,0.0137546245672221);
#1571=ELLIPSE('',#32358,0.0195018727625836,0.013754631431718);
#1572=ELLIPSE('',#32360,0.0195034997306828,0.0137549157237274);
#1573=ELLIPSE('',#32362,0.0195030685021256,0.0137548403891337);
#1574=ELLIPSE('',#32364,0.0195027524929019,0.0137547851847966);
#1575=ELLIPSE('',#32366,0.0195025132809425,0.0137547433941156);
#1576=ELLIPSE('',#32368,0.0195023280193708,0.0137547110253143);
#1577=ELLIPSE('',#32370,0.0195021823053841,0.0137546855626124);
#1578=ELLIPSE('',#32372,0.0195020666474398,0.0137546653482691);
#1579=ELLIPSE('',#32374,0.0195019745733335,0.0137546492518631);
#1580=ELLIPSE('',#32376,0.0195019015619959,0.0137546364836322);
#1581=ELLIPSE('',#32378,0.0195018443987879,0.0137546264818748);
#1582=ELLIPSE('',#32380,0.0195018007910457,0.0137546188457536);
#1583=ELLIPSE('',#32382,0.0195017691158159,0.0137546132912084);
#1584=ELLIPSE('',#32384,0.0195017482624727,0.013754609623408);
#1585=ELLIPSE('',#32386,0.0195017375337736,0.0137546077193644);
#1586=ELLIPSE('',#32388,0.0195017365885347,0.0137546075177382);
#1587=ELLIPSE('',#32390,0.019501745417596,0.0137546090143437);
#1588=ELLIPSE('',#32392,0.0195017643505816,0.0137546122627688);
#1589=ELLIPSE('',#32394,0.0195017941005605,0.0137546173811125);
#1590=ELLIPSE('',#32396,0.019501835864167,0.0137546245672222);
#1591=ELLIPSE('',#32398,0.0195162536830855,0.0137573643713537);
#1592=ELLIPSE('',#32400,0.0195034997307414,0.013754915723739);
#1593=ELLIPSE('',#32402,0.0195030685021161,0.0137548403891323);
#1594=ELLIPSE('',#32404,0.0195027524929008,0.0137547851847961);
#1595=ELLIPSE('',#32406,0.0195025132809546,0.0137547433941189);
#1596=ELLIPSE('',#32408,0.0195023280193482,0.0137547110253084);
#1597=ELLIPSE('',#32425,0.0195034997306463,0.0137549157237206);
#1598=ELLIPSE('',#32427,0.0195030685021557,0.0137548403891397);
#1599=ELLIPSE('',#32429,0.0195027524928776,0.0137547851847918);
#1600=ELLIPSE('',#32431,0.0195025132809776,0.0137547433941213);
#1601=ELLIPSE('',#32433,0.019502328019347,0.0137547110253081);
#1602=ELLIPSE('',#32435,0.0195021823053738,0.0137546855626116);
#1603=ELLIPSE('',#32437,0.0195020666474525,0.0137546653482711);
#1604=ELLIPSE('',#32439,0.0195019745733739,0.013754649251872);
#1605=ELLIPSE('',#32441,0.0195019015619764,0.0137546364836293);
#1606=ELLIPSE('',#32443,0.0195018443987816,0.0137546264818739);
#1607=ELLIPSE('',#32445,0.0195018007910337,0.0137546188457504);
#1608=ELLIPSE('',#32447,0.0195017691158341,0.0137546132912121);
#1609=ELLIPSE('',#32449,0.0195017482624509,0.0137546096234037);
#1610=ELLIPSE('',#32451,0.0195017375337853,0.0137546077193653);
#1611=ELLIPSE('',#32453,0.0195017365886309,0.0137546075177561);
#1612=ELLIPSE('',#32455,0.0195017454176055,0.0137546090143461);
#1613=ELLIPSE('',#32457,0.0195017643505986,0.0137546122627731);
#1614=ELLIPSE('',#32459,0.0195017941005311,0.0137546173811059);
#1615=ELLIPSE('',#32461,0.0195018358641241,0.0137546245672129);
#1616=ELLIPSE('',#32465,0.0195034997306858,0.0137549157237271);
#1617=ELLIPSE('',#32467,0.0195030685021635,0.0137548403891432);
#1618=ELLIPSE('',#32469,0.019502752492881,0.0137547851847926);
#1619=ELLIPSE('',#32471,0.0195025132809236,0.0137547433941134);
#1620=ELLIPSE('',#32473,0.0195023280193679,0.0137547110253125);
#1621=ELLIPSE('',#32475,0.0195021823054267,0.0137546855626225);
#1622=ELLIPSE('',#32477,0.0195020666474927,0.0137546653482813);
#1623=ELLIPSE('',#32479,0.019501974573308,0.0137546492518591);
#1624=ELLIPSE('',#32481,0.0195019015619601,0.0137546364836262);
#1625=ELLIPSE('',#32483,0.0195018443987825,0.0137546264818736);
#1626=ELLIPSE('',#32485,0.0195018007910841,0.0137546188457617);
#1627=ELLIPSE('',#32487,0.0195017691158046,0.0137546132912069);
#1628=ELLIPSE('',#32489,0.0195017482624746,0.0137546096234107);
#1629=ELLIPSE('',#32491,0.0195017375337627,0.0137546077193623);
#1630=ELLIPSE('',#32493,0.0195017365885639,0.0137546075177438);
#1631=ELLIPSE('',#32495,0.0195017454175912,0.0137546090143448);
#1632=ELLIPSE('',#32497,0.0195017643506125,0.0137546122627745);
#1633=ELLIPSE('',#32499,0.0195017941005712,0.0137546173811145);
#1634=ELLIPSE('',#32501,0.0195018358641553,0.013754624567221);
#1635=ELLIPSE('',#32503,0.0195018727626295,0.0137546314317287);
#1636=ELLIPSE('',#32505,0.0195034997307231,0.0137549157237351);
#1637=ELLIPSE('',#32507,0.0195030685021692,0.0137548403891432);
#1638=ELLIPSE('',#32509,0.0195027524928953,0.013754785184795);
#1639=ELLIPSE('',#32511,0.0195025132809505,0.0137547433941165);
#1640=ELLIPSE('',#32513,0.0195023280194302,0.0137547110253254);
#1641=ELLIPSE('',#32515,0.019502182305463,0.0137546855626286);
#1642=ELLIPSE('',#32517,0.0195020666474861,0.0137546653482797);
#1643=ELLIPSE('',#32519,0.0195019745732981,0.0137546492518571);
#1644=ELLIPSE('',#32521,0.019501901562003,0.0137546364836345);
#1645=ELLIPSE('',#32523,0.0195018443988218,0.0137546264818824);
#1646=ELLIPSE('',#32525,0.0195018007911448,0.0137546188457728);
#1647=ELLIPSE('',#32527,0.0195017691157916,0.0137546132912057);
#1648=ELLIPSE('',#32529,0.0195017482624564,0.013754609623407);
#1649=ELLIPSE('',#32531,0.0195017375338029,0.0137546077193704);
#1650=ELLIPSE('',#32533,0.0195017365886144,0.0137546075177533);
#1651=ELLIPSE('',#32535,0.0195017454176306,0.0137546090143512);
#1652=ELLIPSE('',#32537,0.0195017643505891,0.0137546122627708);
#1653=ELLIPSE('',#32539,0.0195017941005193,0.013754617381105);
#1654=ELLIPSE('',#32541,0.0195018358642213,0.0137546245672329);
#1655=ELLIPSE('',#32543,0.0195162536837232,0.0137573643714884);
#1656=ELLIPSE('',#32545,0.0195034997306679,0.0137549157237246);
#1657=ELLIPSE('',#32547,0.0195030685021047,0.0137548403891311);
#1658=ELLIPSE('',#32549,0.0195027524929266,0.0137547851848028);
#1659=ELLIPSE('',#32551,0.0195025132809874,0.0137547433941253);
#1660=ELLIPSE('',#32553,0.0195023280194086,0.013754711025321);
#1661=ELLIPSE('',#32555,0.0195021823054203,0.0137546855626212);
#1662=ELLIPSE('',#32557,0.0195020666475111,0.0137546653482846);
#1663=ELLIPSE('',#32559,0.0195019745733549,0.0137546492518684);
#1664=ELLIPSE('',#32561,0.0195019015619592,0.0137546364836273);
#1665=ELLIPSE('',#32563,0.0195018443988324,0.0137546264818843);
#1666=ELLIPSE('',#32565,0.0195018007910703,0.0137546188457585);
#1667=ELLIPSE('',#32567,0.0195017691158645,0.0137546132912193);
#1668=ELLIPSE('',#32569,0.0195017482624579,0.0137546096234066);
#1669=ELLIPSE('',#32571,0.0195017375338027,0.0137546077193706);
#1670=ELLIPSE('',#32573,0.0195017365886083,0.0137546075177516);
#1671=ELLIPSE('',#32575,0.019501745417535,0.0137546090143326);
#1672=ELLIPSE('',#32577,0.0195017643506093,0.0137546122627733);
#1673=ELLIPSE('',#32579,0.0195017941005168,0.013754617381103);
#1674=ELLIPSE('',#32581,0.0195018358640787,0.0137546245672056);
#1675=ELLIPSE('',#32598,0.0195017365886013,0.0137546075177502);
#1676=ELLIPSE('',#32600,0.0195017454175941,0.0137546090143434);
#1677=ELLIPSE('',#32602,0.0195017643505789,0.0137546122627681);
#1678=ELLIPSE('',#32604,0.0195017941005255,0.0137546173811058);
#1679=ELLIPSE('',#32606,0.0195018358641318,0.0137546245672154);
#1680=ELLIPSE('',#32622,0.051274964768551,0.0469971417993774);
#1681=ELLIPSE('',#32624,0.0512707788579671,0.0469842741354326);
#1682=ELLIPSE('',#32626,0.0512707788562332,0.0469842741344865);
#1683=ELLIPSE('',#32627,0.0512749647685533,0.0469971417993787);
#1684=ELLIPSE('',#32630,0.0512707788571307,0.0469842741349983);
#1685=ELLIPSE('',#32631,0.0512749647672664,0.0469971417987026);
#1686=ELLIPSE('',#32634,0.0512707788571389,0.0469842741349856);
#1687=ELLIPSE('',#32635,0.0512749647681367,0.0469971417991575);
#1688=ELLIPSE('',#32638,0.0512707788569124,0.0469842741348335);
#1689=ELLIPSE('',#32639,0.051274964768467,0.0469971417993732);
#1690=ELLIPSE('',#32642,0.051270778857559,0.0469842741351648);
#1691=ELLIPSE('',#32643,0.0512749647697504,0.0469971418000396);
#1692=ELLIPSE('',#32646,0.051270778857562,0.0469842741352078);
#1693=ELLIPSE('',#32647,0.0512749647676798,0.0469971417989218);
#1694=ELLIPSE('',#32650,0.0512707788610954,0.0469842741371193);
#1695=ELLIPSE('',#32651,0.0512749647674827,0.0469971417988075);
#1696=ELLIPSE('',#32654,0.0512707788555596,0.0469842741341208);
#1697=ELLIPSE('',#32655,0.0512749647677061,0.0469971417989105);
#1698=ELLIPSE('',#32658,0.0512707788650729,0.0469842741392919);
#1699=ELLIPSE('',#32659,0.0512749647702881,0.0469971418003199);
#1700=ELLIPSE('',#32662,0.0512707788560203,0.0469842741343728);
#1701=ELLIPSE('',#32663,0.0512749647689969,0.0469971417996401);
#1702=ELLIPSE('',#32666,0.0512707788567884,0.046984274134799);
#1703=ELLIPSE('',#32667,0.0512749647681247,0.0469971417991492);
#1704=ELLIPSE('',#32670,0.0512707788573083,0.0469842741350659);
#1705=ELLIPSE('',#32671,0.0512749647690658,0.0469971417996437);
#1706=ELLIPSE('',#32674,0.0512707788615306,0.046984274137359);
#1707=ELLIPSE('',#32675,0.051274964767619,0.0469971417988856);
#1708=ELLIPSE('',#32678,0.0512707788928482,0.0469842741544496);
#1709=ELLIPSE('',#32679,0.0512749647695684,0.0469971417999069);
#1710=ELLIPSE('',#32682,0.051270778857717,0.0469842741353091);
#1711=ELLIPSE('',#32683,0.0512749647683041,0.0469971417992544);
#1712=ELLIPSE('',#32686,0.051270778855901,0.046984274134278);
#1713=ELLIPSE('',#32687,0.0512749647692079,0.0469971417997307);
#1714=ELLIPSE('',#32690,0.0512707788585063,0.0469842741357279);
#1715=ELLIPSE('',#32691,0.0512749647681597,0.0469971417991513);
#1716=ELLIPSE('',#32694,0.0512707788568602,0.0469842741348085);
#1717=ELLIPSE('',#32695,0.0512749647674443,0.0469971417987893);
#1718=ELLIPSE('',#32698,0.0512707788568387,0.0469842741347804);
#1719=ELLIPSE('',#32699,0.0512749647678151,0.0469971417990189);
#1720=ELLIPSE('',#32702,0.0512707788582789,0.0469842741356006);
#1721=ELLIPSE('',#32703,0.05127496476906,0.0469971417996405);
#1722=ELLIPSE('',#32706,0.051270778856965,0.0469842741348763);
#1723=ELLIPSE('',#32707,0.0512749647686908,0.046997141799481);
#1724=ELLIPSE('',#32710,0.0512707788563555,0.0469842741344815);
#1725=ELLIPSE('',#32711,0.0512749647673275,0.0469971417987118);
#1726=ELLIPSE('',#32714,0.0512707788571547,0.0469842741350112);
#1727=ELLIPSE('',#32715,0.0512749647685426,0.046997141799397);
#1728=ELLIPSE('',#32718,0.0512707788556612,0.0469842741341707);
#1729=ELLIPSE('',#32719,0.0512749647699517,0.0469971418001559);
#1730=ELLIPSE('',#32722,0.0512707788576472,0.0469842741352346);
#1731=ELLIPSE('',#32723,0.0512749647672529,0.0469971417986806);
#1732=ELLIPSE('',#32726,0.0512707788618793,0.0469842741375491);
#1733=ELLIPSE('',#32727,0.0512749647679756,0.0469971417990623);
#1734=ELLIPSE('',#32730,0.0512707788555002,0.0469842741340957);
#1735=ELLIPSE('',#32731,0.0512749647688844,0.046997141799544);
#1736=ELLIPSE('',#32734,0.0512707788566344,0.0469842741346946);
#1737=ELLIPSE('',#32735,0.051274964769648,0.046997141799953);
#1738=ELLIPSE('',#32738,0.0512707788584597,0.0469842741356599);
#1739=ELLIPSE('',#32739,0.0512749647679757,0.0469971417990702);
#1740=ELLIPSE('',#32742,0.0512707788568172,0.0469842741347837);
#1741=ELLIPSE('',#32743,0.051274964767697,0.0469971417989173);
#1742=ELLIPSE('',#32746,0.0512707788670663,0.0469842741404324);
#1743=ELLIPSE('',#32747,0.0512749647689531,0.0469971417995761);
#1744=ELLIPSE('',#32750,0.0512707788557115,0.0469842741341769);
#1745=ELLIPSE('',#32751,0.0512749647694815,0.0469971417999415);
#1746=ELLIPSE('',#32754,0.0512707788568934,0.0469842741348491);
#1747=ELLIPSE('',#32755,0.0512749647661315,0.0469971417980767);
#1748=ELLIPSE('',#32758,0.0512707788572177,0.0469842741350563);
#1749=ELLIPSE('',#32759,0.0512749647680353,0.0469971417991282);
#1750=ELLIPSE('',#32762,0.0512707788587383,0.046984274135853);
#1751=ELLIPSE('',#32763,0.0512749647684727,0.0469971417993084);
#1752=ELLIPSE('',#32766,0.0512707788631157,0.0469842741382362);
#1753=ELLIPSE('',#32767,0.0512749647685272,0.0469971417993756);
#1754=ELLIPSE('',#32770,0.0512707788564907,0.0469842741346169);
#1755=ELLIPSE('',#32771,0.0512749647685682,0.0469971417994032);
#1756=ELLIPSE('',#32774,0.0512707788585969,0.0469842741357701);
#1757=ELLIPSE('',#32775,0.0512749647676235,0.0469971417988947);
#1758=ELLIPSE('',#32778,0.0512707788751318,0.0469842741447984);
#1759=ELLIPSE('',#32779,0.0512749647678178,0.0469971417990053);
#1760=ELLIPSE('',#32782,0.0512707788575899,0.0469842741352132);
#1761=ELLIPSE('',#32783,0.0512749647677413,0.0469971417989442);
#1762=ELLIPSE('',#32786,0.0512707788579549,0.0469842741354182);
#1763=ELLIPSE('',#32787,0.0512749647704146,0.0469971418003949);
#1764=ELLIPSE('',#32790,0.0512707788581164,0.0469842741355277);
#1765=ELLIPSE('',#32791,0.0512749647678976,0.0469971417990442);
#1766=ELLIPSE('',#32794,0.0512707788570414,0.0469842741348829);
#1767=ELLIPSE('',#32795,0.0512749647696248,0.0469971417999634);
#1768=ELLIPSE('',#32798,0.0512707789395351,0.0469842741799766);
#1769=ELLIPSE('',#32799,0.0512749647687745,0.0469971417995203);
#1770=ELLIPSE('',#32802,0.0512707788562593,0.0469842741344864);
#1771=ELLIPSE('',#32803,0.0512749647684955,0.046997141799316);
#1772=ELLIPSE('',#32806,0.0512707788603725,0.0469842741367327);
#1773=ELLIPSE('',#32807,0.0512749647690289,0.0469971417996681);
#1774=ELLIPSE('',#32810,0.0512707788577797,0.0469842741353011);
#1775=ELLIPSE('',#32811,0.0512749647683414,0.0469971417992803);
#1776=ELLIPSE('',#32814,0.051270778856875,0.0469842741348193);
#1777=ELLIPSE('',#32815,0.0512749647684586,0.0469971417993373);
#1778=ELLIPSE('',#32818,0.051270778920832,0.0469842741697548);
#1779=ELLIPSE('',#32819,0.0512749647689089,0.0469971417995588);
#1780=ELLIPSE('',#32822,0.0512707788568015,0.0469842741347871);
#1781=ELLIPSE('',#32823,0.0512749647679381,0.0469971417990666);
#1782=ELLIPSE('',#32826,0.0512707788566487,0.046984274134668);
#1783=ELLIPSE('',#32827,0.0512749647684683,0.0469971417993365);
#1784=ELLIPSE('',#32830,0.051270778856618,0.0469842741346731);
#1785=ELLIPSE('',#32831,0.0512749647693393,0.0469971417998184);
#1786=ELLIPSE('',#32834,0.0512707788568358,0.0469842741348282);
#1787=ELLIPSE('',#32835,0.0512749647674564,0.0469971417987839);
#1788=ELLIPSE('',#32838,0.0512707788557633,0.0469842741342339);
#1789=ELLIPSE('',#32839,0.0512749647690638,0.0469971417996539);
#1790=ELLIPSE('',#32842,0.0512707788566786,0.0469842741346996);
#1791=ELLIPSE('',#32843,0.0512749647672967,0.0469971417987006);
#1792=ELLIPSE('',#32846,0.0512707788621377,0.0469842741376985);
#1793=ELLIPSE('',#32847,0.0512749647686591,0.046997141799446);
#1794=ELLIPSE('',#32850,0.0512707788564809,0.0469842741346051);
#1795=ELLIPSE('',#32851,0.0512749647682497,0.0469971417992212);
#1796=ELLIPSE('',#32854,0.0512707788573564,0.0469842741350646);
#1797=ELLIPSE('',#32855,0.0512749647687658,0.0469971417994997);
#1798=ELLIPSE('',#32858,0.051270778874813,0.0469842741446368);
#1799=ELLIPSE('',#32859,0.0512749647675386,0.046997141798832);
#1800=ELLIPSE('',#32862,0.0512707788565269,0.0469842741346491);
#1801=ELLIPSE('',#32863,0.0512749647691996,0.0469971417997275);
#1802=ELLIPSE('',#32866,0.0512707788580797,0.0469842741354721);
#1803=ELLIPSE('',#32867,0.0512749647681002,0.0469971417991393);
#1804=ELLIPSE('',#32870,0.0512707788579047,0.0469842741354009);
#1805=ELLIPSE('',#32871,0.0512749647678865,0.0469971417990283);
#1806=ELLIPSE('',#32874,0.0512707788574115,0.046984274135125);
#1807=ELLIPSE('',#32875,0.0512749647671369,0.0469971417986091);
#1808=ELLIPSE('',#32878,0.0512749647690318,0.0469971417996552);
#1809=ELLIPSE('',#32880,0.0512707788566348,0.0469842741346708);
#1810=ELLIPSE('',#32882,0.0512749647679538,0.0469971417990534);
#1811=ELLIPSE('',#32884,0.0512707788562212,0.0469842741344524);
#1812=ELLIPSE('',#32886,0.051274964768521,0.0469971417993772);
#1813=ELLIPSE('',#32888,0.051270778856042,0.0469842741343731);
#1814=ELLIPSE('',#32890,0.0512749647675581,0.0469971417988677);
#1815=ELLIPSE('',#32892,0.0512707788559885,0.0469842741343514);
#1816=ELLIPSE('',#32894,0.0512749647693218,0.0469971417997968);
#1817=ELLIPSE('',#32896,0.0512707788571387,0.0469842741349643);
#1818=ELLIPSE('',#32898,0.0512749647679417,0.0469971417990759);
#1819=ELLIPSE('',#32900,0.0512707788922353,0.0469842741541131);
#1820=ELLIPSE('',#32902,0.051274964769059,0.046997141799664);
#1821=ELLIPSE('',#32904,0.0512707788612464,0.0469842741372165);
#1822=ELLIPSE('',#32906,0.0512749647686166,0.0469971417994078);
#1823=ELLIPSE('',#32908,0.0512707788558472,0.0469842741342397);
#1824=ELLIPSE('',#32910,0.0512749647686363,0.0469971417994427);
#1825=ELLIPSE('',#32912,0.0512707788567449,0.0469842741347651);
#1826=ELLIPSE('',#32914,0.0512749647684367,0.0469971417993216);
#1827=ELLIPSE('',#32916,0.0512707788561666,0.0469842741344253);
#1828=ELLIPSE('',#32918,0.0512749647683517,0.046997141799283);
#1829=ELLIPSE('',#32920,0.0512707788648064,0.0469842741391505);
#1830=ELLIPSE('',#32922,0.0512749647688174,0.0469971417995523);
#1831=ELLIPSE('',#32924,0.051270778857567,0.0469842741352074);
#1832=ELLIPSE('',#32926,0.0512749647694904,0.0469971417998601);
#1833=ELLIPSE('',#32928,0.0512707788575527,0.0469842741351904);
#1834=ELLIPSE('',#32930,0.0512749647677225,0.0469971417989513);
#1835=ELLIPSE('',#32932,0.0512707788585909,0.0469842741357571);
#1836=ELLIPSE('',#32934,0.051270778940575,0.0469842741805314);
#1837=ELLIPSE('',#32935,0.0512749647683344,0.0469971417992899);
#1838=ELLIPSE('',#33096,0.0512707788678624,0.04698427414088);
#1839=ELLIPSE('',#33097,0.0512749647679163,0.0469971417991227);
#1840=ELLIPSE('',#33099,0.0512749647654335,0.0469971417977818);
#1841=ELLIPSE('',#33100,0.0512707788568347,0.0469842741348514);
#1842=ELLIPSE('',#33102,0.0512749647672852,0.0469971417988039);
#1843=ELLIPSE('',#33103,0.0512707788564686,0.0469842741346539);
#1844=ELLIPSE('',#33105,0.0512749647659393,0.0469971417980464);
#1845=ELLIPSE('',#33106,0.0512707788556944,0.0469842741342504);
#1846=ELLIPSE('',#33108,0.0512749647686629,0.0469971417995544);
#1847=ELLIPSE('',#33109,0.0512707788564297,0.0469842741346479);
#1848=ELLIPSE('',#33111,0.0512749647671486,0.0469971417987065);
#1849=ELLIPSE('',#33112,0.0512707788597197,0.0469842741364453);
#1850=ELLIPSE('',#33114,0.0512749647666077,0.0469971417984174);
#1851=ELLIPSE('',#33115,0.0512707788555701,0.0469842741341628);
#1852=ELLIPSE('',#33117,0.0512749647679515,0.0469971417991682);
#1853=ELLIPSE('',#33118,0.0512707788587403,0.0469842741359266);
#1854=ELLIPSE('',#33120,0.0512749647675462,0.0469971417988912);
#1855=ELLIPSE('',#33121,0.0512707788561996,0.0469842741345216);
#1856=ELLIPSE('',#33123,0.0512749647665171,0.0469971417983294);
#1857=ELLIPSE('',#33124,0.0512707788563593,0.0469842741346364);
#1858=ELLIPSE('',#33126,0.0512749647671419,0.0469971417986936);
#1859=ELLIPSE('',#33127,0.0512707788554834,0.0469842741341348);
#1860=ELLIPSE('',#33129,0.0512749647679126,0.0469971417991247);
#1861=ELLIPSE('',#33130,0.0512707788566136,0.0469842741347507);
#1862=ELLIPSE('',#33132,0.051274964765861,0.0469971417980122);
#1863=ELLIPSE('',#33133,0.0512707788569887,0.0469842741349521);
#1864=ELLIPSE('',#33135,0.0512749647673257,0.046997141798794);
#1865=ELLIPSE('',#33136,0.0512707788578384,0.0469842741354011);
#1866=ELLIPSE('',#33138,0.0512749647685051,0.046997141799409);
#1867=ELLIPSE('',#33139,0.0512707788566497,0.0469842741347448);
#1868=ELLIPSE('',#33141,0.0512749647664023,0.0469971417983194);
#1869=ELLIPSE('',#33142,0.0512707788557973,0.0469842741343033);
#1870=ELLIPSE('',#33144,0.0512749647657081,0.0469971417979273);
#1871=ELLIPSE('',#33145,0.0512707788560454,0.0469842741344356);
#1872=ELLIPSE('',#33147,0.0512749647672847,0.0469971417988018);
#1873=ELLIPSE('',#33148,0.0512707788908472,0.0469842741534398);
#1874=ELLIPSE('',#33150,0.0512749647656979,0.0469971417979225);
#1875=ELLIPSE('',#33151,0.0512707788619598,0.0469842741376821);
#1876=ELLIPSE('',#33153,0.0512749647673844,0.0469971417987892);
#1877=ELLIPSE('',#33154,0.0512707788554361,0.0469842741341347);
#1878=ELLIPSE('',#33156,0.0512749647665351,0.0469971417983737);
#1879=ELLIPSE('',#33157,0.051270778857401,0.0469842741351899);
#1880=ELLIPSE('',#33159,0.0512749647648224,0.0469971417974593);
#1881=ELLIPSE('',#33160,0.051270778857135,0.0469842741350546);
#1882=ELLIPSE('',#33162,0.051274964767923,0.046997141799147);
#1883=ELLIPSE('',#33163,0.0512707788632245,0.0469842741383353);
#1884=ELLIPSE('',#33165,0.0512749647670837,0.0469971417986601);
#1885=ELLIPSE('',#33166,0.0512707788575274,0.0469842741352789);
#1886=ELLIPSE('',#33168,0.0512749647661063,0.046997141798163);
#1887=ELLIPSE('',#33169,0.0512707788614728,0.0469842741374068);
#1888=ELLIPSE('',#33171,0.0512749647661745,0.0469971417981727);
#1889=ELLIPSE('',#33172,0.0512707788561374,0.0469842741344828);
#1890=ELLIPSE('',#33174,0.0512749647684627,0.0469971417993818);
#1891=ELLIPSE('',#33175,0.0512707788547222,0.0469842741337518);
#1892=ELLIPSE('',#33177,0.0512749647675423,0.0469971417989238);
#1893=ELLIPSE('',#33178,0.0512707788556497,0.0469842741342235);
#1894=ELLIPSE('',#33180,0.0512749647674664,0.0469971417988657);
#1895=ELLIPSE('',#33181,0.0512707788563694,0.0469842741346094);
#1896=ELLIPSE('',#33183,0.0512749647689012,0.0469971417996608);
#1897=ELLIPSE('',#33184,0.0512707788554915,0.0469842741341037);
#1898=ELLIPSE('',#33186,0.0512749647674053,0.0469971417988339);
#1899=ELLIPSE('',#33187,0.0512707788551391,0.0469842741339346);
#1900=ELLIPSE('',#33189,0.051274964767584,0.046997141798928);
#1901=ELLIPSE('',#33190,0.0512707788578603,0.0469842741354062);
#1902=ELLIPSE('',#33192,0.0512749647667973,0.046997141798492);
#1903=ELLIPSE('',#33193,0.0512707788554342,0.0469842741340614);
#1904=ELLIPSE('',#33195,0.0512749647663277,0.0469971417982546);
#1905=ELLIPSE('',#33196,0.051270778856014,0.0469842741344105);
#1906=ELLIPSE('',#33198,0.0512749647644558,0.0469971417972658);
#1907=ELLIPSE('',#33199,0.051270778856549,0.046984274134693);
#1908=ELLIPSE('',#33201,0.0512749647655728,0.0469971417978321);
#1909=ELLIPSE('',#33202,0.0512707788565064,0.0469842741346634);
#1910=ELLIPSE('',#33204,0.0512749647677657,0.0469971417990299);
#1911=ELLIPSE('',#33205,0.0512707788566898,0.0469842741347819);
#1912=ELLIPSE('',#33207,0.0512749647676116,0.0469971417989766);
#1913=ELLIPSE('',#33208,0.0512707788912617,0.0469842741536714);
#1914=ELLIPSE('',#33210,0.0512749647664018,0.0469971417982991);
#1915=ELLIPSE('',#33211,0.0512707788616718,0.0469842741375278);
#1916=ELLIPSE('',#33213,0.0512749647667201,0.046997141798501);
#1917=ELLIPSE('',#33214,0.0512707788559321,0.046984274134359);
#1918=ELLIPSE('',#33216,0.0512749647688712,0.0469971417996063);
#1919=ELLIPSE('',#33217,0.0512707788570311,0.0469842741349509);
#1920=ELLIPSE('',#33219,0.0512749647675863,0.0469971417989162);
#1921=ELLIPSE('',#33220,0.0512707788563448,0.0469842741345939);
#1922=ELLIPSE('',#33222,0.0512749647671262,0.0469971417987068);
#1923=ELLIPSE('',#33223,0.0512707788650867,0.0469842741393638);
#1924=ELLIPSE('',#33225,0.0512749647686962,0.0469971417995509);
#1925=ELLIPSE('',#33226,0.0512707788567886,0.0469842741348241);
#1926=ELLIPSE('',#33228,0.0512749647672976,0.0469971417987731);
#1927=ELLIPSE('',#33229,0.0512707788570162,0.0469842741349496);
#1928=ELLIPSE('',#33231,0.0512749647667697,0.0469971417984931);
#1929=ELLIPSE('',#33232,0.0512707788584097,0.0469842741357168);
#1930=ELLIPSE('',#33234,0.0512749647672832,0.0469971417987584);
#1931=ELLIPSE('',#33235,0.0512707788570115,0.0469842741349691);
#1932=ELLIPSE('',#33237,0.0512749647672073,0.0469971417987249);
#1933=ELLIPSE('',#33238,0.0512707789405328,0.0469842741805533);
#1934=ELLIPSE('',#33240,0.0512749647662809,0.0469971417982346);
#1935=ELLIPSE('',#33241,0.0512707788564733,0.0469842741346687);
#1936=ELLIPSE('',#33243,0.0512749647659994,0.0469971417980507);
#1937=ELLIPSE('',#33244,0.0512707788571204,0.0469842741349872);
#1938=ELLIPSE('',#33246,0.0512749647671319,0.0469971417987083);
#1939=ELLIPSE('',#33247,0.0512707788566097,0.0469842741347329);
#1940=ELLIPSE('',#33249,0.0512749647668497,0.0469971417985515);
#1941=ELLIPSE('',#33250,0.0512707788560048,0.0469842741344256);
#1942=ELLIPSE('',#33252,0.051274964765999,0.0469971417980718);
#1943=ELLIPSE('',#33253,0.0512707788746663,0.0469842741446355);
#1944=ELLIPSE('',#33255,0.0512749647672519,0.0469971417987563);
#1945=ELLIPSE('',#33256,0.051270778855846,0.0469842741343271);
#1946=ELLIPSE('',#33258,0.0512749647662359,0.0469971417982146);
#1947=ELLIPSE('',#33259,0.0512707788574978,0.0469842741352291);
#1948=ELLIPSE('',#33261,0.0512749647668179,0.0469971417985263);
#1949=ELLIPSE('',#33262,0.0512707788607044,0.0469842741369976);
#1950=ELLIPSE('',#33264,0.0512749647674441,0.0469971417988379);
#1951=ELLIPSE('',#33265,0.0512707788568965,0.0469842741348871);
#1952=ELLIPSE('',#33267,0.0512749647672645,0.0469971417987703);
#1953=ELLIPSE('',#33268,0.0512707788559945,0.0469842741344026);
#1954=ELLIPSE('',#33270,0.0512749647680151,0.0469971417991764);
#1955=ELLIPSE('',#33271,0.0512707788560419,0.04698427413443);
#1956=ELLIPSE('',#33273,0.0512749647667931,0.0469971417984966);
#1957=ELLIPSE('',#33274,0.0512707788563537,0.0469842741346079);
#1958=ELLIPSE('',#33276,0.0512749647674696,0.0469971417988977);
#1959=ELLIPSE('',#33277,0.0512707788571896,0.0469842741350665);
#1960=ELLIPSE('',#33279,0.0512749647673948,0.046997141798837);
#1961=ELLIPSE('',#33280,0.0512707788555549,0.0469842741341569);
#1962=ELLIPSE('',#33282,0.0512749647668783,0.0469971417985539);
#1963=ELLIPSE('',#33283,0.0512707789210852,0.0469842741699459);
#1964=ELLIPSE('',#33285,0.0512749647677305,0.0469971417990099);
#1965=ELLIPSE('',#33286,0.0512707788552415,0.0469842741340032);
#1966=ELLIPSE('',#33288,0.0512707788564181,0.0469842741346374);
#1967=ELLIPSE('',#33289,0.0512749647669761,0.0469971417985938);
#1968=ELLIPSE('',#33291,0.051270778856969,0.0469842741349151);
#1969=ELLIPSE('',#33292,0.0512749647670935,0.046997141798684);
#1970=ELLIPSE('',#33294,0.0512707788562384,0.0469842741345515);
#1971=ELLIPSE('',#33295,0.0512749647675247,0.0469971417988957);
#1972=ELLIPSE('',#33297,0.0512707788573216,0.0469842741351317);
#1973=ELLIPSE('',#33298,0.0512749647668487,0.046997141798569);
#1974=ELLIPSE('',#33300,0.0512707788622439,0.0469842741378278);
#1975=ELLIPSE('',#33301,0.0512749647677751,0.0469971417990674);
#1976=ELLIPSE('',#33303,0.0512707788576837,0.046984274135325);
#1977=ELLIPSE('',#33304,0.0512749647668911,0.0469971417985504);
#1978=ELLIPSE('',#33306,0.0512707788569353,0.0469842741349273);
#1979=ELLIPSE('',#33307,0.0512749647675315,0.0469971417989158);
#1980=ELLIPSE('',#33309,0.0512707788759282,0.0469842741452617);
#1981=ELLIPSE('',#33310,0.0512749647661136,0.0469971417981488);
#1982=ELLIPSE('',#33312,0.0512707788557471,0.0469842741342912);
#1983=ELLIPSE('',#33313,0.051274964767063,0.0469971417986624);
#1984=ELLIPSE('',#33315,0.0512707788562218,0.0469842741345251);
#1985=ELLIPSE('',#33316,0.0512749647674796,0.0469971417988927);
#1986=ELLIPSE('',#33318,0.0512707788562634,0.0469842741345331);
#1987=ELLIPSE('',#33319,0.0512749647672643,0.0469971417987429);
#1988=ELLIPSE('',#33321,0.0512707788550995,0.0469842741339394);
#1989=ELLIPSE('',#33322,0.0512749647667936,0.0469971417984887);
#1990=ELLIPSE('',#33324,0.0512707789393949,0.0469842741799506);
#1991=ELLIPSE('',#33325,0.0512749647666032,0.0469971417983921);
#1992=ELLIPSE('',#33327,0.0512707788579345,0.0469842741354427);
#1993=ELLIPSE('',#33328,0.0512749647659267,0.0469971417980537);
#1994=ELLIPSE('',#33330,0.0512749647694732,0.0469971417999488);
#1995=ELLIPSE('',#33331,0.0512707788565522,0.0469842741347113);
#1996=ELLIPSE('',#33335,0.0512707788554107,0.0469842741340208);
#1997=ELLIPSE('',#33336,0.0512749647674929,0.0469971417988238);
#1998=ELLIPSE('',#33341,0.0512749647664458,0.0469971417983288);
#1999=ELLIPSE('',#33342,0.0512707788586759,0.0469842741358754);
#2000=ELLIPSE('',#33648,0.0195162536838815,0.0137573643715162);
#2001=ELLIPSE('',#33649,0.0195162536830269,0.0137573643713391);
#2002=ELLIPSE('',#33651,0.0195162536835621,0.0137573643714695);
#2003=ELLIPSE('',#33652,0.019516253683001,0.0137573643713521);
#2004=ELLIPSE('',#33654,0.0195162536836977,0.0137573643714721);
#2005=ELLIPSE('',#33655,0.0195162536830636,0.0137573643713535);
#2006=ELLIPSE('',#33657,0.0195162536837443,0.0137573643714943);
#2007=ELLIPSE('',#33658,0.0195162536831223,0.0137573643713688);
#2008=ELLIPSE('',#33660,0.019516253683803,0.013757364371504);
#2009=ELLIPSE('',#33661,0.0195162536829111,0.0137573643713217);
#2010=ELLIPSE('',#33663,0.0195162536837688,0.0137573643714986);
#2011=ELLIPSE('',#33664,0.0195162536830749,0.0137573643713556);
#2012=ELLIPSE('',#33666,0.0195162536837257,0.0137573643714922);
#2013=ELLIPSE('',#33667,0.0195162536830703,0.0137573643713494);
#2014=ELLIPSE('',#33669,0.0195162536838104,0.013757364371505);
#2015=ELLIPSE('',#33670,0.0195162536830614,0.0137573643713493);
#2016=ELLIPSE('',#33672,0.0195162536837473,0.0137573643714877);
#2017=ELLIPSE('',#33673,0.0195162536830537,0.0137573643713548);
#2018=ELLIPSE('',#33675,0.0195162536838422,0.0137573643715182);
#2019=ELLIPSE('',#33676,0.0195162536831755,0.0137573643713807);
#2020=ELLIPSE('',#33678,0.0195162536837639,0.0137573643714952);
#2021=ELLIPSE('',#33679,0.0195162536830792,0.0137573643713542);
#2022=ELLIPSE('',#33681,0.0195162536835653,0.0137573643714501);
#2023=ELLIPSE('',#33682,0.0195162536831025,0.0137573643713567);
#2024=ELLIPSE('',#33684,0.0195162536835776,0.0137573643714587);
#2025=ELLIPSE('',#33685,0.0195162536828947,0.01375736437132);
#2026=ELLIPSE('',#33687,0.0195162536837483,0.0137573643714995);
#2027=ELLIPSE('',#33688,0.0195162536831204,0.0137573643713664);
#2028=ELLIPSE('',#33690,0.0195162536835793,0.0137573643714601);
#2029=ELLIPSE('',#33691,0.0195162536830448,0.0137573643713492);
#2030=ELLIPSE('',#33700,0.0195034997306777,0.013754915723726);
#2031=ELLIPSE('',#33702,0.0195030685020683,0.0137548403891227);
#2032=ELLIPSE('',#33704,0.0195027524929284,0.0137547851848027);
#2033=ELLIPSE('',#33706,0.0195025132809572,0.0137547433941177);
#2034=ELLIPSE('',#33708,0.0195023280193677,0.0137547110253133);
#2035=ELLIPSE('',#33710,0.0195021823053853,0.0137546855626127);
#2036=ELLIPSE('',#33712,0.0195020666474465,0.0137546653482711);
#2037=ELLIPSE('',#33714,0.0195019745733047,0.0137546492518586);
#2038=ELLIPSE('',#33716,0.0195019015620118,0.0137546364836367);
#2039=ELLIPSE('',#33718,0.0195018443987318,0.0137546264818649);
#2040=ELLIPSE('',#33720,0.0195018007910573,0.0137546188457545);
#2041=ELLIPSE('',#33722,0.0195017691158091,0.0137546132912077);
#2042=ELLIPSE('',#33724,0.0195017482624769,0.0137546096234092);
#2043=ELLIPSE('',#33726,0.0195017375337946,0.0137546077193674);
#2044=ELLIPSE('',#33728,0.0195017365885567,0.0137546075177427);
#2045=ELLIPSE('',#33730,0.0195017454175912,0.0137546090143427);
#2046=ELLIPSE('',#33732,0.0195017643506138,0.0137546122627749);
#2047=ELLIPSE('',#33734,0.0195017941005044,0.0137546173811011);
#2048=ELLIPSE('',#33736,0.0195018358641676,0.0137546245672221);
#2049=ELLIPSE('',#33738,0.0195018727625836,0.013754631431718);
#2050=ELLIPSE('',#33740,0.0195034997306828,0.0137549157237274);
#2051=ELLIPSE('',#33742,0.0195030685021256,0.0137548403891337);
#2052=ELLIPSE('',#33744,0.0195027524929019,0.0137547851847966);
#2053=ELLIPSE('',#33746,0.0195025132809425,0.0137547433941156);
#2054=ELLIPSE('',#33748,0.0195023280193708,0.0137547110253143);
#2055=ELLIPSE('',#33750,0.0195021823053841,0.0137546855626124);
#2056=ELLIPSE('',#33752,0.0195020666474398,0.0137546653482691);
#2057=ELLIPSE('',#33754,0.0195019745733335,0.0137546492518631);
#2058=ELLIPSE('',#33756,0.0195019015619959,0.0137546364836322);
#2059=ELLIPSE('',#33758,0.0195018443987879,0.0137546264818748);
#2060=ELLIPSE('',#33760,0.0195018007910457,0.0137546188457536);
#2061=ELLIPSE('',#33762,0.0195017691158159,0.0137546132912084);
#2062=ELLIPSE('',#33764,0.0195017482624727,0.013754609623408);
#2063=ELLIPSE('',#33766,0.0195017375337736,0.0137546077193644);
#2064=ELLIPSE('',#33768,0.0195017365885347,0.0137546075177382);
#2065=ELLIPSE('',#33770,0.019501745417596,0.0137546090143437);
#2066=ELLIPSE('',#33772,0.0195017643505816,0.0137546122627688);
#2067=ELLIPSE('',#33774,0.0195017941005605,0.0137546173811125);
#2068=ELLIPSE('',#33776,0.019501835864167,0.0137546245672222);
#2069=ELLIPSE('',#33778,0.0195162536830855,0.0137573643713537);
#2070=ELLIPSE('',#33780,0.0195034997307414,0.013754915723739);
#2071=ELLIPSE('',#33782,0.0195030685021161,0.0137548403891323);
#2072=ELLIPSE('',#33784,0.0195027524929008,0.0137547851847961);
#2073=ELLIPSE('',#33786,0.0195025132809546,0.0137547433941189);
#2074=ELLIPSE('',#33788,0.0195023280193482,0.0137547110253084);
#2075=ELLIPSE('',#33805,0.0195034997306463,0.0137549157237206);
#2076=ELLIPSE('',#33807,0.0195030685021557,0.0137548403891397);
#2077=ELLIPSE('',#33809,0.0195027524928776,0.0137547851847918);
#2078=ELLIPSE('',#33811,0.0195025132809776,0.0137547433941213);
#2079=ELLIPSE('',#33813,0.019502328019347,0.0137547110253081);
#2080=ELLIPSE('',#33815,0.0195021823053738,0.0137546855626116);
#2081=ELLIPSE('',#33817,0.0195020666474525,0.0137546653482711);
#2082=ELLIPSE('',#33819,0.0195019745733739,0.013754649251872);
#2083=ELLIPSE('',#33821,0.0195019015619764,0.0137546364836293);
#2084=ELLIPSE('',#33823,0.0195018443987816,0.0137546264818739);
#2085=ELLIPSE('',#33825,0.0195018007910337,0.0137546188457504);
#2086=ELLIPSE('',#33827,0.0195017691158341,0.0137546132912121);
#2087=ELLIPSE('',#33829,0.0195017482624509,0.0137546096234037);
#2088=ELLIPSE('',#33831,0.0195017375337853,0.0137546077193653);
#2089=ELLIPSE('',#33833,0.0195017365886309,0.0137546075177561);
#2090=ELLIPSE('',#33835,0.0195017454176055,0.0137546090143461);
#2091=ELLIPSE('',#33837,0.0195017643505986,0.0137546122627731);
#2092=ELLIPSE('',#33839,0.0195017941005311,0.0137546173811059);
#2093=ELLIPSE('',#33841,0.0195018358641241,0.0137546245672129);
#2094=ELLIPSE('',#33845,0.0195034997306858,0.0137549157237271);
#2095=ELLIPSE('',#33847,0.0195030685021635,0.0137548403891432);
#2096=ELLIPSE('',#33849,0.019502752492881,0.0137547851847926);
#2097=ELLIPSE('',#33851,0.0195025132809236,0.0137547433941134);
#2098=ELLIPSE('',#33853,0.0195023280193679,0.0137547110253125);
#2099=ELLIPSE('',#33855,0.0195021823054267,0.0137546855626225);
#2100=ELLIPSE('',#33857,0.0195020666474927,0.0137546653482813);
#2101=ELLIPSE('',#33859,0.019501974573308,0.0137546492518591);
#2102=ELLIPSE('',#33861,0.0195019015619601,0.0137546364836262);
#2103=ELLIPSE('',#33863,0.0195018443987825,0.0137546264818736);
#2104=ELLIPSE('',#33865,0.0195018007910841,0.0137546188457617);
#2105=ELLIPSE('',#33867,0.0195017691158046,0.0137546132912069);
#2106=ELLIPSE('',#33869,0.0195017482624746,0.0137546096234107);
#2107=ELLIPSE('',#33871,0.0195017375337627,0.0137546077193623);
#2108=ELLIPSE('',#33873,0.0195017365885639,0.0137546075177438);
#2109=ELLIPSE('',#33875,0.0195017454175912,0.0137546090143448);
#2110=ELLIPSE('',#33877,0.0195017643506125,0.0137546122627745);
#2111=ELLIPSE('',#33879,0.0195017941005712,0.0137546173811145);
#2112=ELLIPSE('',#33881,0.0195018358641553,0.013754624567221);
#2113=ELLIPSE('',#33883,0.0195018727626295,0.0137546314317287);
#2114=ELLIPSE('',#33885,0.0195034997307231,0.0137549157237351);
#2115=ELLIPSE('',#33887,0.0195030685021692,0.0137548403891432);
#2116=ELLIPSE('',#33889,0.0195027524928953,0.013754785184795);
#2117=ELLIPSE('',#33891,0.0195025132809505,0.0137547433941165);
#2118=ELLIPSE('',#33893,0.0195023280194302,0.0137547110253254);
#2119=ELLIPSE('',#33895,0.019502182305463,0.0137546855626286);
#2120=ELLIPSE('',#33897,0.0195020666474861,0.0137546653482797);
#2121=ELLIPSE('',#33899,0.0195019745732981,0.0137546492518571);
#2122=ELLIPSE('',#33901,0.019501901562003,0.0137546364836345);
#2123=ELLIPSE('',#33903,0.0195018443988218,0.0137546264818824);
#2124=ELLIPSE('',#33905,0.0195018007911448,0.0137546188457728);
#2125=ELLIPSE('',#33907,0.0195017691157916,0.0137546132912057);
#2126=ELLIPSE('',#33909,0.0195017482624564,0.013754609623407);
#2127=ELLIPSE('',#33911,0.0195017375338029,0.0137546077193704);
#2128=ELLIPSE('',#33913,0.0195017365886144,0.0137546075177533);
#2129=ELLIPSE('',#33915,0.0195017454176306,0.0137546090143512);
#2130=ELLIPSE('',#33917,0.0195017643505891,0.0137546122627708);
#2131=ELLIPSE('',#33919,0.0195017941005193,0.013754617381105);
#2132=ELLIPSE('',#33921,0.0195018358642213,0.0137546245672329);
#2133=ELLIPSE('',#33923,0.0195162536837232,0.0137573643714884);
#2134=ELLIPSE('',#33925,0.0195034997306679,0.0137549157237246);
#2135=ELLIPSE('',#33927,0.0195030685021047,0.0137548403891311);
#2136=ELLIPSE('',#33929,0.0195027524929266,0.0137547851848028);
#2137=ELLIPSE('',#33931,0.0195025132809874,0.0137547433941253);
#2138=ELLIPSE('',#33933,0.0195023280194086,0.013754711025321);
#2139=ELLIPSE('',#33935,0.0195021823054203,0.0137546855626212);
#2140=ELLIPSE('',#33937,0.0195020666475111,0.0137546653482846);
#2141=ELLIPSE('',#33939,0.0195019745733549,0.0137546492518684);
#2142=ELLIPSE('',#33941,0.0195019015619592,0.0137546364836273);
#2143=ELLIPSE('',#33943,0.0195018443988324,0.0137546264818843);
#2144=ELLIPSE('',#33945,0.0195018007910703,0.0137546188457585);
#2145=ELLIPSE('',#33947,0.0195017691158645,0.0137546132912193);
#2146=ELLIPSE('',#33949,0.0195017482624579,0.0137546096234066);
#2147=ELLIPSE('',#33951,0.0195017375338027,0.0137546077193706);
#2148=ELLIPSE('',#33953,0.0195017365886083,0.0137546075177516);
#2149=ELLIPSE('',#33955,0.019501745417535,0.0137546090143326);
#2150=ELLIPSE('',#33957,0.0195017643506093,0.0137546122627733);
#2151=ELLIPSE('',#33959,0.0195017941005168,0.013754617381103);
#2152=ELLIPSE('',#33961,0.0195018358640787,0.0137546245672056);
#2153=ELLIPSE('',#33978,0.0195017365886013,0.0137546075177502);
#2154=ELLIPSE('',#33980,0.0195017454175941,0.0137546090143434);
#2155=ELLIPSE('',#33982,0.0195017643505789,0.0137546122627681);
#2156=ELLIPSE('',#33984,0.0195017941005255,0.0137546173811058);
#2157=ELLIPSE('',#33986,0.0195018358641318,0.0137546245672154);
#2158=ELLIPSE('',#34002,0.051274964768551,0.0469971417993774);
#2159=ELLIPSE('',#34004,0.0512707788579671,0.0469842741354326);
#2160=ELLIPSE('',#34006,0.0512707788562332,0.0469842741344865);
#2161=ELLIPSE('',#34007,0.0512749647685533,0.0469971417993787);
#2162=ELLIPSE('',#34010,0.0512707788571307,0.0469842741349983);
#2163=ELLIPSE('',#34011,0.0512749647672664,0.0469971417987026);
#2164=ELLIPSE('',#34014,0.0512707788571389,0.0469842741349856);
#2165=ELLIPSE('',#34015,0.0512749647681367,0.0469971417991575);
#2166=ELLIPSE('',#34018,0.0512707788569124,0.0469842741348335);
#2167=ELLIPSE('',#34019,0.051274964768467,0.0469971417993732);
#2168=ELLIPSE('',#34022,0.051270778857559,0.0469842741351648);
#2169=ELLIPSE('',#34023,0.0512749647697504,0.0469971418000396);
#2170=ELLIPSE('',#34026,0.051270778857562,0.0469842741352078);
#2171=ELLIPSE('',#34027,0.0512749647676798,0.0469971417989218);
#2172=ELLIPSE('',#34030,0.0512707788610954,0.0469842741371193);
#2173=ELLIPSE('',#34031,0.0512749647674827,0.0469971417988075);
#2174=ELLIPSE('',#34034,0.0512707788555596,0.0469842741341208);
#2175=ELLIPSE('',#34035,0.0512749647677061,0.0469971417989105);
#2176=ELLIPSE('',#34038,0.0512707788650729,0.0469842741392919);
#2177=ELLIPSE('',#34039,0.0512749647702881,0.0469971418003199);
#2178=ELLIPSE('',#34042,0.0512707788560203,0.0469842741343728);
#2179=ELLIPSE('',#34043,0.0512749647689969,0.0469971417996401);
#2180=ELLIPSE('',#34046,0.0512707788567884,0.046984274134799);
#2181=ELLIPSE('',#34047,0.0512749647681247,0.0469971417991492);
#2182=ELLIPSE('',#34050,0.0512707788573083,0.0469842741350659);
#2183=ELLIPSE('',#34051,0.0512749647690658,0.0469971417996437);
#2184=ELLIPSE('',#34054,0.0512707788615306,0.046984274137359);
#2185=ELLIPSE('',#34055,0.051274964767619,0.0469971417988856);
#2186=ELLIPSE('',#34058,0.0512707788928482,0.0469842741544496);
#2187=ELLIPSE('',#34059,0.0512749647695684,0.0469971417999069);
#2188=ELLIPSE('',#34062,0.051270778857717,0.0469842741353091);
#2189=ELLIPSE('',#34063,0.0512749647683041,0.0469971417992544);
#2190=ELLIPSE('',#34066,0.051270778855901,0.046984274134278);
#2191=ELLIPSE('',#34067,0.0512749647692079,0.0469971417997307);
#2192=ELLIPSE('',#34070,0.0512707788585063,0.0469842741357279);
#2193=ELLIPSE('',#34071,0.0512749647681597,0.0469971417991513);
#2194=ELLIPSE('',#34074,0.0512707788568602,0.0469842741348085);
#2195=ELLIPSE('',#34075,0.0512749647674443,0.0469971417987893);
#2196=ELLIPSE('',#34078,0.0512707788568387,0.0469842741347804);
#2197=ELLIPSE('',#34079,0.0512749647678151,0.0469971417990189);
#2198=ELLIPSE('',#34082,0.0512707788582789,0.0469842741356006);
#2199=ELLIPSE('',#34083,0.05127496476906,0.0469971417996405);
#2200=ELLIPSE('',#34086,0.051270778856965,0.0469842741348763);
#2201=ELLIPSE('',#34087,0.0512749647686908,0.046997141799481);
#2202=ELLIPSE('',#34090,0.0512707788563555,0.0469842741344815);
#2203=ELLIPSE('',#34091,0.0512749647673275,0.0469971417987118);
#2204=ELLIPSE('',#34094,0.0512707788571547,0.0469842741350112);
#2205=ELLIPSE('',#34095,0.0512749647685426,0.046997141799397);
#2206=ELLIPSE('',#34098,0.0512707788556612,0.0469842741341707);
#2207=ELLIPSE('',#34099,0.0512749647699517,0.0469971418001559);
#2208=ELLIPSE('',#34102,0.0512707788576472,0.0469842741352346);
#2209=ELLIPSE('',#34103,0.0512749647672529,0.0469971417986806);
#2210=ELLIPSE('',#34106,0.0512707788618793,0.0469842741375491);
#2211=ELLIPSE('',#34107,0.0512749647679756,0.0469971417990623);
#2212=ELLIPSE('',#34110,0.0512707788555002,0.0469842741340957);
#2213=ELLIPSE('',#34111,0.0512749647688844,0.046997141799544);
#2214=ELLIPSE('',#34114,0.0512707788566344,0.0469842741346946);
#2215=ELLIPSE('',#34115,0.051274964769648,0.046997141799953);
#2216=ELLIPSE('',#34118,0.0512707788584597,0.0469842741356599);
#2217=ELLIPSE('',#34119,0.0512749647679757,0.0469971417990702);
#2218=ELLIPSE('',#34122,0.0512707788568172,0.0469842741347837);
#2219=ELLIPSE('',#34123,0.051274964767697,0.0469971417989173);
#2220=ELLIPSE('',#34126,0.0512707788670663,0.0469842741404324);
#2221=ELLIPSE('',#34127,0.0512749647689531,0.0469971417995761);
#2222=ELLIPSE('',#34130,0.0512707788557115,0.0469842741341769);
#2223=ELLIPSE('',#34131,0.0512749647694815,0.0469971417999415);
#2224=ELLIPSE('',#34134,0.0512707788568934,0.0469842741348491);
#2225=ELLIPSE('',#34135,0.0512749647661315,0.0469971417980767);
#2226=ELLIPSE('',#34138,0.0512707788572177,0.0469842741350563);
#2227=ELLIPSE('',#34139,0.0512749647680353,0.0469971417991282);
#2228=ELLIPSE('',#34142,0.0512707788587383,0.046984274135853);
#2229=ELLIPSE('',#34143,0.0512749647684727,0.0469971417993084);
#2230=ELLIPSE('',#34146,0.0512707788631157,0.0469842741382362);
#2231=ELLIPSE('',#34147,0.0512749647685272,0.0469971417993756);
#2232=ELLIPSE('',#34150,0.0512707788564907,0.0469842741346169);
#2233=ELLIPSE('',#34151,0.0512749647685682,0.0469971417994032);
#2234=ELLIPSE('',#34154,0.0512707788585969,0.0469842741357701);
#2235=ELLIPSE('',#34155,0.0512749647676235,0.0469971417988947);
#2236=ELLIPSE('',#34158,0.0512707788751318,0.0469842741447984);
#2237=ELLIPSE('',#34159,0.0512749647678178,0.0469971417990053);
#2238=ELLIPSE('',#34162,0.0512707788575899,0.0469842741352132);
#2239=ELLIPSE('',#34163,0.0512749647677413,0.0469971417989442);
#2240=ELLIPSE('',#34166,0.0512707788579549,0.0469842741354182);
#2241=ELLIPSE('',#34167,0.0512749647704146,0.0469971418003949);
#2242=ELLIPSE('',#34170,0.0512707788581164,0.0469842741355277);
#2243=ELLIPSE('',#34171,0.0512749647678976,0.0469971417990442);
#2244=ELLIPSE('',#34174,0.0512707788570414,0.0469842741348829);
#2245=ELLIPSE('',#34175,0.0512749647696248,0.0469971417999634);
#2246=ELLIPSE('',#34178,0.0512707789395351,0.0469842741799766);
#2247=ELLIPSE('',#34179,0.0512749647687745,0.0469971417995203);
#2248=ELLIPSE('',#34182,0.0512707788562593,0.0469842741344864);
#2249=ELLIPSE('',#34183,0.0512749647684955,0.046997141799316);
#2250=ELLIPSE('',#34186,0.0512707788603725,0.0469842741367327);
#2251=ELLIPSE('',#34187,0.0512749647690289,0.0469971417996681);
#2252=ELLIPSE('',#34190,0.0512707788577797,0.0469842741353011);
#2253=ELLIPSE('',#34191,0.0512749647683414,0.0469971417992803);
#2254=ELLIPSE('',#34194,0.051270778856875,0.0469842741348193);
#2255=ELLIPSE('',#34195,0.0512749647684586,0.0469971417993373);
#2256=ELLIPSE('',#34198,0.051270778920832,0.0469842741697548);
#2257=ELLIPSE('',#34199,0.0512749647689089,0.0469971417995588);
#2258=ELLIPSE('',#34202,0.0512707788568015,0.0469842741347871);
#2259=ELLIPSE('',#34203,0.0512749647679381,0.0469971417990666);
#2260=ELLIPSE('',#34206,0.0512707788566487,0.046984274134668);
#2261=ELLIPSE('',#34207,0.0512749647684683,0.0469971417993365);
#2262=ELLIPSE('',#34210,0.051270778856618,0.0469842741346731);
#2263=ELLIPSE('',#34211,0.0512749647693393,0.0469971417998184);
#2264=ELLIPSE('',#34214,0.0512707788568358,0.0469842741348282);
#2265=ELLIPSE('',#34215,0.0512749647674564,0.0469971417987839);
#2266=ELLIPSE('',#34218,0.0512707788557633,0.0469842741342339);
#2267=ELLIPSE('',#34219,0.0512749647690638,0.0469971417996539);
#2268=ELLIPSE('',#34222,0.0512707788566786,0.0469842741346996);
#2269=ELLIPSE('',#34223,0.0512749647672967,0.0469971417987006);
#2270=ELLIPSE('',#34226,0.0512707788621377,0.0469842741376985);
#2271=ELLIPSE('',#34227,0.0512749647686591,0.046997141799446);
#2272=ELLIPSE('',#34230,0.0512707788564809,0.0469842741346051);
#2273=ELLIPSE('',#34231,0.0512749647682497,0.0469971417992212);
#2274=ELLIPSE('',#34234,0.0512707788573564,0.0469842741350646);
#2275=ELLIPSE('',#34235,0.0512749647687658,0.0469971417994997);
#2276=ELLIPSE('',#34238,0.051270778874813,0.0469842741446368);
#2277=ELLIPSE('',#34239,0.0512749647675386,0.046997141798832);
#2278=ELLIPSE('',#34242,0.0512707788565269,0.0469842741346491);
#2279=ELLIPSE('',#34243,0.0512749647691996,0.0469971417997275);
#2280=ELLIPSE('',#34246,0.0512707788580797,0.0469842741354721);
#2281=ELLIPSE('',#34247,0.0512749647681002,0.0469971417991393);
#2282=ELLIPSE('',#34250,0.0512707788579047,0.0469842741354009);
#2283=ELLIPSE('',#34251,0.0512749647678865,0.0469971417990283);
#2284=ELLIPSE('',#34254,0.0512707788574115,0.046984274135125);
#2285=ELLIPSE('',#34255,0.0512749647671369,0.0469971417986091);
#2286=ELLIPSE('',#34258,0.0512749647690318,0.0469971417996552);
#2287=ELLIPSE('',#34260,0.0512707788566348,0.0469842741346708);
#2288=ELLIPSE('',#34262,0.0512749647679538,0.0469971417990534);
#2289=ELLIPSE('',#34264,0.0512707788562212,0.0469842741344524);
#2290=ELLIPSE('',#34266,0.051274964768521,0.0469971417993772);
#2291=ELLIPSE('',#34268,0.051270778856042,0.0469842741343731);
#2292=ELLIPSE('',#34270,0.0512749647675581,0.0469971417988677);
#2293=ELLIPSE('',#34272,0.0512707788559885,0.0469842741343514);
#2294=ELLIPSE('',#34274,0.0512749647693218,0.0469971417997968);
#2295=ELLIPSE('',#34276,0.0512707788571387,0.0469842741349643);
#2296=ELLIPSE('',#34278,0.0512749647679417,0.0469971417990759);
#2297=ELLIPSE('',#34280,0.0512707788922353,0.0469842741541131);
#2298=ELLIPSE('',#34282,0.051274964769059,0.046997141799664);
#2299=ELLIPSE('',#34284,0.0512707788612464,0.0469842741372165);
#2300=ELLIPSE('',#34286,0.0512749647686166,0.0469971417994078);
#2301=ELLIPSE('',#34288,0.0512707788558472,0.0469842741342397);
#2302=ELLIPSE('',#34290,0.0512749647686363,0.0469971417994427);
#2303=ELLIPSE('',#34292,0.0512707788567449,0.0469842741347651);
#2304=ELLIPSE('',#34294,0.0512749647684367,0.0469971417993216);
#2305=ELLIPSE('',#34296,0.0512707788561666,0.0469842741344253);
#2306=ELLIPSE('',#34298,0.0512749647683517,0.046997141799283);
#2307=ELLIPSE('',#34300,0.0512707788648064,0.0469842741391505);
#2308=ELLIPSE('',#34302,0.0512749647688174,0.0469971417995523);
#2309=ELLIPSE('',#34304,0.051270778857567,0.0469842741352074);
#2310=ELLIPSE('',#34306,0.0512749647694904,0.0469971417998601);
#2311=ELLIPSE('',#34308,0.0512707788575527,0.0469842741351904);
#2312=ELLIPSE('',#34310,0.0512749647677225,0.0469971417989513);
#2313=ELLIPSE('',#34312,0.0512707788585909,0.0469842741357571);
#2314=ELLIPSE('',#34314,0.051270778940575,0.0469842741805314);
#2315=ELLIPSE('',#34315,0.0512749647683344,0.0469971417992899);
#2316=ELLIPSE('',#34476,0.0512707788678624,0.04698427414088);
#2317=ELLIPSE('',#34477,0.0512749647679163,0.0469971417991227);
#2318=ELLIPSE('',#34479,0.0512749647654335,0.0469971417977818);
#2319=ELLIPSE('',#34480,0.0512707788568347,0.0469842741348514);
#2320=ELLIPSE('',#34482,0.0512749647672852,0.0469971417988039);
#2321=ELLIPSE('',#34483,0.0512707788564686,0.0469842741346539);
#2322=ELLIPSE('',#34485,0.0512749647659393,0.0469971417980464);
#2323=ELLIPSE('',#34486,0.0512707788556944,0.0469842741342504);
#2324=ELLIPSE('',#34488,0.0512749647686629,0.0469971417995544);
#2325=ELLIPSE('',#34489,0.0512707788564297,0.0469842741346479);
#2326=ELLIPSE('',#34491,0.0512749647671486,0.0469971417987065);
#2327=ELLIPSE('',#34492,0.0512707788597197,0.0469842741364453);
#2328=ELLIPSE('',#34494,0.0512749647666077,0.0469971417984174);
#2329=ELLIPSE('',#34495,0.0512707788555701,0.0469842741341628);
#2330=ELLIPSE('',#34497,0.0512749647679515,0.0469971417991682);
#2331=ELLIPSE('',#34498,0.0512707788587403,0.0469842741359266);
#2332=ELLIPSE('',#34500,0.0512749647675462,0.0469971417988912);
#2333=ELLIPSE('',#34501,0.0512707788561996,0.0469842741345216);
#2334=ELLIPSE('',#34503,0.0512749647665171,0.0469971417983294);
#2335=ELLIPSE('',#34504,0.0512707788563593,0.0469842741346364);
#2336=ELLIPSE('',#34506,0.0512749647671419,0.0469971417986936);
#2337=ELLIPSE('',#34507,0.0512707788554834,0.0469842741341348);
#2338=ELLIPSE('',#34509,0.0512749647679126,0.0469971417991247);
#2339=ELLIPSE('',#34510,0.0512707788566136,0.0469842741347507);
#2340=ELLIPSE('',#34512,0.051274964765861,0.0469971417980122);
#2341=ELLIPSE('',#34513,0.0512707788569887,0.0469842741349521);
#2342=ELLIPSE('',#34515,0.0512749647673257,0.046997141798794);
#2343=ELLIPSE('',#34516,0.0512707788578384,0.0469842741354011);
#2344=ELLIPSE('',#34518,0.0512749647685051,0.046997141799409);
#2345=ELLIPSE('',#34519,0.0512707788566497,0.0469842741347448);
#2346=ELLIPSE('',#34521,0.0512749647664023,0.0469971417983194);
#2347=ELLIPSE('',#34522,0.0512707788557973,0.0469842741343033);
#2348=ELLIPSE('',#34524,0.0512749647657081,0.0469971417979273);
#2349=ELLIPSE('',#34525,0.0512707788560454,0.0469842741344356);
#2350=ELLIPSE('',#34527,0.0512749647672847,0.0469971417988018);
#2351=ELLIPSE('',#34528,0.0512707788908472,0.0469842741534398);
#2352=ELLIPSE('',#34530,0.0512749647656979,0.0469971417979225);
#2353=ELLIPSE('',#34531,0.0512707788619598,0.0469842741376821);
#2354=ELLIPSE('',#34533,0.0512749647673844,0.0469971417987892);
#2355=ELLIPSE('',#34534,0.0512707788554361,0.0469842741341347);
#2356=ELLIPSE('',#34536,0.0512749647665351,0.0469971417983737);
#2357=ELLIPSE('',#34537,0.051270778857401,0.0469842741351899);
#2358=ELLIPSE('',#34539,0.0512749647648224,0.0469971417974593);
#2359=ELLIPSE('',#34540,0.051270778857135,0.0469842741350546);
#2360=ELLIPSE('',#34542,0.051274964767923,0.046997141799147);
#2361=ELLIPSE('',#34543,0.0512707788632245,0.0469842741383353);
#2362=ELLIPSE('',#34545,0.0512749647670837,0.0469971417986601);
#2363=ELLIPSE('',#34546,0.0512707788575274,0.0469842741352789);
#2364=ELLIPSE('',#34548,0.0512749647661063,0.046997141798163);
#2365=ELLIPSE('',#34549,0.0512707788614728,0.0469842741374068);
#2366=ELLIPSE('',#34551,0.0512749647661745,0.0469971417981727);
#2367=ELLIPSE('',#34552,0.0512707788561374,0.0469842741344828);
#2368=ELLIPSE('',#34554,0.0512749647684627,0.0469971417993818);
#2369=ELLIPSE('',#34555,0.0512707788547222,0.0469842741337518);
#2370=ELLIPSE('',#34557,0.0512749647675423,0.0469971417989238);
#2371=ELLIPSE('',#34558,0.0512707788556497,0.0469842741342235);
#2372=ELLIPSE('',#34560,0.0512749647674664,0.0469971417988657);
#2373=ELLIPSE('',#34561,0.0512707788563694,0.0469842741346094);
#2374=ELLIPSE('',#34563,0.0512749647689012,0.0469971417996608);
#2375=ELLIPSE('',#34564,0.0512707788554915,0.0469842741341037);
#2376=ELLIPSE('',#34566,0.0512749647674053,0.0469971417988339);
#2377=ELLIPSE('',#34567,0.0512707788551391,0.0469842741339346);
#2378=ELLIPSE('',#34569,0.051274964767584,0.046997141798928);
#2379=ELLIPSE('',#34570,0.0512707788578603,0.0469842741354062);
#2380=ELLIPSE('',#34572,0.0512749647667973,0.046997141798492);
#2381=ELLIPSE('',#34573,0.0512707788554342,0.0469842741340614);
#2382=ELLIPSE('',#34575,0.0512749647663277,0.0469971417982546);
#2383=ELLIPSE('',#34576,0.051270778856014,0.0469842741344105);
#2384=ELLIPSE('',#34578,0.0512749647644558,0.0469971417972658);
#2385=ELLIPSE('',#34579,0.051270778856549,0.046984274134693);
#2386=ELLIPSE('',#34581,0.0512749647655728,0.0469971417978321);
#2387=ELLIPSE('',#34582,0.0512707788565064,0.0469842741346634);
#2388=ELLIPSE('',#34584,0.0512749647677657,0.0469971417990299);
#2389=ELLIPSE('',#34585,0.0512707788566898,0.0469842741347819);
#2390=ELLIPSE('',#34587,0.0512749647676116,0.0469971417989766);
#2391=ELLIPSE('',#34588,0.0512707788912617,0.0469842741536714);
#2392=ELLIPSE('',#34590,0.0512749647664018,0.0469971417982991);
#2393=ELLIPSE('',#34591,0.0512707788616718,0.0469842741375278);
#2394=ELLIPSE('',#34593,0.0512749647667201,0.046997141798501);
#2395=ELLIPSE('',#34594,0.0512707788559321,0.046984274134359);
#2396=ELLIPSE('',#34596,0.0512749647688712,0.0469971417996063);
#2397=ELLIPSE('',#34597,0.0512707788570311,0.0469842741349509);
#2398=ELLIPSE('',#34599,0.0512749647675863,0.0469971417989162);
#2399=ELLIPSE('',#34600,0.0512707788563448,0.0469842741345939);
#2400=ELLIPSE('',#34602,0.0512749647671262,0.0469971417987068);
#2401=ELLIPSE('',#34603,0.0512707788650867,0.0469842741393638);
#2402=ELLIPSE('',#34605,0.0512749647686962,0.0469971417995509);
#2403=ELLIPSE('',#34606,0.0512707788567886,0.0469842741348241);
#2404=ELLIPSE('',#34608,0.0512749647672976,0.0469971417987731);
#2405=ELLIPSE('',#34609,0.0512707788570162,0.0469842741349496);
#2406=ELLIPSE('',#34611,0.0512749647667697,0.0469971417984931);
#2407=ELLIPSE('',#34612,0.0512707788584097,0.0469842741357168);
#2408=ELLIPSE('',#34614,0.0512749647672832,0.0469971417987584);
#2409=ELLIPSE('',#34615,0.0512707788570115,0.0469842741349691);
#2410=ELLIPSE('',#34617,0.0512749647672073,0.0469971417987249);
#2411=ELLIPSE('',#34618,0.0512707789405328,0.0469842741805533);
#2412=ELLIPSE('',#34620,0.0512749647662809,0.0469971417982346);
#2413=ELLIPSE('',#34621,0.0512707788564733,0.0469842741346687);
#2414=ELLIPSE('',#34623,0.0512749647659994,0.0469971417980507);
#2415=ELLIPSE('',#34624,0.0512707788571204,0.0469842741349872);
#2416=ELLIPSE('',#34626,0.0512749647671319,0.0469971417987083);
#2417=ELLIPSE('',#34627,0.0512707788566097,0.0469842741347329);
#2418=ELLIPSE('',#34629,0.0512749647668497,0.0469971417985515);
#2419=ELLIPSE('',#34630,0.0512707788560048,0.0469842741344256);
#2420=ELLIPSE('',#34632,0.051274964765999,0.0469971417980718);
#2421=ELLIPSE('',#34633,0.0512707788746663,0.0469842741446355);
#2422=ELLIPSE('',#34635,0.0512749647672519,0.0469971417987563);
#2423=ELLIPSE('',#34636,0.051270778855846,0.0469842741343271);
#2424=ELLIPSE('',#34638,0.0512749647662359,0.0469971417982146);
#2425=ELLIPSE('',#34639,0.0512707788574978,0.0469842741352291);
#2426=ELLIPSE('',#34641,0.0512749647668179,0.0469971417985263);
#2427=ELLIPSE('',#34642,0.0512707788607044,0.0469842741369976);
#2428=ELLIPSE('',#34644,0.0512749647674441,0.0469971417988379);
#2429=ELLIPSE('',#34645,0.0512707788568965,0.0469842741348871);
#2430=ELLIPSE('',#34647,0.0512749647672645,0.0469971417987703);
#2431=ELLIPSE('',#34648,0.0512707788559945,0.0469842741344026);
#2432=ELLIPSE('',#34650,0.0512749647680151,0.0469971417991764);
#2433=ELLIPSE('',#34651,0.0512707788560419,0.04698427413443);
#2434=ELLIPSE('',#34653,0.0512749647667931,0.0469971417984966);
#2435=ELLIPSE('',#34654,0.0512707788563537,0.0469842741346079);
#2436=ELLIPSE('',#34656,0.0512749647674696,0.0469971417988977);
#2437=ELLIPSE('',#34657,0.0512707788571896,0.0469842741350665);
#2438=ELLIPSE('',#34659,0.0512749647673948,0.046997141798837);
#2439=ELLIPSE('',#34660,0.0512707788555549,0.0469842741341569);
#2440=ELLIPSE('',#34662,0.0512749647668783,0.0469971417985539);
#2441=ELLIPSE('',#34663,0.0512707789210852,0.0469842741699459);
#2442=ELLIPSE('',#34665,0.0512749647677305,0.0469971417990099);
#2443=ELLIPSE('',#34666,0.0512707788552415,0.0469842741340032);
#2444=ELLIPSE('',#34668,0.0512707788564181,0.0469842741346374);
#2445=ELLIPSE('',#34669,0.0512749647669761,0.0469971417985938);
#2446=ELLIPSE('',#34671,0.051270778856969,0.0469842741349151);
#2447=ELLIPSE('',#34672,0.0512749647670935,0.046997141798684);
#2448=ELLIPSE('',#34674,0.0512707788562384,0.0469842741345515);
#2449=ELLIPSE('',#34675,0.0512749647675247,0.0469971417988957);
#2450=ELLIPSE('',#34677,0.0512707788573216,0.0469842741351317);
#2451=ELLIPSE('',#34678,0.0512749647668487,0.046997141798569);
#2452=ELLIPSE('',#34680,0.0512707788622439,0.0469842741378278);
#2453=ELLIPSE('',#34681,0.0512749647677751,0.0469971417990674);
#2454=ELLIPSE('',#34683,0.0512707788576837,0.046984274135325);
#2455=ELLIPSE('',#34684,0.0512749647668911,0.0469971417985504);
#2456=ELLIPSE('',#34686,0.0512707788569353,0.0469842741349273);
#2457=ELLIPSE('',#34687,0.0512749647675315,0.0469971417989158);
#2458=ELLIPSE('',#34689,0.0512707788759282,0.0469842741452617);
#2459=ELLIPSE('',#34690,0.0512749647661136,0.0469971417981488);
#2460=ELLIPSE('',#34692,0.0512707788557471,0.0469842741342912);
#2461=ELLIPSE('',#34693,0.051274964767063,0.0469971417986624);
#2462=ELLIPSE('',#34695,0.0512707788562218,0.0469842741345251);
#2463=ELLIPSE('',#34696,0.0512749647674796,0.0469971417988927);
#2464=ELLIPSE('',#34698,0.0512707788562634,0.0469842741345331);
#2465=ELLIPSE('',#34699,0.0512749647672643,0.0469971417987429);
#2466=ELLIPSE('',#34701,0.0512707788550995,0.0469842741339394);
#2467=ELLIPSE('',#34702,0.0512749647667936,0.0469971417984887);
#2468=ELLIPSE('',#34704,0.0512707789393949,0.0469842741799506);
#2469=ELLIPSE('',#34705,0.0512749647666032,0.0469971417983921);
#2470=ELLIPSE('',#34707,0.0512707788579345,0.0469842741354427);
#2471=ELLIPSE('',#34708,0.0512749647659267,0.0469971417980537);
#2472=ELLIPSE('',#34710,0.0512749647694732,0.0469971417999488);
#2473=ELLIPSE('',#34711,0.0512707788565522,0.0469842741347113);
#2474=ELLIPSE('',#34715,0.0512707788554107,0.0469842741340208);
#2475=ELLIPSE('',#34716,0.0512749647674929,0.0469971417988238);
#2476=ELLIPSE('',#34721,0.0512749647664458,0.0469971417983288);
#2477=ELLIPSE('',#34722,0.0512707788586759,0.0469842741358754);
#2478=ELLIPSE('',#35028,0.0195162536838815,0.0137573643715162);
#2479=ELLIPSE('',#35029,0.0195162536830269,0.0137573643713391);
#2480=ELLIPSE('',#35031,0.0195162536835621,0.0137573643714695);
#2481=ELLIPSE('',#35032,0.019516253683001,0.0137573643713521);
#2482=ELLIPSE('',#35034,0.0195162536836977,0.0137573643714721);
#2483=ELLIPSE('',#35035,0.0195162536830636,0.0137573643713535);
#2484=ELLIPSE('',#35037,0.0195162536837443,0.0137573643714943);
#2485=ELLIPSE('',#35038,0.0195162536831223,0.0137573643713688);
#2486=ELLIPSE('',#35040,0.019516253683803,0.013757364371504);
#2487=ELLIPSE('',#35041,0.0195162536829111,0.0137573643713217);
#2488=ELLIPSE('',#35043,0.0195162536837688,0.0137573643714986);
#2489=ELLIPSE('',#35044,0.0195162536830749,0.0137573643713556);
#2490=ELLIPSE('',#35046,0.0195162536837257,0.0137573643714922);
#2491=ELLIPSE('',#35047,0.0195162536830703,0.0137573643713494);
#2492=ELLIPSE('',#35049,0.0195162536838104,0.013757364371505);
#2493=ELLIPSE('',#35050,0.0195162536830614,0.0137573643713493);
#2494=ELLIPSE('',#35052,0.0195162536837473,0.0137573643714877);
#2495=ELLIPSE('',#35053,0.0195162536830537,0.0137573643713548);
#2496=ELLIPSE('',#35055,0.0195162536838422,0.0137573643715182);
#2497=ELLIPSE('',#35056,0.0195162536831755,0.0137573643713807);
#2498=ELLIPSE('',#35058,0.0195162536837639,0.0137573643714952);
#2499=ELLIPSE('',#35059,0.0195162536830792,0.0137573643713542);
#2500=ELLIPSE('',#35061,0.0195162536835653,0.0137573643714501);
#2501=ELLIPSE('',#35062,0.0195162536831025,0.0137573643713567);
#2502=ELLIPSE('',#35064,0.0195162536835776,0.0137573643714587);
#2503=ELLIPSE('',#35065,0.0195162536828947,0.01375736437132);
#2504=ELLIPSE('',#35067,0.0195162536837483,0.0137573643714995);
#2505=ELLIPSE('',#35068,0.0195162536831204,0.0137573643713664);
#2506=ELLIPSE('',#35070,0.0195162536835793,0.0137573643714601);
#2507=ELLIPSE('',#35071,0.0195162536830448,0.0137573643713492);
#2508=ELLIPSE('',#35080,0.0195034997306777,0.013754915723726);
#2509=ELLIPSE('',#35082,0.0195030685020683,0.0137548403891227);
#2510=ELLIPSE('',#35084,0.0195027524929284,0.0137547851848027);
#2511=ELLIPSE('',#35086,0.0195025132809572,0.0137547433941177);
#2512=ELLIPSE('',#35088,0.0195023280193677,0.0137547110253133);
#2513=ELLIPSE('',#35090,0.0195021823053853,0.0137546855626127);
#2514=ELLIPSE('',#35092,0.0195020666474465,0.0137546653482711);
#2515=ELLIPSE('',#35094,0.0195019745733047,0.0137546492518586);
#2516=ELLIPSE('',#35096,0.0195019015620118,0.0137546364836367);
#2517=ELLIPSE('',#35098,0.0195018443987318,0.0137546264818649);
#2518=ELLIPSE('',#35100,0.0195018007910573,0.0137546188457545);
#2519=ELLIPSE('',#35102,0.0195017691158091,0.0137546132912077);
#2520=ELLIPSE('',#35104,0.0195017482624769,0.0137546096234092);
#2521=ELLIPSE('',#35106,0.0195017375337946,0.0137546077193674);
#2522=ELLIPSE('',#35108,0.0195017365885567,0.0137546075177427);
#2523=ELLIPSE('',#35110,0.0195017454175912,0.0137546090143427);
#2524=ELLIPSE('',#35112,0.0195017643506138,0.0137546122627749);
#2525=ELLIPSE('',#35114,0.0195017941005044,0.0137546173811011);
#2526=ELLIPSE('',#35116,0.0195018358641676,0.0137546245672221);
#2527=ELLIPSE('',#35118,0.0195018727625836,0.013754631431718);
#2528=ELLIPSE('',#35120,0.0195034997306828,0.0137549157237274);
#2529=ELLIPSE('',#35122,0.0195030685021256,0.0137548403891337);
#2530=ELLIPSE('',#35124,0.0195027524929019,0.0137547851847966);
#2531=ELLIPSE('',#35126,0.0195025132809425,0.0137547433941156);
#2532=ELLIPSE('',#35128,0.0195023280193708,0.0137547110253143);
#2533=ELLIPSE('',#35130,0.0195021823053841,0.0137546855626124);
#2534=ELLIPSE('',#35132,0.0195020666474398,0.0137546653482691);
#2535=ELLIPSE('',#35134,0.0195019745733335,0.0137546492518631);
#2536=ELLIPSE('',#35136,0.0195019015619959,0.0137546364836322);
#2537=ELLIPSE('',#35138,0.0195018443987879,0.0137546264818748);
#2538=ELLIPSE('',#35140,0.0195018007910457,0.0137546188457536);
#2539=ELLIPSE('',#35142,0.0195017691158159,0.0137546132912084);
#2540=ELLIPSE('',#35144,0.0195017482624727,0.013754609623408);
#2541=ELLIPSE('',#35146,0.0195017375337736,0.0137546077193644);
#2542=ELLIPSE('',#35148,0.0195017365885347,0.0137546075177382);
#2543=ELLIPSE('',#35150,0.019501745417596,0.0137546090143437);
#2544=ELLIPSE('',#35152,0.0195017643505816,0.0137546122627688);
#2545=ELLIPSE('',#35154,0.0195017941005605,0.0137546173811125);
#2546=ELLIPSE('',#35156,0.019501835864167,0.0137546245672222);
#2547=ELLIPSE('',#35158,0.0195162536830855,0.0137573643713537);
#2548=ELLIPSE('',#35160,0.0195034997307414,0.013754915723739);
#2549=ELLIPSE('',#35162,0.0195030685021161,0.0137548403891323);
#2550=ELLIPSE('',#35164,0.0195027524929008,0.0137547851847961);
#2551=ELLIPSE('',#35166,0.0195025132809546,0.0137547433941189);
#2552=ELLIPSE('',#35168,0.0195023280193482,0.0137547110253084);
#2553=ELLIPSE('',#35185,0.0195034997306463,0.0137549157237206);
#2554=ELLIPSE('',#35187,0.0195030685021557,0.0137548403891397);
#2555=ELLIPSE('',#35189,0.0195027524928776,0.0137547851847918);
#2556=ELLIPSE('',#35191,0.0195025132809776,0.0137547433941213);
#2557=ELLIPSE('',#35193,0.019502328019347,0.0137547110253081);
#2558=ELLIPSE('',#35195,0.0195021823053738,0.0137546855626116);
#2559=ELLIPSE('',#35197,0.0195020666474525,0.0137546653482711);
#2560=ELLIPSE('',#35199,0.0195019745733739,0.013754649251872);
#2561=ELLIPSE('',#35201,0.0195019015619764,0.0137546364836293);
#2562=ELLIPSE('',#35203,0.0195018443987816,0.0137546264818739);
#2563=ELLIPSE('',#35205,0.0195018007910337,0.0137546188457504);
#2564=ELLIPSE('',#35207,0.0195017691158341,0.0137546132912121);
#2565=ELLIPSE('',#35209,0.0195017482624509,0.0137546096234037);
#2566=ELLIPSE('',#35211,0.0195017375337853,0.0137546077193653);
#2567=ELLIPSE('',#35213,0.0195017365886309,0.0137546075177561);
#2568=ELLIPSE('',#35215,0.0195017454176055,0.0137546090143461);
#2569=ELLIPSE('',#35217,0.0195017643505986,0.0137546122627731);
#2570=ELLIPSE('',#35219,0.0195017941005311,0.0137546173811059);
#2571=ELLIPSE('',#35221,0.0195018358641241,0.0137546245672129);
#2572=ELLIPSE('',#35225,0.0195034997306858,0.0137549157237271);
#2573=ELLIPSE('',#35227,0.0195030685021635,0.0137548403891432);
#2574=ELLIPSE('',#35229,0.019502752492881,0.0137547851847926);
#2575=ELLIPSE('',#35231,0.0195025132809236,0.0137547433941134);
#2576=ELLIPSE('',#35233,0.0195023280193679,0.0137547110253125);
#2577=ELLIPSE('',#35235,0.0195021823054267,0.0137546855626225);
#2578=ELLIPSE('',#35237,0.0195020666474927,0.0137546653482813);
#2579=ELLIPSE('',#35239,0.019501974573308,0.0137546492518591);
#2580=ELLIPSE('',#35241,0.0195019015619601,0.0137546364836262);
#2581=ELLIPSE('',#35243,0.0195018443987825,0.0137546264818736);
#2582=ELLIPSE('',#35245,0.0195018007910841,0.0137546188457617);
#2583=ELLIPSE('',#35247,0.0195017691158046,0.0137546132912069);
#2584=ELLIPSE('',#35249,0.0195017482624746,0.0137546096234107);
#2585=ELLIPSE('',#35251,0.0195017375337627,0.0137546077193623);
#2586=ELLIPSE('',#35253,0.0195017365885639,0.0137546075177438);
#2587=ELLIPSE('',#35255,0.0195017454175912,0.0137546090143448);
#2588=ELLIPSE('',#35257,0.0195017643506125,0.0137546122627745);
#2589=ELLIPSE('',#35259,0.0195017941005712,0.0137546173811145);
#2590=ELLIPSE('',#35261,0.0195018358641553,0.013754624567221);
#2591=ELLIPSE('',#35263,0.0195018727626295,0.0137546314317287);
#2592=ELLIPSE('',#35265,0.0195034997307231,0.0137549157237351);
#2593=ELLIPSE('',#35267,0.0195030685021692,0.0137548403891432);
#2594=ELLIPSE('',#35269,0.0195027524928953,0.013754785184795);
#2595=ELLIPSE('',#35271,0.0195025132809505,0.0137547433941165);
#2596=ELLIPSE('',#35273,0.0195023280194302,0.0137547110253254);
#2597=ELLIPSE('',#35275,0.019502182305463,0.0137546855626286);
#2598=ELLIPSE('',#35277,0.0195020666474861,0.0137546653482797);
#2599=ELLIPSE('',#35279,0.0195019745732981,0.0137546492518571);
#2600=ELLIPSE('',#35281,0.019501901562003,0.0137546364836345);
#2601=ELLIPSE('',#35283,0.0195018443988218,0.0137546264818824);
#2602=ELLIPSE('',#35285,0.0195018007911448,0.0137546188457728);
#2603=ELLIPSE('',#35287,0.0195017691157916,0.0137546132912057);
#2604=ELLIPSE('',#35289,0.0195017482624564,0.013754609623407);
#2605=ELLIPSE('',#35291,0.0195017375338029,0.0137546077193704);
#2606=ELLIPSE('',#35293,0.0195017365886144,0.0137546075177533);
#2607=ELLIPSE('',#35295,0.0195017454176306,0.0137546090143512);
#2608=ELLIPSE('',#35297,0.0195017643505891,0.0137546122627708);
#2609=ELLIPSE('',#35299,0.0195017941005193,0.013754617381105);
#2610=ELLIPSE('',#35301,0.0195018358642213,0.0137546245672329);
#2611=ELLIPSE('',#35303,0.0195162536837232,0.0137573643714884);
#2612=ELLIPSE('',#35305,0.0195034997306679,0.0137549157237246);
#2613=ELLIPSE('',#35307,0.0195030685021047,0.0137548403891311);
#2614=ELLIPSE('',#35309,0.0195027524929266,0.0137547851848028);
#2615=ELLIPSE('',#35311,0.0195025132809874,0.0137547433941253);
#2616=ELLIPSE('',#35313,0.0195023280194086,0.013754711025321);
#2617=ELLIPSE('',#35315,0.0195021823054203,0.0137546855626212);
#2618=ELLIPSE('',#35317,0.0195020666475111,0.0137546653482846);
#2619=ELLIPSE('',#35319,0.0195019745733549,0.0137546492518684);
#2620=ELLIPSE('',#35321,0.0195019015619592,0.0137546364836273);
#2621=ELLIPSE('',#35323,0.0195018443988324,0.0137546264818843);
#2622=ELLIPSE('',#35325,0.0195018007910703,0.0137546188457585);
#2623=ELLIPSE('',#35327,0.0195017691158645,0.0137546132912193);
#2624=ELLIPSE('',#35329,0.0195017482624579,0.0137546096234066);
#2625=ELLIPSE('',#35331,0.0195017375338027,0.0137546077193706);
#2626=ELLIPSE('',#35333,0.0195017365886083,0.0137546075177516);
#2627=ELLIPSE('',#35335,0.019501745417535,0.0137546090143326);
#2628=ELLIPSE('',#35337,0.0195017643506093,0.0137546122627733);
#2629=ELLIPSE('',#35339,0.0195017941005168,0.013754617381103);
#2630=ELLIPSE('',#35341,0.0195018358640787,0.0137546245672056);
#2631=ELLIPSE('',#35358,0.0195017365886013,0.0137546075177502);
#2632=ELLIPSE('',#35360,0.0195017454175941,0.0137546090143434);
#2633=ELLIPSE('',#35362,0.0195017643505789,0.0137546122627681);
#2634=ELLIPSE('',#35364,0.0195017941005255,0.0137546173811058);
#2635=ELLIPSE('',#35366,0.0195018358641318,0.0137546245672154);
#2636=ELLIPSE('',#35382,0.051274964768551,0.0469971417993774);
#2637=ELLIPSE('',#35384,0.0512707788579671,0.0469842741354326);
#2638=ELLIPSE('',#35386,0.0512707788562332,0.0469842741344865);
#2639=ELLIPSE('',#35387,0.0512749647685533,0.0469971417993787);
#2640=ELLIPSE('',#35390,0.0512707788571307,0.0469842741349983);
#2641=ELLIPSE('',#35391,0.0512749647672664,0.0469971417987026);
#2642=ELLIPSE('',#35394,0.0512707788571389,0.0469842741349856);
#2643=ELLIPSE('',#35395,0.0512749647681367,0.0469971417991575);
#2644=ELLIPSE('',#35398,0.0512707788569124,0.0469842741348335);
#2645=ELLIPSE('',#35399,0.051274964768467,0.0469971417993732);
#2646=ELLIPSE('',#35402,0.051270778857559,0.0469842741351648);
#2647=ELLIPSE('',#35403,0.0512749647697504,0.0469971418000396);
#2648=ELLIPSE('',#35406,0.051270778857562,0.0469842741352078);
#2649=ELLIPSE('',#35407,0.0512749647676798,0.0469971417989218);
#2650=ELLIPSE('',#35410,0.0512707788610954,0.0469842741371193);
#2651=ELLIPSE('',#35411,0.0512749647674827,0.0469971417988075);
#2652=ELLIPSE('',#35414,0.0512707788555596,0.0469842741341208);
#2653=ELLIPSE('',#35415,0.0512749647677061,0.0469971417989105);
#2654=ELLIPSE('',#35418,0.0512707788650729,0.0469842741392919);
#2655=ELLIPSE('',#35419,0.0512749647702881,0.0469971418003199);
#2656=ELLIPSE('',#35422,0.0512707788560203,0.0469842741343728);
#2657=ELLIPSE('',#35423,0.0512749647689969,0.0469971417996401);
#2658=ELLIPSE('',#35426,0.0512707788567884,0.046984274134799);
#2659=ELLIPSE('',#35427,0.0512749647681247,0.0469971417991492);
#2660=ELLIPSE('',#35430,0.0512707788573083,0.0469842741350659);
#2661=ELLIPSE('',#35431,0.0512749647690658,0.0469971417996437);
#2662=ELLIPSE('',#35434,0.0512707788615306,0.046984274137359);
#2663=ELLIPSE('',#35435,0.051274964767619,0.0469971417988856);
#2664=ELLIPSE('',#35438,0.0512707788928482,0.0469842741544496);
#2665=ELLIPSE('',#35439,0.0512749647695684,0.0469971417999069);
#2666=ELLIPSE('',#35442,0.051270778857717,0.0469842741353091);
#2667=ELLIPSE('',#35443,0.0512749647683041,0.0469971417992544);
#2668=ELLIPSE('',#35446,0.051270778855901,0.046984274134278);
#2669=ELLIPSE('',#35447,0.0512749647692079,0.0469971417997307);
#2670=ELLIPSE('',#35450,0.0512707788585063,0.0469842741357279);
#2671=ELLIPSE('',#35451,0.0512749647681597,0.0469971417991513);
#2672=ELLIPSE('',#35454,0.0512707788568602,0.0469842741348085);
#2673=ELLIPSE('',#35455,0.0512749647674443,0.0469971417987893);
#2674=ELLIPSE('',#35458,0.0512707788568387,0.0469842741347804);
#2675=ELLIPSE('',#35459,0.0512749647678151,0.0469971417990189);
#2676=ELLIPSE('',#35462,0.0512707788582789,0.0469842741356006);
#2677=ELLIPSE('',#35463,0.05127496476906,0.0469971417996405);
#2678=ELLIPSE('',#35466,0.051270778856965,0.0469842741348763);
#2679=ELLIPSE('',#35467,0.0512749647686908,0.046997141799481);
#2680=ELLIPSE('',#35470,0.0512707788563555,0.0469842741344815);
#2681=ELLIPSE('',#35471,0.0512749647673275,0.0469971417987118);
#2682=ELLIPSE('',#35474,0.0512707788571547,0.0469842741350112);
#2683=ELLIPSE('',#35475,0.0512749647685426,0.046997141799397);
#2684=ELLIPSE('',#35478,0.0512707788556612,0.0469842741341707);
#2685=ELLIPSE('',#35479,0.0512749647699517,0.0469971418001559);
#2686=ELLIPSE('',#35482,0.0512707788576472,0.0469842741352346);
#2687=ELLIPSE('',#35483,0.0512749647672529,0.0469971417986806);
#2688=ELLIPSE('',#35486,0.0512707788618793,0.0469842741375491);
#2689=ELLIPSE('',#35487,0.0512749647679756,0.0469971417990623);
#2690=ELLIPSE('',#35490,0.0512707788555002,0.0469842741340957);
#2691=ELLIPSE('',#35491,0.0512749647688844,0.046997141799544);
#2692=ELLIPSE('',#35494,0.0512707788566344,0.0469842741346946);
#2693=ELLIPSE('',#35495,0.051274964769648,0.046997141799953);
#2694=ELLIPSE('',#35498,0.0512707788584597,0.0469842741356599);
#2695=ELLIPSE('',#35499,0.0512749647679757,0.0469971417990702);
#2696=ELLIPSE('',#35502,0.0512707788568172,0.0469842741347837);
#2697=ELLIPSE('',#35503,0.051274964767697,0.0469971417989173);
#2698=ELLIPSE('',#35506,0.0512707788670663,0.0469842741404324);
#2699=ELLIPSE('',#35507,0.0512749647689531,0.0469971417995761);
#2700=ELLIPSE('',#35510,0.0512707788557115,0.0469842741341769);
#2701=ELLIPSE('',#35511,0.0512749647694815,0.0469971417999415);
#2702=ELLIPSE('',#35514,0.0512707788568934,0.0469842741348491);
#2703=ELLIPSE('',#35515,0.0512749647661315,0.0469971417980767);
#2704=ELLIPSE('',#35518,0.0512707788572177,0.0469842741350563);
#2705=ELLIPSE('',#35519,0.0512749647680353,0.0469971417991282);
#2706=ELLIPSE('',#35522,0.0512707788587383,0.046984274135853);
#2707=ELLIPSE('',#35523,0.0512749647684727,0.0469971417993084);
#2708=ELLIPSE('',#35526,0.0512707788631157,0.0469842741382362);
#2709=ELLIPSE('',#35527,0.0512749647685272,0.0469971417993756);
#2710=ELLIPSE('',#35530,0.0512707788564907,0.0469842741346169);
#2711=ELLIPSE('',#35531,0.0512749647685682,0.0469971417994032);
#2712=ELLIPSE('',#35534,0.0512707788585969,0.0469842741357701);
#2713=ELLIPSE('',#35535,0.0512749647676235,0.0469971417988947);
#2714=ELLIPSE('',#35538,0.0512707788751318,0.0469842741447984);
#2715=ELLIPSE('',#35539,0.0512749647678178,0.0469971417990053);
#2716=ELLIPSE('',#35542,0.0512707788575899,0.0469842741352132);
#2717=ELLIPSE('',#35543,0.0512749647677413,0.0469971417989442);
#2718=ELLIPSE('',#35546,0.0512707788579549,0.0469842741354182);
#2719=ELLIPSE('',#35547,0.0512749647704146,0.0469971418003949);
#2720=ELLIPSE('',#35550,0.0512707788581164,0.0469842741355277);
#2721=ELLIPSE('',#35551,0.0512749647678976,0.0469971417990442);
#2722=ELLIPSE('',#35554,0.0512707788570414,0.0469842741348829);
#2723=ELLIPSE('',#35555,0.0512749647696248,0.0469971417999634);
#2724=ELLIPSE('',#35558,0.0512707789395351,0.0469842741799766);
#2725=ELLIPSE('',#35559,0.0512749647687745,0.0469971417995203);
#2726=ELLIPSE('',#35562,0.0512707788562593,0.0469842741344864);
#2727=ELLIPSE('',#35563,0.0512749647684955,0.046997141799316);
#2728=ELLIPSE('',#35566,0.0512707788603725,0.0469842741367327);
#2729=ELLIPSE('',#35567,0.0512749647690289,0.0469971417996681);
#2730=ELLIPSE('',#35570,0.0512707788577797,0.0469842741353011);
#2731=ELLIPSE('',#35571,0.0512749647683414,0.0469971417992803);
#2732=ELLIPSE('',#35574,0.051270778856875,0.0469842741348193);
#2733=ELLIPSE('',#35575,0.0512749647684586,0.0469971417993373);
#2734=ELLIPSE('',#35578,0.051270778920832,0.0469842741697548);
#2735=ELLIPSE('',#35579,0.0512749647689089,0.0469971417995588);
#2736=ELLIPSE('',#35582,0.0512707788568015,0.0469842741347871);
#2737=ELLIPSE('',#35583,0.0512749647679381,0.0469971417990666);
#2738=ELLIPSE('',#35586,0.0512707788566487,0.046984274134668);
#2739=ELLIPSE('',#35587,0.0512749647684683,0.0469971417993365);
#2740=ELLIPSE('',#35590,0.051270778856618,0.0469842741346731);
#2741=ELLIPSE('',#35591,0.0512749647693393,0.0469971417998184);
#2742=ELLIPSE('',#35594,0.0512707788568358,0.0469842741348282);
#2743=ELLIPSE('',#35595,0.0512749647674564,0.0469971417987839);
#2744=ELLIPSE('',#35598,0.0512707788557633,0.0469842741342339);
#2745=ELLIPSE('',#35599,0.0512749647690638,0.0469971417996539);
#2746=ELLIPSE('',#35602,0.0512707788566786,0.0469842741346996);
#2747=ELLIPSE('',#35603,0.0512749647672967,0.0469971417987006);
#2748=ELLIPSE('',#35606,0.0512707788621377,0.0469842741376985);
#2749=ELLIPSE('',#35607,0.0512749647686591,0.046997141799446);
#2750=ELLIPSE('',#35610,0.0512707788564809,0.0469842741346051);
#2751=ELLIPSE('',#35611,0.0512749647682497,0.0469971417992212);
#2752=ELLIPSE('',#35614,0.0512707788573564,0.0469842741350646);
#2753=ELLIPSE('',#35615,0.0512749647687658,0.0469971417994997);
#2754=ELLIPSE('',#35618,0.051270778874813,0.0469842741446368);
#2755=ELLIPSE('',#35619,0.0512749647675386,0.046997141798832);
#2756=ELLIPSE('',#35622,0.0512707788565269,0.0469842741346491);
#2757=ELLIPSE('',#35623,0.0512749647691996,0.0469971417997275);
#2758=ELLIPSE('',#35626,0.0512707788580797,0.0469842741354721);
#2759=ELLIPSE('',#35627,0.0512749647681002,0.0469971417991393);
#2760=ELLIPSE('',#35630,0.0512707788579047,0.0469842741354009);
#2761=ELLIPSE('',#35631,0.0512749647678865,0.0469971417990283);
#2762=ELLIPSE('',#35634,0.0512707788574115,0.046984274135125);
#2763=ELLIPSE('',#35635,0.0512749647671369,0.0469971417986091);
#2764=ELLIPSE('',#35638,0.0512749647690318,0.0469971417996552);
#2765=ELLIPSE('',#35640,0.0512707788566348,0.0469842741346708);
#2766=ELLIPSE('',#35642,0.0512749647679538,0.0469971417990534);
#2767=ELLIPSE('',#35644,0.0512707788562212,0.0469842741344524);
#2768=ELLIPSE('',#35646,0.051274964768521,0.0469971417993772);
#2769=ELLIPSE('',#35648,0.051270778856042,0.0469842741343731);
#2770=ELLIPSE('',#35650,0.0512749647675581,0.0469971417988677);
#2771=ELLIPSE('',#35652,0.0512707788559885,0.0469842741343514);
#2772=ELLIPSE('',#35654,0.0512749647693218,0.0469971417997968);
#2773=ELLIPSE('',#35656,0.0512707788571387,0.0469842741349643);
#2774=ELLIPSE('',#35658,0.0512749647679417,0.0469971417990759);
#2775=ELLIPSE('',#35660,0.0512707788922353,0.0469842741541131);
#2776=ELLIPSE('',#35662,0.051274964769059,0.046997141799664);
#2777=ELLIPSE('',#35664,0.0512707788612464,0.0469842741372165);
#2778=ELLIPSE('',#35666,0.0512749647686166,0.0469971417994078);
#2779=ELLIPSE('',#35668,0.0512707788558472,0.0469842741342397);
#2780=ELLIPSE('',#35670,0.0512749647686363,0.0469971417994427);
#2781=ELLIPSE('',#35672,0.0512707788567449,0.0469842741347651);
#2782=ELLIPSE('',#35674,0.0512749647684367,0.0469971417993216);
#2783=ELLIPSE('',#35676,0.0512707788561666,0.0469842741344253);
#2784=ELLIPSE('',#35678,0.0512749647683517,0.046997141799283);
#2785=ELLIPSE('',#35680,0.0512707788648064,0.0469842741391505);
#2786=ELLIPSE('',#35682,0.0512749647688174,0.0469971417995523);
#2787=ELLIPSE('',#35684,0.051270778857567,0.0469842741352074);
#2788=ELLIPSE('',#35686,0.0512749647694904,0.0469971417998601);
#2789=ELLIPSE('',#35688,0.0512707788575527,0.0469842741351904);
#2790=ELLIPSE('',#35690,0.0512749647677225,0.0469971417989513);
#2791=ELLIPSE('',#35692,0.0512707788585909,0.0469842741357571);
#2792=ELLIPSE('',#35694,0.051270778940575,0.0469842741805314);
#2793=ELLIPSE('',#35695,0.0512749647683344,0.0469971417992899);
#2794=ELLIPSE('',#35856,0.0512707788678624,0.04698427414088);
#2795=ELLIPSE('',#35857,0.0512749647679163,0.0469971417991227);
#2796=ELLIPSE('',#35859,0.0512749647654335,0.0469971417977818);
#2797=ELLIPSE('',#35860,0.0512707788568347,0.0469842741348514);
#2798=ELLIPSE('',#35862,0.0512749647672852,0.0469971417988039);
#2799=ELLIPSE('',#35863,0.0512707788564686,0.0469842741346539);
#2800=ELLIPSE('',#35865,0.0512749647659393,0.0469971417980464);
#2801=ELLIPSE('',#35866,0.0512707788556944,0.0469842741342504);
#2802=ELLIPSE('',#35868,0.0512749647686629,0.0469971417995544);
#2803=ELLIPSE('',#35869,0.0512707788564297,0.0469842741346479);
#2804=ELLIPSE('',#35871,0.0512749647671486,0.0469971417987065);
#2805=ELLIPSE('',#35872,0.0512707788597197,0.0469842741364453);
#2806=ELLIPSE('',#35874,0.0512749647666077,0.0469971417984174);
#2807=ELLIPSE('',#35875,0.0512707788555701,0.0469842741341628);
#2808=ELLIPSE('',#35877,0.0512749647679515,0.0469971417991682);
#2809=ELLIPSE('',#35878,0.0512707788587403,0.0469842741359266);
#2810=ELLIPSE('',#35880,0.0512749647675462,0.0469971417988912);
#2811=ELLIPSE('',#35881,0.0512707788561996,0.0469842741345216);
#2812=ELLIPSE('',#35883,0.0512749647665171,0.0469971417983294);
#2813=ELLIPSE('',#35884,0.0512707788563593,0.0469842741346364);
#2814=ELLIPSE('',#35886,0.0512749647671419,0.0469971417986936);
#2815=ELLIPSE('',#35887,0.0512707788554834,0.0469842741341348);
#2816=ELLIPSE('',#35889,0.0512749647679126,0.0469971417991247);
#2817=ELLIPSE('',#35890,0.0512707788566136,0.0469842741347507);
#2818=ELLIPSE('',#35892,0.051274964765861,0.0469971417980122);
#2819=ELLIPSE('',#35893,0.0512707788569887,0.0469842741349521);
#2820=ELLIPSE('',#35895,0.0512749647673257,0.046997141798794);
#2821=ELLIPSE('',#35896,0.0512707788578384,0.0469842741354011);
#2822=ELLIPSE('',#35898,0.0512749647685051,0.046997141799409);
#2823=ELLIPSE('',#35899,0.0512707788566497,0.0469842741347448);
#2824=ELLIPSE('',#35901,0.0512749647664023,0.0469971417983194);
#2825=ELLIPSE('',#35902,0.0512707788557973,0.0469842741343033);
#2826=ELLIPSE('',#35904,0.0512749647657081,0.0469971417979273);
#2827=ELLIPSE('',#35905,0.0512707788560454,0.0469842741344356);
#2828=ELLIPSE('',#35907,0.0512749647672847,0.0469971417988018);
#2829=ELLIPSE('',#35908,0.0512707788908472,0.0469842741534398);
#2830=ELLIPSE('',#35910,0.0512749647656979,0.0469971417979225);
#2831=ELLIPSE('',#35911,0.0512707788619598,0.0469842741376821);
#2832=ELLIPSE('',#35913,0.0512749647673844,0.0469971417987892);
#2833=ELLIPSE('',#35914,0.0512707788554361,0.0469842741341347);
#2834=ELLIPSE('',#35916,0.0512749647665351,0.0469971417983737);
#2835=ELLIPSE('',#35917,0.051270778857401,0.0469842741351899);
#2836=ELLIPSE('',#35919,0.0512749647648224,0.0469971417974593);
#2837=ELLIPSE('',#35920,0.051270778857135,0.0469842741350546);
#2838=ELLIPSE('',#35922,0.051274964767923,0.046997141799147);
#2839=ELLIPSE('',#35923,0.0512707788632245,0.0469842741383353);
#2840=ELLIPSE('',#35925,0.0512749647670837,0.0469971417986601);
#2841=ELLIPSE('',#35926,0.0512707788575274,0.0469842741352789);
#2842=ELLIPSE('',#35928,0.0512749647661063,0.046997141798163);
#2843=ELLIPSE('',#35929,0.0512707788614728,0.0469842741374068);
#2844=ELLIPSE('',#35931,0.0512749647661745,0.0469971417981727);
#2845=ELLIPSE('',#35932,0.0512707788561374,0.0469842741344828);
#2846=ELLIPSE('',#35934,0.0512749647684627,0.0469971417993818);
#2847=ELLIPSE('',#35935,0.0512707788547222,0.0469842741337518);
#2848=ELLIPSE('',#35937,0.0512749647675423,0.0469971417989238);
#2849=ELLIPSE('',#35938,0.0512707788556497,0.0469842741342235);
#2850=ELLIPSE('',#35940,0.0512749647674664,0.0469971417988657);
#2851=ELLIPSE('',#35941,0.0512707788563694,0.0469842741346094);
#2852=ELLIPSE('',#35943,0.0512749647689012,0.0469971417996608);
#2853=ELLIPSE('',#35944,0.0512707788554915,0.0469842741341037);
#2854=ELLIPSE('',#35946,0.0512749647674053,0.0469971417988339);
#2855=ELLIPSE('',#35947,0.0512707788551391,0.0469842741339346);
#2856=ELLIPSE('',#35949,0.051274964767584,0.046997141798928);
#2857=ELLIPSE('',#35950,0.0512707788578603,0.0469842741354062);
#2858=ELLIPSE('',#35952,0.0512749647667973,0.046997141798492);
#2859=ELLIPSE('',#35953,0.0512707788554342,0.0469842741340614);
#2860=ELLIPSE('',#35955,0.0512749647663277,0.0469971417982546);
#2861=ELLIPSE('',#35956,0.051270778856014,0.0469842741344105);
#2862=ELLIPSE('',#35958,0.0512749647644558,0.0469971417972658);
#2863=ELLIPSE('',#35959,0.051270778856549,0.046984274134693);
#2864=ELLIPSE('',#35961,0.0512749647655728,0.0469971417978321);
#2865=ELLIPSE('',#35962,0.0512707788565064,0.0469842741346634);
#2866=ELLIPSE('',#35964,0.0512749647677657,0.0469971417990299);
#2867=ELLIPSE('',#35965,0.0512707788566898,0.0469842741347819);
#2868=ELLIPSE('',#35967,0.0512749647676116,0.0469971417989766);
#2869=ELLIPSE('',#35968,0.0512707788912617,0.0469842741536714);
#2870=ELLIPSE('',#35970,0.0512749647664018,0.0469971417982991);
#2871=ELLIPSE('',#35971,0.0512707788616718,0.0469842741375278);
#2872=ELLIPSE('',#35973,0.0512749647667201,0.046997141798501);
#2873=ELLIPSE('',#35974,0.0512707788559321,0.046984274134359);
#2874=ELLIPSE('',#35976,0.0512749647688712,0.0469971417996063);
#2875=ELLIPSE('',#35977,0.0512707788570311,0.0469842741349509);
#2876=ELLIPSE('',#35979,0.0512749647675863,0.0469971417989162);
#2877=ELLIPSE('',#35980,0.0512707788563448,0.0469842741345939);
#2878=ELLIPSE('',#35982,0.0512749647671262,0.0469971417987068);
#2879=ELLIPSE('',#35983,0.0512707788650867,0.0469842741393638);
#2880=ELLIPSE('',#35985,0.0512749647686962,0.0469971417995509);
#2881=ELLIPSE('',#35986,0.0512707788567886,0.0469842741348241);
#2882=ELLIPSE('',#35988,0.0512749647672976,0.0469971417987731);
#2883=ELLIPSE('',#35989,0.0512707788570162,0.0469842741349496);
#2884=ELLIPSE('',#35991,0.0512749647667697,0.0469971417984931);
#2885=ELLIPSE('',#35992,0.0512707788584097,0.0469842741357168);
#2886=ELLIPSE('',#35994,0.0512749647672832,0.0469971417987584);
#2887=ELLIPSE('',#35995,0.0512707788570115,0.0469842741349691);
#2888=ELLIPSE('',#35997,0.0512749647672073,0.0469971417987249);
#2889=ELLIPSE('',#35998,0.0512707789405328,0.0469842741805533);
#2890=ELLIPSE('',#36000,0.0512749647662809,0.0469971417982346);
#2891=ELLIPSE('',#36001,0.0512707788564733,0.0469842741346687);
#2892=ELLIPSE('',#36003,0.0512749647659994,0.0469971417980507);
#2893=ELLIPSE('',#36004,0.0512707788571204,0.0469842741349872);
#2894=ELLIPSE('',#36006,0.0512749647671319,0.0469971417987083);
#2895=ELLIPSE('',#36007,0.0512707788566097,0.0469842741347329);
#2896=ELLIPSE('',#36009,0.0512749647668497,0.0469971417985515);
#2897=ELLIPSE('',#36010,0.0512707788560048,0.0469842741344256);
#2898=ELLIPSE('',#36012,0.051274964765999,0.0469971417980718);
#2899=ELLIPSE('',#36013,0.0512707788746663,0.0469842741446355);
#2900=ELLIPSE('',#36015,0.0512749647672519,0.0469971417987563);
#2901=ELLIPSE('',#36016,0.051270778855846,0.0469842741343271);
#2902=ELLIPSE('',#36018,0.0512749647662359,0.0469971417982146);
#2903=ELLIPSE('',#36019,0.0512707788574978,0.0469842741352291);
#2904=ELLIPSE('',#36021,0.0512749647668179,0.0469971417985263);
#2905=ELLIPSE('',#36022,0.0512707788607044,0.0469842741369976);
#2906=ELLIPSE('',#36024,0.0512749647674441,0.0469971417988379);
#2907=ELLIPSE('',#36025,0.0512707788568965,0.0469842741348871);
#2908=ELLIPSE('',#36027,0.0512749647672645,0.0469971417987703);
#2909=ELLIPSE('',#36028,0.0512707788559945,0.0469842741344026);
#2910=ELLIPSE('',#36030,0.0512749647680151,0.0469971417991764);
#2911=ELLIPSE('',#36031,0.0512707788560419,0.04698427413443);
#2912=ELLIPSE('',#36033,0.0512749647667931,0.0469971417984966);
#2913=ELLIPSE('',#36034,0.0512707788563537,0.0469842741346079);
#2914=ELLIPSE('',#36036,0.0512749647674696,0.0469971417988977);
#2915=ELLIPSE('',#36037,0.0512707788571896,0.0469842741350665);
#2916=ELLIPSE('',#36039,0.0512749647673948,0.046997141798837);
#2917=ELLIPSE('',#36040,0.0512707788555549,0.0469842741341569);
#2918=ELLIPSE('',#36042,0.0512749647668783,0.0469971417985539);
#2919=ELLIPSE('',#36043,0.0512707789210852,0.0469842741699459);
#2920=ELLIPSE('',#36045,0.0512749647677305,0.0469971417990099);
#2921=ELLIPSE('',#36046,0.0512707788552415,0.0469842741340032);
#2922=ELLIPSE('',#36048,0.0512707788564181,0.0469842741346374);
#2923=ELLIPSE('',#36049,0.0512749647669761,0.0469971417985938);
#2924=ELLIPSE('',#36051,0.051270778856969,0.0469842741349151);
#2925=ELLIPSE('',#36052,0.0512749647670935,0.046997141798684);
#2926=ELLIPSE('',#36054,0.0512707788562384,0.0469842741345515);
#2927=ELLIPSE('',#36055,0.0512749647675247,0.0469971417988957);
#2928=ELLIPSE('',#36057,0.0512707788573216,0.0469842741351317);
#2929=ELLIPSE('',#36058,0.0512749647668487,0.046997141798569);
#2930=ELLIPSE('',#36060,0.0512707788622439,0.0469842741378278);
#2931=ELLIPSE('',#36061,0.0512749647677751,0.0469971417990674);
#2932=ELLIPSE('',#36063,0.0512707788576837,0.046984274135325);
#2933=ELLIPSE('',#36064,0.0512749647668911,0.0469971417985504);
#2934=ELLIPSE('',#36066,0.0512707788569353,0.0469842741349273);
#2935=ELLIPSE('',#36067,0.0512749647675315,0.0469971417989158);
#2936=ELLIPSE('',#36069,0.0512707788759282,0.0469842741452617);
#2937=ELLIPSE('',#36070,0.0512749647661136,0.0469971417981488);
#2938=ELLIPSE('',#36072,0.0512707788557471,0.0469842741342912);
#2939=ELLIPSE('',#36073,0.051274964767063,0.0469971417986624);
#2940=ELLIPSE('',#36075,0.0512707788562218,0.0469842741345251);
#2941=ELLIPSE('',#36076,0.0512749647674796,0.0469971417988927);
#2942=ELLIPSE('',#36078,0.0512707788562634,0.0469842741345331);
#2943=ELLIPSE('',#36079,0.0512749647672643,0.0469971417987429);
#2944=ELLIPSE('',#36081,0.0512707788550995,0.0469842741339394);
#2945=ELLIPSE('',#36082,0.0512749647667936,0.0469971417984887);
#2946=ELLIPSE('',#36084,0.0512707789393949,0.0469842741799506);
#2947=ELLIPSE('',#36085,0.0512749647666032,0.0469971417983921);
#2948=ELLIPSE('',#36087,0.0512707788579345,0.0469842741354427);
#2949=ELLIPSE('',#36088,0.0512749647659267,0.0469971417980537);
#2950=ELLIPSE('',#36090,0.0512749647694732,0.0469971417999488);
#2951=ELLIPSE('',#36091,0.0512707788565522,0.0469842741347113);
#2952=ELLIPSE('',#36095,0.0512707788554107,0.0469842741340208);
#2953=ELLIPSE('',#36096,0.0512749647674929,0.0469971417988238);
#2954=ELLIPSE('',#36101,0.0512749647664458,0.0469971417983288);
#2955=ELLIPSE('',#36102,0.0512707788586759,0.0469842741358754);
#2956=CONICAL_SURFACE('',#32228,1.17524047358084,0.785398163397443);
#2957=CONICAL_SURFACE('',#32263,1.17524047358084,0.785398163397443);
#2958=CONICAL_SURFACE('',#32312,1.55162884844711,0.78539816339745);
#2959=CONICAL_SURFACE('',#32318,2.73627063036812,0.785398163397448);
#2960=CONICAL_SURFACE('',#32463,2.68872936963188,0.785398163397435);
#2961=CONICAL_SURFACE('',#33351,1732.05080756885,1.04719755119659);
#2962=CONICAL_SURFACE('',#33608,1.17524047358084,0.785398163397443);
#2963=CONICAL_SURFACE('',#33643,1.17524047358084,0.785398163397443);
#2964=CONICAL_SURFACE('',#33692,1.55162884844711,0.78539816339745);
#2965=CONICAL_SURFACE('',#33698,2.73627063036812,0.785398163397448);
#2966=CONICAL_SURFACE('',#33843,2.68872936963188,0.785398163397435);
#2967=CONICAL_SURFACE('',#34731,1732.05080756885,1.04719755119659);
#2968=CONICAL_SURFACE('',#34988,1.17524047358084,0.785398163397443);
#2969=CONICAL_SURFACE('',#35023,1.17524047358084,0.785398163397443);
#2970=CONICAL_SURFACE('',#35072,1.55162884844711,0.78539816339745);
#2971=CONICAL_SURFACE('',#35078,2.73627063036812,0.785398163397448);
#2972=CONICAL_SURFACE('',#35223,2.68872936963188,0.785398163397435);
#2973=CONICAL_SURFACE('',#36111,1732.05080756885,1.04719755119659);
#2974=B_SPLINE_CURVE_WITH_KNOTS('',3,(#46248,#46249,#46250,#46251,#46252,
#46253,#46254,#46255,#46256,#46257,#46258,#46259,#46260,#46261,#46262,#46263,
#46264,#46265,#46266,#46267,#46268,#46269,#46270,#46271,#46272,#46273,#46274,
#46275,#46276,#46277,#46278,#46279,#46280,#46281,#46282,#46283),
 .UNSPECIFIED.,.F.,.F.,(4,2,2,2,2,2,2,2,2,2,2,2,2,2,2,2,2,4),(-0.945073641183675,
-0.895238035194944,-0.83625541046657,-0.779319325111488,-0.719695813140934,
-0.661359932358853,-0.603989382535731,-0.544046656752618,-0.486380595229568,
-0.427463950957105,-0.368285170516134,-0.311258814957492,-0.251615042406746,
-0.193080680180277,-0.135881569867343,-0.0757214675349668,-0.0372079607299379,
-9.99999995143774E-7),.UNSPECIFIED.);
#2975=B_SPLINE_CURVE_WITH_KNOTS('',3,(#46289,#46290,#46291,#46292,#46293,
#46294,#46295,#46296,#46297,#46298,#46299,#46300,#46301,#46302,#46303,#46304,
#46305,#46306,#46307,#46308,#46309,#46310,#46311,#46312,#46313,#46314,#46315,
#46316,#46317,#46318,#46319,#46320,#46321,#46322),.UNSPECIFIED.,.F.,.F.,
(4,2,2,2,2,2,2,2,2,2,2,2,2,2,2,2,4),(-27.258759550315,-27.2281298462553,
-27.1982051538512,-27.1403355656588,-27.0801605899845,-27.0231066733285,
-26.9645639497272,-26.9050010855415,-26.8479917157334,-26.7888070303952,
-26.7302213719406,-26.6725610910419,-26.6126177738291,-26.5554428144319,
-26.4971129260297,-26.4375855046171,-26.4315188069733),.UNSPECIFIED.);
#2976=B_SPLINE_CURVE_WITH_KNOTS('',3,(#46327,#46328,#46329,#46330,#46331,
#46332,#46333,#46334,#46335,#46336,#46337,#46338,#46339,#46340,#46341,#46342,
#46343,#46344,#46345,#46346,#46347,#46348,#46349,#46350,#46351,#46352,#46353,
#46354,#46355,#46356,#46357,#46358,#46359,#46360,#46361,#46362),
 .UNSPECIFIED.,.F.,.F.,(4,2,2,2,2,2,2,2,2,2,2,2,2,2,2,2,2,4),(-1.89025095676006,
-1.83161362612537,-1.77291723413503,-1.71588088128378,-1.65621305093223,
-1.59816806724067,-1.54019307596245,-1.48057902624682,-1.42320721251111,
-1.36315245228605,-1.30433237640506,-1.24738924893859,-1.18775702178512,
-1.12958586526634,-1.07195013380193,-1.0121910944455,-0.954689933605391,
-0.945073641183675),.UNSPECIFIED.);
#2977=B_SPLINE_CURVE_WITH_KNOTS('',3,(#46363,#46364,#46365,#46366,#46367,
#46368,#46369,#46370,#46371,#46372,#46373,#46374,#46375,#46376,#46377,#46378,
#46379,#46380,#46381,#46382,#46383,#46384,#46385,#46386,#46387,#46388,#46389,
#46390,#46391,#46392,#46393,#46394,#46395,#46396,#46397,#46398),
 .UNSPECIFIED.,.F.,.F.,(4,2,2,2,2,2,2,2,2,2,2,2,2,2,2,2,2,4),(-26.4315188069733,
-26.3807149169946,-26.3217404209326,-26.2626652889544,-26.2051855221022,
-26.1454428390691,-26.08804784233,-26.0298996832198,-25.970377539516,-25.9135472636022,
-25.8547523829465,-25.7951046336945,-25.7377721236726,-25.6781939173096,
-25.6204935481626,-25.5624909627037,-25.5029463840743,-25.4881909358829),
 .UNSPECIFIED.);
#2978=B_SPLINE_CURVE_WITH_KNOTS('',3,(#46403,#46404,#46405,#46406,#46407,
#46408,#46409,#46410,#46411,#46412,#46413,#46414,#46415,#46416,#46417,#46418,
#46419,#46420,#46421,#46422,#46423,#46424,#46425,#46426,#46427,#46428,#46429,
#46430,#46431,#46432,#46433,#46434,#46435,#46436,#46437,#46438,#46439,#46440),
 .UNSPECIFIED.,.F.,.F.,(4,2,2,2,2,2,2,2,2,2,2,2,2,2,2,2,2,2,4),(-2.83625896355377,
-2.82853093222041,-2.76886611006394,-2.71046756100465,-2.65308502383756,
-2.59307616772703,-2.5353480705631,-2.47645222776391,-2.41720668492958,
-2.36012338869581,-2.30043449435393,-2.24183347940531,-2.1846099393252,
-2.12437972037366,-2.06645193254166,-2.00798057621261,-1.94850769470731,
-1.89126109663031,-1.89025095676006),.UNSPECIFIED.);
#2979=B_SPLINE_CURVE_WITH_KNOTS('',3,(#46441,#46442,#46443,#46444,#46445,
#46446,#46447,#46448,#46449,#46450,#46451,#46452,#46453,#46454,#46455,#46456,
#46457,#46458,#46459,#46460,#46461,#46462,#46463,#46464,#46465,#46466,#46467,
#46468,#46469,#46470,#46471,#46472,#46473,#46474,#46475,#46476),
 .UNSPECIFIED.,.F.,.F.,(4,2,2,2,2,2,2,2,2,2,2,2,2,2,2,2,2,4),(-25.4881909358829,
-25.4460636732589,-25.3874120918811,-25.3278816537184,-25.2706841301686,
-25.2112575632321,-25.1531186176646,-25.0952452143788,-25.0350644348795,
-24.9780430196917,-24.9194961959997,-24.8599520194551,-24.8029424006809,
-24.7437542679059,-24.6852489172368,-24.6275880933991,-24.5676424609794,
-24.544394043377),.UNSPECIFIED.);
#2980=B_SPLINE_CURVE_WITH_KNOTS('',3,(#46481,#46482,#46483,#46484,#46485,
#46486,#46487,#46488,#46489,#46490,#46491,#46492,#46493,#46494,#46495,#46496,
#46497,#46498,#46499,#46500,#46501,#46502,#46503,#46504,#46505,#46506,#46507,
#46508,#46509,#46510,#46511,#46512,#46513,#46514,#46515,#46516),
 .UNSPECIFIED.,.F.,.F.,(4,2,2,2,2,2,2,2,2,2,2,2,2,2,2,2,2,4),(-3.78192035948685,
-3.76562796298537,-3.70592564973338,-3.6478278361799,-3.5898592957152,-3.53018901929876,
-3.47276427223133,-3.41274694188657,-3.3538687217505,-3.29689298752725,
-3.2372230084892,-3.17899386626536,-3.12135698149028,-3.06153650613278,
-3.00397762776562,-2.94455692608413,-2.88551146939021,-2.83625896355377),
 .UNSPECIFIED.);
#2981=B_SPLINE_CURVE_WITH_KNOTS('',3,(#46517,#46518,#46519,#46520,#46521,
#46522,#46523,#46524,#46525,#46526,#46527,#46528,#46529,#46530,#46531,#46532,
#46533,#46534,#46535,#46536,#46537,#46538,#46539,#46540,#46541,#46542,#46543,
#46544,#46545,#46546,#46547,#46548,#46549,#46550,#46551,#46552),
 .UNSPECIFIED.,.F.,.F.,(4,2,2,2,2,2,2,2,2,2,2,2,2,2,2,2,2,4),(-24.544394043377,
-24.5105131978097,-24.4521827141638,-24.3926780124691,-24.3358195936076,
-24.2768451471733,-24.2178632708879,-24.1603868788961,-24.1006461200198,
-24.0433090290329,-23.9851645307063,-23.9256688814307,-23.8688632830925,
-23.8100726156683,-23.7505272749807,-23.6932025949219,-23.6336311604901,
-23.6014349735858),.UNSPECIFIED.);
#2982=B_SPLINE_CURVE_WITH_KNOTS('',3,(#46557,#46558,#46559,#46560,#46561,
#46562,#46563,#46564,#46565,#46566,#46567,#46568,#46569,#46570,#46571,#46572,
#46573,#46574,#46575,#46576,#46577,#46578,#46579,#46580,#46581,#46582,#46583,
#46584,#46585,#46586,#46587,#46588,#46589,#46590,#46591,#46592),
 .UNSPECIFIED.,.F.,.F.,(4,2,2,2,2,2,2,2,2,2,2,2,2,2,2,2,2,4),(-4.72839430207058,
-4.70337431740566,-4.64331595464347,-4.58554178921411,-4.52667966073054,
-4.4673838894256,-4.41025831032806,-4.35054027250619,-4.29188896156004,
-4.23465469260147,-4.17437122548907,-4.11639389057874,-4.05794278357937,
-3.99841660337735,-3.94111979450562,-3.88143640467257,-3.82268708479341,
-3.78192035948685),.UNSPECIFIED.);
#2983=B_SPLINE_CURVE_WITH_KNOTS('',3,(#46593,#46594,#46595,#46596,#46597,
#46598,#46599,#46600,#46601,#46602,#46603,#46604,#46605,#46606,#46607,#46608,
#46609,#46610,#46611,#46612,#46613,#46614,#46615,#46616,#46617,#46618,#46619,
#46620,#46621,#46622,#46623,#46624,#46625,#46626,#46627,#46628),
 .UNSPECIFIED.,.F.,.F.,(4,2,2,2,2,2,2,2,2,2,2,2,2,2,2,2,2,4),(-23.6014349735858,
-23.5759985868542,-23.5180045036599,-23.458489879113,-23.4016430359386,
-23.3430005479742,-23.2834982736845,-23.226310920464,-23.166893628097,-23.1088378874003,
-23.0509758826866,-22.9908049952875,-22.9338319947597,-22.8752964277514,
-22.8157879004539,-22.7587920199088,-22.6996160282244,-22.6581171675807),
 .UNSPECIFIED.);
#2984=B_SPLINE_CURVE_WITH_KNOTS('',3,(#46633,#46634,#46635,#46636,#46637,
#46638,#46639,#46640,#46641,#46642,#46643,#46644,#46645,#46646,#46647,#46648,
#46649,#46650,#46651,#46652,#46653,#46654,#46655,#46656,#46657,#46658,#46659,
#46660,#46661,#46662,#46663,#46664,#46665,#46666,#46667,#46668),
 .UNSPECIFIED.,.F.,.F.,(4,2,2,2,2,2,2,2,2,2,2,2,2,2,2,2,2,4),(-5.67439159596968,
-5.64047766140835,-5.58076721688331,-5.52330498546526,-5.4633387313466,
-5.40441833910885,-5.34742402529794,-5.28773207490788,-5.22946075409439,
-5.17183622553644,-5.11197061930769,-5.05436969869878,-4.99499338073396,
-4.9359013779351,-4.878890651626,-4.8192004273671,-4.76075532631967,-4.72839430207058),
 .UNSPECIFIED.);
#2985=B_SPLINE_CURVE_WITH_KNOTS('',3,(#46669,#46670,#46671,#46672,#46673,
#46674,#46675,#46676,#46677,#46678,#46679,#46680,#46681,#46682,#46683,#46684,
#46685,#46686,#46687,#46688,#46689,#46690,#46691,#46692,#46693,#46694,#46695,
#46696,#46697,#46698,#46699,#46700,#46701,#46702,#46703,#46704),
 .UNSPECIFIED.,.F.,.F.,(4,2,2,2,2,2,2,2,2,2,2,2,2,2,2,2,2,4),(-22.6581171675807,
-22.6412102410835,-22.5835641689142,-22.5236319902899,-22.4665652482388,
-22.4082496043878,-22.3487848861067,-22.2919531828174,-22.2329943725634,
-22.1741263229248,-22.1166686457465,-22.0569456248039,-21.9996842855768,
-21.9415589369491,-21.8821072544915,-21.8253417468782,-21.7665709936596,
-21.7157628302399),.UNSPECIFIED.);
#2986=B_SPLINE_CURVE_WITH_KNOTS('',3,(#46709,#46710,#46711,#46712,#46713,
#46714,#46715,#46716,#46717,#46718,#46719,#46720,#46721,#46722,#46723,#46724,
#46725,#46726,#46727,#46728,#46729,#46730,#46731,#46732,#46733,#46734,#46735,
#46736,#46737,#46738,#46739,#46740,#46741,#46742,#46743,#46744),
 .UNSPECIFIED.,.F.,.F.,(4,2,2,2,2,2,2,2,2,2,2,2,2,2,2,2,2,4),(-6.62109380521341,
-6.57761768259959,-6.51828740763027,-6.46113362202641,-6.40140207096381,
-6.34271600715298,-6.28548482095171,-6.22516410228413,-6.16715260360109,
-6.10873547077658,-6.04917186097877,-5.99184011673613,-5.93213648107799,
-5.8733499659965,-5.81628212661826,-5.75656105013342,-5.69842598086126,
-5.67439159596968),.UNSPECIFIED.);
#2987=B_SPLINE_CURVE_WITH_KNOTS('',3,(#46745,#46746,#46747,#46748,#46749,
#46750,#46751,#46752,#46753,#46754,#46755,#46756,#46757,#46758,#46759,#46760,
#46761,#46762,#46763,#46764,#46765,#46766,#46767,#46768,#46769,#46770,#46771,
#46772,#46773,#46774,#46775,#46776,#46777,#46778,#46779,#46780),
 .UNSPECIFIED.,.F.,.F.,(4,2,2,2,2,2,2,2,2,2,2,2,2,2,2,2,2,4),(-21.7157628302399,
-21.7071499734112,-21.6498486291818,-21.5902999589255,-21.5327541629797,
-21.4747842600729,-21.4153173211779,-21.3585227590009,-21.2999052492263,
-21.2398720875173,-21.1826905454483,-21.1232764692568,-21.065378520901,
-21.0075245508875,-20.9480158554619,-20.8911101904613,-20.8326059984683,
-20.7731793950157),.UNSPECIFIED.);
#2988=B_SPLINE_CURVE_WITH_KNOTS('',3,(#46785,#46786,#46787,#46788,#46789,
#46790,#46791,#46792,#46793,#46794,#46795,#46796,#46797,#46798,#46799,#46800,
#46801,#46802,#46803,#46804,#46805,#46806,#46807,#46808,#46809,#46810,#46811,
#46812,#46813,#46814,#46815,#46816,#46817,#46818,#46819,#46820),
 .UNSPECIFIED.,.F.,.F.,(4,2,2,2,2,2,2,2,2,2,2,2,2,2,2,2,2,4),(-7.56721318319246,
-7.51440195941646,-7.4554548070908,-7.39845589958658,-7.33875763160917,
-7.28045937419718,-7.22286133868259,-7.16296628560166,-7.10533842940707,
-7.04602095897405,-6.9868979771895,-6.92987099130527,-6.87017100691209,
-6.81169474396116,-6.75432913502786,-6.69423710481114,-6.63643211656935,
-6.62109380521341),.UNSPECIFIED.);
#2989=B_SPLINE_CURVE_WITH_KNOTS('',3,(#46821,#46822,#46823,#46824,#46825,
#46826,#46827,#46828,#46829,#46830,#46831,#46832,#46833,#46834,#46835,#46836,
#46837,#46838,#46839,#46840,#46841,#46842,#46843,#46844,#46845,#46846,#46847,
#46848,#46849,#46850,#46851,#46852,#46853,#46854,#46855,#46856,#46857,#46858),
 .UNSPECIFIED.,.F.,.F.,(4,2,2,2,2,2,2,2,2,2,2,2,2,2,2,2,2,2,4),(-20.7731793950157,
-20.7731201315055,-20.7160582025871,-20.6567792566783,-20.5983599289237,
-20.5406164839802,-20.4805811221967,-20.4234656784966,-20.3650514109911,
-20.305511597516,-20.2485949896086,-20.1895371334662,-20.1306696919239,
-20.0731189832228,-20.0132974755221,-19.9560008596223,-19.8977815738613,
-19.8382589546996,-19.8295444030046),.UNSPECIFIED.);
#2990=B_SPLINE_CURVE_WITH_KNOTS('',3,(#46863,#46864,#46865,#46866,#46867,
#46868,#46869,#46870,#46871,#46872,#46873,#46874,#46875,#46876,#46877,#46878,
#46879,#46880,#46881,#46882,#46883,#46884,#46885,#46886,#46887,#46888,#46889,
#46890,#46891,#46892,#46893,#46894,#46895,#46896,#46897,#46898,#46899,#46900),
 .UNSPECIFIED.,.F.,.F.,(4,2,2,2,2,2,2,2,2,2,2,2,2,2,2,2,2,2,4),(-8.51391269073544,
-8.51222365838152,-8.45249428513948,-8.39378861667143,-8.33657472393003,
-8.27623231073072,-8.21820164401039,-8.1598332741766,-8.10024765479814,
-8.04289584139225,-7.98318755401621,-7.92437912604881,-7.86731677437594,
-7.80759259896721,-7.74943539170332,-7.6915218402897,-7.631786775557,-7.57430204194946,
-7.56721318319246),.UNSPECIFIED.);
#2991=B_SPLINE_CURVE_WITH_KNOTS('',3,(#46901,#46902,#46903,#46904,#46905,
#46906,#46907,#46908,#46909,#46910,#46911,#46912,#46913,#46914,#46915,#46916,
#46917,#46918,#46919,#46920,#46921,#46922,#46923,#46924,#46925,#46926,#46927,
#46928,#46929,#46930,#46931,#46932,#46933,#46934,#46935,#46936),
 .UNSPECIFIED.,.F.,.F.,(4,2,2,2,2,2,2,2,2,2,2,2,2,2,2,2,2,4),(-19.8295444030046,
-19.781422440649,-19.7225572817117,-19.6631471763022,-19.6057577545878,
-19.5461159927651,-19.4885461013889,-19.4304876297435,-19.3709535721035,
-19.3141007093386,-19.2553941827952,-19.1953773792029,-19.1381132548424,
-19.0786120692882,-19.0206974716804,-18.9627608300149,-18.9031885891784,
-18.8860416189937),.UNSPECIFIED.);
#2992=B_SPLINE_CURVE_WITH_KNOTS('',3,(#46941,#46942,#46943,#46944,#46945,
#46946,#46947,#46948,#46949,#46950,#46951,#46952,#46953,#46954,#46955,#46956,
#46957,#46958,#46959,#46960,#46961,#46962,#46963,#46964,#46965,#46966,#46967,
#46968,#46969,#46970,#46971,#46972,#46973,#46974,#46975,#46976),
 .UNSPECIFIED.,.F.,.F.,(4,2,2,2,2,2,2,2,2,2,2,2,2,2,2,2,2,4),(-9.4600020867739,
-9.44946097484441,-9.38977226427863,-9.3314620836995,-9.27390543364871,
-9.21399634460654,-9.15635642704838,-9.09711384600216,-9.03797514352587,
-8.98094579786149,-8.92125183936447,-8.86275948675276,-8.8054237975235,
-8.7453135764027,-8.68749269541132,-8.62874128051507,-8.56939184171518,
-8.51391269073544),.UNSPECIFIED.);
#2993=B_SPLINE_CURVE_WITH_KNOTS('',3,(#46977,#46978,#46979,#46980,#46981,
#46982,#46983,#46984,#46985,#46986,#46987,#46988,#46989,#46990,#46991,#46992,
#46993,#46994,#46995,#46996,#46997,#46998,#46999,#47000,#47001,#47002,#47003,
#47004,#47005,#47006,#47007,#47008,#47009,#47010,#47011,#47012),
 .UNSPECIFIED.,.F.,.F.,(4,2,2,2,2,2,2,2,2,2,2,2,2,2,2,2,2,4),(-18.8860416189937,
-18.8462348900712,-18.7876476548069,-18.7280968440835,-18.6709555484027,
-18.6115929558287,-18.5531716016611,-18.495349324202,-18.4352301709226,
-18.3780798368063,-18.319585679885,-18.2599881331103,-18.2030028878512,
-18.1438648978918,-18.0850090800984,-18.0273834680497,-17.9674824112817,
-17.941522876477),.UNSPECIFIED.);
#2994=B_SPLINE_CURVE_WITH_KNOTS('',3,(#47017,#47018,#47019,#47020,#47021,
#47022,#47023,#47024,#47025,#47026,#47027,#47028,#47029,#47030,#47031,#47032,
#47033,#47034,#47035,#47036,#47037,#47038,#47039,#47040,#47041,#47042,#47043,
#47044,#47045,#47046,#47047,#47048,#47049,#47050,#47051,#47052),
 .UNSPECIFIED.,.F.,.F.,(4,2,2,2,2,2,2,2,2,2,2,2,2,2,2,2,2,4),(-10.4063262286273,
-10.387392591544,-10.3270439303512,-10.2690090232558,-10.210705562305,-10.1511132343272,
-10.09375612853,-10.034059046947,-9.97524386932148,-9.91820163035005,-9.8584903134111,
-9.80032595747233,-9.74246277833438,-9.68271846928724,-9.62522607647149,
-9.56540900336133,-9.50645028314585,-9.4600020867739),.UNSPECIFIED.);
#2995=B_SPLINE_CURVE_WITH_KNOTS('',3,(#47053,#47054,#47055,#47056,#47057,
#47058,#47059,#47060,#47061,#47062,#47063,#47064,#47065,#47066,#47067,#47068,
#47069,#47070,#47071,#47072,#47073,#47074,#47075,#47076,#47077,#47078,#47079,
#47080,#47081,#47082,#47083,#47084,#47085,#47086,#47087,#47088),
 .UNSPECIFIED.,.F.,.F.,(4,2,2,2,2,2,2,2,2,2,2,2,2,2,2,2,2,4),(-17.941522876477,
-17.9101636562757,-17.8518687182981,-17.7922922877475,-17.7354001068821,
-17.6764590004862,-17.6170707989498,-17.5596109797981,-17.4998945731994,
-17.4423134048219,-17.3841841685699,-17.3245998970605,-17.2677034424408,
-17.2089258668494,-17.1489368038417,-17.0916073172332,-17.0320369692312,
-16.997272415308),.UNSPECIFIED.);
#2996=B_SPLINE_CURVE_WITH_KNOTS('',3,(#47093,#47094,#47095,#47096,#47097,
#47098,#47099,#47100,#47101,#47102,#47103,#47104,#47105,#47106,#47107,#47108,
#47109,#47110,#47111,#47112,#47113,#47114,#47115,#47116,#47117,#47118,#47119,
#47120,#47121,#47122,#47123,#47124,#47125,#47126,#47127,#47128),
 .UNSPECIFIED.,.F.,.F.,(4,2,2,2,2,2,2,2,2,2,2,2,2,2,2,2,2,4),(-11.3522871924595,
-11.324430394275,-11.264522730746,-11.2068857092522,-11.1477360236872,-11.08859687367,
-11.0315792760543,-10.9719076335357,-10.9134142640608,-10.8561239489264,
-10.796010976838,-10.7381891351563,-10.6795177406942,-10.620164420077,-10.5629956093436,
-10.5032845165816,-10.4445743180876,-10.4063262286273),.UNSPECIFIED.);
#2997=B_SPLINE_CURVE_WITH_KNOTS('',3,(#47129,#47130,#47131,#47132,#47133,
#47134,#47135,#47136,#47137,#47138,#47139,#47140,#47141,#47142,#47143,#47144,
#47145,#47146,#47147,#47148,#47149,#47150,#47151,#47152,#47153,#47154,#47155,
#47156,#47157,#47158,#47159,#47160,#47161,#47162,#47163,#47164),
 .UNSPECIFIED.,.F.,.F.,(4,2,2,2,2,2,2,2,2,2,2,2,2,2,2,2,2,4),(-16.997272415308,
-16.974118579872,-16.9161165902415,-16.8564975009602,-16.7995101512218,
-16.7408573501075,-16.6812582779792,-16.6240545216982,-16.5646258893359,
-16.5062147666311,-16.448330624569,-16.388145391231,-16.3309738020301,-16.2724169024022,
-16.2127779950283,-16.155739296564,-16.0965384948368,-16.052121842989),
 .UNSPECIFIED.);
#2998=B_SPLINE_CURVE_WITH_KNOTS('',3,(#47169,#47170,#47171,#47172,#47173,
#47174,#47175,#47176,#47177,#47178,#47179,#47180,#47181,#47182,#47183,#47184,
#47185,#47186,#47187,#47188,#47189,#47190,#47191,#47192,#47193,#47194,#47195,
#47196,#47197,#47198,#47199,#47200,#47201,#47202,#47203,#47204),
 .UNSPECIFIED.,.F.,.F.,(4,2,2,2,2,2,2,2,2,2,2,2,2,2,2,2,2,4),(-12.2980151684053,
-12.2608049534251,-12.2012214180354,-12.1438740189948,-12.0842046319712,
-12.0253980696236,-11.9683912868138,-11.9087094544592,-11.8505531273409,
-11.7927573534416,-11.7330193273245,-11.6755342944868,-11.6158192576419,
-11.5568642629696,-11.4998992163216,-11.4402365277277,-11.3819295252021,
-11.3522871924595),.UNSPECIFIED.);
#2999=B_SPLINE_CURVE_WITH_KNOTS('',3,(#47205,#47206,#47207,#47208,#47209,
#47210,#47211,#47212,#47213,#47214,#47215,#47216,#47217,#47218,#47219,#47220,
#47221,#47222,#47223,#47224,#47225,#47226,#47227,#47228,#47229,#47230,#47231,
#47232,#47233,#47234,#47235,#47236,#47237,#47238,#47239,#47240),
 .UNSPECIFIED.,.F.,.F.,(4,2,2,2,2,2,2,2,2,2,2,2,2,2,2,2,2,4),(-16.052121842989,
-16.0377063442003,-15.9800225041649,-15.9200592855784,-15.8627316418797,
-15.8043778785959,-15.7447638720137,-15.6878306019307,-15.6288305455336,
-15.5694764347843,-15.5119625793001,-15.452188569769,-15.3946092699113,
-15.3364257590099,-15.2768073817686,-15.2198815508401,-15.1610495793805,
-15.1073443691545),.UNSPECIFIED.);
#3000=B_SPLINE_CURVE_WITH_KNOTS('',3,(#47245,#47246,#47247,#47248,#47249,
#47250,#47251,#47252,#47253,#47254,#47255,#47256,#47257,#47258,#47259,#47260,
#47261,#47262,#47263,#47264,#47265,#47266,#47267,#47268,#47269,#47270,#47271,
#47272,#47273,#47274,#47275,#47276,#47277,#47278,#47279,#47280),
 .UNSPECIFIED.,.F.,.F.,(4,2,2,2,2,2,2,2,2,2,2,2,2,2,2,2,2,4),(-13.2436220538442,
-13.1973293402993,-13.1382053560805,-13.0812140676331,-13.0215819437106,
-12.9631029490451,-12.905874761448,-12.8457747640532,-12.787967213325,-12.7293949980337,
-12.670053341907,-12.6128978517491,-12.5532219431716,-12.494522530246,-12.4373888207658,
-12.3770495663262,-12.3190255916381,-12.2980151684053),.UNSPECIFIED.);
#3001=B_SPLINE_CURVE_WITH_KNOTS('',3,(#47281,#47282,#47283,#47284,#47285,
#47286,#47287,#47288,#47289,#47290,#47291,#47292,#47293,#47294,#47295,#47296,
#47297,#47298,#47299,#47300,#47301,#47302,#47303,#47304,#47305,#47306,#47307,
#47308,#47309,#47310,#47311,#47312,#47313,#47314,#47315,#47316,#47317,#47318),
 .UNSPECIFIED.,.F.,.F.,(4,2,2,2,2,2,2,2,2,2,2,2,2,2,2,2,2,2,4),(-15.1073443691545,
-15.1011008892937,-15.0437220848592,-14.9840992717133,-14.926190394778,
-14.8681392181562,-14.8084892686686,-14.7514823595925,-14.6927803091387,
-14.6331489331619,-14.5758985339276,-14.5164203125443,-14.4580324516964,
-14.4001023522461,-14.339867608388,-14.2826884114687,-14.2240848432797,
-14.1644203791933,-14.161791521072),.UNSPECIFIED.);
#3002=B_SPLINE_CURVE_WITH_KNOTS('',3,(#47323,#47324,#47325,#47326,#47327,
#47328,#47329,#47330,#47331,#47332,#47333,#47334,#47335,#47336,#47337,#47338,
#47339,#47340,#47341,#47342,#47343,#47344,#47345,#47346,#47347,#47348,#47349,
#47350,#47351,#47352,#47353,#47354,#47355,#47356,#47357,#47358),
 .UNSPECIFIED.,.F.,.F.,(4,2,2,2,2,2,2,2,2,2,2,2,2,2,2,2,2,4),(-14.1885859699234,
-14.1330844909293,-14.0738030834317,-14.0151322001193,-13.9573780431577,
-13.8973369154889,-13.8400747014035,-13.781649842778,-13.7220284098382,
-13.6650669338426,-13.6061313895152,-13.5492060305576,-13.4895868440872,
-13.4312985326842,-13.3738747554208,-13.3139843572995,-13.2563655957482,
-13.2436220538442),.UNSPECIFIED.);
#3003=B_SPLINE_CURVE_WITH_KNOTS('',3,(#47359,#47360,#47361,#47362,#47363,
#47364,#47365,#47366,#47367,#47368,#47369,#47370,#47371,#47372,#47373,#47374,
#47375,#47376,#47377,#47378,#47379,#47380,#47381,#47382,#47383,#47384,#47385,
#47386,#47387,#47388,#47389,#47390,#47391,#47392,#47393,#47394),
 .UNSPECIFIED.,.F.,.F.,(4,2,2,2,2,2,2,2,2,2,2,2,2,2,2,2,2,4),(-14.161791521072,
-14.1073426685626,-14.0480953063394,-13.9892999039839,-13.9315735440484,
-13.8715645099561,-13.8142414960538,-13.7558447627025,-13.6962089327002,
-13.6392486779599,-13.5802573437773,-13.5233108369954,-13.4636758610349,
-13.4053314288153,-13.3479464458854,-13.2879951425265,-13.2303206406094,
-13.2166062380566),.UNSPECIFIED.);
#3004=B_SPLINE_CURVE_WITH_KNOTS('',3,(#47399,#47400,#47401,#47402,#47403,
#47404,#47405,#47406,#47407,#47408,#47409,#47410,#47411,#47412,#47413,#47414,
#47415,#47416,#47417,#47418,#47419,#47420,#47421,#47422,#47423,#47424,#47425,
#47426,#47427,#47428,#47429,#47430,#47431,#47432,#47433,#47434,#47435,#47436),
 .UNSPECIFIED.,.F.,.F.,(4,2,2,2,2,2,2,2,2,2,2,2,2,2,2,2,2,2,4),(-15.1341561055544,
-15.1269994338561,-15.0695799723091,-15.0099125340775,-14.9520739190766,
-14.8939828445778,-14.8343297519005,-14.7773366004228,-14.7185951213641,
-14.6589576423824,-14.6016713251844,-14.5421535644632,-14.4838629359255,
-14.4258987192761,-14.3656251166082,-14.3084824988271,-14.2498440170218,
-14.1901865832963,-14.1885859699234),.UNSPECIFIED.);
#3005=B_SPLINE_CURVE_WITH_KNOTS('',3,(#47437,#47438,#47439,#47440,#47441,
#47442,#47443,#47444,#47445,#47446,#47447,#47448,#47449,#47450,#47451,#47452,
#47453,#47454,#47455,#47456,#47457,#47458,#47459,#47460,#47461,#47462,#47463,
#47464,#47465,#47466,#47467,#47468,#47469,#47470,#47471,#47472),
 .UNSPECIFIED.,.F.,.F.,(4,2,2,2,2,2,2,2,2,2,2,2,2,2,2,2,2,4),(-13.2166062380566,
-13.1713851979337,-13.1121981319385,-13.0551628296182,-12.9955080421381,
-12.9369655576865,-12.8797535453401,-12.819585289645,-12.761715189623,-12.7032194250943,
-12.6438086463492,-12.586620577358,-12.5270150261763,-12.4683803900242,
-12.4113696886299,-12.35174219741,-12.2937588655423,-12.2712695292436),
 .UNSPECIFIED.);
#3006=B_SPLINE_CURVE_WITH_KNOTS('',3,(#47477,#47478,#47479,#47480,#47481,
#47482,#47483,#47484,#47485,#47486,#47487,#47488,#47489,#47490,#47491,#47492,
#47493,#47494,#47495,#47496,#47497,#47498,#47499,#47500,#47501,#47502,#47503,
#47504,#47505,#47506,#47507,#47508,#47509,#47510,#47511,#47512),
 .UNSPECIFIED.,.F.,.F.,(4,2,2,2,2,2,2,2,2,2,2,2,2,2,2,2,2,4),(-16.0791645683298,
-16.0637629880179,-16.0060223350212,-15.9459969234656,-15.8887024341941,
-15.8302912537239,-15.7706612508563,-15.7136999051047,-15.654642811055,
-15.5954057874932,-15.5378426704977,-15.4780146687669,-15.4204898319656,
-15.3622571133794,-15.3026293793744,-15.2456979578477,-15.1868171504776,
-15.1341561055544),.UNSPECIFIED.);
#3007=B_SPLINE_CURVE_WITH_KNOTS('',3,(#47513,#47514,#47515,#47516,#47517,
#47518,#47519,#47520,#47521,#47522,#47523,#47524,#47525,#47526,#47527,#47528,
#47529,#47530,#47531,#47532,#47533,#47534,#47535,#47536,#47537,#47538,#47539,
#47540,#47541,#47542,#47543,#47544,#47545,#47546,#47547,#47548),
 .UNSPECIFIED.,.F.,.F.,(4,2,2,2,2,2,2,2,2,2,2,2,2,2,2,2,2,4),(-12.2712695292436,
-12.2357754508004,-12.1762270533728,-12.1189170680661,-12.0588176303639,
-12.0000655464483,-11.943159299172,-11.8835712422689,-11.8254678956475,
-11.7678321870858,-11.708145031833,-11.6507114242844,-11.5912213696332,
-11.5323122460786,-11.4754266605439,-11.4158513420701,-11.3575887654668,
-11.3269908932583),.UNSPECIFIED.);
#3008=B_SPLINE_CURVE_WITH_KNOTS('',3,(#47553,#47554,#47555,#47556,#47557,
#47558,#47559,#47560,#47561,#47562,#47563,#47564,#47565,#47566,#47567,#47568,
#47569,#47570,#47571,#47572,#47573,#47574,#47575,#47576,#47577,#47578,#47579,
#47580,#47581,#47582,#47583,#47584,#47585,#47586,#47587,#47588),
 .UNSPECIFIED.,.F.,.F.,(4,2,2,2,2,2,2,2,2,2,2,2,2,2,2,2,2,4),(-17.0247741151702,
-17.0006922494049,-16.942620899042,-16.8829683888398,-16.8259674619989,
-16.7672454552544,-16.7076101234707,-16.6503415003102,-16.590843286514,
-16.5325014804607,-16.4745540351945,-16.4142996421448,-16.357137434069,
-16.2985161360182,-16.2388539992256,-16.1817640975146,-16.1224994016558,
-16.0791645683298),.UNSPECIFIED.);
#3009=B_SPLINE_CURVE_WITH_KNOTS('',3,(#47589,#47590,#47591,#47592,#47593,
#47594,#47595,#47596,#47597,#47598,#47599,#47600,#47601,#47602,#47603,#47604,
#47605,#47606,#47607,#47608,#47609,#47610,#47611,#47612,#47613,#47614,#47615,
#47616,#47617,#47618,#47619,#47620,#47621,#47622,#47623,#47624),
 .UNSPECIFIED.,.F.,.F.,(4,2,2,2,2,2,2,2,2,2,2,2,2,2,2,2,2,4),(-11.3269908932583,
-11.3002304831747,-11.2403651502537,-11.1827717007332,-11.1238285355636,
-11.064728011521,-11.0077668972893,-10.9481757635054,-10.8897195155163,
-10.8325471683827,-10.7724692707686,-10.7146842840278,-10.6561946025542,
-10.5968740051404,-10.5397395269343,-10.4801014814801,-10.4214223488875,
-10.3822526002173),.UNSPECIFIED.);
#3010=B_SPLINE_CURVE_WITH_KNOTS('',3,(#47629,#47630,#47631,#47632,#47633,
#47634,#47635,#47636,#47637,#47638,#47639,#47640,#47641,#47642,#47643,#47644,
#47645,#47646,#47647,#47648,#47649,#47650,#47651,#47652,#47653,#47654,#47655,
#47656,#47657,#47658,#47659,#47660,#47661,#47662,#47663,#47664),
 .UNSPECIFIED.,.F.,.F.,(4,2,2,2,2,2,2,2,2,2,2,2,2,2,2,2,2,4),(-17.9696970255303,
-17.937289370862,-17.8789069021961,-17.8192841522869,-17.7623368372575,
-17.7033082433986,-17.6440100001385,-17.5864714106887,-17.526670356869,
-17.4691167328281,-17.4109085209012,-17.3512845924667,-17.2943555190345,
-17.2354990142404,-17.1756126480208,-17.1182132969445,-17.0585679978772,
-17.0247741151702),.UNSPECIFIED.);
#3011=B_SPLINE_CURVE_WITH_KNOTS('',3,(#47665,#47666,#47667,#47668,#47669,
#47670,#47671,#47672,#47673,#47674,#47675,#47676,#47677,#47678,#47679,#47680,
#47681,#47682,#47683,#47684,#47685,#47686,#47687,#47688,#47689,#47690,#47691,
#47692,#47693,#47694,#47695,#47696,#47697,#47698,#47699,#47700),
 .UNSPECIFIED.,.F.,.F.,(4,2,2,2,2,2,2,2,2,2,2,2,2,2,2,2,2,4),(-10.3822526002173,
-10.3643343540307,-10.3046400968479,-10.246613334744,-10.1885181147052,
-10.128927402479,-10.0715754084394,-10.011325400927,-9.9525347708931,-9.89556195447909,
-9.83591091083034,-9.77776999750488,-9.72003077893023,-9.66030722303232,
-9.60283704872725,-9.54320316116386,-9.48426076178981,-9.43689892858011),
 .UNSPECIFIED.);
#3012=B_SPLINE_CURVE_WITH_KNOTS('',3,(#47705,#47706,#47707,#47708,#47709,
#47710,#47711,#47712,#47713,#47714,#47715,#47716,#47717,#47718,#47719,#47720,
#47721,#47722,#47723,#47724,#47725,#47726,#47727,#47728,#47729,#47730,#47731,
#47732,#47733,#47734,#47735,#47736,#47737,#47738,#47739,#47740),
 .UNSPECIFIED.,.F.,.F.,(4,2,2,2,2,2,2,2,2,2,2,2,2,2,2,2,2,4),(-18.9151145034862,
-18.8743164654268,-18.8156291548377,-18.7560115648048,-18.6987754493173,
-18.6393121439161,-18.5809341256596,-18.5230183981635,-18.4627987144582,
-18.4056311968295,-18.3470421802252,-18.2873910545073,-18.2303271150055,
-18.171094421965,-18.1123080260466,-18.0545957689432,-17.9946015046478,
-17.9696970255303),.UNSPECIFIED.);
#3013=B_SPLINE_CURVE_WITH_KNOTS('',3,(#47741,#47742,#47743,#47744,#47745,
#47746,#47747,#47748,#47749,#47750,#47751,#47752,#47753,#47754,#47755,#47756,
#47757,#47758,#47759,#47760,#47761,#47762,#47763,#47764,#47765,#47766,#47767,
#47768,#47769,#47770,#47771,#47772,#47773,#47774,#47775,#47776),
 .UNSPECIFIED.,.F.,.F.,(4,2,2,2,2,2,2,2,2,2,2,2,2,2,2,2,2,4),(-9.43689892858011,
-9.42732171849391,-9.36768738295302,-9.30939248028644,-9.25194272911408,
-9.19204622378449,-9.13442101602013,-9.07534568068709,-9.01621630273034,
-8.95921594082851,-8.89957004368503,-8.84108593111714,-8.78383634874988,
-8.72373170856049,-8.6659190669351,-8.60731272480359,-8.54796686813959,
-8.49156038630827),.UNSPECIFIED.);
#3014=B_SPLINE_CURVE_WITH_KNOTS('',3,(#47781,#47782,#47783,#47784,#47785,
#47786,#47787,#47788,#47789,#47790,#47791,#47792,#47793,#47794,#47795,#47796,
#47797,#47798,#47799,#47800,#47801,#47802,#47803,#47804,#47805,#47806,#47807,
#47808,#47809,#47810,#47811,#47812,#47813,#47814,#47815,#47816),
 .UNSPECIFIED.,.F.,.F.,(4,2,2,2,2,2,2,2,2,2,2,2,2,2,2,2,2,4),(-19.8597382210236,
-19.810451373043,-19.7514667566491,-19.6921219719675,-19.6346229403372,
-19.5748644342208,-19.5172962645061,-19.4591277252691,-19.3995232496075,
-19.3426105099162,-19.2837936446735,-19.2238539608265,-19.1664896413472,
-19.1068819617647,-19.0489837573588,-18.9909471893313,-18.9313109305834,
-18.9151145034862),.UNSPECIFIED.);
#3015=B_SPLINE_CURVE_WITH_KNOTS('',3,(#47817,#47818,#47819,#47820,#47821,
#47822,#47823,#47824,#47825,#47826,#47827,#47828,#47829,#47830,#47831,#47832,
#47833,#47834,#47835,#47836,#47837,#47838,#47839,#47840,#47841,#47842,#47843,
#47844,#47845,#47846,#47847,#47848,#47849,#47850,#47851,#47852,#47853,#47854),
 .UNSPECIFIED.,.F.,.F.,(4,2,2,2,2,2,2,2,2,2,2,2,2,2,2,2,2,2,4),(-8.49156038630827,
-8.49080675575303,-8.43111857134256,-8.37241526446117,-8.31526501763932,
-8.25492233706489,-8.19689441801019,-8.13864530142174,-8.07905854481672,
-8.02170761683104,-7.96202852596394,-7.9032187975688,-7.84619976450985,
-7.78650760972943,-7.72834831916545,-7.67052935317836,-7.61078895216033,
-7.55330118212272,-7.54539583975842),.UNSPECIFIED.);
#3016=B_SPLINE_CURVE_WITH_KNOTS('',3,(#47859,#47860,#47861,#47862,#47863,
#47864,#47865,#47866,#47867,#47868,#47869,#47870,#47871,#47872,#47873,#47874,
#47875,#47876,#47877,#47878,#47879,#47880,#47881,#47882,#47883,#47884,#47885,
#47886,#47887,#47888,#47889,#47890,#47891,#47892,#47893,#47894,#47895,#47896),
 .UNSPECIFIED.,.F.,.F.,(4,2,2,2,2,2,2,2,2,2,2,2,2,2,2,2,2,2,4),(-20.8047268284554,
-20.8036363389145,-20.7464479008663,-20.6870352594353,-20.6286348915891,
-20.5707661629285,-20.510597073108,-20.4534380889162,-20.3948967931479,
-20.3352722771837,-20.2782483009287,-20.219063232801,-20.1602410153004,
-20.1025723093681,-20.0426249323872,-19.9853090960203,-19.9269706384341,
-19.867370764855,-19.8597382210236),.UNSPECIFIED.);
#3017=B_SPLINE_CURVE_WITH_KNOTS('',3,(#47897,#47898,#47899,#47900,#47901,
#47902,#47903,#47904,#47905,#47906,#47907,#47908,#47909,#47910,#47911,#47912,
#47913,#47914,#47915,#47916,#47917,#47918,#47919,#47920,#47921,#47922,#47923,
#47924,#47925,#47926,#47927,#47928,#47929,#47930,#47931,#47932),
 .UNSPECIFIED.,.F.,.F.,(4,2,2,2,2,2,2,2,2,2,2,2,2,2,2,2,2,4),(-7.54539583975842,
-7.49355110204946,-7.43459460077228,-7.37762115395009,-7.31794932817515,
-7.25964100917192,-7.20212210603924,-7.14221371611197,-7.08457547245393,
-7.02539392871746,-6.96625468515904,-6.90923296876007,-6.84955345859718,
-6.79106019408235,-6.73375428080265,-6.6736419972573,-6.61582024058893,
-6.59962043014718),.UNSPECIFIED.);
#3018=B_SPLINE_CURVE_WITH_KNOTS('',3,(#47937,#47938,#47939,#47940,#47941,
#47942,#47943,#47944,#47945,#47946,#47947,#47948,#47949,#47950,#47951,#47952,
#47953,#47954,#47955,#47956,#47957,#47958,#47959,#47960,#47961,#47962,#47963,
#47964,#47965,#47966,#47967,#47968,#47969,#47970,#47971,#47972),
 .UNSPECIFIED.,.F.,.F.,(4,2,2,2,2,2,2,2,2,2,2,2,2,2,2,2,2,4),(-21.7489046572791,
-21.7392153866495,-21.6817714549229,-21.6220716583751,-21.5645025223573,
-21.5063893301253,-21.4468200256293,-21.3899376073178,-21.3311762213552,
-21.2711970668162,-21.2138831121422,-21.1543289862749,-21.0964221879644,
-21.0384358621701,-20.9788315240901,-20.9218575630073,-20.8632205676017,
-20.8047268284554),.UNSPECIFIED.);
#3019=B_SPLINE_CURVE_WITH_KNOTS('',3,(#47973,#47974,#47975,#47976,#47977,
#47978,#47979,#47980,#47981,#47982,#47983,#47984,#47985,#47986,#47987,#47988,
#47989,#47990,#47991,#47992,#47993,#47994,#47995,#47996,#47997,#47998,#47999,
#48000,#48001,#48002,#48003,#48004,#48005,#48006,#48007,#48008),
 .UNSPECIFIED.,.F.,.F.,(4,2,2,2,2,2,2,2,2,2,2,2,2,2,2,2,2,4),(-6.59962043014718,
-6.55712143056447,-6.49776917806976,-6.44060046014423,-6.3808828825634,
-6.32217397813377,-6.26498116754636,-6.20463437850135,-6.14660066752985,
-6.0882749718812,-6.02868466855325,-5.9713291133043,-5.91162795849117,-5.85281481524407,
-5.79576557777481,-5.73604961995392,-5.67788743624381,-5.65305968192749),
 .UNSPECIFIED.);
#3020=B_SPLINE_CURVE_WITH_KNOTS('',3,(#48013,#48014,#48015,#48016,#48017,
#48018,#48019,#48020,#48021,#48022,#48023,#48024,#48025,#48026,#48027,#48028,
#48029,#48030,#48031,#48032,#48033,#48034,#48035,#48036,#48037,#48038,#48039,
#48040,#48041,#48042,#48043,#48044,#48045,#48046,#48047,#48048),
 .UNSPECIFIED.,.F.,.F.,(4,2,2,2,2,2,2,2,2,2,2,2,2,2,2,2,2,4),(-22.6930944862137,
-22.6750742815793,-22.6172685137948,-22.5571666469156,-22.5000298336195,
-22.4415523883347,-22.3819703093803,-22.3250007752965,-22.2658796385637,
-22.2070346049225,-22.1494252073759,-22.0895411174023,-22.0322350703383,
-21.9739565284333,-21.9143953015877,-21.8575179583935,-21.7985933937003,
-21.7489046572791),.UNSPECIFIED.);
#3021=B_SPLINE_CURVE_WITH_KNOTS('',3,(#48049,#48050,#48051,#48052,#48053,
#48054,#48055,#48056,#48057,#48058,#48059,#48060,#48061,#48062,#48063,#48064,
#48065,#48066,#48067,#48068,#48069,#48070,#48071,#48072,#48073,#48074,#48075,
#48076,#48077,#48078,#48079,#48080,#48081,#48082,#48083,#48084),
 .UNSPECIFIED.,.F.,.F.,(4,2,2,2,2,2,2,2,2,2,2,2,2,2,2,2,2,4),(-5.65305968192749,
-5.62000697109407,-5.56026553634326,-5.50277548740805,-5.4429300395589,
-5.38397497750277,-5.32698226097639,-5.2672900308627,-5.20898363219345,
-5.15141280935565,-5.09150820934248,-5.03387211917237,-4.97460397585247,
-4.91547032791341,-4.8584416373336,-4.79874535977046,-4.74025819094778,
-4.7070192889843),.UNSPECIFIED.);
#3022=B_SPLINE_CURVE_WITH_KNOTS('',3,(#48089,#48090,#48091,#48092,#48093,
#48094,#48095,#48096,#48097,#48098,#48099,#48100,#48101,#48102,#48103,#48104,
#48105,#48106,#48107,#48108,#48109,#48110,#48111,#48112,#48113,#48114,#48115,
#48116,#48117,#48118,#48119,#48120,#48121,#48122,#48123,#48124),
 .UNSPECIFIED.,.F.,.F.,(4,2,2,2,2,2,2,2,2,2,2,2,2,2,2,2,2,4),(-23.6367224740298,
-23.6102009889967,-23.5521597036553,-23.4926417159663,-23.435803856614,
-23.3771146729451,-23.3171085926091,-23.2598611088234,-23.2003772998387,
-23.1424751745089,-23.0845553127723,-23.0249989156642,-22.9680595588619,
-22.9094892557851,-22.8499543793008,-22.7928294928815,-22.7334840265615,
-22.6930944862137),.UNSPECIFIED.);
#3023=B_SPLINE_CURVE_WITH_KNOTS('',3,(#48125,#48126,#48127,#48128,#48129,
#48130,#48131,#48132,#48133,#48134,#48135,#48136,#48137,#48138,#48139,#48140,
#48141,#48142,#48143,#48144,#48145,#48146,#48147,#48148,#48149,#48150,#48151,
#48152,#48153,#48154,#48155,#48156,#48157,#48158,#48159,#48160),
 .UNSPECIFIED.,.F.,.F.,(4,2,2,2,2,2,2,2,2,2,2,2,2,2,2,2,2,4),(-4.7070192889843,
-4.68291221701188,-4.62280788263384,-4.56499211835275,-4.50621920975702,
-4.44687598188547,-4.3897125228076,-4.32998213906469,-4.27128283566224,
-4.21406294394457,-4.15372759490239,-4.09570314650131,-4.03731813708901,
-3.97773968458231,-3.92039439080922,-3.86068740451247,-3.80188610698126,
-3.76030733114506),.UNSPECIFIED.);
#3024=B_SPLINE_CURVE_WITH_KNOTS('',3,(#48165,#48166,#48167,#48168,#48169,
#48170,#48171,#48172,#48173,#48174,#48175,#48176,#48177,#48178,#48179,#48180,
#48181,#48182,#48183,#48184,#48185,#48186,#48187,#48188,#48189,#48190,#48191,
#48192,#48193,#48194,#48195,#48196,#48197,#48198,#48199,#48200),
 .UNSPECIFIED.,.F.,.F.,(4,2,2,2,2,2,2,2,2,2,2,2,2,2,2,2,2,4),(-24.5799045977848,
-24.544864402261,-24.4864680402579,-24.4269448204466,-24.3700449713328,
-24.3110051741305,-24.2521492970098,-24.1946159613695,-24.1348126294181,
-24.0775296073419,-24.0193278864891,-23.9598215850082,-23.9030009070175,
-23.8441534701742,-23.7847543450619,-23.7273819445697,-23.667757974583,
-23.6367224740298),.UNSPECIFIED.);
#3025=B_SPLINE_CURVE_WITH_KNOTS('',3,(#48201,#48202,#48203,#48204,#48205,
#48206,#48207,#48208,#48209,#48210,#48211,#48212,#48213,#48214,#48215,#48216,
#48217,#48218,#48219,#48220,#48221,#48222,#48223,#48224,#48225,#48226,#48227,
#48228,#48229,#48230,#48231,#48232,#48233,#48234,#48235,#48236),
 .UNSPECIFIED.,.F.,.F.,(4,2,2,2,2,2,2,2,2,2,2,2,2,2,2,2,2,4),(-3.76030733114506,
-3.74482173076156,-3.6850983260828,-3.62694832744347,-3.56902286769636,
-3.50929583899485,-3.45181843527126,-3.39189585023894,-3.33295745069471,
-3.27595993809932,-3.21626352613547,-3.15797408399984,-3.1003669659872,
-3.04048156422391,-2.98286252158158,-2.92352507208656,-2.86441225193454,
-2.81422223630842),.UNSPECIFIED.);
#3026=B_SPLINE_CURVE_WITH_KNOTS('',3,(#48241,#48242,#48243,#48244,#48245,
#48246,#48247,#48248,#48249,#48250,#48251,#48252,#48253,#48254,#48255,#48256,
#48257,#48258,#48259,#48260,#48261,#48262,#48263,#48264,#48265,#48266,#48267,
#48268,#48269,#48270,#48271,#48272,#48273,#48274,#48275,#48276),
 .UNSPECIFIED.,.F.,.F.,(4,2,2,2,2,2,2,2,2,2,2,2,2,2,2,2,2,4),(-25.5227587485597,
-25.47965708315,-25.421058174348,-25.361036462416,-25.3038727637219,-25.2444773184052,
-25.1865926949701,-25.128756714116,-25.0692650147963,-25.0123746718861,
-24.9538886316087,-24.8944198504469,-24.8373755091807,-24.7781149174187,
-24.7197080007783,-24.6619822469935,-24.6019654058989,-24.5799045977848),
 .UNSPECIFIED.);
#3027=B_SPLINE_CURVE_WITH_KNOTS('',3,(#48277,#48278,#48279,#48280,#48281,
#48282,#48283,#48284,#48285,#48286,#48287,#48288,#48289,#48290,#48291,#48292,
#48293,#48294,#48295,#48296,#48297,#48298,#48299,#48300,#48301,#48302,#48303,
#48304,#48305,#48306,#48307,#48308,#48309,#48310,#48311,#48312,#48313,#48314),
 .UNSPECIFIED.,.F.,.F.,(4,2,2,2,2,2,2,2,2,2,2,2,2,2,2,2,2,2,4),(-2.81422223630842,
-2.80739059809379,-2.74769363128926,-2.68922759545975,-2.63185666495599,
-2.57177569602702,-2.51398082031509,-2.45515020591261,-2.39583126811454,
-2.3386868262193,-2.27895955966271,-2.22028492138649,-2.16305256653281,
-2.1027441052407,-2.04474383487291,-1.98631516239258,-1.92676386570169,
-1.86944360522889,-1.86759610747369),.UNSPECIFIED.);
#3028=B_SPLINE_CURVE_WITH_KNOTS('',3,(#48319,#48320,#48321,#48322,#48323,
#48324,#48325,#48326,#48327,#48328,#48329,#48330,#48331,#48332,#48333,#48334,
#48335,#48336,#48337,#48338,#48339,#48340,#48341,#48342,#48343,#48344,#48345,
#48346,#48347,#48348,#48349,#48350,#48351,#48352,#48353,#48354),
 .UNSPECIFIED.,.F.,.F.,(4,2,2,2,2,2,2,2,2,2,2,2,2,2,2,2,2,4),(-26.4647006629411,
-26.4128164821547,-26.3538770628634,-26.295021282913,-26.2375822529352,
-26.1778787398139,-26.1206318744523,-26.0625253754812,-26.0030911980923,
-25.9463425849355,-25.8875908503495,-25.8281815100278,-25.7708984260118,
-25.7113688412011,-25.6538368035759,-25.595885334023,-25.5364356344578,
-25.5227587485597),.UNSPECIFIED.);
#3029=B_SPLINE_CURVE_WITH_KNOTS('',3,(#48355,#48356,#48357,#48358,#48359,
#48360,#48361,#48362,#48363,#48364,#48365,#48366,#48367,#48368,#48369,#48370,
#48371,#48372,#48373,#48374,#48375,#48376,#48377,#48378,#48379,#48380,#48381,
#48382,#48383,#48384,#48385,#48386,#48387,#48388,#48389,#48390),
 .UNSPECIFIED.,.F.,.F.,(4,2,2,2,2,2,2,2,2,2,2,2,2,2,2,2,2,4),(-1.86759610747369,
-1.8097465170722,-1.7509722323765,-1.69390716991027,-1.63419213717573,-1.57606932036452,
-1.51811407870063,-1.45841685307261,-1.40096694869804,-1.34098343757821,
-1.28207692999559,-1.22508871615811,-1.16540388332849,-1.10714645181714,
-1.0495176707267,-0.989666932708261,-0.932079853846146,-0.921606618540025),
 .UNSPECIFIED.);
#3030=B_SPLINE_CURVE_WITH_KNOTS('',3,(#48396,#48397,#48398,#48399,#48400,
#48401,#48402,#48403,#48404,#48405,#48406,#48407,#48408,#48409,#48410,#48411,
#48412,#48413,#48414,#48415),.UNSPECIFIED.,.F.,.F.,(4,2,2,2,2,2,2,2,2,4),
(9.99987117032003E-7,0.0282047267175922,0.0500972781633209,0.077222937740314,
0.107624298477487,0.137340418712146,0.157932276880896,0.175135732483776,
0.191462844907497,0.203440126186273),.UNSPECIFIED.);
#3031=B_SPLINE_CURVE_WITH_KNOTS('',3,(#48421,#48422,#48423,#48424,#48425,
#48426,#48427,#48428),.UNSPECIFIED.,.F.,.F.,(4,2,2,4),(21.4315064013737,
21.4634357935859,21.4930318613417,21.5226265917604),.UNSPECIFIED.);
#3032=B_SPLINE_CURVE_WITH_KNOTS('',3,(#48434,#48435,#48436,#48437,#48438,
#48439,#48440,#48441,#48442,#48443,#48444,#48445,#48446,#48447,#48448,#48449,
#48450,#48451,#48452,#48453,#48454,#48455,#48456,#48457,#48458,#48459,#48460,
#48461,#48462,#48463,#48464,#48465,#48466,#48467,#48468,#48469),
 .UNSPECIFIED.,.F.,.F.,(4,2,2,2,2,2,2,2,2,2,2,2,2,2,2,2,2,4),(20.6936878716818,
20.7322285263897,20.7783057175789,20.8227795047066,20.8693557730982,20.9149428892879,
20.9597524851927,21.0065846852777,21.0516438851204,21.0976519395239,21.1438788790039,
21.188432473727,21.2350392941589,21.2807854576605,21.3254925240272,21.3724982892632,
21.417717724476,21.4315064013737),.UNSPECIFIED.);
#3033=B_SPLINE_CURVE_WITH_KNOTS('',3,(#48470,#48471,#48472,#48473,#48474,
#48475,#48476,#48477,#48478,#48479,#48480,#48481,#48482,#48483,#48484,#48485,
#48486,#48487,#48488,#48489,#48490,#48491,#48492,#48493,#48494,#48495,#48496,
#48497,#48498,#48499,#48500,#48501,#48502,#48503,#48504,#48505),
 .UNSPECIFIED.,.F.,.F.,(4,2,2,2,2,2,2,2,2,2,2,2,2,2,2,2,2,4),(9.99999999753597E-7,
0.0364903991492045,0.0742057367939146,0.120984278340417,0.165716260437277,
0.212135354668823,0.258243398942271,0.303486376579508,0.350510827449709,
0.395451299070227,0.441223703670797,0.487964967533294,0.532602258835938,
0.578864855147042,0.625329100321987,0.670440021753448,0.717320863549735,
0.740262878339932),.UNSPECIFIED.);
#3034=B_SPLINE_CURVE_WITH_KNOTS('',3,(#48510,#48511,#48512,#48513,#48514,
#48515,#48516,#48517,#48518,#48519,#48520,#48521,#48522,#48523,#48524,#48525,
#48526,#48527,#48528,#48529,#48530,#48531,#48532,#48533,#48534,#48535,#48536,
#48537,#48538,#48539,#48540,#48541,#48542,#48543,#48544,#48545),
 .UNSPECIFIED.,.F.,.F.,(4,2,2,2,2,2,2,2,2,2,2,2,2,2,2,2,2,4),(19.9559680414516,
20.0008504784901,20.0467368410681,20.0912761832143,20.1378918451635,20.1832739295335,
20.2285046006904,20.275104513086,20.3199511087905,20.366754624975,20.4127173643503,
20.4571887454312,20.5037686894442,20.5492336658488,20.5942218762843,20.6409180608554,
20.6858523218674,20.6936878716818),.UNSPECIFIED.);
#3035=B_SPLINE_CURVE_WITH_KNOTS('',3,(#48546,#48547,#48548,#48549,#48550,
#48551,#48552,#48553,#48554,#48555,#48556,#48557,#48558,#48559,#48560,#48561,
#48562,#48563,#48564,#48565,#48566,#48567,#48568,#48569,#48570,#48571,#48572,
#48573,#48574,#48575,#48576,#48577,#48578,#48579,#48580,#48581),
 .UNSPECIFIED.,.F.,.F.,(4,2,2,2,2,2,2,2,2,2,2,2,2,2,2,2,2,4),(0.740262878339932,
0.762427102215096,0.808069985401053,0.854808846272841,0.899429812570394,
0.945570872042072,0.992454683227221,1.03747065146669,1.08424743869661,1.12958660656193,
1.175138889682,1.22190780149668,1.26658471043468,1.31264188421903,1.35939848501362,
1.4043392205548,1.45103260193205,1.48067239646651),.UNSPECIFIED.);
#3036=B_SPLINE_CURVE_WITH_KNOTS('',3,(#48586,#48587,#48588,#48589,#48590,
#48591,#48592,#48593,#48594,#48595,#48596,#48597,#48598,#48599,#48600,#48601,
#48602,#48603,#48604,#48605,#48606,#48607,#48608,#48609,#48610,#48611,#48612,
#48613,#48614,#48615,#48616,#48617,#48618,#48619,#48620,#48621,#48622,#48623),
 .UNSPECIFIED.,.F.,.F.,(4,2,2,2,2,2,2,2,2,2,2,2,2,2,2,2,2,2,4),(19.2175408288878,
19.2219373965907,19.2685210725085,19.3141891378125,19.3589248216993,19.4058460198647,
19.4509870738391,19.4968133764095,19.5431350504829,19.5877640910998,19.6343990565288,
19.6802461513431,19.72492597093,19.7720411959568,19.8173618084826,19.8629496498953,
19.9094715861334,19.954248068259,19.9559680414516),.UNSPECIFIED.);
#3037=B_SPLINE_CURVE_WITH_KNOTS('',3,(#48624,#48625,#48626,#48627,#48628,
#48629,#48630,#48631,#48632,#48633,#48634,#48635,#48636,#48637,#48638,#48639,
#48640,#48641,#48642,#48643,#48644,#48645,#48646,#48647,#48648,#48649,#48650,
#48651,#48652,#48653,#48654,#48655,#48656,#48657,#48658,#48659),
 .UNSPECIFIED.,.F.,.F.,(4,2,2,2,2,2,2,2,2,2,2,2,2,2,2,2,2,4),(1.48067239646651,
1.49671326012625,1.54219831558785,1.5894859449329,1.63428944893413,1.68030245144421,
1.72708174969527,1.77186789842175,1.81835464146615,1.86425678940839,1.90955548631379,
1.95664189809396,2.00148568453804,2.0473126858144,2.0940334671172,2.13867975719358,
2.18499121801513,2.22108960850334),.UNSPECIFIED.);
#3038=B_SPLINE_CURVE_WITH_KNOTS('',3,(#48664,#48665,#48666,#48667,#48668,
#48669,#48670,#48671,#48672,#48673,#48674,#48675,#48676,#48677,#48678,#48679,
#48680,#48681,#48682,#48683,#48684,#48685,#48686,#48687,#48688,#48689,#48690,
#48691,#48692,#48693,#48694,#48695,#48696,#48697,#48698,#48699),
 .UNSPECIFIED.,.F.,.F.,(4,2,2,2,2,2,2,2,2,2,2,2,2,2,2,2,2,4),(18.4801374015765,
18.4907658335562,18.5373515680576,18.5827705444335,18.6278503823358,18.6744946234866,
18.7193811539994,18.7659288026933,18.8119468369207,18.8564049550709,18.9029730508313,
18.9484975984601,18.9933693854802,19.0401328543241,19.0851285772229,19.1312801323088,
19.1774331204032,19.2175408288878),.UNSPECIFIED.);
#3039=B_SPLINE_CURVE_WITH_KNOTS('',3,(#48700,#48701,#48702,#48703,#48704,
#48705,#48706,#48707,#48708,#48709,#48710,#48711,#48712,#48713,#48714,#48715,
#48716,#48717,#48718,#48719,#48720,#48721,#48722,#48723,#48724,#48725,#48726,
#48727,#48728,#48729,#48730,#48731,#48732,#48733,#48734,#48735),
 .UNSPECIFIED.,.F.,.F.,(4,2,2,2,2,2,2,2,2,2,2,2,2,2,2,2,2,4),(2.22108960850334,
2.23120408655543,2.27635041769103,2.32327161206725,2.368237212408,2.41391337637609,
2.46061197050217,2.50519713949817,2.5513666691862,2.59796482416004,2.64299465171328,
2.68978881476098,2.73495033654449,2.78051325760178,2.82722340804027,2.87182391079689,
2.91788757586549,2.96056667106229),.UNSPECIFIED.);
#3040=B_SPLINE_CURVE_WITH_KNOTS('',3,(#48740,#48741,#48742,#48743,#48744,
#48745,#48746,#48747,#48748,#48749,#48750,#48751,#48752,#48753,#48754,#48755,
#48756,#48757,#48758,#48759,#48760,#48761,#48762,#48763,#48764,#48765,#48766,
#48767,#48768,#48769,#48770,#48771,#48772,#48773,#48774,#48775),
 .UNSPECIFIED.,.F.,.F.,(4,2,2,2,2,2,2,2,2,2,2,2,2,2,2,2,2,4),(17.7416164546727,
17.7581937026132,17.8052897667917,17.8505949548622,17.8963342504639,17.9428341472151,
17.9875910340227,18.0342105180494,18.0800707723051,18.124652551507,18.1712871824617,
18.2166406572815,18.2619848045744,18.3085503929415,18.3533657882032,18.4003592098579,
18.446278791736,18.4801374015765),.UNSPECIFIED.);
#3041=B_SPLINE_CURVE_WITH_KNOTS('',3,(#48776,#48777,#48778,#48779,#48780,
#48781,#48782,#48783,#48784,#48785,#48786,#48787,#48788,#48789,#48790,#48791,
#48792,#48793,#48794,#48795,#48796,#48797,#48798,#48799,#48800,#48801,#48802,
#48803,#48804,#48805,#48806,#48807,#48808,#48809,#48810,#48811,#48812,#48813),
 .UNSPECIFIED.,.F.,.F.,(4,2,2,2,2,2,2,2,2,2,2,2,2,2,2,2,2,2,4),(2.96056667106229,
2.96492507840458,3.00987622748865,3.05658369115965,3.10200096713613,3.14749048109044,
3.19424386894225,3.23892780465305,3.28492439308362,3.33166335864177,3.3765506531,
3.42318675517329,3.46898366970959,3.51441887461108,3.56165143931351,3.60649480370264,
3.65245839321213,3.69924258617203,3.70124435567),.UNSPECIFIED.);
#3042=B_SPLINE_CURVE_WITH_KNOTS('',3,(#48818,#48819,#48820,#48821,#48822,
#48823,#48824,#48825,#48826,#48827,#48828,#48829,#48830,#48831,#48832,#48833,
#48834,#48835,#48836,#48837,#48838,#48839,#48840,#48841,#48842,#48843,#48844,
#48845,#48846,#48847,#48848,#48849,#48850,#48851,#48852,#48853),
 .UNSPECIFIED.,.F.,.F.,(4,2,2,2,2,2,2,2,2,2,2,2,2,2,2,2,2,4),(17.002935008964,
17.0259159067871,17.0726902796453,17.117698909592,17.1640720079207,17.2102290646699,
17.2547667636235,17.301404789293,17.3470724875982,17.391917818806,17.4388344123328,
17.4839738011972,17.5299894371059,17.5763017108472,17.6209316820209,17.6676058954979,
17.7134384045876,17.7416164546727),.UNSPECIFIED.);
#3043=B_SPLINE_CURVE_WITH_KNOTS('',3,(#48854,#48855,#48856,#48857,#48858,
#48859,#48860,#48861,#48862,#48863,#48864,#48865,#48866,#48867,#48868,#48869,
#48870,#48871,#48872,#48873,#48874,#48875,#48876,#48877,#48878,#48879,#48880,
#48881,#48882,#48883,#48884,#48885,#48886,#48887,#48888,#48889),
 .UNSPECIFIED.,.F.,.F.,(4,2,2,2,2,2,2,2,2,2,2,2,2,2,2,2,2,4),(3.70124435567,
3.74399270352421,3.79043516379055,3.83649298289209,3.88175593971899,3.92880219425985,
3.97372113000247,4.01951325018307,4.0662546751028,4.11089815702418,4.15717909203302,
4.20358177465394,4.24870726106109,4.29560414076508,4.34067748019848,4.38633433906348,
4.43306819834531,4.44139309323576),.UNSPECIFIED.);
#3044=B_SPLINE_CURVE_WITH_KNOTS('',3,(#48894,#48895,#48896,#48897,#48898,
#48899,#48900,#48901,#48902,#48903,#48904,#48905,#48906,#48907,#48908,#48909,
#48910,#48911,#48912,#48913,#48914,#48915,#48916,#48917,#48918,#48919,#48920,
#48921,#48922,#48923,#48924,#48925,#48926,#48927,#48928,#48929),
 .UNSPECIFIED.,.F.,.F.,(4,2,2,2,2,2,2,2,2,2,2,2,2,2,2,2,2,4),(16.2641372477882,
16.2938030439013,16.3403922128616,16.3852327649267,16.4318876926505,16.4778418228271,
16.5224230010358,16.5690903677485,16.6145405429621,16.6597873151308,16.7064589317587,
16.7513738187352,16.7981669545333,16.8442036947422,16.8887271733991,16.9353636748532,
16.9809031318305,17.002935008964),.UNSPECIFIED.);
#3045=B_SPLINE_CURVE_WITH_KNOTS('',3,(#48930,#48931,#48932,#48933,#48934,
#48935,#48936,#48937,#48938,#48939,#48940,#48941,#48942,#48943,#48944,#48945,
#48946,#48947,#48948,#48949,#48950,#48951,#48952,#48953,#48954,#48955,#48956,
#48957,#48958,#48959,#48960,#48961,#48962,#48963,#48964,#48965),
 .UNSPECIFIED.,.F.,.F.,(4,2,2,2,2,2,2,2,2,2,2,2,2,2,2,2,2,4),(4.44139309323576,
4.47768369479005,4.52383758291686,4.57065155177945,4.61567630686354,4.66246297203597,
4.70776020748785,4.7533204420323,4.80007956137218,4.8447406734777,4.8908048094463,
4.93755248955131,4.98249808878681,5.02919719884178,5.0748218415068,5.12031038865077,
5.16760288129374,5.1818539671131),.UNSPECIFIED.);
#3046=B_SPLINE_CURVE_WITH_KNOTS('',3,(#48970,#48971,#48972,#48973,#48974,
#48975,#48976,#48977,#48978,#48979,#48980,#48981,#48982,#48983,#48984,#48985,
#48986,#48987,#48988,#48989,#48990,#48991,#48992,#48993,#48994,#48995,#48996,
#48997,#48998,#48999,#49000,#49001,#49002,#49003,#49004,#49005),
 .UNSPECIFIED.,.F.,.F.,(4,2,2,2,2,2,2,2,2,2,2,2,2,2,2,2,2,4),(15.5253008226521,
15.5614208712953,15.6076307463169,15.6521806514462,15.6988024510405,15.7445285973342,
15.7892808885852,15.8362633798431,15.8814623032694,15.9272761463232,15.9736600003967,
16.0183472154503,16.0650263145743,16.1109370835491,16.1556467547297,16.2028290254408,
16.2482129532865,16.2641372477882),.UNSPECIFIED.);
#3047=B_SPLINE_CURVE_WITH_KNOTS('',3,(#49006,#49007,#49008,#49009,#49010,
#49011,#49012,#49013,#49014,#49015,#49016,#49017,#49018,#49019,#49020,#49021,
#49022,#49023,#49024,#49025,#49026,#49027,#49028,#49029,#49030,#49031,#49032,
#49033,#49034,#49035,#49036,#49037,#49038,#49039,#49040,#49041),
 .UNSPECIFIED.,.F.,.F.,(4,2,2,2,2,2,2,2,2,2,2,2,2,2,2,2,2,4),(5.1818539671131,
5.21237880454505,5.258394968262,5.30515700825967,5.34994371692685,5.39643143835995,
5.44226233196025,5.48755936077848,5.53464520113254,5.57944804045745,5.62527291369698,
5.67197040786348,5.71660500923211,5.76291244064308,5.80904038797896,5.85417959966551,
5.90109443452282,5.92163532828753),.UNSPECIFIED.);
#3048=B_SPLINE_CURVE_WITH_KNOTS('',3,(#49046,#49047,#49048,#49049,#49050,
#49051,#49052,#49053,#49054,#49055,#49056,#49057,#49058,#49059,#49060,#49061,
#49062,#49063,#49064,#49065,#49066,#49067,#49068,#49069,#49070,#49071,#49072,
#49073,#49074,#49075,#49076,#49077,#49078,#49079,#49080,#49081),
 .UNSPECIFIED.,.F.,.F.,(4,2,2,2,2,2,2,2,2,2,2,2,2,2,2,2,2,4),(14.7873695620709,
14.8300506862385,14.8760153817406,14.9205240016754,14.9671371535707,15.0126019576596,
15.0576755801971,15.1043686547149,15.149301357282,15.1958140370104,15.2418832855322,
15.286374482974,15.3329751561295,15.3785518380475,15.4234279626835,15.4702466599603,
15.5152945505239,15.5253008226521),.UNSPECIFIED.);
#3049=B_SPLINE_CURVE_WITH_KNOTS('',3,(#49082,#49083,#49084,#49085,#49086,
#49087,#49088,#49089,#49090,#49091,#49092,#49093,#49094,#49095,#49096,#49097,
#49098,#49099,#49100,#49101,#49102,#49103,#49104,#49105,#49106,#49107,#49108,
#49109,#49110,#49111,#49112,#49113,#49114,#49115,#49116,#49117),
 .UNSPECIFIED.,.F.,.F.,(4,2,2,2,2,2,2,2,2,2,2,2,2,2,2,2,2,4),(5.92163532828753,
5.94600637034905,5.99167472503286,6.03834442621258,6.08290534138804,6.12906543193699,
6.17556776582538,6.22058468374404,6.26736631647045,6.31246290290152,6.358011917132,
6.40468792773244,6.44925237282631,6.4953007135921,6.54223498706927,6.58716711269207,
6.63385553062737,6.66068791027176),.UNSPECIFIED.);
#3050=B_SPLINE_CURVE_WITH_KNOTS('',3,(#49122,#49123,#49124,#49125,#49126,
#49127,#49128,#49129,#49130,#49131,#49132,#49133,#49134,#49135,#49136,#49137,
#49138,#49139,#49140,#49141,#49142,#49143,#49144,#49145,#49146,#49147,#49148,
#49149,#49150,#49151,#49152,#49153,#49154,#49155,#49156,#49157,#49158,#49159),
 .UNSPECIFIED.,.F.,.F.,(4,2,2,2,2,2,2,2,2,2,2,2,2,2,2,2,2,2,4),(14.0482100339955,
14.0502949245492,14.096984232057,14.142851009537,14.1876060347159,14.2347388331608,
14.2800782706825,14.3257899974572,14.3723273782223,14.41711976203,14.463762437258,
14.5096613573186,14.55425504223,14.6009122351073,14.6463049690835,14.6916352778898,
14.7382430334376,14.7830983471007,14.7873695620709),.UNSPECIFIED.);
#3051=B_SPLINE_CURVE_WITH_KNOTS('',3,(#49160,#49161,#49162,#49163,#49164,
#49165,#49166,#49167,#49168,#49169,#49170,#49171,#49172,#49173,#49174,#49175,
#49176,#49177,#49178,#49179,#49180,#49181,#49182,#49183,#49184,#49185,#49186,
#49187,#49188,#49189,#49190,#49191,#49192,#49193,#49194,#49195),
 .UNSPECIFIED.,.F.,.F.,(4,2,2,2,2,2,2,2,2,2,2,2,2,2,2,2,2,4),(6.66068791027176,
6.67919937428358,6.72466854077273,6.77138281680808,6.8160205136328,6.86199546468963,
6.90869606620136,6.95356006101863,7.00017259357045,7.04588152905359,7.09129151458587,
7.13849904618301,7.1832836822818,7.22922137847032,7.27595882272717,7.32067836819823,
7.3670926336791,7.40074313214862),.UNSPECIFIED.);
#3052=B_SPLINE_CURVE_WITH_KNOTS('',3,(#49200,#49201,#49202,#49203,#49204,
#49205,#49206,#49207,#49208,#49209,#49210,#49211,#49212,#49213,#49214,#49215,
#49216,#49217,#49218,#49219,#49220,#49221,#49222,#49223,#49224,#49225,#49226,
#49227,#49228,#49229,#49230,#49231,#49232,#49233,#49234,#49235),
 .UNSPECIFIED.,.F.,.F.,(4,2,2,2,2,2,2,2,2,2,2,2,2,2,2,2,2,4),(13.3095464675158,
13.3179418806692,13.3645829204745,13.4101456027589,13.4551345123131,13.5019343594699,
13.5469666402861,13.5932875705783,13.6394722908042,13.6840250076321,13.7306726518614,
13.7763692796775,13.8212020202917,13.8681498816812,13.9133183606713,13.9592929931832,
14.0056379903772,14.0482100339955),.UNSPECIFIED.);
#3053=B_SPLINE_CURVE_WITH_KNOTS('',3,(#49236,#49237,#49238,#49239,#49240,
#49241,#49242,#49243,#49244,#49245,#49246,#49247,#49248,#49249,#49250,#49251,
#49252,#49253,#49254,#49255,#49256,#49257,#49258,#49259,#49260,#49261,#49262,
#49263,#49264,#49265,#49266,#49267,#49268,#49269,#49270,#49271),
 .UNSPECIFIED.,.F.,.F.,(4,2,2,2,2,2,2,2,2,2,2,2,2,2,2,2,2,4),(7.40074313214862,
7.41304791193527,7.45828058796883,7.50529645981043,7.55014367964178,7.59590467610001,
7.64259365979734,7.68719438829927,7.73344217485688,7.77972977945611,7.82481959518803,
7.87168035903332,7.91667006179515,7.96229014337893,8.00896624300127,8.05352690669973,
8.09964223179755,8.13994719566162),.UNSPECIFIED.);
#3054=B_SPLINE_CURVE_WITH_KNOTS('',3,(#49276,#49277,#49278,#49279,#49280,
#49281,#49282,#49283,#49284,#49285,#49286,#49287,#49288,#49289,#49290,#49291,
#49292,#49293,#49294,#49295,#49296,#49297,#49298,#49299,#49300,#49301,#49302,
#49303,#49304,#49305,#49306,#49307,#49308,#49309,#49310,#49311),
 .UNSPECIFIED.,.F.,.F.,(4,2,2,2,2,2,2,2,2,2,2,2,2,2,2,2,2,4),(12.5705412100685,
12.5848546363202,12.6320513419363,12.6774479779185,12.7229914291377,12.7695957874756,
12.8144503148156,12.8611058709474,12.9070763074098,12.951650697705,12.9983178350321,
13.0437851961517,13.0889992823918,13.1356902587469,13.1806230630583,13.2273560115123,
13.2734149408359,13.3095464675158),.UNSPECIFIED.);
#3055=B_SPLINE_CURVE_WITH_KNOTS('',3,(#49312,#49313,#49314,#49315,#49316,
#49317,#49318,#49319,#49320,#49321,#49322,#49323,#49324,#49325,#49326,#49327,
#49328,#49329,#49330,#49331,#49332,#49333,#49334,#49335,#49336,#49337,#49338,
#49339,#49340,#49341,#49342,#49343,#49344,#49345,#49346,#49347,#49348,#49349),
 .UNSPECIFIED.,.F.,.F.,(4,2,2,2,2,2,2,2,2,2,2,2,2,2,2,2,2,2,4),(8.13994719566162,
8.1463316268328,8.19131496388372,8.2380593874591,8.28326280667136,8.33020598996195,
8.37537161294956,8.42146167930536,8.46779890512908,8.51245656585315,8.55916791039741,
8.60502388501555,8.64982522039719,8.69694438308839,8.7422725099988,8.78807715134522,
8.83459899420235,8.87937738670119,8.87958134265245),.UNSPECIFIED.);
#3056=B_SPLINE_CURVE_WITH_KNOTS('',3,(#49354,#49355,#49356,#49357,#49358,
#49359,#49360,#49361,#49362,#49363,#49364,#49365,#49366,#49367,#49368,#49369,
#49370,#49371,#49372,#49373,#49374,#49375,#49376,#49377,#49378,#49379,#49380,
#49381,#49382,#49383,#49384,#49385,#49386,#49387,#49388,#49389),
 .UNSPECIFIED.,.F.,.F.,(4,2,2,2,2,2,2,2,2,2,2,2,2,2,2,2,2,4),(11.8321815561307,
11.8527802750529,11.8996021687833,11.9446521456017,11.9907033317147,12.0369186139489,
12.0814657613186,12.1280739153687,12.1738072480122,12.2185277557899,12.2655192350349,
12.3107256977114,12.3564778448273,12.4028721237148,12.4475687949672,12.4942402335744,
12.5401634891127,12.5705412100685),.UNSPECIFIED.);
#3057=B_SPLINE_CURVE_WITH_KNOTS('',3,(#49390,#49391,#49392,#49393,#49394,
#49395,#49396,#49397,#49398,#49399,#49400,#49401,#49402,#49403,#49404,#49405,
#49406,#49407,#49408,#49409,#49410,#49411,#49412,#49413,#49414,#49415,#49416,
#49417,#49418,#49419,#49420,#49421,#49422,#49423,#49424,#49425),
 .UNSPECIFIED.,.F.,.F.,(4,2,2,2,2,2,2,2,2,2,2,2,2,2,2,2,2,4),(8.87958134265245,
8.92602852613987,8.97190922554665,9.01652860508801,9.06319528540556,9.10856829663463,
9.15396816684055,9.20055253946269,9.24538645185148,9.29245567553163,9.33839133852289,
9.38290947461184,9.42952391977244,9.47495799934766,9.52008834525836,9.56674688093536,
9.6116477128901,9.61793661341104),.UNSPECIFIED.);
#3058=B_SPLINE_CURVE_WITH_KNOTS('',3,(#49430,#49431,#49432,#49433,#49434,
#49435,#49436,#49437,#49438,#49439,#49440,#49441,#49442,#49443,#49444,#49445,
#49446,#49447,#49448,#49449,#49450,#49451,#49452,#49453,#49454,#49455,#49456,
#49457,#49458,#49459,#49460,#49461,#49462,#49463,#49464,#49465),
 .UNSPECIFIED.,.F.,.F.,(4,2,2,2,2,2,2,2,2,2,2,2,2,2,2,2,2,4),(11.0945157929649,
11.1213867420797,11.1679850354348,11.212830558321,11.2596899586864,11.3056487691199,
11.3501304725593,11.3967192229775,11.4421794409724,11.4871976310158,11.5338877382452,
11.5788167443302,11.6252436424475,11.6713128846608,11.7157888443594,11.7623703136435,
11.8079484981885,11.8321815561307),.UNSPECIFIED.);
#3059=B_SPLINE_CURVE_WITH_KNOTS('',3,(#49466,#49467,#49468,#49469,#49470,
#49471,#49472,#49473,#49474,#49475,#49476,#49477,#49478,#49479,#49480,#49481,
#49482,#49483,#49484,#49485,#49486,#49487,#49488,#49489,#49490,#49491,#49492,
#49493,#49494,#49495,#49496,#49497,#49498,#49499,#49500,#49501),
 .UNSPECIFIED.,.F.,.F.,(4,2,2,2,2,2,2,2,2,2,2,2,2,2,2,2,2,4),(9.61793661341104,
9.65826687912693,9.70429689093938,9.74877836477337,9.79537166131895,9.84090708321871,
9.88582218876157,9.93259567749554,9.97760169196064,10.0238180381891,10.0699792278232,
10.1144983947581,10.1611035398683,10.2067785301348,10.2515491657397,10.2984763720027,
10.3436239452287,10.3558181882677),.UNSPECIFIED.);
#3060=B_SPLINE_CURVE_WITH_KNOTS('',3,(#49506,#49507,#49508,#49509,#49510,
#49511,#49512,#49513,#49514,#49515,#49516,#49517,#49518,#49519,#49520,#49521,
#49522,#49523,#49524,#49525,#49526,#49527,#49528,#49529,#49530,#49531,#49532,
#49533,#49534,#49535,#49536,#49537,#49538,#49539,#49540,#49541),
 .UNSPECIFIED.,.F.,.F.,(4,2,2,2,2,2,2,2,2,2,2,2,2,2,2,2,2,4),(10.3558181865992,
10.3895062288278,10.4358326314552,10.4804680791543,10.5271205064737,10.5729708577389,
10.6176765737363,10.6647940480184,10.710117621532,10.7557512885806,10.8022746889798,
10.8470530120057,10.8936670905081,10.9395538338801,10.9841105681321,11.0307384394129,
11.0761201700909,11.0945157929649),.UNSPECIFIED.);
#3061=B_SPLINE_CURVE_WITH_KNOTS('',3,(#49542,#49543,#49544,#49545,#49546,
#49547,#49548,#49549,#49550,#49551,#49552,#49553,#49554,#49555,#49556,#49557,
#49558,#49559,#49560,#49561,#49562,#49563,#49564,#49565,#49566,#49567,#49568,
#49569,#49570,#49571,#49572,#49573,#49574,#49575,#49576,#49577),
 .UNSPECIFIED.,.F.,.F.,(4,2,2,2,2,2,2,2,2,2,2,2,2,2,2,2,2,4),(10.3558181882677,
10.3895062304569,10.4358326331012,10.4804680808162,10.5271205081509,10.572970859433,
10.6176765754436,10.6647940497431,10.7101176232735,10.7557512903329,10.8022746907493,
10.8470530137919,10.8936670923103,10.9395538356998,10.9841105699663,11.0307384412633,
11.0761201719588,11.0945157948807),.UNSPECIFIED.);
#3062=B_SPLINE_CURVE_WITH_KNOTS('',3,(#49582,#49583,#49584,#49585,#49586,
#49587,#49588,#49589,#49590,#49591,#49592,#49593,#49594,#49595,#49596,#49597,
#49598,#49599,#49600,#49601,#49602,#49603,#49604,#49605,#49606,#49607,#49608,
#49609,#49610,#49611,#49612,#49613,#49614,#49615,#49616,#49617),
 .UNSPECIFIED.,.F.,.F.,(4,2,2,2,2,2,2,2,2,2,2,2,2,2,2,2,2,4),(9.61793661197057,
9.65826687772365,9.7042968895204,9.74877836334091,9.79537165987244,9.84090708175655,
9.88582218728856,9.93259567600637,9.977601690456,10.0238180366761,10.069979226294,
10.1144983932143,10.16110353831,10.2067785285603,10.2515491641532,10.2984763703993,
10.3436239436092,10.3558181865992),.UNSPECIFIED.);
#3063=B_SPLINE_CURVE_WITH_KNOTS('',3,(#49618,#49619,#49620,#49621,#49622,
#49623,#49624,#49625,#49626,#49627,#49628,#49629,#49630,#49631,#49632,#49633,
#49634,#49635,#49636,#49637,#49638,#49639,#49640,#49641,#49642,#49643,#49644,
#49645,#49646,#49647,#49648,#49649,#49650,#49651,#49652,#49653),
 .UNSPECIFIED.,.F.,.F.,(4,2,2,2,2,2,2,2,2,2,2,2,2,2,2,2,2,4),(11.0945157948807,
11.1213867439599,11.1679850373331,11.2128305602366,11.2596899606121,11.3056487710637,
11.3501304745185,11.3967192249533,11.4421794429662,11.4871976330225,11.5338877402705,
11.5788167463733,11.625243644501,11.6713128867326,11.7157888464474,11.762370315748,
11.8079485003112,11.8321815583089),.UNSPECIFIED.);
#3064=B_SPLINE_CURVE_WITH_KNOTS('',3,(#49658,#49659,#49660,#49661,#49662,
#49663,#49664,#49665,#49666,#49667,#49668,#49669,#49670,#49671,#49672,#49673,
#49674,#49675,#49676,#49677,#49678,#49679,#49680,#49681,#49682,#49683,#49684,
#49685,#49686,#49687,#49688,#49689,#49690,#49691,#49692,#49693),
 .UNSPECIFIED.,.F.,.F.,(4,2,2,2,2,2,2,2,2,2,2,2,2,2,2,2,2,4),(8.87958134142251,
8.92602852493827,8.97190922433066,9.01652860386053,9.06319528416507,9.10856829537987,
9.15396816557657,9.20055253818396,9.24538645055861,9.29245567423173,9.33839133720815,
9.38290947328484,9.42952391843202,9.47495799799238,9.5200883438932,9.56674687955462,
9.61164771149445,9.61793661197057),.UNSPECIFIED.);
#3065=B_SPLINE_CURVE_WITH_KNOTS('',3,(#49694,#49695,#49696,#49697,#49698,
#49699,#49700,#49701,#49702,#49703,#49704,#49705,#49706,#49707,#49708,#49709,
#49710,#49711,#49712,#49713,#49714,#49715,#49716,#49717,#49718,#49719,#49720,
#49721,#49722,#49723,#49724,#49725,#49726,#49727,#49728,#49729),
 .UNSPECIFIED.,.F.,.F.,(4,2,2,2,2,2,2,2,2,2,2,2,2,2,2,2,2,4),(11.8321815583089,
11.8527802771891,11.8996021709384,11.9446521477749,11.9907033338989,12.0369186161519,
12.0814657635389,12.128073917606,12.1738072502682,12.2185277580605,12.2655192373249,
12.31072570002,12.3564778471481,12.402872126055,12.4475687973262,12.4942402359512,
12.5401634915089,12.5705412125212),.UNSPECIFIED.);
#3066=B_SPLINE_CURVE_WITH_KNOTS('',3,(#49734,#49735,#49736,#49737,#49738,
#49739,#49740,#49741,#49742,#49743,#49744,#49745,#49746,#49747,#49748,#49749,
#49750,#49751,#49752,#49753,#49754,#49755,#49756,#49757,#49758,#49759,#49760,
#49761,#49762,#49763,#49764,#49765,#49766,#49767,#49768,#49769,#49770,#49771),
 .UNSPECIFIED.,.F.,.F.,(4,2,2,2,2,2,2,2,2,2,2,2,2,2,2,2,2,2,4),(8.13994719462425,
8.14633162583834,8.19131496287961,8.23805938644507,8.28326280564246,8.33020598891935,
8.37537161189387,8.42146167824292,8.46779890405304,8.51245656476452,8.55916790929672,
8.60502388390122,8.64982521927269,8.69694438194964,8.74227250884644,8.78807715018487,
8.83459899302762,8.87937738551268,8.87958134142251),.UNSPECIFIED.);
#3067=B_SPLINE_CURVE_WITH_KNOTS('',3,(#49772,#49773,#49774,#49775,#49776,
#49777,#49778,#49779,#49780,#49781,#49782,#49783,#49784,#49785,#49786,#49787,
#49788,#49789,#49790,#49791,#49792,#49793,#49794,#49795,#49796,#49797,#49798,
#49799,#49800,#49801,#49802,#49803,#49804,#49805,#49806,#49807),
 .UNSPECIFIED.,.F.,.F.,(4,2,2,2,2,2,2,2,2,2,2,2,2,2,2,2,2,4),(12.5705412125212,
12.5848546387325,12.6320513443688,12.6774479803703,12.7229914316032,12.7695957899609,
12.81445031732,12.8611058734703,12.9070763099523,12.9516507002645,12.99831783761,
13.0437851987491,13.0889992850039,13.1356902613794,13.1806230657103,13.2273560141773,
13.2734149435215,13.3095464702606),.UNSPECIFIED.);
#3068=B_SPLINE_CURVE_WITH_KNOTS('',3,(#49812,#49813,#49814,#49815,#49816,
#49817,#49818,#49819,#49820,#49821,#49822,#49823,#49824,#49825,#49826,#49827,
#49828,#49829,#49830,#49831,#49832,#49833,#49834,#49835,#49836,#49837,#49838,
#49839,#49840,#49841,#49842,#49843,#49844,#49845,#49846,#49847),
 .UNSPECIFIED.,.F.,.F.,(4,2,2,2,2,2,2,2,2,2,2,2,2,2,2,2,2,4),(7.4007431312885,
7.41304791111891,7.45828058714382,7.50529645897655,7.55014367879521,7.59590467524459,
7.64259365893083,7.68719438742294,7.73344217397141,7.7797297785534,7.82481959427612,
7.87168035811193,7.91667006085986,7.96229014243438,8.00896624204524,8.05352690573283,
8.09964223082121,8.13994719462425),.UNSPECIFIED.);
#3069=B_SPLINE_CURVE_WITH_KNOTS('',3,(#49848,#49849,#49850,#49851,#49852,
#49853,#49854,#49855,#49856,#49857,#49858,#49859,#49860,#49861,#49862,#49863,
#49864,#49865,#49866,#49867,#49868,#49869,#49870,#49871,#49872,#49873,#49874,
#49875,#49876,#49877,#49878,#49879,#49880,#49881,#49882,#49883),
 .UNSPECIFIED.,.F.,.F.,(4,2,2,2,2,2,2,2,2,2,2,2,2,2,2,2,2,4),(13.3095464702606,
13.317941883373,13.3645829231975,13.4101456055024,13.4551345150724,13.5019343622502,
13.5469666430868,13.5932875733925,13.6394722936394,13.6840250104865,13.7306726547352,
13.7763692825722,13.8212020232032,13.8681498846145,13.9133183636254,13.9592929961519,
14.0056379933677,14.0482100370503),.UNSPECIFIED.);
#3070=B_SPLINE_CURVE_WITH_KNOTS('',3,(#49888,#49889,#49890,#49891,#49892,
#49893,#49894,#49895,#49896,#49897,#49898,#49899,#49900,#49901,#49902,#49903,
#49904,#49905,#49906,#49907,#49908,#49909,#49910,#49911,#49912,#49913,#49914,
#49915,#49916,#49917,#49918,#49919,#49920,#49921,#49922,#49923),
 .UNSPECIFIED.,.F.,.F.,(4,2,2,2,2,2,2,2,2,2,2,2,2,2,2,2,2,4),(6.66068790957161,
6.67919937362265,6.72466854010414,6.77138281612983,6.81602051294445,6.86199546399339,
6.90869606549543,6.95356006030469,7.00017259284827,7.04588152831696,7.09129151384102,
7.13849904542972,7.18328368151711,7.22922137769738,7.27595882194379,7.32067836740631,
7.36709263287862,7.4007431312885),.UNSPECIFIED.);
#3071=B_SPLINE_CURVE_WITH_KNOTS('',3,(#49924,#49925,#49926,#49927,#49928,
#49929,#49930,#49931,#49932,#49933,#49934,#49935,#49936,#49937,#49938,#49939,
#49940,#49941,#49942,#49943,#49944,#49945,#49946,#49947,#49948,#49949,#49950,
#49951,#49952,#49953,#49954,#49955,#49956,#49957,#49958,#49959,#49960,#49961),
 .UNSPECIFIED.,.F.,.F.,(4,2,2,2,2,2,2,2,2,2,2,2,2,2,2,2,2,2,4),(14.0482100370503,
14.0502949275604,14.0969842350884,14.1428510125903,14.1876060377872,14.2347388362546,
14.2800782737978,14.3257900005883,14.3723273813755,14.4171197652046,14.4637624404534,
14.5096613605359,14.5542550454664,14.6009122383646,14.6463049723626,14.6916352811859,
14.7382430367566,14.7830983504416,14.7873695654535),.UNSPECIFIED.);
#3072=B_SPLINE_CURVE_WITH_KNOTS('',3,(#49966,#49967,#49968,#49969,#49970,
#49971,#49972,#49973,#49974,#49975,#49976,#49977,#49978,#49979,#49980,#49981,
#49982,#49983,#49984,#49985,#49986,#49987,#49988,#49989,#49990,#49991,#49992,
#49993,#49994,#49995,#49996,#49997,#49998,#49999,#50000,#50001),
 .UNSPECIFIED.,.F.,.F.,(4,2,2,2,2,2,2,2,2,2,2,2,2,2,2,2,2,4),(5.92163532773223,
5.94600636983764,5.99167472451486,6.03834442568581,6.08290534085326,6.12906543139539,
6.17556776526837,6.22058468317993,6.26736631589905,6.31246290231792,6.35801191654115,
6.40468792713218,6.44925237221679,6.49530071297518,6.5422349864363,6.58716711205166,
6.6338555299793,6.66068790957161),.UNSPECIFIED.);
#3073=B_SPLINE_CURVE_WITH_KNOTS('',3,(#50002,#50003,#50004,#50005,#50006,
#50007,#50008,#50009,#50010,#50011,#50012,#50013,#50014,#50015,#50016,#50017,
#50018,#50019,#50020,#50021,#50022,#50023,#50024,#50025,#50026,#50027,#50028,
#50029,#50030,#50031,#50032,#50033,#50034,#50035,#50036,#50037),
 .UNSPECIFIED.,.F.,.F.,(4,2,2,2,2,2,2,2,2,2,2,2,2,2,2,2,2,4),(14.7873695654535,
14.8300506895943,14.8760153851188,14.9205240050731,14.9671371569893,15.0126019611003,
15.057675583655,15.1043686581955,15.1493013607845,15.1958140405279,15.2418832890724,
15.2863744865348,15.3329751597116,15.3785518416522,15.4234279663063,15.4702466636066,
15.5152945541928,15.52530082637),.UNSPECIFIED.);
#3074=B_SPLINE_CURVE_WITH_KNOTS('',3,(#50042,#50043,#50044,#50045,#50046,
#50047,#50048,#50049,#50050,#50051,#50052,#50053,#50054,#50055,#50056,#50057,
#50058,#50059,#50060,#50061,#50062,#50063,#50064,#50065,#50066,#50067,#50068,
#50069,#50070,#50071,#50072,#50073,#50074,#50075,#50076,#50077),
 .UNSPECIFIED.,.F.,.F.,(4,2,2,2,2,2,2,2,2,2,2,2,2,2,2,2,2,4),(5.18185396668694,
5.21237880416024,5.25839496787151,5.30515700786141,5.34994371652288,5.39643143795004,
5.44226233153737,5.48755936034949,5.53464520069729,5.57944804001234,5.62527291324563,
5.6719704074037,5.71660500876536,5.76291244016987,5.80904038749152,5.85417959917163,
5.90109443402236,5.92163532773223),.UNSPECIFIED.);
#3075=B_SPLINE_CURVE_WITH_KNOTS('',3,(#50078,#50079,#50080,#50081,#50082,
#50083,#50084,#50085,#50086,#50087,#50088,#50089,#50090,#50091,#50092,#50093,
#50094,#50095,#50096,#50097,#50098,#50099,#50100,#50101,#50102,#50103,#50104,
#50105,#50106,#50107,#50108,#50109,#50110,#50111,#50112,#50113),
 .UNSPECIFIED.,.F.,.F.,(4,2,2,2,2,2,2,2,2,2,2,2,2,2,2,2,2,4),(15.52530082637,
15.5614208749801,15.6076307500252,15.6521806551763,15.6988024547926,15.7445286011097,
15.7892808923799,15.8362633836619,15.8814623071114,15.927276150182,15.9736600042795,
16.0183472193562,16.0650263185026,16.1109370875013,16.1556467587023,16.2028290294383,
16.2482129573077,16.2641372518591),.UNSPECIFIED.);
#3076=B_SPLINE_CURVE_WITH_KNOTS('',3,(#50118,#50119,#50120,#50121,#50122,
#50123,#50124,#50125,#50126,#50127,#50128,#50129,#50130,#50131,#50132,#50133,
#50134,#50135,#50136,#50137,#50138,#50139,#50140,#50141,#50142,#50143,#50144,
#50145,#50146,#50147,#50148,#50149,#50150,#50151,#50152,#50153),
 .UNSPECIFIED.,.F.,.F.,(4,2,2,2,2,2,2,2,2,2,2,2,2,2,2,2,2,4),(4.44139309291887,
4.4776836945143,4.52383758263681,4.5706515514869,4.61567630656631,4.66246297173395,
4.70776020717613,4.75332044171567,4.80007956104877,4.84474067314722,4.89080480911077,
4.93755248920882,4.9824980884388,5.02919719848812,5.0748218411417,5.12031038828011,
5.16760288091741,5.18185396668694),.UNSPECIFIED.);
#3077=B_SPLINE_CURVE_WITH_KNOTS('',3,(#50154,#50155,#50156,#50157,#50158,
#50159,#50160,#50161,#50162,#50163,#50164,#50165,#50166,#50167,#50168,#50169,
#50170,#50171,#50172,#50173,#50174,#50175,#50176,#50177,#50178,#50179,#50180,
#50181,#50182,#50183,#50184,#50185,#50186,#50187,#50188,#50189),
 .UNSPECIFIED.,.F.,.F.,(4,2,2,2,2,2,2,2,2,2,2,2,2,2,2,2,2,4),(16.2641372518591,
16.2938030479407,16.3403922169256,16.3852327690144,16.4318876967614,16.4778418269624,
16.5224230051924,16.5690903719281,16.6145405471659,16.6597873193538,16.7064589360066,
16.7513738230071,16.7981669588227,16.8442036990566,16.8887271777361,16.9353636792139,
16.9809031362162,17.002935013404),.UNSPECIFIED.);
#3078=B_SPLINE_CURVE_WITH_KNOTS('',3,(#50194,#50195,#50196,#50197,#50198,
#50199,#50200,#50201,#50202,#50203,#50204,#50205,#50206,#50207,#50208,#50209,
#50210,#50211,#50212,#50213,#50214,#50215,#50216,#50217,#50218,#50219,#50220,
#50221,#50222,#50223,#50224,#50225,#50226,#50227,#50228,#50229),
 .UNSPECIFIED.,.F.,.F.,(4,2,2,2,2,2,2,2,2,2,2,2,2,2,2,2,2,4),(3.70124435544509,
3.74399270334172,3.79043516360456,3.83649298269546,3.88175593951858,3.92880219405563,
3.97372112979052,4.0195132499672,4.06625467488101,4.11089815679736,4.15717909180209,
4.20358177441128,4.24870726081431,4.29560414051408,4.34067747993884,4.38633433879972,
4.43306819807542,4.44139309291887),.UNSPECIFIED.);
#3079=B_SPLINE_CURVE_WITH_KNOTS('',3,(#50230,#50231,#50232,#50233,#50234,
#50235,#50236,#50237,#50238,#50239,#50240,#50241,#50242,#50243,#50244,#50245,
#50246,#50247,#50248,#50249,#50250,#50251,#50252,#50253,#50254,#50255,#50256,
#50257,#50258,#50259,#50260,#50261,#50262,#50263,#50264,#50265),
 .UNSPECIFIED.,.F.,.F.,(4,2,2,2,2,2,2,2,2,2,2,2,2,2,2,2,2,4),(17.002935013404,
17.025915911193,17.072690284077,17.1176989140485,17.1640720123954,17.2102290691703,
17.2547667681474,17.3014047938411,17.3470724921718,17.3919178234011,17.4388344169549,
17.4839738058451,17.5299894417733,17.576301715541,17.6209316867396,17.6676059002416,
17.7134384093576,17.7416164595014),.UNSPECIFIED.);
#3080=B_SPLINE_CURVE_WITH_KNOTS('',3,(#50270,#50271,#50272,#50273,#50274,
#50275,#50276,#50277,#50278,#50279,#50280,#50281,#50282,#50283,#50284,#50285,
#50286,#50287,#50288,#50289,#50290,#50291,#50292,#50293,#50294,#50295,#50296,
#50297,#50298,#50299,#50300,#50301,#50302,#50303,#50304,#50305,#50306,#50307),
 .UNSPECIFIED.,.F.,.F.,(4,2,2,2,2,2,2,2,2,2,2,2,2,2,2,2,2,2,4),(2.96056667091537,
2.96492507829847,3.00987622737974,3.05658369104791,3.10200096701632,3.14749048096761,
3.19424386881459,3.23892780451988,3.28492439294727,3.33166335850067,3.37655065295563,
3.42318675502558,3.46898366955253,3.51441887445073,3.56165143914983,3.60649480353247,
3.65245839303867,3.69924258599329,3.70124435544509),.UNSPECIFIED.);
#3081=B_SPLINE_CURVE_WITH_KNOTS('',3,(#50308,#50309,#50310,#50311,#50312,
#50313,#50314,#50315,#50316,#50317,#50318,#50319,#50320,#50321,#50322,#50323,
#50324,#50325,#50326,#50327,#50328,#50329,#50330,#50331,#50332,#50333,#50334,
#50335,#50336,#50337,#50338,#50339,#50340,#50341,#50342,#50343),
 .UNSPECIFIED.,.F.,.F.,(4,2,2,2,2,2,2,2,2,2,2,2,2,2,2,2,2,4),(17.7416164595014,
17.7581937074056,17.8052897716113,17.8505949597077,17.8963342553297,17.9428341521077,
17.9875910389412,18.0342105229933,18.0800707772756,18.1246525565008,18.1712871874809,
18.216640662327,18.2619848096412,18.3085503980356,18.3533657933236,18.400359214998,
18.4462787969036,18.4801374068086),.UNSPECIFIED.);
#3082=B_SPLINE_CURVE_WITH_KNOTS('',3,(#50348,#50349,#50350,#50351,#50352,
#50353,#50354,#50355,#50356,#50357,#50358,#50359,#50360,#50361,#50362,#50363,
#50364,#50365,#50366,#50367,#50368,#50369,#50370,#50371,#50372,#50373,#50374,
#50375,#50376,#50377,#50378,#50379,#50380,#50381,#50382,#50383),
 .UNSPECIFIED.,.F.,.F.,(4,2,2,2,2,2,2,2,2,2,2,2,2,2,2,2,2,4),(2.22108960842022,
2.23120408651738,2.27635041765121,2.32327161202571,2.36823721236016,2.41391337632635,
2.46061197044848,2.50519713944098,2.5513666691269,2.59796482409036,2.64299465164124,
2.68978881468655,2.73495033646277,2.78051325751773,2.82722340795193,2.87182391070409,
2.91788757577027,2.96056667091537),.UNSPECIFIED.);
#3083=B_SPLINE_CURVE_WITH_KNOTS('',3,(#50384,#50385,#50386,#50387,#50388,
#50389,#50390,#50391,#50392,#50393,#50394,#50395,#50396,#50397,#50398,#50399,
#50400,#50401,#50402,#50403,#50404,#50405,#50406,#50407,#50408,#50409,#50410,
#50411,#50412,#50413,#50414,#50415,#50416,#50417,#50418,#50419),
 .UNSPECIFIED.,.F.,.F.,(4,2,2,2,2,2,2,2,2,2,2,2,2,2,2,2,2,4),(18.4801374068086,
18.4907658387484,18.5373515732759,18.5827705496792,18.6278503876037,18.6744946287827,
18.7193811593225,18.7659288080364,18.8119468422919,18.8564049604675,18.9029730562544,
18.9484976039111,18.9933693909541,19.040132859827,19.0851285827534,19.1312801378602,
19.1774331259836,19.2175408345414),.UNSPECIFIED.);
#3084=B_SPLINE_CURVE_WITH_KNOTS('',3,(#50424,#50425,#50426,#50427,#50428,
#50429,#50430,#50431,#50432,#50433,#50434,#50435,#50436,#50437,#50438,#50439,
#50440,#50441,#50442,#50443,#50444,#50445,#50446,#50447,#50448,#50449,#50450,
#50451,#50452,#50453,#50454,#50455,#50456,#50457,#50458,#50459),
 .UNSPECIFIED.,.F.,.F.,(4,2,2,2,2,2,2,2,2,2,2,2,2,2,2,2,2,4),(1.48067239643092,
1.4967132601331,1.54219831559389,1.58948594493822,1.63428944893559,1.68030245144475,
1.72708174969294,1.77186789841824,1.81835464146151,1.86425678939566,1.90955548629973,
1.95664189807863,2.00148568451759,2.04731268579268,2.09403346709215,2.13867975716629,
2.18499121798638,2.22108960842022),.UNSPECIFIED.);
#3085=B_SPLINE_CURVE_WITH_KNOTS('',3,(#50460,#50461,#50462,#50463,#50464,
#50465,#50466,#50467,#50468,#50469,#50470,#50471,#50472,#50473,#50474,#50475,
#50476,#50477,#50478,#50479,#50480,#50481,#50482,#50483,#50484,#50485,#50486,
#50487,#50488,#50489,#50490,#50491,#50492,#50493,#50494,#50495,#50496,#50497),
 .UNSPECIFIED.,.F.,.F.,(4,2,2,2,2,2,2,2,2,2,2,2,2,2,2,2,2,2,4),(19.2175408345414,
19.221937402198,19.2685210781433,19.3141891434761,19.3589248273872,19.4058460255822,
19.4509870795851,19.4968133821774,19.5431350562803,19.5877640969252,19.634399062382,
19.6802461572256,19.724925976838,19.7720412018952,19.81736181445,19.862949655886,
19.9094715921544,19.954248074309,19.955968047547),.UNSPECIFIED.);
#3086=B_SPLINE_CURVE_WITH_KNOTS('',3,(#50502,#50503,#50504,#50505,#50506,
#50507,#50508,#50509,#50510,#50511,#50512,#50513,#50514,#50515,#50516,#50517,
#50518,#50519,#50520,#50521,#50522,#50523,#50524,#50525,#50526,#50527,#50528,
#50529,#50530,#50531,#50532,#50533,#50534,#50535,#50536,#50537),
 .UNSPECIFIED.,.F.,.F.,(4,2,2,2,2,2,2,2,2,2,2,2,2,2,2,2,2,4),(0.740262878330326,
0.76242710224918,0.808069985435835,0.854808846306471,0.899429812602798,
0.94557087207502,0.992454683252572,1.03747065149212,1.08424743872217,1.12958660658263,
1.17513888970271,1.22190780151563,1.26658471045133,1.31264188423565,1.35939848502835,
1.40433922056887,1.45103260194552,1.48067239643092),.UNSPECIFIED.);
#3087=B_SPLINE_CURVE_WITH_KNOTS('',3,(#50538,#50539,#50540,#50541,#50542,
#50543,#50544,#50545,#50546,#50547,#50548,#50549,#50550,#50551,#50552,#50553,
#50554,#50555,#50556,#50557,#50558,#50559,#50560,#50561,#50562,#50563,#50564,
#50565,#50566,#50567,#50568,#50569,#50570,#50571,#50572,#50573),
 .UNSPECIFIED.,.F.,.F.,(4,2,2,2,2,2,2,2,2,2,2,2,2,2,2,2,2,4),(19.955968047547,
20.000850484569,20.0467368471769,20.0912761893499,20.1378918513278,20.1832739357276,
20.2285046069091,20.2751045193351,20.3199511150685,20.3667546312751,20.4127173706803,
20.4571887517883,20.5037686958299,20.5492336722642,20.5942218827244,20.6409180673264,
20.685852328368,20.6936878782319),.UNSPECIFIED.);
#3088=B_SPLINE_CURVE_WITH_KNOTS('',3,(#50578,#50579,#50580,#50581,#50582,
#50583,#50584,#50585,#50586,#50587,#50588,#50589,#50590,#50591,#50592,#50593,
#50594,#50595,#50596,#50597,#50598,#50599,#50600,#50601,#50602,#50603,#50604,
#50605,#50606,#50607,#50608,#50609,#50610,#50611,#50612,#50613),
 .UNSPECIFIED.,.F.,.F.,(4,2,2,2,2,2,2,2,2,2,2,2,2,2,2,2,2,4),(1.00000014275486E-6,
0.0364903991724837,0.0742057368406976,0.120984278386942,0.16571626048475,
0.212135354717781,0.258243398985401,0.303486376623694,0.350510827495094,
0.395451299112592,0.441223703714196,0.487964967575798,0.532602258878132,
0.578864855190162,0.62532910035835,0.67044002179057,0.717320863587734,0.740262878330326),
 .UNSPECIFIED.);
#3089=B_SPLINE_CURVE_WITH_KNOTS('',3,(#50614,#50615,#50616,#50617,#50618,
#50619,#50620,#50621,#50622,#50623,#50624,#50625,#50626,#50627,#50628,#50629,
#50630,#50631,#50632,#50633,#50634,#50635,#50636,#50637,#50638,#50639,#50640,
#50641,#50642,#50643,#50644,#50645,#50646,#50647,#50648,#50649),
 .UNSPECIFIED.,.F.,.F.,(4,2,2,2,2,2,2,2,2,2,2,2,2,2,2,2,2,4),(20.6936878782319,
20.732228532913,20.778305724133,20.8227795112891,20.8693557797099,20.9149428959302,
20.9597524918607,21.0065846919771,21.0516438918501,21.0976519462771,21.1438788857884,
21.188432480541,21.2350393010027,21.2807854645354,21.325492530929,21.3724982961973,
21.417717731441,21.4315064083924),.UNSPECIFIED.);
#3090=B_SPLINE_CURVE_WITH_KNOTS('',3,(#50652,#50653,#50654,#50655,#50656,
#50657,#50658,#50659),.UNSPECIFIED.,.F.,.F.,(4,2,2,4),(21.4315064083924,
21.4634358005757,21.493031868375,21.522626598838),.UNSPECIFIED.);
#3091=B_SPLINE_CURVE_WITH_KNOTS('',3,(#50664,#50665,#50666,#50667,#50668,
#50669,#50670,#50671,#50672,#50673,#50674,#50675),.UNSPECIFIED.,.F.,.F.,
(4,2,2,2,2,4),(-0.220493779628296,-0.188155373461082,-0.153829429857051,
-0.103952453260852,-0.0536656706932583,-1.00000014990886E-6),
 .UNSPECIFIED.);
#3092=B_SPLINE_CURVE_WITH_KNOTS('',3,(#50678,#50679,#50680,#50681,#50682,
#50683,#50684,#50685,#50686,#50687,#50688,#50689,#50690,#50691,#50692,#50693,
#50694,#50695,#50696,#50697,#50698,#50699),.UNSPECIFIED.,.F.,.F.,(4,2,2,
2,2,2,2,2,2,2,4),(0.203440126186273,0.213167596868103,0.241856386112924,
0.272211919544501,0.305118112000406,0.341399456620154,0.378879659132554,
0.40534149334872,0.429291364608543,0.44378295238274,0.459192789470913),
 .UNSPECIFIED.);
#3093=B_SPLINE_CURVE_WITH_KNOTS('',3,(#50701,#50702,#50703,#50704,#50705,
#50706,#50707,#50708,#50709,#50710,#50711,#50712,#50713,#50714,#50715,#50716,
#50717,#50718,#50719,#50720,#50721,#50722,#50723,#50724,#50725,#50726,#50727,
#50728,#50729,#50730,#50731,#50732,#50733,#50734),.UNSPECIFIED.,.F.,.F.,
(4,2,2,2,2,2,2,2,2,2,2,2,2,2,2,2,4),(-0.921606618540025,-0.872688627355351,
-0.813612023857313,-0.756611351546357,-0.69692945872276,-0.638499761548747,
-0.581118209737007,-0.521076231967445,-0.463317306881228,-0.4044438926574,
-0.345164740388026,-0.288053249414949,-0.228344796882901,-0.169710130792356,
-0.112479424024743,-0.0563089256119929,-9.99999990258793E-7),
 .UNSPECIFIED.);
#3094=B_SPLINE_CURVE_WITH_KNOTS('',3,(#50735,#50736,#50737,#50738,#50739,
#50740,#50741,#50742,#50743,#50744,#50745,#50746,#50747,#50748,#50749,#50750,
#50751,#50752,#50753,#50754,#50755,#50756,#50757,#50758,#50759,#50760,#50761,
#50762,#50763,#50764,#50765,#50766),.UNSPECIFIED.,.F.,.F.,(4,2,2,2,2,2,
2,2,2,2,2,2,2,2,2,4),(-27.2675995337344,-27.2205810783644,-27.1716030839864,
-27.1114524980469,-27.0544959346273,-26.9959799991961,-26.9364896777515,
-26.8795127522937,-26.8203565510693,-26.7619639947482,-26.7043369916545,
-26.6444247756288,-26.5873734790364,-26.5290771329393,-26.4696302887724,
-26.4647006629411),.UNSPECIFIED.);
#3095=B_SPLINE_CURVE_WITH_KNOTS('',3,(#50943,#50944,#50945,#50946,#50947,
#50948,#50949,#50950),.UNSPECIFIED.,.F.,.F.,(4,2,2,4),(-0.00426615559741139,
-0.00353262795509977,-0.00302253710286643,-0.00251244625063308),
 .UNSPECIFIED.);
#3096=B_SPLINE_CURVE_WITH_KNOTS('',3,(#51864,#51865,#51866,#51867,#51868,
#51869,#51870,#51871),.UNSPECIFIED.,.F.,.F.,(4,2,2,4),(-0.00251244625063308,
-0.00200235539839974,-0.0014922645461664,-0.000758736903856822),
 .UNSPECIFIED.);
#3097=B_SPLINE_CURVE_WITH_KNOTS('',3,(#51876,#51877,#51878,#51879,#51880,
#51881,#51882,#51883),.UNSPECIFIED.,.F.,.F.,(4,2,2,4),(-0.00932716297425779,
-0.00859363533194745,-0.0080835444797141,-0.00757345362748076),
 .UNSPECIFIED.);
#3098=B_SPLINE_CURVE_WITH_KNOTS('',3,(#52797,#52798,#52799,#52800,#52801,
#52802,#52803,#52804),.UNSPECIFIED.,.F.,.F.,(4,2,2,4),(-0.00757345362748076,
-0.00706336277524741,-0.00655327192301407,-0.00581974428070595),
 .UNSPECIFIED.);
#3099=B_SPLINE_CURVE_WITH_KNOTS('',3,(#54800,#54801,#54802,#54803,#54804,
#54805,#54806,#54807,#54808,#54809,#54810,#54811,#54812,#54813,#54814,#54815,
#54816,#54817,#54818,#54819,#54820,#54821,#54822,#54823,#54824,#54825,#54826,
#54827),.UNSPECIFIED.,.F.,.F.,(4,2,2,2,2,2,2,2,2,2,2,2,2,4),(1.00000052656661E-6,
0.0405527857266322,0.0799421814660319,0.1262631587317,0.186952165234641,
0.270820823781497,0.348937293245129,0.459507052180891,0.623823282878412,
0.790896670749941,0.927459468885873,1.05843758188768,1.16179395572833,1.24835467272154),
 .UNSPECIFIED.);
#3100=B_SPLINE_CURVE_WITH_KNOTS('',3,(#55937,#55938,#55939,#55940,#55941,
#55942,#55943,#55944,#55945,#55946,#55947,#55948,#55949,#55950,#55951,#55952,
#55953,#55954,#55955,#55956,#55957,#55958,#55959,#55960,#55961,#55962,#55963,
#55964,#55965,#55966,#55967,#55968,#55969,#55970,#55971,#55972),
 .UNSPECIFIED.,.F.,.F.,(4,2,2,2,2,2,2,2,2,2,2,2,2,2,2,2,2,4),(-0.945073641183675,
-0.895238035194944,-0.83625541046657,-0.779319325111488,-0.719695813140934,
-0.661359932358853,-0.603989382535731,-0.544046656752618,-0.486380595229568,
-0.427463950957105,-0.368285170516134,-0.311258814957492,-0.251615042406746,
-0.193080680180277,-0.135881569867343,-0.0757214675349668,-0.0372079607299379,
-9.99999995143774E-7),.UNSPECIFIED.);
#3101=B_SPLINE_CURVE_WITH_KNOTS('',3,(#55978,#55979,#55980,#55981,#55982,
#55983,#55984,#55985,#55986,#55987,#55988,#55989,#55990,#55991,#55992,#55993,
#55994,#55995,#55996,#55997,#55998,#55999,#56000,#56001,#56002,#56003,#56004,
#56005,#56006,#56007,#56008,#56009,#56010,#56011),.UNSPECIFIED.,.F.,.F.,
(4,2,2,2,2,2,2,2,2,2,2,2,2,2,2,2,4),(-27.258759550315,-27.2281298462553,
-27.1982051538512,-27.1403355656588,-27.0801605899845,-27.0231066733285,
-26.9645639497272,-26.9050010855415,-26.8479917157334,-26.7888070303952,
-26.7302213719406,-26.6725610910419,-26.6126177738291,-26.5554428144319,
-26.4971129260297,-26.4375855046171,-26.4315188069733),.UNSPECIFIED.);
#3102=B_SPLINE_CURVE_WITH_KNOTS('',3,(#56016,#56017,#56018,#56019,#56020,
#56021,#56022,#56023,#56024,#56025,#56026,#56027,#56028,#56029,#56030,#56031,
#56032,#56033,#56034,#56035,#56036,#56037,#56038,#56039,#56040,#56041,#56042,
#56043,#56044,#56045,#56046,#56047,#56048,#56049,#56050,#56051),
 .UNSPECIFIED.,.F.,.F.,(4,2,2,2,2,2,2,2,2,2,2,2,2,2,2,2,2,4),(-1.89025095676006,
-1.83161362612537,-1.77291723413503,-1.71588088128378,-1.65621305093223,
-1.59816806724067,-1.54019307596245,-1.48057902624682,-1.42320721251111,
-1.36315245228605,-1.30433237640506,-1.24738924893859,-1.18775702178512,
-1.12958586526634,-1.07195013380193,-1.0121910944455,-0.954689933605391,
-0.945073641183675),.UNSPECIFIED.);
#3103=B_SPLINE_CURVE_WITH_KNOTS('',3,(#56052,#56053,#56054,#56055,#56056,
#56057,#56058,#56059,#56060,#56061,#56062,#56063,#56064,#56065,#56066,#56067,
#56068,#56069,#56070,#56071,#56072,#56073,#56074,#56075,#56076,#56077,#56078,
#56079,#56080,#56081,#56082,#56083,#56084,#56085,#56086,#56087),
 .UNSPECIFIED.,.F.,.F.,(4,2,2,2,2,2,2,2,2,2,2,2,2,2,2,2,2,4),(-26.4315188069733,
-26.3807149169946,-26.3217404209326,-26.2626652889544,-26.2051855221022,
-26.1454428390691,-26.08804784233,-26.0298996832198,-25.970377539516,-25.9135472636022,
-25.8547523829465,-25.7951046336945,-25.7377721236726,-25.6781939173096,
-25.6204935481626,-25.5624909627037,-25.5029463840743,-25.4881909358829),
 .UNSPECIFIED.);
#3104=B_SPLINE_CURVE_WITH_KNOTS('',3,(#56092,#56093,#56094,#56095,#56096,
#56097,#56098,#56099,#56100,#56101,#56102,#56103,#56104,#56105,#56106,#56107,
#56108,#56109,#56110,#56111,#56112,#56113,#56114,#56115,#56116,#56117,#56118,
#56119,#56120,#56121,#56122,#56123,#56124,#56125,#56126,#56127,#56128,#56129),
 .UNSPECIFIED.,.F.,.F.,(4,2,2,2,2,2,2,2,2,2,2,2,2,2,2,2,2,2,4),(-2.83625896355377,
-2.82853093222041,-2.76886611006394,-2.71046756100465,-2.65308502383756,
-2.59307616772703,-2.5353480705631,-2.47645222776391,-2.41720668492958,
-2.36012338869581,-2.30043449435393,-2.24183347940531,-2.1846099393252,
-2.12437972037366,-2.06645193254166,-2.00798057621261,-1.94850769470731,
-1.89126109663031,-1.89025095676006),.UNSPECIFIED.);
#3105=B_SPLINE_CURVE_WITH_KNOTS('',3,(#56130,#56131,#56132,#56133,#56134,
#56135,#56136,#56137,#56138,#56139,#56140,#56141,#56142,#56143,#56144,#56145,
#56146,#56147,#56148,#56149,#56150,#56151,#56152,#56153,#56154,#56155,#56156,
#56157,#56158,#56159,#56160,#56161,#56162,#56163,#56164,#56165),
 .UNSPECIFIED.,.F.,.F.,(4,2,2,2,2,2,2,2,2,2,2,2,2,2,2,2,2,4),(-25.4881909358829,
-25.4460636732589,-25.3874120918811,-25.3278816537184,-25.2706841301686,
-25.2112575632321,-25.1531186176646,-25.0952452143788,-25.0350644348795,
-24.9780430196917,-24.9194961959997,-24.8599520194551,-24.8029424006809,
-24.7437542679059,-24.6852489172368,-24.6275880933991,-24.5676424609794,
-24.544394043377),.UNSPECIFIED.);
#3106=B_SPLINE_CURVE_WITH_KNOTS('',3,(#56170,#56171,#56172,#56173,#56174,
#56175,#56176,#56177,#56178,#56179,#56180,#56181,#56182,#56183,#56184,#56185,
#56186,#56187,#56188,#56189,#56190,#56191,#56192,#56193,#56194,#56195,#56196,
#56197,#56198,#56199,#56200,#56201,#56202,#56203,#56204,#56205),
 .UNSPECIFIED.,.F.,.F.,(4,2,2,2,2,2,2,2,2,2,2,2,2,2,2,2,2,4),(-3.78192035948685,
-3.76562796298537,-3.70592564973338,-3.6478278361799,-3.5898592957152,-3.53018901929876,
-3.47276427223133,-3.41274694188657,-3.3538687217505,-3.29689298752725,
-3.2372230084892,-3.17899386626536,-3.12135698149028,-3.06153650613278,
-3.00397762776562,-2.94455692608413,-2.88551146939021,-2.83625896355377),
 .UNSPECIFIED.);
#3107=B_SPLINE_CURVE_WITH_KNOTS('',3,(#56206,#56207,#56208,#56209,#56210,
#56211,#56212,#56213,#56214,#56215,#56216,#56217,#56218,#56219,#56220,#56221,
#56222,#56223,#56224,#56225,#56226,#56227,#56228,#56229,#56230,#56231,#56232,
#56233,#56234,#56235,#56236,#56237,#56238,#56239,#56240,#56241),
 .UNSPECIFIED.,.F.,.F.,(4,2,2,2,2,2,2,2,2,2,2,2,2,2,2,2,2,4),(-24.544394043377,
-24.5105131978097,-24.4521827141638,-24.3926780124691,-24.3358195936076,
-24.2768451471733,-24.2178632708879,-24.1603868788961,-24.1006461200198,
-24.0433090290329,-23.9851645307063,-23.9256688814307,-23.8688632830925,
-23.8100726156683,-23.7505272749807,-23.6932025949219,-23.6336311604901,
-23.6014349735858),.UNSPECIFIED.);
#3108=B_SPLINE_CURVE_WITH_KNOTS('',3,(#56246,#56247,#56248,#56249,#56250,
#56251,#56252,#56253,#56254,#56255,#56256,#56257,#56258,#56259,#56260,#56261,
#56262,#56263,#56264,#56265,#56266,#56267,#56268,#56269,#56270,#56271,#56272,
#56273,#56274,#56275,#56276,#56277,#56278,#56279,#56280,#56281),
 .UNSPECIFIED.,.F.,.F.,(4,2,2,2,2,2,2,2,2,2,2,2,2,2,2,2,2,4),(-4.72839430207058,
-4.70337431740566,-4.64331595464347,-4.58554178921411,-4.52667966073054,
-4.4673838894256,-4.41025831032806,-4.35054027250619,-4.29188896156004,
-4.23465469260147,-4.17437122548907,-4.11639389057874,-4.05794278357937,
-3.99841660337735,-3.94111979450562,-3.88143640467257,-3.82268708479341,
-3.78192035948685),.UNSPECIFIED.);
#3109=B_SPLINE_CURVE_WITH_KNOTS('',3,(#56282,#56283,#56284,#56285,#56286,
#56287,#56288,#56289,#56290,#56291,#56292,#56293,#56294,#56295,#56296,#56297,
#56298,#56299,#56300,#56301,#56302,#56303,#56304,#56305,#56306,#56307,#56308,
#56309,#56310,#56311,#56312,#56313,#56314,#56315,#56316,#56317),
 .UNSPECIFIED.,.F.,.F.,(4,2,2,2,2,2,2,2,2,2,2,2,2,2,2,2,2,4),(-23.6014349735858,
-23.5759985868542,-23.5180045036599,-23.458489879113,-23.4016430359386,
-23.3430005479742,-23.2834982736845,-23.226310920464,-23.166893628097,-23.1088378874003,
-23.0509758826866,-22.9908049952875,-22.9338319947597,-22.8752964277514,
-22.8157879004539,-22.7587920199088,-22.6996160282244,-22.6581171675807),
 .UNSPECIFIED.);
#3110=B_SPLINE_CURVE_WITH_KNOTS('',3,(#56322,#56323,#56324,#56325,#56326,
#56327,#56328,#56329,#56330,#56331,#56332,#56333,#56334,#56335,#56336,#56337,
#56338,#56339,#56340,#56341,#56342,#56343,#56344,#56345,#56346,#56347,#56348,
#56349,#56350,#56351,#56352,#56353,#56354,#56355,#56356,#56357),
 .UNSPECIFIED.,.F.,.F.,(4,2,2,2,2,2,2,2,2,2,2,2,2,2,2,2,2,4),(-5.67439159596968,
-5.64047766140835,-5.58076721688331,-5.52330498546526,-5.4633387313466,
-5.40441833910885,-5.34742402529794,-5.28773207490788,-5.22946075409439,
-5.17183622553644,-5.11197061930769,-5.05436969869878,-4.99499338073396,
-4.9359013779351,-4.878890651626,-4.8192004273671,-4.76075532631967,-4.72839430207058),
 .UNSPECIFIED.);
#3111=B_SPLINE_CURVE_WITH_KNOTS('',3,(#56358,#56359,#56360,#56361,#56362,
#56363,#56364,#56365,#56366,#56367,#56368,#56369,#56370,#56371,#56372,#56373,
#56374,#56375,#56376,#56377,#56378,#56379,#56380,#56381,#56382,#56383,#56384,
#56385,#56386,#56387,#56388,#56389,#56390,#56391,#56392,#56393),
 .UNSPECIFIED.,.F.,.F.,(4,2,2,2,2,2,2,2,2,2,2,2,2,2,2,2,2,4),(-22.6581171675807,
-22.6412102410835,-22.5835641689142,-22.5236319902899,-22.4665652482388,
-22.4082496043878,-22.3487848861067,-22.2919531828174,-22.2329943725634,
-22.1741263229248,-22.1166686457465,-22.0569456248039,-21.9996842855768,
-21.9415589369491,-21.8821072544915,-21.8253417468782,-21.7665709936596,
-21.7157628302399),.UNSPECIFIED.);
#3112=B_SPLINE_CURVE_WITH_KNOTS('',3,(#56398,#56399,#56400,#56401,#56402,
#56403,#56404,#56405,#56406,#56407,#56408,#56409,#56410,#56411,#56412,#56413,
#56414,#56415,#56416,#56417,#56418,#56419,#56420,#56421,#56422,#56423,#56424,
#56425,#56426,#56427,#56428,#56429,#56430,#56431,#56432,#56433),
 .UNSPECIFIED.,.F.,.F.,(4,2,2,2,2,2,2,2,2,2,2,2,2,2,2,2,2,4),(-6.62109380521341,
-6.57761768259959,-6.51828740763027,-6.46113362202641,-6.40140207096381,
-6.34271600715298,-6.28548482095171,-6.22516410228413,-6.16715260360109,
-6.10873547077658,-6.04917186097877,-5.99184011673613,-5.93213648107799,
-5.8733499659965,-5.81628212661826,-5.75656105013342,-5.69842598086126,
-5.67439159596968),.UNSPECIFIED.);
#3113=B_SPLINE_CURVE_WITH_KNOTS('',3,(#56434,#56435,#56436,#56437,#56438,
#56439,#56440,#56441,#56442,#56443,#56444,#56445,#56446,#56447,#56448,#56449,
#56450,#56451,#56452,#56453,#56454,#56455,#56456,#56457,#56458,#56459,#56460,
#56461,#56462,#56463,#56464,#56465,#56466,#56467,#56468,#56469),
 .UNSPECIFIED.,.F.,.F.,(4,2,2,2,2,2,2,2,2,2,2,2,2,2,2,2,2,4),(-21.7157628302399,
-21.7071499734112,-21.6498486291818,-21.5902999589255,-21.5327541629797,
-21.4747842600729,-21.4153173211779,-21.3585227590009,-21.2999052492263,
-21.2398720875173,-21.1826905454483,-21.1232764692568,-21.065378520901,
-21.0075245508875,-20.9480158554619,-20.8911101904613,-20.8326059984683,
-20.7731793950157),.UNSPECIFIED.);
#3114=B_SPLINE_CURVE_WITH_KNOTS('',3,(#56474,#56475,#56476,#56477,#56478,
#56479,#56480,#56481,#56482,#56483,#56484,#56485,#56486,#56487,#56488,#56489,
#56490,#56491,#56492,#56493,#56494,#56495,#56496,#56497,#56498,#56499,#56500,
#56501,#56502,#56503,#56504,#56505,#56506,#56507,#56508,#56509),
 .UNSPECIFIED.,.F.,.F.,(4,2,2,2,2,2,2,2,2,2,2,2,2,2,2,2,2,4),(-7.56721318319246,
-7.51440195941646,-7.4554548070908,-7.39845589958658,-7.33875763160917,
-7.28045937419718,-7.22286133868259,-7.16296628560166,-7.10533842940707,
-7.04602095897405,-6.9868979771895,-6.92987099130527,-6.87017100691209,
-6.81169474396116,-6.75432913502786,-6.69423710481114,-6.63643211656935,
-6.62109380521341),.UNSPECIFIED.);
#3115=B_SPLINE_CURVE_WITH_KNOTS('',3,(#56510,#56511,#56512,#56513,#56514,
#56515,#56516,#56517,#56518,#56519,#56520,#56521,#56522,#56523,#56524,#56525,
#56526,#56527,#56528,#56529,#56530,#56531,#56532,#56533,#56534,#56535,#56536,
#56537,#56538,#56539,#56540,#56541,#56542,#56543,#56544,#56545,#56546,#56547),
 .UNSPECIFIED.,.F.,.F.,(4,2,2,2,2,2,2,2,2,2,2,2,2,2,2,2,2,2,4),(-20.7731793950157,
-20.7731201315055,-20.7160582025871,-20.6567792566783,-20.5983599289237,
-20.5406164839802,-20.4805811221967,-20.4234656784966,-20.3650514109911,
-20.305511597516,-20.2485949896086,-20.1895371334662,-20.1306696919239,
-20.0731189832228,-20.0132974755221,-19.9560008596223,-19.8977815738613,
-19.8382589546996,-19.8295444030046),.UNSPECIFIED.);
#3116=B_SPLINE_CURVE_WITH_KNOTS('',3,(#56552,#56553,#56554,#56555,#56556,
#56557,#56558,#56559,#56560,#56561,#56562,#56563,#56564,#56565,#56566,#56567,
#56568,#56569,#56570,#56571,#56572,#56573,#56574,#56575,#56576,#56577,#56578,
#56579,#56580,#56581,#56582,#56583,#56584,#56585,#56586,#56587,#56588,#56589),
 .UNSPECIFIED.,.F.,.F.,(4,2,2,2,2,2,2,2,2,2,2,2,2,2,2,2,2,2,4),(-8.51391269073544,
-8.51222365838152,-8.45249428513948,-8.39378861667143,-8.33657472393003,
-8.27623231073072,-8.21820164401039,-8.1598332741766,-8.10024765479814,
-8.04289584139225,-7.98318755401621,-7.92437912604881,-7.86731677437594,
-7.80759259896721,-7.74943539170332,-7.6915218402897,-7.631786775557,-7.57430204194946,
-7.56721318319246),.UNSPECIFIED.);
#3117=B_SPLINE_CURVE_WITH_KNOTS('',3,(#56590,#56591,#56592,#56593,#56594,
#56595,#56596,#56597,#56598,#56599,#56600,#56601,#56602,#56603,#56604,#56605,
#56606,#56607,#56608,#56609,#56610,#56611,#56612,#56613,#56614,#56615,#56616,
#56617,#56618,#56619,#56620,#56621,#56622,#56623,#56624,#56625),
 .UNSPECIFIED.,.F.,.F.,(4,2,2,2,2,2,2,2,2,2,2,2,2,2,2,2,2,4),(-19.8295444030046,
-19.781422440649,-19.7225572817117,-19.6631471763022,-19.6057577545878,
-19.5461159927651,-19.4885461013889,-19.4304876297435,-19.3709535721035,
-19.3141007093386,-19.2553941827952,-19.1953773792029,-19.1381132548424,
-19.0786120692882,-19.0206974716804,-18.9627608300149,-18.9031885891784,
-18.8860416189937),.UNSPECIFIED.);
#3118=B_SPLINE_CURVE_WITH_KNOTS('',3,(#56630,#56631,#56632,#56633,#56634,
#56635,#56636,#56637,#56638,#56639,#56640,#56641,#56642,#56643,#56644,#56645,
#56646,#56647,#56648,#56649,#56650,#56651,#56652,#56653,#56654,#56655,#56656,
#56657,#56658,#56659,#56660,#56661,#56662,#56663,#56664,#56665),
 .UNSPECIFIED.,.F.,.F.,(4,2,2,2,2,2,2,2,2,2,2,2,2,2,2,2,2,4),(-9.4600020867739,
-9.44946097484441,-9.38977226427863,-9.3314620836995,-9.27390543364871,
-9.21399634460654,-9.15635642704838,-9.09711384600216,-9.03797514352587,
-8.98094579786149,-8.92125183936447,-8.86275948675276,-8.8054237975235,
-8.7453135764027,-8.68749269541132,-8.62874128051507,-8.56939184171518,
-8.51391269073544),.UNSPECIFIED.);
#3119=B_SPLINE_CURVE_WITH_KNOTS('',3,(#56666,#56667,#56668,#56669,#56670,
#56671,#56672,#56673,#56674,#56675,#56676,#56677,#56678,#56679,#56680,#56681,
#56682,#56683,#56684,#56685,#56686,#56687,#56688,#56689,#56690,#56691,#56692,
#56693,#56694,#56695,#56696,#56697,#56698,#56699,#56700,#56701),
 .UNSPECIFIED.,.F.,.F.,(4,2,2,2,2,2,2,2,2,2,2,2,2,2,2,2,2,4),(-18.8860416189937,
-18.8462348900712,-18.7876476548069,-18.7280968440835,-18.6709555484027,
-18.6115929558287,-18.5531716016611,-18.495349324202,-18.4352301709226,
-18.3780798368063,-18.319585679885,-18.2599881331103,-18.2030028878512,
-18.1438648978918,-18.0850090800984,-18.0273834680497,-17.9674824112817,
-17.941522876477),.UNSPECIFIED.);
#3120=B_SPLINE_CURVE_WITH_KNOTS('',3,(#56706,#56707,#56708,#56709,#56710,
#56711,#56712,#56713,#56714,#56715,#56716,#56717,#56718,#56719,#56720,#56721,
#56722,#56723,#56724,#56725,#56726,#56727,#56728,#56729,#56730,#56731,#56732,
#56733,#56734,#56735,#56736,#56737,#56738,#56739,#56740,#56741),
 .UNSPECIFIED.,.F.,.F.,(4,2,2,2,2,2,2,2,2,2,2,2,2,2,2,2,2,4),(-10.4063262286273,
-10.387392591544,-10.3270439303512,-10.2690090232558,-10.210705562305,-10.1511132343272,
-10.09375612853,-10.034059046947,-9.97524386932148,-9.91820163035005,-9.8584903134111,
-9.80032595747233,-9.74246277833438,-9.68271846928724,-9.62522607647149,
-9.56540900336133,-9.50645028314585,-9.4600020867739),.UNSPECIFIED.);
#3121=B_SPLINE_CURVE_WITH_KNOTS('',3,(#56742,#56743,#56744,#56745,#56746,
#56747,#56748,#56749,#56750,#56751,#56752,#56753,#56754,#56755,#56756,#56757,
#56758,#56759,#56760,#56761,#56762,#56763,#56764,#56765,#56766,#56767,#56768,
#56769,#56770,#56771,#56772,#56773,#56774,#56775,#56776,#56777),
 .UNSPECIFIED.,.F.,.F.,(4,2,2,2,2,2,2,2,2,2,2,2,2,2,2,2,2,4),(-17.941522876477,
-17.9101636562757,-17.8518687182981,-17.7922922877475,-17.7354001068821,
-17.6764590004862,-17.6170707989498,-17.5596109797981,-17.4998945731994,
-17.4423134048219,-17.3841841685699,-17.3245998970605,-17.2677034424408,
-17.2089258668494,-17.1489368038417,-17.0916073172332,-17.0320369692312,
-16.997272415308),.UNSPECIFIED.);
#3122=B_SPLINE_CURVE_WITH_KNOTS('',3,(#56782,#56783,#56784,#56785,#56786,
#56787,#56788,#56789,#56790,#56791,#56792,#56793,#56794,#56795,#56796,#56797,
#56798,#56799,#56800,#56801,#56802,#56803,#56804,#56805,#56806,#56807,#56808,
#56809,#56810,#56811,#56812,#56813,#56814,#56815,#56816,#56817),
 .UNSPECIFIED.,.F.,.F.,(4,2,2,2,2,2,2,2,2,2,2,2,2,2,2,2,2,4),(-11.3522871924595,
-11.324430394275,-11.264522730746,-11.2068857092522,-11.1477360236872,-11.08859687367,
-11.0315792760543,-10.9719076335357,-10.9134142640608,-10.8561239489264,
-10.796010976838,-10.7381891351563,-10.6795177406942,-10.620164420077,-10.5629956093436,
-10.5032845165816,-10.4445743180876,-10.4063262286273),.UNSPECIFIED.);
#3123=B_SPLINE_CURVE_WITH_KNOTS('',3,(#56818,#56819,#56820,#56821,#56822,
#56823,#56824,#56825,#56826,#56827,#56828,#56829,#56830,#56831,#56832,#56833,
#56834,#56835,#56836,#56837,#56838,#56839,#56840,#56841,#56842,#56843,#56844,
#56845,#56846,#56847,#56848,#56849,#56850,#56851,#56852,#56853),
 .UNSPECIFIED.,.F.,.F.,(4,2,2,2,2,2,2,2,2,2,2,2,2,2,2,2,2,4),(-16.997272415308,
-16.974118579872,-16.9161165902415,-16.8564975009602,-16.7995101512218,
-16.7408573501075,-16.6812582779792,-16.6240545216982,-16.5646258893359,
-16.5062147666311,-16.448330624569,-16.388145391231,-16.3309738020301,-16.2724169024022,
-16.2127779950283,-16.155739296564,-16.0965384948368,-16.052121842989),
 .UNSPECIFIED.);
#3124=B_SPLINE_CURVE_WITH_KNOTS('',3,(#56858,#56859,#56860,#56861,#56862,
#56863,#56864,#56865,#56866,#56867,#56868,#56869,#56870,#56871,#56872,#56873,
#56874,#56875,#56876,#56877,#56878,#56879,#56880,#56881,#56882,#56883,#56884,
#56885,#56886,#56887,#56888,#56889,#56890,#56891,#56892,#56893),
 .UNSPECIFIED.,.F.,.F.,(4,2,2,2,2,2,2,2,2,2,2,2,2,2,2,2,2,4),(-12.2980151684053,
-12.2608049534251,-12.2012214180354,-12.1438740189948,-12.0842046319712,
-12.0253980696236,-11.9683912868138,-11.9087094544592,-11.8505531273409,
-11.7927573534416,-11.7330193273245,-11.6755342944868,-11.6158192576419,
-11.5568642629696,-11.4998992163216,-11.4402365277277,-11.3819295252021,
-11.3522871924595),.UNSPECIFIED.);
#3125=B_SPLINE_CURVE_WITH_KNOTS('',3,(#56894,#56895,#56896,#56897,#56898,
#56899,#56900,#56901,#56902,#56903,#56904,#56905,#56906,#56907,#56908,#56909,
#56910,#56911,#56912,#56913,#56914,#56915,#56916,#56917,#56918,#56919,#56920,
#56921,#56922,#56923,#56924,#56925,#56926,#56927,#56928,#56929),
 .UNSPECIFIED.,.F.,.F.,(4,2,2,2,2,2,2,2,2,2,2,2,2,2,2,2,2,4),(-16.052121842989,
-16.0377063442003,-15.9800225041649,-15.9200592855784,-15.8627316418797,
-15.8043778785959,-15.7447638720137,-15.6878306019307,-15.6288305455336,
-15.5694764347843,-15.5119625793001,-15.452188569769,-15.3946092699113,
-15.3364257590099,-15.2768073817686,-15.2198815508401,-15.1610495793805,
-15.1073443691545),.UNSPECIFIED.);
#3126=B_SPLINE_CURVE_WITH_KNOTS('',3,(#56934,#56935,#56936,#56937,#56938,
#56939,#56940,#56941,#56942,#56943,#56944,#56945,#56946,#56947,#56948,#56949,
#56950,#56951,#56952,#56953,#56954,#56955,#56956,#56957,#56958,#56959,#56960,
#56961,#56962,#56963,#56964,#56965,#56966,#56967,#56968,#56969),
 .UNSPECIFIED.,.F.,.F.,(4,2,2,2,2,2,2,2,2,2,2,2,2,2,2,2,2,4),(-13.2436220538442,
-13.1973293402993,-13.1382053560805,-13.0812140676331,-13.0215819437106,
-12.9631029490451,-12.905874761448,-12.8457747640532,-12.787967213325,-12.7293949980337,
-12.670053341907,-12.6128978517491,-12.5532219431716,-12.494522530246,-12.4373888207658,
-12.3770495663262,-12.3190255916381,-12.2980151684053),.UNSPECIFIED.);
#3127=B_SPLINE_CURVE_WITH_KNOTS('',3,(#56970,#56971,#56972,#56973,#56974,
#56975,#56976,#56977,#56978,#56979,#56980,#56981,#56982,#56983,#56984,#56985,
#56986,#56987,#56988,#56989,#56990,#56991,#56992,#56993,#56994,#56995,#56996,
#56997,#56998,#56999,#57000,#57001,#57002,#57003,#57004,#57005,#57006,#57007),
 .UNSPECIFIED.,.F.,.F.,(4,2,2,2,2,2,2,2,2,2,2,2,2,2,2,2,2,2,4),(-15.1073443691545,
-15.1011008892937,-15.0437220848592,-14.9840992717133,-14.926190394778,
-14.8681392181562,-14.8084892686686,-14.7514823595925,-14.6927803091387,
-14.6331489331619,-14.5758985339276,-14.5164203125443,-14.4580324516964,
-14.4001023522461,-14.339867608388,-14.2826884114687,-14.2240848432797,
-14.1644203791933,-14.161791521072),.UNSPECIFIED.);
#3128=B_SPLINE_CURVE_WITH_KNOTS('',3,(#57012,#57013,#57014,#57015,#57016,
#57017,#57018,#57019,#57020,#57021,#57022,#57023,#57024,#57025,#57026,#57027,
#57028,#57029,#57030,#57031,#57032,#57033,#57034,#57035,#57036,#57037,#57038,
#57039,#57040,#57041,#57042,#57043,#57044,#57045,#57046,#57047),
 .UNSPECIFIED.,.F.,.F.,(4,2,2,2,2,2,2,2,2,2,2,2,2,2,2,2,2,4),(-14.1885859699234,
-14.1330844909293,-14.0738030834317,-14.0151322001193,-13.9573780431577,
-13.8973369154889,-13.8400747014035,-13.781649842778,-13.7220284098382,
-13.6650669338426,-13.6061313895152,-13.5492060305576,-13.4895868440872,
-13.4312985326842,-13.3738747554208,-13.3139843572995,-13.2563655957482,
-13.2436220538442),.UNSPECIFIED.);
#3129=B_SPLINE_CURVE_WITH_KNOTS('',3,(#57048,#57049,#57050,#57051,#57052,
#57053,#57054,#57055,#57056,#57057,#57058,#57059,#57060,#57061,#57062,#57063,
#57064,#57065,#57066,#57067,#57068,#57069,#57070,#57071,#57072,#57073,#57074,
#57075,#57076,#57077,#57078,#57079,#57080,#57081,#57082,#57083),
 .UNSPECIFIED.,.F.,.F.,(4,2,2,2,2,2,2,2,2,2,2,2,2,2,2,2,2,4),(-14.161791521072,
-14.1073426685626,-14.0480953063394,-13.9892999039839,-13.9315735440484,
-13.8715645099561,-13.8142414960538,-13.7558447627025,-13.6962089327002,
-13.6392486779599,-13.5802573437773,-13.5233108369954,-13.4636758610349,
-13.4053314288153,-13.3479464458854,-13.2879951425265,-13.2303206406094,
-13.2166062380566),.UNSPECIFIED.);
#3130=B_SPLINE_CURVE_WITH_KNOTS('',3,(#57088,#57089,#57090,#57091,#57092,
#57093,#57094,#57095,#57096,#57097,#57098,#57099,#57100,#57101,#57102,#57103,
#57104,#57105,#57106,#57107,#57108,#57109,#57110,#57111,#57112,#57113,#57114,
#57115,#57116,#57117,#57118,#57119,#57120,#57121,#57122,#57123,#57124,#57125),
 .UNSPECIFIED.,.F.,.F.,(4,2,2,2,2,2,2,2,2,2,2,2,2,2,2,2,2,2,4),(-15.1341561055544,
-15.1269994338561,-15.0695799723091,-15.0099125340775,-14.9520739190766,
-14.8939828445778,-14.8343297519005,-14.7773366004228,-14.7185951213641,
-14.6589576423824,-14.6016713251844,-14.5421535644632,-14.4838629359255,
-14.4258987192761,-14.3656251166082,-14.3084824988271,-14.2498440170218,
-14.1901865832963,-14.1885859699234),.UNSPECIFIED.);
#3131=B_SPLINE_CURVE_WITH_KNOTS('',3,(#57126,#57127,#57128,#57129,#57130,
#57131,#57132,#57133,#57134,#57135,#57136,#57137,#57138,#57139,#57140,#57141,
#57142,#57143,#57144,#57145,#57146,#57147,#57148,#57149,#57150,#57151,#57152,
#57153,#57154,#57155,#57156,#57157,#57158,#57159,#57160,#57161),
 .UNSPECIFIED.,.F.,.F.,(4,2,2,2,2,2,2,2,2,2,2,2,2,2,2,2,2,4),(-13.2166062380566,
-13.1713851979337,-13.1121981319385,-13.0551628296182,-12.9955080421381,
-12.9369655576865,-12.8797535453401,-12.819585289645,-12.761715189623,-12.7032194250943,
-12.6438086463492,-12.586620577358,-12.5270150261763,-12.4683803900242,
-12.4113696886299,-12.35174219741,-12.2937588655423,-12.2712695292436),
 .UNSPECIFIED.);
#3132=B_SPLINE_CURVE_WITH_KNOTS('',3,(#57166,#57167,#57168,#57169,#57170,
#57171,#57172,#57173,#57174,#57175,#57176,#57177,#57178,#57179,#57180,#57181,
#57182,#57183,#57184,#57185,#57186,#57187,#57188,#57189,#57190,#57191,#57192,
#57193,#57194,#57195,#57196,#57197,#57198,#57199,#57200,#57201),
 .UNSPECIFIED.,.F.,.F.,(4,2,2,2,2,2,2,2,2,2,2,2,2,2,2,2,2,4),(-16.0791645683298,
-16.0637629880179,-16.0060223350212,-15.9459969234656,-15.8887024341941,
-15.8302912537239,-15.7706612508563,-15.7136999051047,-15.654642811055,
-15.5954057874932,-15.5378426704977,-15.4780146687669,-15.4204898319656,
-15.3622571133794,-15.3026293793744,-15.2456979578477,-15.1868171504776,
-15.1341561055544),.UNSPECIFIED.);
#3133=B_SPLINE_CURVE_WITH_KNOTS('',3,(#57202,#57203,#57204,#57205,#57206,
#57207,#57208,#57209,#57210,#57211,#57212,#57213,#57214,#57215,#57216,#57217,
#57218,#57219,#57220,#57221,#57222,#57223,#57224,#57225,#57226,#57227,#57228,
#57229,#57230,#57231,#57232,#57233,#57234,#57235,#57236,#57237),
 .UNSPECIFIED.,.F.,.F.,(4,2,2,2,2,2,2,2,2,2,2,2,2,2,2,2,2,4),(-12.2712695292436,
-12.2357754508004,-12.1762270533728,-12.1189170680661,-12.0588176303639,
-12.0000655464483,-11.943159299172,-11.8835712422689,-11.8254678956475,
-11.7678321870858,-11.708145031833,-11.6507114242844,-11.5912213696332,
-11.5323122460786,-11.4754266605439,-11.4158513420701,-11.3575887654668,
-11.3269908932583),.UNSPECIFIED.);
#3134=B_SPLINE_CURVE_WITH_KNOTS('',3,(#57242,#57243,#57244,#57245,#57246,
#57247,#57248,#57249,#57250,#57251,#57252,#57253,#57254,#57255,#57256,#57257,
#57258,#57259,#57260,#57261,#57262,#57263,#57264,#57265,#57266,#57267,#57268,
#57269,#57270,#57271,#57272,#57273,#57274,#57275,#57276,#57277),
 .UNSPECIFIED.,.F.,.F.,(4,2,2,2,2,2,2,2,2,2,2,2,2,2,2,2,2,4),(-17.0247741151702,
-17.0006922494049,-16.942620899042,-16.8829683888398,-16.8259674619989,
-16.7672454552544,-16.7076101234707,-16.6503415003102,-16.590843286514,
-16.5325014804607,-16.4745540351945,-16.4142996421448,-16.357137434069,
-16.2985161360182,-16.2388539992256,-16.1817640975146,-16.1224994016558,
-16.0791645683298),.UNSPECIFIED.);
#3135=B_SPLINE_CURVE_WITH_KNOTS('',3,(#57278,#57279,#57280,#57281,#57282,
#57283,#57284,#57285,#57286,#57287,#57288,#57289,#57290,#57291,#57292,#57293,
#57294,#57295,#57296,#57297,#57298,#57299,#57300,#57301,#57302,#57303,#57304,
#57305,#57306,#57307,#57308,#57309,#57310,#57311,#57312,#57313),
 .UNSPECIFIED.,.F.,.F.,(4,2,2,2,2,2,2,2,2,2,2,2,2,2,2,2,2,4),(-11.3269908932583,
-11.3002304831747,-11.2403651502537,-11.1827717007332,-11.1238285355636,
-11.064728011521,-11.0077668972893,-10.9481757635054,-10.8897195155163,
-10.8325471683827,-10.7724692707686,-10.7146842840278,-10.6561946025542,
-10.5968740051404,-10.5397395269343,-10.4801014814801,-10.4214223488875,
-10.3822526002173),.UNSPECIFIED.);
#3136=B_SPLINE_CURVE_WITH_KNOTS('',3,(#57318,#57319,#57320,#57321,#57322,
#57323,#57324,#57325,#57326,#57327,#57328,#57329,#57330,#57331,#57332,#57333,
#57334,#57335,#57336,#57337,#57338,#57339,#57340,#57341,#57342,#57343,#57344,
#57345,#57346,#57347,#57348,#57349,#57350,#57351,#57352,#57353),
 .UNSPECIFIED.,.F.,.F.,(4,2,2,2,2,2,2,2,2,2,2,2,2,2,2,2,2,4),(-17.9696970255303,
-17.937289370862,-17.8789069021961,-17.8192841522869,-17.7623368372575,
-17.7033082433986,-17.6440100001385,-17.5864714106887,-17.526670356869,
-17.4691167328281,-17.4109085209012,-17.3512845924667,-17.2943555190345,
-17.2354990142404,-17.1756126480208,-17.1182132969445,-17.0585679978772,
-17.0247741151702),.UNSPECIFIED.);
#3137=B_SPLINE_CURVE_WITH_KNOTS('',3,(#57354,#57355,#57356,#57357,#57358,
#57359,#57360,#57361,#57362,#57363,#57364,#57365,#57366,#57367,#57368,#57369,
#57370,#57371,#57372,#57373,#57374,#57375,#57376,#57377,#57378,#57379,#57380,
#57381,#57382,#57383,#57384,#57385,#57386,#57387,#57388,#57389),
 .UNSPECIFIED.,.F.,.F.,(4,2,2,2,2,2,2,2,2,2,2,2,2,2,2,2,2,4),(-10.3822526002173,
-10.3643343540307,-10.3046400968479,-10.246613334744,-10.1885181147052,
-10.128927402479,-10.0715754084394,-10.011325400927,-9.9525347708931,-9.89556195447909,
-9.83591091083034,-9.77776999750488,-9.72003077893023,-9.66030722303232,
-9.60283704872725,-9.54320316116386,-9.48426076178981,-9.43689892858011),
 .UNSPECIFIED.);
#3138=B_SPLINE_CURVE_WITH_KNOTS('',3,(#57394,#57395,#57396,#57397,#57398,
#57399,#57400,#57401,#57402,#57403,#57404,#57405,#57406,#57407,#57408,#57409,
#57410,#57411,#57412,#57413,#57414,#57415,#57416,#57417,#57418,#57419,#57420,
#57421,#57422,#57423,#57424,#57425,#57426,#57427,#57428,#57429),
 .UNSPECIFIED.,.F.,.F.,(4,2,2,2,2,2,2,2,2,2,2,2,2,2,2,2,2,4),(-18.9151145034862,
-18.8743164654268,-18.8156291548377,-18.7560115648048,-18.6987754493173,
-18.6393121439161,-18.5809341256596,-18.5230183981635,-18.4627987144582,
-18.4056311968295,-18.3470421802252,-18.2873910545073,-18.2303271150055,
-18.171094421965,-18.1123080260466,-18.0545957689432,-17.9946015046478,
-17.9696970255303),.UNSPECIFIED.);
#3139=B_SPLINE_CURVE_WITH_KNOTS('',3,(#57430,#57431,#57432,#57433,#57434,
#57435,#57436,#57437,#57438,#57439,#57440,#57441,#57442,#57443,#57444,#57445,
#57446,#57447,#57448,#57449,#57450,#57451,#57452,#57453,#57454,#57455,#57456,
#57457,#57458,#57459,#57460,#57461,#57462,#57463,#57464,#57465),
 .UNSPECIFIED.,.F.,.F.,(4,2,2,2,2,2,2,2,2,2,2,2,2,2,2,2,2,4),(-9.43689892858011,
-9.42732171849391,-9.36768738295302,-9.30939248028644,-9.25194272911408,
-9.19204622378449,-9.13442101602013,-9.07534568068709,-9.01621630273034,
-8.95921594082851,-8.89957004368503,-8.84108593111714,-8.78383634874988,
-8.72373170856049,-8.6659190669351,-8.60731272480359,-8.54796686813959,
-8.49156038630827),.UNSPECIFIED.);
#3140=B_SPLINE_CURVE_WITH_KNOTS('',3,(#57470,#57471,#57472,#57473,#57474,
#57475,#57476,#57477,#57478,#57479,#57480,#57481,#57482,#57483,#57484,#57485,
#57486,#57487,#57488,#57489,#57490,#57491,#57492,#57493,#57494,#57495,#57496,
#57497,#57498,#57499,#57500,#57501,#57502,#57503,#57504,#57505),
 .UNSPECIFIED.,.F.,.F.,(4,2,2,2,2,2,2,2,2,2,2,2,2,2,2,2,2,4),(-19.8597382210236,
-19.810451373043,-19.7514667566491,-19.6921219719675,-19.6346229403372,
-19.5748644342208,-19.5172962645061,-19.4591277252691,-19.3995232496075,
-19.3426105099162,-19.2837936446735,-19.2238539608265,-19.1664896413472,
-19.1068819617647,-19.0489837573588,-18.9909471893313,-18.9313109305834,
-18.9151145034862),.UNSPECIFIED.);
#3141=B_SPLINE_CURVE_WITH_KNOTS('',3,(#57506,#57507,#57508,#57509,#57510,
#57511,#57512,#57513,#57514,#57515,#57516,#57517,#57518,#57519,#57520,#57521,
#57522,#57523,#57524,#57525,#57526,#57527,#57528,#57529,#57530,#57531,#57532,
#57533,#57534,#57535,#57536,#57537,#57538,#57539,#57540,#57541,#57542,#57543),
 .UNSPECIFIED.,.F.,.F.,(4,2,2,2,2,2,2,2,2,2,2,2,2,2,2,2,2,2,4),(-8.49156038630827,
-8.49080675575303,-8.43111857134256,-8.37241526446117,-8.31526501763932,
-8.25492233706489,-8.19689441801019,-8.13864530142174,-8.07905854481672,
-8.02170761683104,-7.96202852596394,-7.9032187975688,-7.84619976450985,
-7.78650760972943,-7.72834831916545,-7.67052935317836,-7.61078895216033,
-7.55330118212272,-7.54539583975842),.UNSPECIFIED.);
#3142=B_SPLINE_CURVE_WITH_KNOTS('',3,(#57548,#57549,#57550,#57551,#57552,
#57553,#57554,#57555,#57556,#57557,#57558,#57559,#57560,#57561,#57562,#57563,
#57564,#57565,#57566,#57567,#57568,#57569,#57570,#57571,#57572,#57573,#57574,
#57575,#57576,#57577,#57578,#57579,#57580,#57581,#57582,#57583,#57584,#57585),
 .UNSPECIFIED.,.F.,.F.,(4,2,2,2,2,2,2,2,2,2,2,2,2,2,2,2,2,2,4),(-20.8047268284554,
-20.8036363389145,-20.7464479008663,-20.6870352594353,-20.6286348915891,
-20.5707661629285,-20.510597073108,-20.4534380889162,-20.3948967931479,
-20.3352722771837,-20.2782483009287,-20.219063232801,-20.1602410153004,
-20.1025723093681,-20.0426249323872,-19.9853090960203,-19.9269706384341,
-19.867370764855,-19.8597382210236),.UNSPECIFIED.);
#3143=B_SPLINE_CURVE_WITH_KNOTS('',3,(#57586,#57587,#57588,#57589,#57590,
#57591,#57592,#57593,#57594,#57595,#57596,#57597,#57598,#57599,#57600,#57601,
#57602,#57603,#57604,#57605,#57606,#57607,#57608,#57609,#57610,#57611,#57612,
#57613,#57614,#57615,#57616,#57617,#57618,#57619,#57620,#57621),
 .UNSPECIFIED.,.F.,.F.,(4,2,2,2,2,2,2,2,2,2,2,2,2,2,2,2,2,4),(-7.54539583975842,
-7.49355110204946,-7.43459460077228,-7.37762115395009,-7.31794932817515,
-7.25964100917192,-7.20212210603924,-7.14221371611197,-7.08457547245393,
-7.02539392871746,-6.96625468515904,-6.90923296876007,-6.84955345859718,
-6.79106019408235,-6.73375428080265,-6.6736419972573,-6.61582024058893,
-6.59962043014718),.UNSPECIFIED.);
#3144=B_SPLINE_CURVE_WITH_KNOTS('',3,(#57626,#57627,#57628,#57629,#57630,
#57631,#57632,#57633,#57634,#57635,#57636,#57637,#57638,#57639,#57640,#57641,
#57642,#57643,#57644,#57645,#57646,#57647,#57648,#57649,#57650,#57651,#57652,
#57653,#57654,#57655,#57656,#57657,#57658,#57659,#57660,#57661),
 .UNSPECIFIED.,.F.,.F.,(4,2,2,2,2,2,2,2,2,2,2,2,2,2,2,2,2,4),(-21.7489046572791,
-21.7392153866495,-21.6817714549229,-21.6220716583751,-21.5645025223573,
-21.5063893301253,-21.4468200256293,-21.3899376073178,-21.3311762213552,
-21.2711970668162,-21.2138831121422,-21.1543289862749,-21.0964221879644,
-21.0384358621701,-20.9788315240901,-20.9218575630073,-20.8632205676017,
-20.8047268284554),.UNSPECIFIED.);
#3145=B_SPLINE_CURVE_WITH_KNOTS('',3,(#57662,#57663,#57664,#57665,#57666,
#57667,#57668,#57669,#57670,#57671,#57672,#57673,#57674,#57675,#57676,#57677,
#57678,#57679,#57680,#57681,#57682,#57683,#57684,#57685,#57686,#57687,#57688,
#57689,#57690,#57691,#57692,#57693,#57694,#57695,#57696,#57697),
 .UNSPECIFIED.,.F.,.F.,(4,2,2,2,2,2,2,2,2,2,2,2,2,2,2,2,2,4),(-6.59962043014718,
-6.55712143056447,-6.49776917806976,-6.44060046014423,-6.3808828825634,
-6.32217397813377,-6.26498116754636,-6.20463437850135,-6.14660066752985,
-6.0882749718812,-6.02868466855325,-5.9713291133043,-5.91162795849117,-5.85281481524407,
-5.79576557777481,-5.73604961995392,-5.67788743624381,-5.65305968192749),
 .UNSPECIFIED.);
#3146=B_SPLINE_CURVE_WITH_KNOTS('',3,(#57702,#57703,#57704,#57705,#57706,
#57707,#57708,#57709,#57710,#57711,#57712,#57713,#57714,#57715,#57716,#57717,
#57718,#57719,#57720,#57721,#57722,#57723,#57724,#57725,#57726,#57727,#57728,
#57729,#57730,#57731,#57732,#57733,#57734,#57735,#57736,#57737),
 .UNSPECIFIED.,.F.,.F.,(4,2,2,2,2,2,2,2,2,2,2,2,2,2,2,2,2,4),(-22.6930944862137,
-22.6750742815793,-22.6172685137948,-22.5571666469156,-22.5000298336195,
-22.4415523883347,-22.3819703093803,-22.3250007752965,-22.2658796385637,
-22.2070346049225,-22.1494252073759,-22.0895411174023,-22.0322350703383,
-21.9739565284333,-21.9143953015877,-21.8575179583935,-21.7985933937003,
-21.7489046572791),.UNSPECIFIED.);
#3147=B_SPLINE_CURVE_WITH_KNOTS('',3,(#57738,#57739,#57740,#57741,#57742,
#57743,#57744,#57745,#57746,#57747,#57748,#57749,#57750,#57751,#57752,#57753,
#57754,#57755,#57756,#57757,#57758,#57759,#57760,#57761,#57762,#57763,#57764,
#57765,#57766,#57767,#57768,#57769,#57770,#57771,#57772,#57773),
 .UNSPECIFIED.,.F.,.F.,(4,2,2,2,2,2,2,2,2,2,2,2,2,2,2,2,2,4),(-5.65305968192749,
-5.62000697109407,-5.56026553634326,-5.50277548740805,-5.4429300395589,
-5.38397497750277,-5.32698226097639,-5.2672900308627,-5.20898363219345,
-5.15141280935565,-5.09150820934248,-5.03387211917237,-4.97460397585247,
-4.91547032791341,-4.8584416373336,-4.79874535977046,-4.74025819094778,
-4.7070192889843),.UNSPECIFIED.);
#3148=B_SPLINE_CURVE_WITH_KNOTS('',3,(#57778,#57779,#57780,#57781,#57782,
#57783,#57784,#57785,#57786,#57787,#57788,#57789,#57790,#57791,#57792,#57793,
#57794,#57795,#57796,#57797,#57798,#57799,#57800,#57801,#57802,#57803,#57804,
#57805,#57806,#57807,#57808,#57809,#57810,#57811,#57812,#57813),
 .UNSPECIFIED.,.F.,.F.,(4,2,2,2,2,2,2,2,2,2,2,2,2,2,2,2,2,4),(-23.6367224740298,
-23.6102009889967,-23.5521597036553,-23.4926417159663,-23.435803856614,
-23.3771146729451,-23.3171085926091,-23.2598611088234,-23.2003772998387,
-23.1424751745089,-23.0845553127723,-23.0249989156642,-22.9680595588619,
-22.9094892557851,-22.8499543793008,-22.7928294928815,-22.7334840265615,
-22.6930944862137),.UNSPECIFIED.);
#3149=B_SPLINE_CURVE_WITH_KNOTS('',3,(#57814,#57815,#57816,#57817,#57818,
#57819,#57820,#57821,#57822,#57823,#57824,#57825,#57826,#57827,#57828,#57829,
#57830,#57831,#57832,#57833,#57834,#57835,#57836,#57837,#57838,#57839,#57840,
#57841,#57842,#57843,#57844,#57845,#57846,#57847,#57848,#57849),
 .UNSPECIFIED.,.F.,.F.,(4,2,2,2,2,2,2,2,2,2,2,2,2,2,2,2,2,4),(-4.7070192889843,
-4.68291221701188,-4.62280788263384,-4.56499211835275,-4.50621920975702,
-4.44687598188547,-4.3897125228076,-4.32998213906469,-4.27128283566224,
-4.21406294394457,-4.15372759490239,-4.09570314650131,-4.03731813708901,
-3.97773968458231,-3.92039439080922,-3.86068740451247,-3.80188610698126,
-3.76030733114506),.UNSPECIFIED.);
#3150=B_SPLINE_CURVE_WITH_KNOTS('',3,(#57854,#57855,#57856,#57857,#57858,
#57859,#57860,#57861,#57862,#57863,#57864,#57865,#57866,#57867,#57868,#57869,
#57870,#57871,#57872,#57873,#57874,#57875,#57876,#57877,#57878,#57879,#57880,
#57881,#57882,#57883,#57884,#57885,#57886,#57887,#57888,#57889),
 .UNSPECIFIED.,.F.,.F.,(4,2,2,2,2,2,2,2,2,2,2,2,2,2,2,2,2,4),(-24.5799045977848,
-24.544864402261,-24.4864680402579,-24.4269448204466,-24.3700449713328,
-24.3110051741305,-24.2521492970098,-24.1946159613695,-24.1348126294181,
-24.0775296073419,-24.0193278864891,-23.9598215850082,-23.9030009070175,
-23.8441534701742,-23.7847543450619,-23.7273819445697,-23.667757974583,
-23.6367224740298),.UNSPECIFIED.);
#3151=B_SPLINE_CURVE_WITH_KNOTS('',3,(#57890,#57891,#57892,#57893,#57894,
#57895,#57896,#57897,#57898,#57899,#57900,#57901,#57902,#57903,#57904,#57905,
#57906,#57907,#57908,#57909,#57910,#57911,#57912,#57913,#57914,#57915,#57916,
#57917,#57918,#57919,#57920,#57921,#57922,#57923,#57924,#57925),
 .UNSPECIFIED.,.F.,.F.,(4,2,2,2,2,2,2,2,2,2,2,2,2,2,2,2,2,4),(-3.76030733114506,
-3.74482173076156,-3.6850983260828,-3.62694832744347,-3.56902286769636,
-3.50929583899485,-3.45181843527126,-3.39189585023894,-3.33295745069471,
-3.27595993809932,-3.21626352613547,-3.15797408399984,-3.1003669659872,
-3.04048156422391,-2.98286252158158,-2.92352507208656,-2.86441225193454,
-2.81422223630842),.UNSPECIFIED.);
#3152=B_SPLINE_CURVE_WITH_KNOTS('',3,(#57930,#57931,#57932,#57933,#57934,
#57935,#57936,#57937,#57938,#57939,#57940,#57941,#57942,#57943,#57944,#57945,
#57946,#57947,#57948,#57949,#57950,#57951,#57952,#57953,#57954,#57955,#57956,
#57957,#57958,#57959,#57960,#57961,#57962,#57963,#57964,#57965),
 .UNSPECIFIED.,.F.,.F.,(4,2,2,2,2,2,2,2,2,2,2,2,2,2,2,2,2,4),(-25.5227587485597,
-25.47965708315,-25.421058174348,-25.361036462416,-25.3038727637219,-25.2444773184052,
-25.1865926949701,-25.128756714116,-25.0692650147963,-25.0123746718861,
-24.9538886316087,-24.8944198504469,-24.8373755091807,-24.7781149174187,
-24.7197080007783,-24.6619822469935,-24.6019654058989,-24.5799045977848),
 .UNSPECIFIED.);
#3153=B_SPLINE_CURVE_WITH_KNOTS('',3,(#57966,#57967,#57968,#57969,#57970,
#57971,#57972,#57973,#57974,#57975,#57976,#57977,#57978,#57979,#57980,#57981,
#57982,#57983,#57984,#57985,#57986,#57987,#57988,#57989,#57990,#57991,#57992,
#57993,#57994,#57995,#57996,#57997,#57998,#57999,#58000,#58001,#58002,#58003),
 .UNSPECIFIED.,.F.,.F.,(4,2,2,2,2,2,2,2,2,2,2,2,2,2,2,2,2,2,4),(-2.81422223630842,
-2.80739059809379,-2.74769363128926,-2.68922759545975,-2.63185666495599,
-2.57177569602702,-2.51398082031509,-2.45515020591261,-2.39583126811454,
-2.3386868262193,-2.27895955966271,-2.22028492138649,-2.16305256653281,
-2.1027441052407,-2.04474383487291,-1.98631516239258,-1.92676386570169,
-1.86944360522889,-1.86759610747369),.UNSPECIFIED.);
#3154=B_SPLINE_CURVE_WITH_KNOTS('',3,(#58008,#58009,#58010,#58011,#58012,
#58013,#58014,#58015,#58016,#58017,#58018,#58019,#58020,#58021,#58022,#58023,
#58024,#58025,#58026,#58027,#58028,#58029,#58030,#58031,#58032,#58033,#58034,
#58035,#58036,#58037,#58038,#58039,#58040,#58041,#58042,#58043),
 .UNSPECIFIED.,.F.,.F.,(4,2,2,2,2,2,2,2,2,2,2,2,2,2,2,2,2,4),(-26.4647006629411,
-26.4128164821547,-26.3538770628634,-26.295021282913,-26.2375822529352,
-26.1778787398139,-26.1206318744523,-26.0625253754812,-26.0030911980923,
-25.9463425849355,-25.8875908503495,-25.8281815100278,-25.7708984260118,
-25.7113688412011,-25.6538368035759,-25.595885334023,-25.5364356344578,
-25.5227587485597),.UNSPECIFIED.);
#3155=B_SPLINE_CURVE_WITH_KNOTS('',3,(#58044,#58045,#58046,#58047,#58048,
#58049,#58050,#58051,#58052,#58053,#58054,#58055,#58056,#58057,#58058,#58059,
#58060,#58061,#58062,#58063,#58064,#58065,#58066,#58067,#58068,#58069,#58070,
#58071,#58072,#58073,#58074,#58075,#58076,#58077,#58078,#58079),
 .UNSPECIFIED.,.F.,.F.,(4,2,2,2,2,2,2,2,2,2,2,2,2,2,2,2,2,4),(-1.86759610747369,
-1.8097465170722,-1.7509722323765,-1.69390716991027,-1.63419213717573,-1.57606932036452,
-1.51811407870063,-1.45841685307261,-1.40096694869804,-1.34098343757821,
-1.28207692999559,-1.22508871615811,-1.16540388332849,-1.10714645181714,
-1.0495176707267,-0.989666932708261,-0.932079853846146,-0.921606618540025),
 .UNSPECIFIED.);
#3156=B_SPLINE_CURVE_WITH_KNOTS('',3,(#58085,#58086,#58087,#58088,#58089,
#58090,#58091,#58092,#58093,#58094,#58095,#58096,#58097,#58098,#58099,#58100,
#58101,#58102,#58103,#58104),.UNSPECIFIED.,.F.,.F.,(4,2,2,2,2,2,2,2,2,4),
(9.99987117032003E-7,0.0282047267175922,0.0500972781633209,0.077222937740314,
0.107624298477487,0.137340418712146,0.157932276880896,0.175135732483776,
0.191462844907497,0.203440126186273),.UNSPECIFIED.);
#3157=B_SPLINE_CURVE_WITH_KNOTS('',3,(#58110,#58111,#58112,#58113,#58114,
#58115,#58116,#58117),.UNSPECIFIED.,.F.,.F.,(4,2,2,4),(21.4315064013737,
21.4634357935859,21.4930318613417,21.5226265917604),.UNSPECIFIED.);
#3158=B_SPLINE_CURVE_WITH_KNOTS('',3,(#58123,#58124,#58125,#58126,#58127,
#58128,#58129,#58130,#58131,#58132,#58133,#58134,#58135,#58136,#58137,#58138,
#58139,#58140,#58141,#58142,#58143,#58144,#58145,#58146,#58147,#58148,#58149,
#58150,#58151,#58152,#58153,#58154,#58155,#58156,#58157,#58158),
 .UNSPECIFIED.,.F.,.F.,(4,2,2,2,2,2,2,2,2,2,2,2,2,2,2,2,2,4),(20.6936878716818,
20.7322285263897,20.7783057175789,20.8227795047066,20.8693557730982,20.9149428892879,
20.9597524851927,21.0065846852777,21.0516438851204,21.0976519395239,21.1438788790039,
21.188432473727,21.2350392941589,21.2807854576605,21.3254925240272,21.3724982892632,
21.417717724476,21.4315064013737),.UNSPECIFIED.);
#3159=B_SPLINE_CURVE_WITH_KNOTS('',3,(#58159,#58160,#58161,#58162,#58163,
#58164,#58165,#58166,#58167,#58168,#58169,#58170,#58171,#58172,#58173,#58174,
#58175,#58176,#58177,#58178,#58179,#58180,#58181,#58182,#58183,#58184,#58185,
#58186,#58187,#58188,#58189,#58190,#58191,#58192,#58193,#58194),
 .UNSPECIFIED.,.F.,.F.,(4,2,2,2,2,2,2,2,2,2,2,2,2,2,2,2,2,4),(9.99999999753597E-7,
0.0364903991492045,0.0742057367939146,0.120984278340417,0.165716260437277,
0.212135354668823,0.258243398942271,0.303486376579508,0.350510827449709,
0.395451299070227,0.441223703670797,0.487964967533294,0.532602258835938,
0.578864855147042,0.625329100321987,0.670440021753448,0.717320863549735,
0.740262878339932),.UNSPECIFIED.);
#3160=B_SPLINE_CURVE_WITH_KNOTS('',3,(#58199,#58200,#58201,#58202,#58203,
#58204,#58205,#58206,#58207,#58208,#58209,#58210,#58211,#58212,#58213,#58214,
#58215,#58216,#58217,#58218,#58219,#58220,#58221,#58222,#58223,#58224,#58225,
#58226,#58227,#58228,#58229,#58230,#58231,#58232,#58233,#58234),
 .UNSPECIFIED.,.F.,.F.,(4,2,2,2,2,2,2,2,2,2,2,2,2,2,2,2,2,4),(19.9559680414516,
20.0008504784901,20.0467368410681,20.0912761832143,20.1378918451635,20.1832739295335,
20.2285046006904,20.275104513086,20.3199511087905,20.366754624975,20.4127173643503,
20.4571887454312,20.5037686894442,20.5492336658488,20.5942218762843,20.6409180608554,
20.6858523218674,20.6936878716818),.UNSPECIFIED.);
#3161=B_SPLINE_CURVE_WITH_KNOTS('',3,(#58235,#58236,#58237,#58238,#58239,
#58240,#58241,#58242,#58243,#58244,#58245,#58246,#58247,#58248,#58249,#58250,
#58251,#58252,#58253,#58254,#58255,#58256,#58257,#58258,#58259,#58260,#58261,
#58262,#58263,#58264,#58265,#58266,#58267,#58268,#58269,#58270),
 .UNSPECIFIED.,.F.,.F.,(4,2,2,2,2,2,2,2,2,2,2,2,2,2,2,2,2,4),(0.740262878339932,
0.762427102215096,0.808069985401053,0.854808846272841,0.899429812570394,
0.945570872042072,0.992454683227221,1.03747065146669,1.08424743869661,1.12958660656193,
1.175138889682,1.22190780149668,1.26658471043468,1.31264188421903,1.35939848501362,
1.4043392205548,1.45103260193205,1.48067239646651),.UNSPECIFIED.);
#3162=B_SPLINE_CURVE_WITH_KNOTS('',3,(#58275,#58276,#58277,#58278,#58279,
#58280,#58281,#58282,#58283,#58284,#58285,#58286,#58287,#58288,#58289,#58290,
#58291,#58292,#58293,#58294,#58295,#58296,#58297,#58298,#58299,#58300,#58301,
#58302,#58303,#58304,#58305,#58306,#58307,#58308,#58309,#58310,#58311,#58312),
 .UNSPECIFIED.,.F.,.F.,(4,2,2,2,2,2,2,2,2,2,2,2,2,2,2,2,2,2,4),(19.2175408288878,
19.2219373965907,19.2685210725085,19.3141891378125,19.3589248216993,19.4058460198647,
19.4509870738391,19.4968133764095,19.5431350504829,19.5877640910998,19.6343990565288,
19.6802461513431,19.72492597093,19.7720411959568,19.8173618084826,19.8629496498953,
19.9094715861334,19.954248068259,19.9559680414516),.UNSPECIFIED.);
#3163=B_SPLINE_CURVE_WITH_KNOTS('',3,(#58313,#58314,#58315,#58316,#58317,
#58318,#58319,#58320,#58321,#58322,#58323,#58324,#58325,#58326,#58327,#58328,
#58329,#58330,#58331,#58332,#58333,#58334,#58335,#58336,#58337,#58338,#58339,
#58340,#58341,#58342,#58343,#58344,#58345,#58346,#58347,#58348),
 .UNSPECIFIED.,.F.,.F.,(4,2,2,2,2,2,2,2,2,2,2,2,2,2,2,2,2,4),(1.48067239646651,
1.49671326012625,1.54219831558785,1.5894859449329,1.63428944893413,1.68030245144421,
1.72708174969527,1.77186789842175,1.81835464146615,1.86425678940839,1.90955548631379,
1.95664189809396,2.00148568453804,2.0473126858144,2.0940334671172,2.13867975719358,
2.18499121801513,2.22108960850334),.UNSPECIFIED.);
#3164=B_SPLINE_CURVE_WITH_KNOTS('',3,(#58353,#58354,#58355,#58356,#58357,
#58358,#58359,#58360,#58361,#58362,#58363,#58364,#58365,#58366,#58367,#58368,
#58369,#58370,#58371,#58372,#58373,#58374,#58375,#58376,#58377,#58378,#58379,
#58380,#58381,#58382,#58383,#58384,#58385,#58386,#58387,#58388),
 .UNSPECIFIED.,.F.,.F.,(4,2,2,2,2,2,2,2,2,2,2,2,2,2,2,2,2,4),(18.4801374015765,
18.4907658335562,18.5373515680576,18.5827705444335,18.6278503823358,18.6744946234866,
18.7193811539994,18.7659288026933,18.8119468369207,18.8564049550709,18.9029730508313,
18.9484975984601,18.9933693854802,19.0401328543241,19.0851285772229,19.1312801323088,
19.1774331204032,19.2175408288878),.UNSPECIFIED.);
#3165=B_SPLINE_CURVE_WITH_KNOTS('',3,(#58389,#58390,#58391,#58392,#58393,
#58394,#58395,#58396,#58397,#58398,#58399,#58400,#58401,#58402,#58403,#58404,
#58405,#58406,#58407,#58408,#58409,#58410,#58411,#58412,#58413,#58414,#58415,
#58416,#58417,#58418,#58419,#58420,#58421,#58422,#58423,#58424),
 .UNSPECIFIED.,.F.,.F.,(4,2,2,2,2,2,2,2,2,2,2,2,2,2,2,2,2,4),(2.22108960850334,
2.23120408655543,2.27635041769103,2.32327161206725,2.368237212408,2.41391337637609,
2.46061197050217,2.50519713949817,2.5513666691862,2.59796482416004,2.64299465171328,
2.68978881476098,2.73495033654449,2.78051325760178,2.82722340804027,2.87182391079689,
2.91788757586549,2.96056667106229),.UNSPECIFIED.);
#3166=B_SPLINE_CURVE_WITH_KNOTS('',3,(#58429,#58430,#58431,#58432,#58433,
#58434,#58435,#58436,#58437,#58438,#58439,#58440,#58441,#58442,#58443,#58444,
#58445,#58446,#58447,#58448,#58449,#58450,#58451,#58452,#58453,#58454,#58455,
#58456,#58457,#58458,#58459,#58460,#58461,#58462,#58463,#58464),
 .UNSPECIFIED.,.F.,.F.,(4,2,2,2,2,2,2,2,2,2,2,2,2,2,2,2,2,4),(17.7416164546727,
17.7581937026132,17.8052897667917,17.8505949548622,17.8963342504639,17.9428341472151,
17.9875910340227,18.0342105180494,18.0800707723051,18.124652551507,18.1712871824617,
18.2166406572815,18.2619848045744,18.3085503929415,18.3533657882032,18.4003592098579,
18.446278791736,18.4801374015765),.UNSPECIFIED.);
#3167=B_SPLINE_CURVE_WITH_KNOTS('',3,(#58465,#58466,#58467,#58468,#58469,
#58470,#58471,#58472,#58473,#58474,#58475,#58476,#58477,#58478,#58479,#58480,
#58481,#58482,#58483,#58484,#58485,#58486,#58487,#58488,#58489,#58490,#58491,
#58492,#58493,#58494,#58495,#58496,#58497,#58498,#58499,#58500,#58501,#58502),
 .UNSPECIFIED.,.F.,.F.,(4,2,2,2,2,2,2,2,2,2,2,2,2,2,2,2,2,2,4),(2.96056667106229,
2.96492507840458,3.00987622748865,3.05658369115965,3.10200096713613,3.14749048109044,
3.19424386894225,3.23892780465305,3.28492439308362,3.33166335864177,3.3765506531,
3.42318675517329,3.46898366970959,3.51441887461108,3.56165143931351,3.60649480370264,
3.65245839321213,3.69924258617203,3.70124435567),.UNSPECIFIED.);
#3168=B_SPLINE_CURVE_WITH_KNOTS('',3,(#58507,#58508,#58509,#58510,#58511,
#58512,#58513,#58514,#58515,#58516,#58517,#58518,#58519,#58520,#58521,#58522,
#58523,#58524,#58525,#58526,#58527,#58528,#58529,#58530,#58531,#58532,#58533,
#58534,#58535,#58536,#58537,#58538,#58539,#58540,#58541,#58542),
 .UNSPECIFIED.,.F.,.F.,(4,2,2,2,2,2,2,2,2,2,2,2,2,2,2,2,2,4),(17.002935008964,
17.0259159067871,17.0726902796453,17.117698909592,17.1640720079207,17.2102290646699,
17.2547667636235,17.301404789293,17.3470724875982,17.391917818806,17.4388344123328,
17.4839738011972,17.5299894371059,17.5763017108472,17.6209316820209,17.6676058954979,
17.7134384045876,17.7416164546727),.UNSPECIFIED.);
#3169=B_SPLINE_CURVE_WITH_KNOTS('',3,(#58543,#58544,#58545,#58546,#58547,
#58548,#58549,#58550,#58551,#58552,#58553,#58554,#58555,#58556,#58557,#58558,
#58559,#58560,#58561,#58562,#58563,#58564,#58565,#58566,#58567,#58568,#58569,
#58570,#58571,#58572,#58573,#58574,#58575,#58576,#58577,#58578),
 .UNSPECIFIED.,.F.,.F.,(4,2,2,2,2,2,2,2,2,2,2,2,2,2,2,2,2,4),(3.70124435567,
3.74399270352421,3.79043516379055,3.83649298289209,3.88175593971899,3.92880219425985,
3.97372113000247,4.01951325018307,4.0662546751028,4.11089815702418,4.15717909203302,
4.20358177465394,4.24870726106109,4.29560414076508,4.34067748019848,4.38633433906348,
4.43306819834531,4.44139309323576),.UNSPECIFIED.);
#3170=B_SPLINE_CURVE_WITH_KNOTS('',3,(#58583,#58584,#58585,#58586,#58587,
#58588,#58589,#58590,#58591,#58592,#58593,#58594,#58595,#58596,#58597,#58598,
#58599,#58600,#58601,#58602,#58603,#58604,#58605,#58606,#58607,#58608,#58609,
#58610,#58611,#58612,#58613,#58614,#58615,#58616,#58617,#58618),
 .UNSPECIFIED.,.F.,.F.,(4,2,2,2,2,2,2,2,2,2,2,2,2,2,2,2,2,4),(16.2641372477882,
16.2938030439013,16.3403922128616,16.3852327649267,16.4318876926505,16.4778418228271,
16.5224230010358,16.5690903677485,16.6145405429621,16.6597873151308,16.7064589317587,
16.7513738187352,16.7981669545333,16.8442036947422,16.8887271733991,16.9353636748532,
16.9809031318305,17.002935008964),.UNSPECIFIED.);
#3171=B_SPLINE_CURVE_WITH_KNOTS('',3,(#58619,#58620,#58621,#58622,#58623,
#58624,#58625,#58626,#58627,#58628,#58629,#58630,#58631,#58632,#58633,#58634,
#58635,#58636,#58637,#58638,#58639,#58640,#58641,#58642,#58643,#58644,#58645,
#58646,#58647,#58648,#58649,#58650,#58651,#58652,#58653,#58654),
 .UNSPECIFIED.,.F.,.F.,(4,2,2,2,2,2,2,2,2,2,2,2,2,2,2,2,2,4),(4.44139309323576,
4.47768369479005,4.52383758291686,4.57065155177945,4.61567630686354,4.66246297203597,
4.70776020748785,4.7533204420323,4.80007956137218,4.8447406734777,4.8908048094463,
4.93755248955131,4.98249808878681,5.02919719884178,5.0748218415068,5.12031038865077,
5.16760288129374,5.1818539671131),.UNSPECIFIED.);
#3172=B_SPLINE_CURVE_WITH_KNOTS('',3,(#58659,#58660,#58661,#58662,#58663,
#58664,#58665,#58666,#58667,#58668,#58669,#58670,#58671,#58672,#58673,#58674,
#58675,#58676,#58677,#58678,#58679,#58680,#58681,#58682,#58683,#58684,#58685,
#58686,#58687,#58688,#58689,#58690,#58691,#58692,#58693,#58694),
 .UNSPECIFIED.,.F.,.F.,(4,2,2,2,2,2,2,2,2,2,2,2,2,2,2,2,2,4),(15.5253008226521,
15.5614208712953,15.6076307463169,15.6521806514462,15.6988024510405,15.7445285973342,
15.7892808885852,15.8362633798431,15.8814623032694,15.9272761463232,15.9736600003967,
16.0183472154503,16.0650263145743,16.1109370835491,16.1556467547297,16.2028290254408,
16.2482129532865,16.2641372477882),.UNSPECIFIED.);
#3173=B_SPLINE_CURVE_WITH_KNOTS('',3,(#58695,#58696,#58697,#58698,#58699,
#58700,#58701,#58702,#58703,#58704,#58705,#58706,#58707,#58708,#58709,#58710,
#58711,#58712,#58713,#58714,#58715,#58716,#58717,#58718,#58719,#58720,#58721,
#58722,#58723,#58724,#58725,#58726,#58727,#58728,#58729,#58730),
 .UNSPECIFIED.,.F.,.F.,(4,2,2,2,2,2,2,2,2,2,2,2,2,2,2,2,2,4),(5.1818539671131,
5.21237880454505,5.258394968262,5.30515700825967,5.34994371692685,5.39643143835995,
5.44226233196025,5.48755936077848,5.53464520113254,5.57944804045745,5.62527291369698,
5.67197040786348,5.71660500923211,5.76291244064308,5.80904038797896,5.85417959966551,
5.90109443452282,5.92163532828753),.UNSPECIFIED.);
#3174=B_SPLINE_CURVE_WITH_KNOTS('',3,(#58735,#58736,#58737,#58738,#58739,
#58740,#58741,#58742,#58743,#58744,#58745,#58746,#58747,#58748,#58749,#58750,
#58751,#58752,#58753,#58754,#58755,#58756,#58757,#58758,#58759,#58760,#58761,
#58762,#58763,#58764,#58765,#58766,#58767,#58768,#58769,#58770),
 .UNSPECIFIED.,.F.,.F.,(4,2,2,2,2,2,2,2,2,2,2,2,2,2,2,2,2,4),(14.7873695620709,
14.8300506862385,14.8760153817406,14.9205240016754,14.9671371535707,15.0126019576596,
15.0576755801971,15.1043686547149,15.149301357282,15.1958140370104,15.2418832855322,
15.286374482974,15.3329751561295,15.3785518380475,15.4234279626835,15.4702466599603,
15.5152945505239,15.5253008226521),.UNSPECIFIED.);
#3175=B_SPLINE_CURVE_WITH_KNOTS('',3,(#58771,#58772,#58773,#58774,#58775,
#58776,#58777,#58778,#58779,#58780,#58781,#58782,#58783,#58784,#58785,#58786,
#58787,#58788,#58789,#58790,#58791,#58792,#58793,#58794,#58795,#58796,#58797,
#58798,#58799,#58800,#58801,#58802,#58803,#58804,#58805,#58806),
 .UNSPECIFIED.,.F.,.F.,(4,2,2,2,2,2,2,2,2,2,2,2,2,2,2,2,2,4),(5.92163532828753,
5.94600637034905,5.99167472503286,6.03834442621258,6.08290534138804,6.12906543193699,
6.17556776582538,6.22058468374404,6.26736631647045,6.31246290290152,6.358011917132,
6.40468792773244,6.44925237282631,6.4953007135921,6.54223498706927,6.58716711269207,
6.63385553062737,6.66068791027176),.UNSPECIFIED.);
#3176=B_SPLINE_CURVE_WITH_KNOTS('',3,(#58811,#58812,#58813,#58814,#58815,
#58816,#58817,#58818,#58819,#58820,#58821,#58822,#58823,#58824,#58825,#58826,
#58827,#58828,#58829,#58830,#58831,#58832,#58833,#58834,#58835,#58836,#58837,
#58838,#58839,#58840,#58841,#58842,#58843,#58844,#58845,#58846,#58847,#58848),
 .UNSPECIFIED.,.F.,.F.,(4,2,2,2,2,2,2,2,2,2,2,2,2,2,2,2,2,2,4),(14.0482100339955,
14.0502949245492,14.096984232057,14.142851009537,14.1876060347159,14.2347388331608,
14.2800782706825,14.3257899974572,14.3723273782223,14.41711976203,14.463762437258,
14.5096613573186,14.55425504223,14.6009122351073,14.6463049690835,14.6916352778898,
14.7382430334376,14.7830983471007,14.7873695620709),.UNSPECIFIED.);
#3177=B_SPLINE_CURVE_WITH_KNOTS('',3,(#58849,#58850,#58851,#58852,#58853,
#58854,#58855,#58856,#58857,#58858,#58859,#58860,#58861,#58862,#58863,#58864,
#58865,#58866,#58867,#58868,#58869,#58870,#58871,#58872,#58873,#58874,#58875,
#58876,#58877,#58878,#58879,#58880,#58881,#58882,#58883,#58884),
 .UNSPECIFIED.,.F.,.F.,(4,2,2,2,2,2,2,2,2,2,2,2,2,2,2,2,2,4),(6.66068791027176,
6.67919937428358,6.72466854077273,6.77138281680808,6.8160205136328,6.86199546468963,
6.90869606620136,6.95356006101863,7.00017259357045,7.04588152905359,7.09129151458587,
7.13849904618301,7.1832836822818,7.22922137847032,7.27595882272717,7.32067836819823,
7.3670926336791,7.40074313214862),.UNSPECIFIED.);
#3178=B_SPLINE_CURVE_WITH_KNOTS('',3,(#58889,#58890,#58891,#58892,#58893,
#58894,#58895,#58896,#58897,#58898,#58899,#58900,#58901,#58902,#58903,#58904,
#58905,#58906,#58907,#58908,#58909,#58910,#58911,#58912,#58913,#58914,#58915,
#58916,#58917,#58918,#58919,#58920,#58921,#58922,#58923,#58924),
 .UNSPECIFIED.,.F.,.F.,(4,2,2,2,2,2,2,2,2,2,2,2,2,2,2,2,2,4),(13.3095464675158,
13.3179418806692,13.3645829204745,13.4101456027589,13.4551345123131,13.5019343594699,
13.5469666402861,13.5932875705783,13.6394722908042,13.6840250076321,13.7306726518614,
13.7763692796775,13.8212020202917,13.8681498816812,13.9133183606713,13.9592929931832,
14.0056379903772,14.0482100339955),.UNSPECIFIED.);
#3179=B_SPLINE_CURVE_WITH_KNOTS('',3,(#58925,#58926,#58927,#58928,#58929,
#58930,#58931,#58932,#58933,#58934,#58935,#58936,#58937,#58938,#58939,#58940,
#58941,#58942,#58943,#58944,#58945,#58946,#58947,#58948,#58949,#58950,#58951,
#58952,#58953,#58954,#58955,#58956,#58957,#58958,#58959,#58960),
 .UNSPECIFIED.,.F.,.F.,(4,2,2,2,2,2,2,2,2,2,2,2,2,2,2,2,2,4),(7.40074313214862,
7.41304791193527,7.45828058796883,7.50529645981043,7.55014367964178,7.59590467610001,
7.64259365979734,7.68719438829927,7.73344217485688,7.77972977945611,7.82481959518803,
7.87168035903332,7.91667006179515,7.96229014337893,8.00896624300127,8.05352690669973,
8.09964223179755,8.13994719566162),.UNSPECIFIED.);
#3180=B_SPLINE_CURVE_WITH_KNOTS('',3,(#58965,#58966,#58967,#58968,#58969,
#58970,#58971,#58972,#58973,#58974,#58975,#58976,#58977,#58978,#58979,#58980,
#58981,#58982,#58983,#58984,#58985,#58986,#58987,#58988,#58989,#58990,#58991,
#58992,#58993,#58994,#58995,#58996,#58997,#58998,#58999,#59000),
 .UNSPECIFIED.,.F.,.F.,(4,2,2,2,2,2,2,2,2,2,2,2,2,2,2,2,2,4),(12.5705412100685,
12.5848546363202,12.6320513419363,12.6774479779185,12.7229914291377,12.7695957874756,
12.8144503148156,12.8611058709474,12.9070763074098,12.951650697705,12.9983178350321,
13.0437851961517,13.0889992823918,13.1356902587469,13.1806230630583,13.2273560115123,
13.2734149408359,13.3095464675158),.UNSPECIFIED.);
#3181=B_SPLINE_CURVE_WITH_KNOTS('',3,(#59001,#59002,#59003,#59004,#59005,
#59006,#59007,#59008,#59009,#59010,#59011,#59012,#59013,#59014,#59015,#59016,
#59017,#59018,#59019,#59020,#59021,#59022,#59023,#59024,#59025,#59026,#59027,
#59028,#59029,#59030,#59031,#59032,#59033,#59034,#59035,#59036,#59037,#59038),
 .UNSPECIFIED.,.F.,.F.,(4,2,2,2,2,2,2,2,2,2,2,2,2,2,2,2,2,2,4),(8.13994719566162,
8.1463316268328,8.19131496388372,8.2380593874591,8.28326280667136,8.33020598996195,
8.37537161294956,8.42146167930536,8.46779890512908,8.51245656585315,8.55916791039741,
8.60502388501555,8.64982522039719,8.69694438308839,8.7422725099988,8.78807715134522,
8.83459899420235,8.87937738670119,8.87958134265245),.UNSPECIFIED.);
#3182=B_SPLINE_CURVE_WITH_KNOTS('',3,(#59043,#59044,#59045,#59046,#59047,
#59048,#59049,#59050,#59051,#59052,#59053,#59054,#59055,#59056,#59057,#59058,
#59059,#59060,#59061,#59062,#59063,#59064,#59065,#59066,#59067,#59068,#59069,
#59070,#59071,#59072,#59073,#59074,#59075,#59076,#59077,#59078),
 .UNSPECIFIED.,.F.,.F.,(4,2,2,2,2,2,2,2,2,2,2,2,2,2,2,2,2,4),(11.8321815561307,
11.8527802750529,11.8996021687833,11.9446521456017,11.9907033317147,12.0369186139489,
12.0814657613186,12.1280739153687,12.1738072480122,12.2185277557899,12.2655192350349,
12.3107256977114,12.3564778448273,12.4028721237148,12.4475687949672,12.4942402335744,
12.5401634891127,12.5705412100685),.UNSPECIFIED.);
#3183=B_SPLINE_CURVE_WITH_KNOTS('',3,(#59079,#59080,#59081,#59082,#59083,
#59084,#59085,#59086,#59087,#59088,#59089,#59090,#59091,#59092,#59093,#59094,
#59095,#59096,#59097,#59098,#59099,#59100,#59101,#59102,#59103,#59104,#59105,
#59106,#59107,#59108,#59109,#59110,#59111,#59112,#59113,#59114),
 .UNSPECIFIED.,.F.,.F.,(4,2,2,2,2,2,2,2,2,2,2,2,2,2,2,2,2,4),(8.87958134265245,
8.92602852613987,8.97190922554665,9.01652860508801,9.06319528540556,9.10856829663463,
9.15396816684055,9.20055253946269,9.24538645185148,9.29245567553163,9.33839133852289,
9.38290947461184,9.42952391977244,9.47495799934766,9.52008834525836,9.56674688093536,
9.6116477128901,9.61793661341104),.UNSPECIFIED.);
#3184=B_SPLINE_CURVE_WITH_KNOTS('',3,(#59119,#59120,#59121,#59122,#59123,
#59124,#59125,#59126,#59127,#59128,#59129,#59130,#59131,#59132,#59133,#59134,
#59135,#59136,#59137,#59138,#59139,#59140,#59141,#59142,#59143,#59144,#59145,
#59146,#59147,#59148,#59149,#59150,#59151,#59152,#59153,#59154),
 .UNSPECIFIED.,.F.,.F.,(4,2,2,2,2,2,2,2,2,2,2,2,2,2,2,2,2,4),(11.0945157929649,
11.1213867420797,11.1679850354348,11.212830558321,11.2596899586864,11.3056487691199,
11.3501304725593,11.3967192229775,11.4421794409724,11.4871976310158,11.5338877382452,
11.5788167443302,11.6252436424475,11.6713128846608,11.7157888443594,11.7623703136435,
11.8079484981885,11.8321815561307),.UNSPECIFIED.);
#3185=B_SPLINE_CURVE_WITH_KNOTS('',3,(#59155,#59156,#59157,#59158,#59159,
#59160,#59161,#59162,#59163,#59164,#59165,#59166,#59167,#59168,#59169,#59170,
#59171,#59172,#59173,#59174,#59175,#59176,#59177,#59178,#59179,#59180,#59181,
#59182,#59183,#59184,#59185,#59186,#59187,#59188,#59189,#59190),
 .UNSPECIFIED.,.F.,.F.,(4,2,2,2,2,2,2,2,2,2,2,2,2,2,2,2,2,4),(9.61793661341104,
9.65826687912693,9.70429689093938,9.74877836477337,9.79537166131895,9.84090708321871,
9.88582218876157,9.93259567749554,9.97760169196064,10.0238180381891,10.0699792278232,
10.1144983947581,10.1611035398683,10.2067785301348,10.2515491657397,10.2984763720027,
10.3436239452287,10.3558181882677),.UNSPECIFIED.);
#3186=B_SPLINE_CURVE_WITH_KNOTS('',3,(#59195,#59196,#59197,#59198,#59199,
#59200,#59201,#59202,#59203,#59204,#59205,#59206,#59207,#59208,#59209,#59210,
#59211,#59212,#59213,#59214,#59215,#59216,#59217,#59218,#59219,#59220,#59221,
#59222,#59223,#59224,#59225,#59226,#59227,#59228,#59229,#59230),
 .UNSPECIFIED.,.F.,.F.,(4,2,2,2,2,2,2,2,2,2,2,2,2,2,2,2,2,4),(10.3558181865992,
10.3895062288278,10.4358326314552,10.4804680791543,10.5271205064737,10.5729708577389,
10.6176765737363,10.6647940480184,10.710117621532,10.7557512885806,10.8022746889798,
10.8470530120057,10.8936670905081,10.9395538338801,10.9841105681321,11.0307384394129,
11.0761201700909,11.0945157929649),.UNSPECIFIED.);
#3187=B_SPLINE_CURVE_WITH_KNOTS('',3,(#59231,#59232,#59233,#59234,#59235,
#59236,#59237,#59238,#59239,#59240,#59241,#59242,#59243,#59244,#59245,#59246,
#59247,#59248,#59249,#59250,#59251,#59252,#59253,#59254,#59255,#59256,#59257,
#59258,#59259,#59260,#59261,#59262,#59263,#59264,#59265,#59266),
 .UNSPECIFIED.,.F.,.F.,(4,2,2,2,2,2,2,2,2,2,2,2,2,2,2,2,2,4),(10.3558181882677,
10.3895062304569,10.4358326331012,10.4804680808162,10.5271205081509,10.572970859433,
10.6176765754436,10.6647940497431,10.7101176232735,10.7557512903329,10.8022746907493,
10.8470530137919,10.8936670923103,10.9395538356998,10.9841105699663,11.0307384412633,
11.0761201719588,11.0945157948807),.UNSPECIFIED.);
#3188=B_SPLINE_CURVE_WITH_KNOTS('',3,(#59271,#59272,#59273,#59274,#59275,
#59276,#59277,#59278,#59279,#59280,#59281,#59282,#59283,#59284,#59285,#59286,
#59287,#59288,#59289,#59290,#59291,#59292,#59293,#59294,#59295,#59296,#59297,
#59298,#59299,#59300,#59301,#59302,#59303,#59304,#59305,#59306),
 .UNSPECIFIED.,.F.,.F.,(4,2,2,2,2,2,2,2,2,2,2,2,2,2,2,2,2,4),(9.61793661197057,
9.65826687772365,9.7042968895204,9.74877836334091,9.79537165987244,9.84090708175655,
9.88582218728856,9.93259567600637,9.977601690456,10.0238180366761,10.069979226294,
10.1144983932143,10.16110353831,10.2067785285603,10.2515491641532,10.2984763703993,
10.3436239436092,10.3558181865992),.UNSPECIFIED.);
#3189=B_SPLINE_CURVE_WITH_KNOTS('',3,(#59307,#59308,#59309,#59310,#59311,
#59312,#59313,#59314,#59315,#59316,#59317,#59318,#59319,#59320,#59321,#59322,
#59323,#59324,#59325,#59326,#59327,#59328,#59329,#59330,#59331,#59332,#59333,
#59334,#59335,#59336,#59337,#59338,#59339,#59340,#59341,#59342),
 .UNSPECIFIED.,.F.,.F.,(4,2,2,2,2,2,2,2,2,2,2,2,2,2,2,2,2,4),(11.0945157948807,
11.1213867439599,11.1679850373331,11.2128305602366,11.2596899606121,11.3056487710637,
11.3501304745185,11.3967192249533,11.4421794429662,11.4871976330225,11.5338877402705,
11.5788167463733,11.625243644501,11.6713128867326,11.7157888464474,11.762370315748,
11.8079485003112,11.8321815583089),.UNSPECIFIED.);
#3190=B_SPLINE_CURVE_WITH_KNOTS('',3,(#59347,#59348,#59349,#59350,#59351,
#59352,#59353,#59354,#59355,#59356,#59357,#59358,#59359,#59360,#59361,#59362,
#59363,#59364,#59365,#59366,#59367,#59368,#59369,#59370,#59371,#59372,#59373,
#59374,#59375,#59376,#59377,#59378,#59379,#59380,#59381,#59382),
 .UNSPECIFIED.,.F.,.F.,(4,2,2,2,2,2,2,2,2,2,2,2,2,2,2,2,2,4),(8.87958134142251,
8.92602852493827,8.97190922433066,9.01652860386053,9.06319528416507,9.10856829537987,
9.15396816557657,9.20055253818396,9.24538645055861,9.29245567423173,9.33839133720815,
9.38290947328484,9.42952391843202,9.47495799799238,9.5200883438932,9.56674687955462,
9.61164771149445,9.61793661197057),.UNSPECIFIED.);
#3191=B_SPLINE_CURVE_WITH_KNOTS('',3,(#59383,#59384,#59385,#59386,#59387,
#59388,#59389,#59390,#59391,#59392,#59393,#59394,#59395,#59396,#59397,#59398,
#59399,#59400,#59401,#59402,#59403,#59404,#59405,#59406,#59407,#59408,#59409,
#59410,#59411,#59412,#59413,#59414,#59415,#59416,#59417,#59418),
 .UNSPECIFIED.,.F.,.F.,(4,2,2,2,2,2,2,2,2,2,2,2,2,2,2,2,2,4),(11.8321815583089,
11.8527802771891,11.8996021709384,11.9446521477749,11.9907033338989,12.0369186161519,
12.0814657635389,12.128073917606,12.1738072502682,12.2185277580605,12.2655192373249,
12.31072570002,12.3564778471481,12.402872126055,12.4475687973262,12.4942402359512,
12.5401634915089,12.5705412125212),.UNSPECIFIED.);
#3192=B_SPLINE_CURVE_WITH_KNOTS('',3,(#59423,#59424,#59425,#59426,#59427,
#59428,#59429,#59430,#59431,#59432,#59433,#59434,#59435,#59436,#59437,#59438,
#59439,#59440,#59441,#59442,#59443,#59444,#59445,#59446,#59447,#59448,#59449,
#59450,#59451,#59452,#59453,#59454,#59455,#59456,#59457,#59458,#59459,#59460),
 .UNSPECIFIED.,.F.,.F.,(4,2,2,2,2,2,2,2,2,2,2,2,2,2,2,2,2,2,4),(8.13994719462425,
8.14633162583834,8.19131496287961,8.23805938644507,8.28326280564246,8.33020598891935,
8.37537161189387,8.42146167824292,8.46779890405304,8.51245656476452,8.55916790929672,
8.60502388390122,8.64982521927269,8.69694438194964,8.74227250884644,8.78807715018487,
8.83459899302762,8.87937738551268,8.87958134142251),.UNSPECIFIED.);
#3193=B_SPLINE_CURVE_WITH_KNOTS('',3,(#59461,#59462,#59463,#59464,#59465,
#59466,#59467,#59468,#59469,#59470,#59471,#59472,#59473,#59474,#59475,#59476,
#59477,#59478,#59479,#59480,#59481,#59482,#59483,#59484,#59485,#59486,#59487,
#59488,#59489,#59490,#59491,#59492,#59493,#59494,#59495,#59496),
 .UNSPECIFIED.,.F.,.F.,(4,2,2,2,2,2,2,2,2,2,2,2,2,2,2,2,2,4),(12.5705412125212,
12.5848546387325,12.6320513443688,12.6774479803703,12.7229914316032,12.7695957899609,
12.81445031732,12.8611058734703,12.9070763099523,12.9516507002645,12.99831783761,
13.0437851987491,13.0889992850039,13.1356902613794,13.1806230657103,13.2273560141773,
13.2734149435215,13.3095464702606),.UNSPECIFIED.);
#3194=B_SPLINE_CURVE_WITH_KNOTS('',3,(#59501,#59502,#59503,#59504,#59505,
#59506,#59507,#59508,#59509,#59510,#59511,#59512,#59513,#59514,#59515,#59516,
#59517,#59518,#59519,#59520,#59521,#59522,#59523,#59524,#59525,#59526,#59527,
#59528,#59529,#59530,#59531,#59532,#59533,#59534,#59535,#59536),
 .UNSPECIFIED.,.F.,.F.,(4,2,2,2,2,2,2,2,2,2,2,2,2,2,2,2,2,4),(7.4007431312885,
7.41304791111891,7.45828058714382,7.50529645897655,7.55014367879521,7.59590467524459,
7.64259365893083,7.68719438742294,7.73344217397141,7.7797297785534,7.82481959427612,
7.87168035811193,7.91667006085986,7.96229014243438,8.00896624204524,8.05352690573283,
8.09964223082121,8.13994719462425),.UNSPECIFIED.);
#3195=B_SPLINE_CURVE_WITH_KNOTS('',3,(#59537,#59538,#59539,#59540,#59541,
#59542,#59543,#59544,#59545,#59546,#59547,#59548,#59549,#59550,#59551,#59552,
#59553,#59554,#59555,#59556,#59557,#59558,#59559,#59560,#59561,#59562,#59563,
#59564,#59565,#59566,#59567,#59568,#59569,#59570,#59571,#59572),
 .UNSPECIFIED.,.F.,.F.,(4,2,2,2,2,2,2,2,2,2,2,2,2,2,2,2,2,4),(13.3095464702606,
13.317941883373,13.3645829231975,13.4101456055024,13.4551345150724,13.5019343622502,
13.5469666430868,13.5932875733925,13.6394722936394,13.6840250104865,13.7306726547352,
13.7763692825722,13.8212020232032,13.8681498846145,13.9133183636254,13.9592929961519,
14.0056379933677,14.0482100370503),.UNSPECIFIED.);
#3196=B_SPLINE_CURVE_WITH_KNOTS('',3,(#59577,#59578,#59579,#59580,#59581,
#59582,#59583,#59584,#59585,#59586,#59587,#59588,#59589,#59590,#59591,#59592,
#59593,#59594,#59595,#59596,#59597,#59598,#59599,#59600,#59601,#59602,#59603,
#59604,#59605,#59606,#59607,#59608,#59609,#59610,#59611,#59612),
 .UNSPECIFIED.,.F.,.F.,(4,2,2,2,2,2,2,2,2,2,2,2,2,2,2,2,2,4),(6.66068790957161,
6.67919937362265,6.72466854010414,6.77138281612983,6.81602051294445,6.86199546399339,
6.90869606549543,6.95356006030469,7.00017259284827,7.04588152831696,7.09129151384102,
7.13849904542972,7.18328368151711,7.22922137769738,7.27595882194379,7.32067836740631,
7.36709263287862,7.4007431312885),.UNSPECIFIED.);
#3197=B_SPLINE_CURVE_WITH_KNOTS('',3,(#59613,#59614,#59615,#59616,#59617,
#59618,#59619,#59620,#59621,#59622,#59623,#59624,#59625,#59626,#59627,#59628,
#59629,#59630,#59631,#59632,#59633,#59634,#59635,#59636,#59637,#59638,#59639,
#59640,#59641,#59642,#59643,#59644,#59645,#59646,#59647,#59648,#59649,#59650),
 .UNSPECIFIED.,.F.,.F.,(4,2,2,2,2,2,2,2,2,2,2,2,2,2,2,2,2,2,4),(14.0482100370503,
14.0502949275604,14.0969842350884,14.1428510125903,14.1876060377872,14.2347388362546,
14.2800782737978,14.3257900005883,14.3723273813755,14.4171197652046,14.4637624404534,
14.5096613605359,14.5542550454664,14.6009122383646,14.6463049723626,14.6916352811859,
14.7382430367566,14.7830983504416,14.7873695654535),.UNSPECIFIED.);
#3198=B_SPLINE_CURVE_WITH_KNOTS('',3,(#59655,#59656,#59657,#59658,#59659,
#59660,#59661,#59662,#59663,#59664,#59665,#59666,#59667,#59668,#59669,#59670,
#59671,#59672,#59673,#59674,#59675,#59676,#59677,#59678,#59679,#59680,#59681,
#59682,#59683,#59684,#59685,#59686,#59687,#59688,#59689,#59690),
 .UNSPECIFIED.,.F.,.F.,(4,2,2,2,2,2,2,2,2,2,2,2,2,2,2,2,2,4),(5.92163532773223,
5.94600636983764,5.99167472451486,6.03834442568581,6.08290534085326,6.12906543139539,
6.17556776526837,6.22058468317993,6.26736631589905,6.31246290231792,6.35801191654115,
6.40468792713218,6.44925237221679,6.49530071297518,6.5422349864363,6.58716711205166,
6.6338555299793,6.66068790957161),.UNSPECIFIED.);
#3199=B_SPLINE_CURVE_WITH_KNOTS('',3,(#59691,#59692,#59693,#59694,#59695,
#59696,#59697,#59698,#59699,#59700,#59701,#59702,#59703,#59704,#59705,#59706,
#59707,#59708,#59709,#59710,#59711,#59712,#59713,#59714,#59715,#59716,#59717,
#59718,#59719,#59720,#59721,#59722,#59723,#59724,#59725,#59726),
 .UNSPECIFIED.,.F.,.F.,(4,2,2,2,2,2,2,2,2,2,2,2,2,2,2,2,2,4),(14.7873695654535,
14.8300506895943,14.8760153851188,14.9205240050731,14.9671371569893,15.0126019611003,
15.057675583655,15.1043686581955,15.1493013607845,15.1958140405279,15.2418832890724,
15.2863744865348,15.3329751597116,15.3785518416522,15.4234279663063,15.4702466636066,
15.5152945541928,15.52530082637),.UNSPECIFIED.);
#3200=B_SPLINE_CURVE_WITH_KNOTS('',3,(#59731,#59732,#59733,#59734,#59735,
#59736,#59737,#59738,#59739,#59740,#59741,#59742,#59743,#59744,#59745,#59746,
#59747,#59748,#59749,#59750,#59751,#59752,#59753,#59754,#59755,#59756,#59757,
#59758,#59759,#59760,#59761,#59762,#59763,#59764,#59765,#59766),
 .UNSPECIFIED.,.F.,.F.,(4,2,2,2,2,2,2,2,2,2,2,2,2,2,2,2,2,4),(5.18185396668694,
5.21237880416024,5.25839496787151,5.30515700786141,5.34994371652288,5.39643143795004,
5.44226233153737,5.48755936034949,5.53464520069729,5.57944804001234,5.62527291324563,
5.6719704074037,5.71660500876536,5.76291244016987,5.80904038749152,5.85417959917163,
5.90109443402236,5.92163532773223),.UNSPECIFIED.);
#3201=B_SPLINE_CURVE_WITH_KNOTS('',3,(#59767,#59768,#59769,#59770,#59771,
#59772,#59773,#59774,#59775,#59776,#59777,#59778,#59779,#59780,#59781,#59782,
#59783,#59784,#59785,#59786,#59787,#59788,#59789,#59790,#59791,#59792,#59793,
#59794,#59795,#59796,#59797,#59798,#59799,#59800,#59801,#59802),
 .UNSPECIFIED.,.F.,.F.,(4,2,2,2,2,2,2,2,2,2,2,2,2,2,2,2,2,4),(15.52530082637,
15.5614208749801,15.6076307500252,15.6521806551763,15.6988024547926,15.7445286011097,
15.7892808923799,15.8362633836619,15.8814623071114,15.927276150182,15.9736600042795,
16.0183472193562,16.0650263185026,16.1109370875013,16.1556467587023,16.2028290294383,
16.2482129573077,16.2641372518591),.UNSPECIFIED.);
#3202=B_SPLINE_CURVE_WITH_KNOTS('',3,(#59807,#59808,#59809,#59810,#59811,
#59812,#59813,#59814,#59815,#59816,#59817,#59818,#59819,#59820,#59821,#59822,
#59823,#59824,#59825,#59826,#59827,#59828,#59829,#59830,#59831,#59832,#59833,
#59834,#59835,#59836,#59837,#59838,#59839,#59840,#59841,#59842),
 .UNSPECIFIED.,.F.,.F.,(4,2,2,2,2,2,2,2,2,2,2,2,2,2,2,2,2,4),(4.44139309291887,
4.4776836945143,4.52383758263681,4.5706515514869,4.61567630656631,4.66246297173395,
4.70776020717613,4.75332044171567,4.80007956104877,4.84474067314722,4.89080480911077,
4.93755248920882,4.9824980884388,5.02919719848812,5.0748218411417,5.12031038828011,
5.16760288091741,5.18185396668694),.UNSPECIFIED.);
#3203=B_SPLINE_CURVE_WITH_KNOTS('',3,(#59843,#59844,#59845,#59846,#59847,
#59848,#59849,#59850,#59851,#59852,#59853,#59854,#59855,#59856,#59857,#59858,
#59859,#59860,#59861,#59862,#59863,#59864,#59865,#59866,#59867,#59868,#59869,
#59870,#59871,#59872,#59873,#59874,#59875,#59876,#59877,#59878),
 .UNSPECIFIED.,.F.,.F.,(4,2,2,2,2,2,2,2,2,2,2,2,2,2,2,2,2,4),(16.2641372518591,
16.2938030479407,16.3403922169256,16.3852327690144,16.4318876967614,16.4778418269624,
16.5224230051924,16.5690903719281,16.6145405471659,16.6597873193538,16.7064589360066,
16.7513738230071,16.7981669588227,16.8442036990566,16.8887271777361,16.9353636792139,
16.9809031362162,17.002935013404),.UNSPECIFIED.);
#3204=B_SPLINE_CURVE_WITH_KNOTS('',3,(#59883,#59884,#59885,#59886,#59887,
#59888,#59889,#59890,#59891,#59892,#59893,#59894,#59895,#59896,#59897,#59898,
#59899,#59900,#59901,#59902,#59903,#59904,#59905,#59906,#59907,#59908,#59909,
#59910,#59911,#59912,#59913,#59914,#59915,#59916,#59917,#59918),
 .UNSPECIFIED.,.F.,.F.,(4,2,2,2,2,2,2,2,2,2,2,2,2,2,2,2,2,4),(3.70124435544509,
3.74399270334172,3.79043516360456,3.83649298269546,3.88175593951858,3.92880219405563,
3.97372112979052,4.0195132499672,4.06625467488101,4.11089815679736,4.15717909180209,
4.20358177441128,4.24870726081431,4.29560414051408,4.34067747993884,4.38633433879972,
4.43306819807542,4.44139309291887),.UNSPECIFIED.);
#3205=B_SPLINE_CURVE_WITH_KNOTS('',3,(#59919,#59920,#59921,#59922,#59923,
#59924,#59925,#59926,#59927,#59928,#59929,#59930,#59931,#59932,#59933,#59934,
#59935,#59936,#59937,#59938,#59939,#59940,#59941,#59942,#59943,#59944,#59945,
#59946,#59947,#59948,#59949,#59950,#59951,#59952,#59953,#59954),
 .UNSPECIFIED.,.F.,.F.,(4,2,2,2,2,2,2,2,2,2,2,2,2,2,2,2,2,4),(17.002935013404,
17.025915911193,17.072690284077,17.1176989140485,17.1640720123954,17.2102290691703,
17.2547667681474,17.3014047938411,17.3470724921718,17.3919178234011,17.4388344169549,
17.4839738058451,17.5299894417733,17.576301715541,17.6209316867396,17.6676059002416,
17.7134384093576,17.7416164595014),.UNSPECIFIED.);
#3206=B_SPLINE_CURVE_WITH_KNOTS('',3,(#59959,#59960,#59961,#59962,#59963,
#59964,#59965,#59966,#59967,#59968,#59969,#59970,#59971,#59972,#59973,#59974,
#59975,#59976,#59977,#59978,#59979,#59980,#59981,#59982,#59983,#59984,#59985,
#59986,#59987,#59988,#59989,#59990,#59991,#59992,#59993,#59994,#59995,#59996),
 .UNSPECIFIED.,.F.,.F.,(4,2,2,2,2,2,2,2,2,2,2,2,2,2,2,2,2,2,4),(2.96056667091537,
2.96492507829847,3.00987622737974,3.05658369104791,3.10200096701632,3.14749048096761,
3.19424386881459,3.23892780451988,3.28492439294727,3.33166335850067,3.37655065295563,
3.42318675502558,3.46898366955253,3.51441887445073,3.56165143914983,3.60649480353247,
3.65245839303867,3.69924258599329,3.70124435544509),.UNSPECIFIED.);
#3207=B_SPLINE_CURVE_WITH_KNOTS('',3,(#59997,#59998,#59999,#60000,#60001,
#60002,#60003,#60004,#60005,#60006,#60007,#60008,#60009,#60010,#60011,#60012,
#60013,#60014,#60015,#60016,#60017,#60018,#60019,#60020,#60021,#60022,#60023,
#60024,#60025,#60026,#60027,#60028,#60029,#60030,#60031,#60032),
 .UNSPECIFIED.,.F.,.F.,(4,2,2,2,2,2,2,2,2,2,2,2,2,2,2,2,2,4),(17.7416164595014,
17.7581937074056,17.8052897716113,17.8505949597077,17.8963342553297,17.9428341521077,
17.9875910389412,18.0342105229933,18.0800707772756,18.1246525565008,18.1712871874809,
18.216640662327,18.2619848096412,18.3085503980356,18.3533657933236,18.400359214998,
18.4462787969036,18.4801374068086),.UNSPECIFIED.);
#3208=B_SPLINE_CURVE_WITH_KNOTS('',3,(#60037,#60038,#60039,#60040,#60041,
#60042,#60043,#60044,#60045,#60046,#60047,#60048,#60049,#60050,#60051,#60052,
#60053,#60054,#60055,#60056,#60057,#60058,#60059,#60060,#60061,#60062,#60063,
#60064,#60065,#60066,#60067,#60068,#60069,#60070,#60071,#60072),
 .UNSPECIFIED.,.F.,.F.,(4,2,2,2,2,2,2,2,2,2,2,2,2,2,2,2,2,4),(2.22108960842022,
2.23120408651738,2.27635041765121,2.32327161202571,2.36823721236016,2.41391337632635,
2.46061197044848,2.50519713944098,2.5513666691269,2.59796482409036,2.64299465164124,
2.68978881468655,2.73495033646277,2.78051325751773,2.82722340795193,2.87182391070409,
2.91788757577027,2.96056667091537),.UNSPECIFIED.);
#3209=B_SPLINE_CURVE_WITH_KNOTS('',3,(#60073,#60074,#60075,#60076,#60077,
#60078,#60079,#60080,#60081,#60082,#60083,#60084,#60085,#60086,#60087,#60088,
#60089,#60090,#60091,#60092,#60093,#60094,#60095,#60096,#60097,#60098,#60099,
#60100,#60101,#60102,#60103,#60104,#60105,#60106,#60107,#60108),
 .UNSPECIFIED.,.F.,.F.,(4,2,2,2,2,2,2,2,2,2,2,2,2,2,2,2,2,4),(18.4801374068086,
18.4907658387484,18.5373515732759,18.5827705496792,18.6278503876037,18.6744946287827,
18.7193811593225,18.7659288080364,18.8119468422919,18.8564049604675,18.9029730562544,
18.9484976039111,18.9933693909541,19.040132859827,19.0851285827534,19.1312801378602,
19.1774331259836,19.2175408345414),.UNSPECIFIED.);
#3210=B_SPLINE_CURVE_WITH_KNOTS('',3,(#60113,#60114,#60115,#60116,#60117,
#60118,#60119,#60120,#60121,#60122,#60123,#60124,#60125,#60126,#60127,#60128,
#60129,#60130,#60131,#60132,#60133,#60134,#60135,#60136,#60137,#60138,#60139,
#60140,#60141,#60142,#60143,#60144,#60145,#60146,#60147,#60148),
 .UNSPECIFIED.,.F.,.F.,(4,2,2,2,2,2,2,2,2,2,2,2,2,2,2,2,2,4),(1.48067239643092,
1.4967132601331,1.54219831559389,1.58948594493822,1.63428944893559,1.68030245144475,
1.72708174969294,1.77186789841824,1.81835464146151,1.86425678939566,1.90955548629973,
1.95664189807863,2.00148568451759,2.04731268579268,2.09403346709215,2.13867975716629,
2.18499121798638,2.22108960842022),.UNSPECIFIED.);
#3211=B_SPLINE_CURVE_WITH_KNOTS('',3,(#60149,#60150,#60151,#60152,#60153,
#60154,#60155,#60156,#60157,#60158,#60159,#60160,#60161,#60162,#60163,#60164,
#60165,#60166,#60167,#60168,#60169,#60170,#60171,#60172,#60173,#60174,#60175,
#60176,#60177,#60178,#60179,#60180,#60181,#60182,#60183,#60184,#60185,#60186),
 .UNSPECIFIED.,.F.,.F.,(4,2,2,2,2,2,2,2,2,2,2,2,2,2,2,2,2,2,4),(19.2175408345414,
19.221937402198,19.2685210781433,19.3141891434761,19.3589248273872,19.4058460255822,
19.4509870795851,19.4968133821774,19.5431350562803,19.5877640969252,19.634399062382,
19.6802461572256,19.724925976838,19.7720412018952,19.81736181445,19.862949655886,
19.9094715921544,19.954248074309,19.955968047547),.UNSPECIFIED.);
#3212=B_SPLINE_CURVE_WITH_KNOTS('',3,(#60191,#60192,#60193,#60194,#60195,
#60196,#60197,#60198,#60199,#60200,#60201,#60202,#60203,#60204,#60205,#60206,
#60207,#60208,#60209,#60210,#60211,#60212,#60213,#60214,#60215,#60216,#60217,
#60218,#60219,#60220,#60221,#60222,#60223,#60224,#60225,#60226),
 .UNSPECIFIED.,.F.,.F.,(4,2,2,2,2,2,2,2,2,2,2,2,2,2,2,2,2,4),(0.740262878330326,
0.76242710224918,0.808069985435835,0.854808846306471,0.899429812602798,
0.94557087207502,0.992454683252572,1.03747065149212,1.08424743872217,1.12958660658263,
1.17513888970271,1.22190780151563,1.26658471045133,1.31264188423565,1.35939848502835,
1.40433922056887,1.45103260194552,1.48067239643092),.UNSPECIFIED.);
#3213=B_SPLINE_CURVE_WITH_KNOTS('',3,(#60227,#60228,#60229,#60230,#60231,
#60232,#60233,#60234,#60235,#60236,#60237,#60238,#60239,#60240,#60241,#60242,
#60243,#60244,#60245,#60246,#60247,#60248,#60249,#60250,#60251,#60252,#60253,
#60254,#60255,#60256,#60257,#60258,#60259,#60260,#60261,#60262),
 .UNSPECIFIED.,.F.,.F.,(4,2,2,2,2,2,2,2,2,2,2,2,2,2,2,2,2,4),(19.955968047547,
20.000850484569,20.0467368471769,20.0912761893499,20.1378918513278,20.1832739357276,
20.2285046069091,20.2751045193351,20.3199511150685,20.3667546312751,20.4127173706803,
20.4571887517883,20.5037686958299,20.5492336722642,20.5942218827244,20.6409180673264,
20.685852328368,20.6936878782319),.UNSPECIFIED.);
#3214=B_SPLINE_CURVE_WITH_KNOTS('',3,(#60267,#60268,#60269,#60270,#60271,
#60272,#60273,#60274,#60275,#60276,#60277,#60278,#60279,#60280,#60281,#60282,
#60283,#60284,#60285,#60286,#60287,#60288,#60289,#60290,#60291,#60292,#60293,
#60294,#60295,#60296,#60297,#60298,#60299,#60300,#60301,#60302),
 .UNSPECIFIED.,.F.,.F.,(4,2,2,2,2,2,2,2,2,2,2,2,2,2,2,2,2,4),(1.00000014275486E-6,
0.0364903991724837,0.0742057368406976,0.120984278386942,0.16571626048475,
0.212135354717781,0.258243398985401,0.303486376623694,0.350510827495094,
0.395451299112592,0.441223703714196,0.487964967575798,0.532602258878132,
0.578864855190162,0.62532910035835,0.67044002179057,0.717320863587734,0.740262878330326),
 .UNSPECIFIED.);
#3215=B_SPLINE_CURVE_WITH_KNOTS('',3,(#60303,#60304,#60305,#60306,#60307,
#60308,#60309,#60310,#60311,#60312,#60313,#60314,#60315,#60316,#60317,#60318,
#60319,#60320,#60321,#60322,#60323,#60324,#60325,#60326,#60327,#60328,#60329,
#60330,#60331,#60332,#60333,#60334,#60335,#60336,#60337,#60338),
 .UNSPECIFIED.,.F.,.F.,(4,2,2,2,2,2,2,2,2,2,2,2,2,2,2,2,2,4),(20.6936878782319,
20.732228532913,20.778305724133,20.8227795112891,20.8693557797099,20.9149428959302,
20.9597524918607,21.0065846919771,21.0516438918501,21.0976519462771,21.1438788857884,
21.188432480541,21.2350393010027,21.2807854645354,21.325492530929,21.3724982961973,
21.417717731441,21.4315064083924),.UNSPECIFIED.);
#3216=B_SPLINE_CURVE_WITH_KNOTS('',3,(#60341,#60342,#60343,#60344,#60345,
#60346,#60347,#60348),.UNSPECIFIED.,.F.,.F.,(4,2,2,4),(21.4315064083924,
21.4634358005757,21.493031868375,21.522626598838),.UNSPECIFIED.);
#3217=B_SPLINE_CURVE_WITH_KNOTS('',3,(#60353,#60354,#60355,#60356,#60357,
#60358,#60359,#60360,#60361,#60362,#60363,#60364),.UNSPECIFIED.,.F.,.F.,
(4,2,2,2,2,4),(-0.220493779628296,-0.188155373461082,-0.153829429857051,
-0.103952453260852,-0.0536656706932583,-1.00000014990886E-6),
 .UNSPECIFIED.);
#3218=B_SPLINE_CURVE_WITH_KNOTS('',3,(#60367,#60368,#60369,#60370,#60371,
#60372,#60373,#60374,#60375,#60376,#60377,#60378,#60379,#60380,#60381,#60382,
#60383,#60384,#60385,#60386,#60387,#60388),.UNSPECIFIED.,.F.,.F.,(4,2,2,
2,2,2,2,2,2,2,4),(0.203440126186273,0.213167596868103,0.241856386112924,
0.272211919544501,0.305118112000406,0.341399456620154,0.378879659132554,
0.40534149334872,0.429291364608543,0.44378295238274,0.459192789470913),
 .UNSPECIFIED.);
#3219=B_SPLINE_CURVE_WITH_KNOTS('',3,(#60390,#60391,#60392,#60393,#60394,
#60395,#60396,#60397,#60398,#60399,#60400,#60401,#60402,#60403,#60404,#60405,
#60406,#60407,#60408,#60409,#60410,#60411,#60412,#60413,#60414,#60415,#60416,
#60417,#60418,#60419,#60420,#60421,#60422,#60423),.UNSPECIFIED.,.F.,.F.,
(4,2,2,2,2,2,2,2,2,2,2,2,2,2,2,2,4),(-0.921606618540025,-0.872688627355351,
-0.813612023857313,-0.756611351546357,-0.69692945872276,-0.638499761548747,
-0.581118209737007,-0.521076231967445,-0.463317306881228,-0.4044438926574,
-0.345164740388026,-0.288053249414949,-0.228344796882901,-0.169710130792356,
-0.112479424024743,-0.0563089256119929,-9.99999990258793E-7),
 .UNSPECIFIED.);
#3220=B_SPLINE_CURVE_WITH_KNOTS('',3,(#60424,#60425,#60426,#60427,#60428,
#60429,#60430,#60431,#60432,#60433,#60434,#60435,#60436,#60437,#60438,#60439,
#60440,#60441,#60442,#60443,#60444,#60445,#60446,#60447,#60448,#60449,#60450,
#60451,#60452,#60453,#60454,#60455),.UNSPECIFIED.,.F.,.F.,(4,2,2,2,2,2,
2,2,2,2,2,2,2,2,2,4),(-27.2675995337344,-27.2205810783644,-27.1716030839864,
-27.1114524980469,-27.0544959346273,-26.9959799991961,-26.9364896777515,
-26.8795127522937,-26.8203565510693,-26.7619639947482,-26.7043369916545,
-26.6444247756288,-26.5873734790364,-26.5290771329393,-26.4696302887724,
-26.4647006629411),.UNSPECIFIED.);
#3221=B_SPLINE_CURVE_WITH_KNOTS('',3,(#60632,#60633,#60634,#60635,#60636,
#60637,#60638,#60639),.UNSPECIFIED.,.F.,.F.,(4,2,2,4),(-0.00426615559741139,
-0.00353262795509977,-0.00302253710286643,-0.00251244625063308),
 .UNSPECIFIED.);
#3222=B_SPLINE_CURVE_WITH_KNOTS('',3,(#61553,#61554,#61555,#61556,#61557,
#61558,#61559,#61560),.UNSPECIFIED.,.F.,.F.,(4,2,2,4),(-0.00251244625063308,
-0.00200235539839974,-0.0014922645461664,-0.000758736903856822),
 .UNSPECIFIED.);
#3223=B_SPLINE_CURVE_WITH_KNOTS('',3,(#61565,#61566,#61567,#61568,#61569,
#61570,#61571,#61572),.UNSPECIFIED.,.F.,.F.,(4,2,2,4),(-0.00932716297425779,
-0.00859363533194745,-0.0080835444797141,-0.00757345362748076),
 .UNSPECIFIED.);
#3224=B_SPLINE_CURVE_WITH_KNOTS('',3,(#62486,#62487,#62488,#62489,#62490,
#62491,#62492,#62493),.UNSPECIFIED.,.F.,.F.,(4,2,2,4),(-0.00757345362748076,
-0.00706336277524741,-0.00655327192301407,-0.00581974428070595),
 .UNSPECIFIED.);
#3225=B_SPLINE_CURVE_WITH_KNOTS('',3,(#64489,#64490,#64491,#64492,#64493,
#64494,#64495,#64496,#64497,#64498,#64499,#64500,#64501,#64502,#64503,#64504,
#64505,#64506,#64507,#64508,#64509,#64510,#64511,#64512,#64513,#64514,#64515,
#64516),.UNSPECIFIED.,.F.,.F.,(4,2,2,2,2,2,2,2,2,2,2,2,2,4),(1.00000052656661E-6,
0.0405527857266322,0.0799421814660319,0.1262631587317,0.186952165234641,
0.270820823781497,0.348937293245129,0.459507052180891,0.623823282878412,
0.790896670749941,0.927459468885873,1.05843758188768,1.16179395572833,1.24835467272154),
 .UNSPECIFIED.);
#3226=B_SPLINE_CURVE_WITH_KNOTS('',3,(#65626,#65627,#65628,#65629,#65630,
#65631,#65632,#65633,#65634,#65635,#65636,#65637,#65638,#65639,#65640,#65641,
#65642,#65643,#65644,#65645,#65646,#65647,#65648,#65649,#65650,#65651,#65652,
#65653,#65654,#65655,#65656,#65657,#65658,#65659,#65660,#65661),
 .UNSPECIFIED.,.F.,.F.,(4,2,2,2,2,2,2,2,2,2,2,2,2,2,2,2,2,4),(-0.945073641183675,
-0.895238035194944,-0.83625541046657,-0.779319325111488,-0.719695813140934,
-0.661359932358853,-0.603989382535731,-0.544046656752618,-0.486380595229568,
-0.427463950957105,-0.368285170516134,-0.311258814957492,-0.251615042406746,
-0.193080680180277,-0.135881569867343,-0.0757214675349668,-0.0372079607299379,
-9.99999995143774E-7),.UNSPECIFIED.);
#3227=B_SPLINE_CURVE_WITH_KNOTS('',3,(#65667,#65668,#65669,#65670,#65671,
#65672,#65673,#65674,#65675,#65676,#65677,#65678,#65679,#65680,#65681,#65682,
#65683,#65684,#65685,#65686,#65687,#65688,#65689,#65690,#65691,#65692,#65693,
#65694,#65695,#65696,#65697,#65698,#65699,#65700),.UNSPECIFIED.,.F.,.F.,
(4,2,2,2,2,2,2,2,2,2,2,2,2,2,2,2,4),(-27.258759550315,-27.2281298462553,
-27.1982051538512,-27.1403355656588,-27.0801605899845,-27.0231066733285,
-26.9645639497272,-26.9050010855415,-26.8479917157334,-26.7888070303952,
-26.7302213719406,-26.6725610910419,-26.6126177738291,-26.5554428144319,
-26.4971129260297,-26.4375855046171,-26.4315188069733),.UNSPECIFIED.);
#3228=B_SPLINE_CURVE_WITH_KNOTS('',3,(#65705,#65706,#65707,#65708,#65709,
#65710,#65711,#65712,#65713,#65714,#65715,#65716,#65717,#65718,#65719,#65720,
#65721,#65722,#65723,#65724,#65725,#65726,#65727,#65728,#65729,#65730,#65731,
#65732,#65733,#65734,#65735,#65736,#65737,#65738,#65739,#65740),
 .UNSPECIFIED.,.F.,.F.,(4,2,2,2,2,2,2,2,2,2,2,2,2,2,2,2,2,4),(-1.89025095676006,
-1.83161362612537,-1.77291723413503,-1.71588088128378,-1.65621305093223,
-1.59816806724067,-1.54019307596245,-1.48057902624682,-1.42320721251111,
-1.36315245228605,-1.30433237640506,-1.24738924893859,-1.18775702178512,
-1.12958586526634,-1.07195013380193,-1.0121910944455,-0.954689933605391,
-0.945073641183675),.UNSPECIFIED.);
#3229=B_SPLINE_CURVE_WITH_KNOTS('',3,(#65741,#65742,#65743,#65744,#65745,
#65746,#65747,#65748,#65749,#65750,#65751,#65752,#65753,#65754,#65755,#65756,
#65757,#65758,#65759,#65760,#65761,#65762,#65763,#65764,#65765,#65766,#65767,
#65768,#65769,#65770,#65771,#65772,#65773,#65774,#65775,#65776),
 .UNSPECIFIED.,.F.,.F.,(4,2,2,2,2,2,2,2,2,2,2,2,2,2,2,2,2,4),(-26.4315188069733,
-26.3807149169946,-26.3217404209326,-26.2626652889544,-26.2051855221022,
-26.1454428390691,-26.08804784233,-26.0298996832198,-25.970377539516,-25.9135472636022,
-25.8547523829465,-25.7951046336945,-25.7377721236726,-25.6781939173096,
-25.6204935481626,-25.5624909627037,-25.5029463840743,-25.4881909358829),
 .UNSPECIFIED.);
#3230=B_SPLINE_CURVE_WITH_KNOTS('',3,(#65781,#65782,#65783,#65784,#65785,
#65786,#65787,#65788,#65789,#65790,#65791,#65792,#65793,#65794,#65795,#65796,
#65797,#65798,#65799,#65800,#65801,#65802,#65803,#65804,#65805,#65806,#65807,
#65808,#65809,#65810,#65811,#65812,#65813,#65814,#65815,#65816,#65817,#65818),
 .UNSPECIFIED.,.F.,.F.,(4,2,2,2,2,2,2,2,2,2,2,2,2,2,2,2,2,2,4),(-2.83625896355377,
-2.82853093222041,-2.76886611006394,-2.71046756100465,-2.65308502383756,
-2.59307616772703,-2.5353480705631,-2.47645222776391,-2.41720668492958,
-2.36012338869581,-2.30043449435393,-2.24183347940531,-2.1846099393252,
-2.12437972037366,-2.06645193254166,-2.00798057621261,-1.94850769470731,
-1.89126109663031,-1.89025095676006),.UNSPECIFIED.);
#3231=B_SPLINE_CURVE_WITH_KNOTS('',3,(#65819,#65820,#65821,#65822,#65823,
#65824,#65825,#65826,#65827,#65828,#65829,#65830,#65831,#65832,#65833,#65834,
#65835,#65836,#65837,#65838,#65839,#65840,#65841,#65842,#65843,#65844,#65845,
#65846,#65847,#65848,#65849,#65850,#65851,#65852,#65853,#65854),
 .UNSPECIFIED.,.F.,.F.,(4,2,2,2,2,2,2,2,2,2,2,2,2,2,2,2,2,4),(-25.4881909358829,
-25.4460636732589,-25.3874120918811,-25.3278816537184,-25.2706841301686,
-25.2112575632321,-25.1531186176646,-25.0952452143788,-25.0350644348795,
-24.9780430196917,-24.9194961959997,-24.8599520194551,-24.8029424006809,
-24.7437542679059,-24.6852489172368,-24.6275880933991,-24.5676424609794,
-24.544394043377),.UNSPECIFIED.);
#3232=B_SPLINE_CURVE_WITH_KNOTS('',3,(#65859,#65860,#65861,#65862,#65863,
#65864,#65865,#65866,#65867,#65868,#65869,#65870,#65871,#65872,#65873,#65874,
#65875,#65876,#65877,#65878,#65879,#65880,#65881,#65882,#65883,#65884,#65885,
#65886,#65887,#65888,#65889,#65890,#65891,#65892,#65893,#65894),
 .UNSPECIFIED.,.F.,.F.,(4,2,2,2,2,2,2,2,2,2,2,2,2,2,2,2,2,4),(-3.78192035948685,
-3.76562796298537,-3.70592564973338,-3.6478278361799,-3.5898592957152,-3.53018901929876,
-3.47276427223133,-3.41274694188657,-3.3538687217505,-3.29689298752725,
-3.2372230084892,-3.17899386626536,-3.12135698149028,-3.06153650613278,
-3.00397762776562,-2.94455692608413,-2.88551146939021,-2.83625896355377),
 .UNSPECIFIED.);
#3233=B_SPLINE_CURVE_WITH_KNOTS('',3,(#65895,#65896,#65897,#65898,#65899,
#65900,#65901,#65902,#65903,#65904,#65905,#65906,#65907,#65908,#65909,#65910,
#65911,#65912,#65913,#65914,#65915,#65916,#65917,#65918,#65919,#65920,#65921,
#65922,#65923,#65924,#65925,#65926,#65927,#65928,#65929,#65930),
 .UNSPECIFIED.,.F.,.F.,(4,2,2,2,2,2,2,2,2,2,2,2,2,2,2,2,2,4),(-24.544394043377,
-24.5105131978097,-24.4521827141638,-24.3926780124691,-24.3358195936076,
-24.2768451471733,-24.2178632708879,-24.1603868788961,-24.1006461200198,
-24.0433090290329,-23.9851645307063,-23.9256688814307,-23.8688632830925,
-23.8100726156683,-23.7505272749807,-23.6932025949219,-23.6336311604901,
-23.6014349735858),.UNSPECIFIED.);
#3234=B_SPLINE_CURVE_WITH_KNOTS('',3,(#65935,#65936,#65937,#65938,#65939,
#65940,#65941,#65942,#65943,#65944,#65945,#65946,#65947,#65948,#65949,#65950,
#65951,#65952,#65953,#65954,#65955,#65956,#65957,#65958,#65959,#65960,#65961,
#65962,#65963,#65964,#65965,#65966,#65967,#65968,#65969,#65970),
 .UNSPECIFIED.,.F.,.F.,(4,2,2,2,2,2,2,2,2,2,2,2,2,2,2,2,2,4),(-4.72839430207058,
-4.70337431740566,-4.64331595464347,-4.58554178921411,-4.52667966073054,
-4.4673838894256,-4.41025831032806,-4.35054027250619,-4.29188896156004,
-4.23465469260147,-4.17437122548907,-4.11639389057874,-4.05794278357937,
-3.99841660337735,-3.94111979450562,-3.88143640467257,-3.82268708479341,
-3.78192035948685),.UNSPECIFIED.);
#3235=B_SPLINE_CURVE_WITH_KNOTS('',3,(#65971,#65972,#65973,#65974,#65975,
#65976,#65977,#65978,#65979,#65980,#65981,#65982,#65983,#65984,#65985,#65986,
#65987,#65988,#65989,#65990,#65991,#65992,#65993,#65994,#65995,#65996,#65997,
#65998,#65999,#66000,#66001,#66002,#66003,#66004,#66005,#66006),
 .UNSPECIFIED.,.F.,.F.,(4,2,2,2,2,2,2,2,2,2,2,2,2,2,2,2,2,4),(-23.6014349735858,
-23.5759985868542,-23.5180045036599,-23.458489879113,-23.4016430359386,
-23.3430005479742,-23.2834982736845,-23.226310920464,-23.166893628097,-23.1088378874003,
-23.0509758826866,-22.9908049952875,-22.9338319947597,-22.8752964277514,
-22.8157879004539,-22.7587920199088,-22.6996160282244,-22.6581171675807),
 .UNSPECIFIED.);
#3236=B_SPLINE_CURVE_WITH_KNOTS('',3,(#66011,#66012,#66013,#66014,#66015,
#66016,#66017,#66018,#66019,#66020,#66021,#66022,#66023,#66024,#66025,#66026,
#66027,#66028,#66029,#66030,#66031,#66032,#66033,#66034,#66035,#66036,#66037,
#66038,#66039,#66040,#66041,#66042,#66043,#66044,#66045,#66046),
 .UNSPECIFIED.,.F.,.F.,(4,2,2,2,2,2,2,2,2,2,2,2,2,2,2,2,2,4),(-5.67439159596968,
-5.64047766140835,-5.58076721688331,-5.52330498546526,-5.4633387313466,
-5.40441833910885,-5.34742402529794,-5.28773207490788,-5.22946075409439,
-5.17183622553644,-5.11197061930769,-5.05436969869878,-4.99499338073396,
-4.9359013779351,-4.878890651626,-4.8192004273671,-4.76075532631967,-4.72839430207058),
 .UNSPECIFIED.);
#3237=B_SPLINE_CURVE_WITH_KNOTS('',3,(#66047,#66048,#66049,#66050,#66051,
#66052,#66053,#66054,#66055,#66056,#66057,#66058,#66059,#66060,#66061,#66062,
#66063,#66064,#66065,#66066,#66067,#66068,#66069,#66070,#66071,#66072,#66073,
#66074,#66075,#66076,#66077,#66078,#66079,#66080,#66081,#66082),
 .UNSPECIFIED.,.F.,.F.,(4,2,2,2,2,2,2,2,2,2,2,2,2,2,2,2,2,4),(-22.6581171675807,
-22.6412102410835,-22.5835641689142,-22.5236319902899,-22.4665652482388,
-22.4082496043878,-22.3487848861067,-22.2919531828174,-22.2329943725634,
-22.1741263229248,-22.1166686457465,-22.0569456248039,-21.9996842855768,
-21.9415589369491,-21.8821072544915,-21.8253417468782,-21.7665709936596,
-21.7157628302399),.UNSPECIFIED.);
#3238=B_SPLINE_CURVE_WITH_KNOTS('',3,(#66087,#66088,#66089,#66090,#66091,
#66092,#66093,#66094,#66095,#66096,#66097,#66098,#66099,#66100,#66101,#66102,
#66103,#66104,#66105,#66106,#66107,#66108,#66109,#66110,#66111,#66112,#66113,
#66114,#66115,#66116,#66117,#66118,#66119,#66120,#66121,#66122),
 .UNSPECIFIED.,.F.,.F.,(4,2,2,2,2,2,2,2,2,2,2,2,2,2,2,2,2,4),(-6.62109380521341,
-6.57761768259959,-6.51828740763027,-6.46113362202641,-6.40140207096381,
-6.34271600715298,-6.28548482095171,-6.22516410228413,-6.16715260360109,
-6.10873547077658,-6.04917186097877,-5.99184011673613,-5.93213648107799,
-5.8733499659965,-5.81628212661826,-5.75656105013342,-5.69842598086126,
-5.67439159596968),.UNSPECIFIED.);
#3239=B_SPLINE_CURVE_WITH_KNOTS('',3,(#66123,#66124,#66125,#66126,#66127,
#66128,#66129,#66130,#66131,#66132,#66133,#66134,#66135,#66136,#66137,#66138,
#66139,#66140,#66141,#66142,#66143,#66144,#66145,#66146,#66147,#66148,#66149,
#66150,#66151,#66152,#66153,#66154,#66155,#66156,#66157,#66158),
 .UNSPECIFIED.,.F.,.F.,(4,2,2,2,2,2,2,2,2,2,2,2,2,2,2,2,2,4),(-21.7157628302399,
-21.7071499734112,-21.6498486291818,-21.5902999589255,-21.5327541629797,
-21.4747842600729,-21.4153173211779,-21.3585227590009,-21.2999052492263,
-21.2398720875173,-21.1826905454483,-21.1232764692568,-21.065378520901,
-21.0075245508875,-20.9480158554619,-20.8911101904613,-20.8326059984683,
-20.7731793950157),.UNSPECIFIED.);
#3240=B_SPLINE_CURVE_WITH_KNOTS('',3,(#66163,#66164,#66165,#66166,#66167,
#66168,#66169,#66170,#66171,#66172,#66173,#66174,#66175,#66176,#66177,#66178,
#66179,#66180,#66181,#66182,#66183,#66184,#66185,#66186,#66187,#66188,#66189,
#66190,#66191,#66192,#66193,#66194,#66195,#66196,#66197,#66198),
 .UNSPECIFIED.,.F.,.F.,(4,2,2,2,2,2,2,2,2,2,2,2,2,2,2,2,2,4),(-7.56721318319246,
-7.51440195941646,-7.4554548070908,-7.39845589958658,-7.33875763160917,
-7.28045937419718,-7.22286133868259,-7.16296628560166,-7.10533842940707,
-7.04602095897405,-6.9868979771895,-6.92987099130527,-6.87017100691209,
-6.81169474396116,-6.75432913502786,-6.69423710481114,-6.63643211656935,
-6.62109380521341),.UNSPECIFIED.);
#3241=B_SPLINE_CURVE_WITH_KNOTS('',3,(#66199,#66200,#66201,#66202,#66203,
#66204,#66205,#66206,#66207,#66208,#66209,#66210,#66211,#66212,#66213,#66214,
#66215,#66216,#66217,#66218,#66219,#66220,#66221,#66222,#66223,#66224,#66225,
#66226,#66227,#66228,#66229,#66230,#66231,#66232,#66233,#66234,#66235,#66236),
 .UNSPECIFIED.,.F.,.F.,(4,2,2,2,2,2,2,2,2,2,2,2,2,2,2,2,2,2,4),(-20.7731793950157,
-20.7731201315055,-20.7160582025871,-20.6567792566783,-20.5983599289237,
-20.5406164839802,-20.4805811221967,-20.4234656784966,-20.3650514109911,
-20.305511597516,-20.2485949896086,-20.1895371334662,-20.1306696919239,
-20.0731189832228,-20.0132974755221,-19.9560008596223,-19.8977815738613,
-19.8382589546996,-19.8295444030046),.UNSPECIFIED.);
#3242=B_SPLINE_CURVE_WITH_KNOTS('',3,(#66241,#66242,#66243,#66244,#66245,
#66246,#66247,#66248,#66249,#66250,#66251,#66252,#66253,#66254,#66255,#66256,
#66257,#66258,#66259,#66260,#66261,#66262,#66263,#66264,#66265,#66266,#66267,
#66268,#66269,#66270,#66271,#66272,#66273,#66274,#66275,#66276,#66277,#66278),
 .UNSPECIFIED.,.F.,.F.,(4,2,2,2,2,2,2,2,2,2,2,2,2,2,2,2,2,2,4),(-8.51391269073544,
-8.51222365838152,-8.45249428513948,-8.39378861667143,-8.33657472393003,
-8.27623231073072,-8.21820164401039,-8.1598332741766,-8.10024765479814,
-8.04289584139225,-7.98318755401621,-7.92437912604881,-7.86731677437594,
-7.80759259896721,-7.74943539170332,-7.6915218402897,-7.631786775557,-7.57430204194946,
-7.56721318319246),.UNSPECIFIED.);
#3243=B_SPLINE_CURVE_WITH_KNOTS('',3,(#66279,#66280,#66281,#66282,#66283,
#66284,#66285,#66286,#66287,#66288,#66289,#66290,#66291,#66292,#66293,#66294,
#66295,#66296,#66297,#66298,#66299,#66300,#66301,#66302,#66303,#66304,#66305,
#66306,#66307,#66308,#66309,#66310,#66311,#66312,#66313,#66314),
 .UNSPECIFIED.,.F.,.F.,(4,2,2,2,2,2,2,2,2,2,2,2,2,2,2,2,2,4),(-19.8295444030046,
-19.781422440649,-19.7225572817117,-19.6631471763022,-19.6057577545878,
-19.5461159927651,-19.4885461013889,-19.4304876297435,-19.3709535721035,
-19.3141007093386,-19.2553941827952,-19.1953773792029,-19.1381132548424,
-19.0786120692882,-19.0206974716804,-18.9627608300149,-18.9031885891784,
-18.8860416189937),.UNSPECIFIED.);
#3244=B_SPLINE_CURVE_WITH_KNOTS('',3,(#66319,#66320,#66321,#66322,#66323,
#66324,#66325,#66326,#66327,#66328,#66329,#66330,#66331,#66332,#66333,#66334,
#66335,#66336,#66337,#66338,#66339,#66340,#66341,#66342,#66343,#66344,#66345,
#66346,#66347,#66348,#66349,#66350,#66351,#66352,#66353,#66354),
 .UNSPECIFIED.,.F.,.F.,(4,2,2,2,2,2,2,2,2,2,2,2,2,2,2,2,2,4),(-9.4600020867739,
-9.44946097484441,-9.38977226427863,-9.3314620836995,-9.27390543364871,
-9.21399634460654,-9.15635642704838,-9.09711384600216,-9.03797514352587,
-8.98094579786149,-8.92125183936447,-8.86275948675276,-8.8054237975235,
-8.7453135764027,-8.68749269541132,-8.62874128051507,-8.56939184171518,
-8.51391269073544),.UNSPECIFIED.);
#3245=B_SPLINE_CURVE_WITH_KNOTS('',3,(#66355,#66356,#66357,#66358,#66359,
#66360,#66361,#66362,#66363,#66364,#66365,#66366,#66367,#66368,#66369,#66370,
#66371,#66372,#66373,#66374,#66375,#66376,#66377,#66378,#66379,#66380,#66381,
#66382,#66383,#66384,#66385,#66386,#66387,#66388,#66389,#66390),
 .UNSPECIFIED.,.F.,.F.,(4,2,2,2,2,2,2,2,2,2,2,2,2,2,2,2,2,4),(-18.8860416189937,
-18.8462348900712,-18.7876476548069,-18.7280968440835,-18.6709555484027,
-18.6115929558287,-18.5531716016611,-18.495349324202,-18.4352301709226,
-18.3780798368063,-18.319585679885,-18.2599881331103,-18.2030028878512,
-18.1438648978918,-18.0850090800984,-18.0273834680497,-17.9674824112817,
-17.941522876477),.UNSPECIFIED.);
#3246=B_SPLINE_CURVE_WITH_KNOTS('',3,(#66395,#66396,#66397,#66398,#66399,
#66400,#66401,#66402,#66403,#66404,#66405,#66406,#66407,#66408,#66409,#66410,
#66411,#66412,#66413,#66414,#66415,#66416,#66417,#66418,#66419,#66420,#66421,
#66422,#66423,#66424,#66425,#66426,#66427,#66428,#66429,#66430),
 .UNSPECIFIED.,.F.,.F.,(4,2,2,2,2,2,2,2,2,2,2,2,2,2,2,2,2,4),(-10.4063262286273,
-10.387392591544,-10.3270439303512,-10.2690090232558,-10.210705562305,-10.1511132343272,
-10.09375612853,-10.034059046947,-9.97524386932148,-9.91820163035005,-9.8584903134111,
-9.80032595747233,-9.74246277833438,-9.68271846928724,-9.62522607647149,
-9.56540900336133,-9.50645028314585,-9.4600020867739),.UNSPECIFIED.);
#3247=B_SPLINE_CURVE_WITH_KNOTS('',3,(#66431,#66432,#66433,#66434,#66435,
#66436,#66437,#66438,#66439,#66440,#66441,#66442,#66443,#66444,#66445,#66446,
#66447,#66448,#66449,#66450,#66451,#66452,#66453,#66454,#66455,#66456,#66457,
#66458,#66459,#66460,#66461,#66462,#66463,#66464,#66465,#66466),
 .UNSPECIFIED.,.F.,.F.,(4,2,2,2,2,2,2,2,2,2,2,2,2,2,2,2,2,4),(-17.941522876477,
-17.9101636562757,-17.8518687182981,-17.7922922877475,-17.7354001068821,
-17.6764590004862,-17.6170707989498,-17.5596109797981,-17.4998945731994,
-17.4423134048219,-17.3841841685699,-17.3245998970605,-17.2677034424408,
-17.2089258668494,-17.1489368038417,-17.0916073172332,-17.0320369692312,
-16.997272415308),.UNSPECIFIED.);
#3248=B_SPLINE_CURVE_WITH_KNOTS('',3,(#66471,#66472,#66473,#66474,#66475,
#66476,#66477,#66478,#66479,#66480,#66481,#66482,#66483,#66484,#66485,#66486,
#66487,#66488,#66489,#66490,#66491,#66492,#66493,#66494,#66495,#66496,#66497,
#66498,#66499,#66500,#66501,#66502,#66503,#66504,#66505,#66506),
 .UNSPECIFIED.,.F.,.F.,(4,2,2,2,2,2,2,2,2,2,2,2,2,2,2,2,2,4),(-11.3522871924595,
-11.324430394275,-11.264522730746,-11.2068857092522,-11.1477360236872,-11.08859687367,
-11.0315792760543,-10.9719076335357,-10.9134142640608,-10.8561239489264,
-10.796010976838,-10.7381891351563,-10.6795177406942,-10.620164420077,-10.5629956093436,
-10.5032845165816,-10.4445743180876,-10.4063262286273),.UNSPECIFIED.);
#3249=B_SPLINE_CURVE_WITH_KNOTS('',3,(#66507,#66508,#66509,#66510,#66511,
#66512,#66513,#66514,#66515,#66516,#66517,#66518,#66519,#66520,#66521,#66522,
#66523,#66524,#66525,#66526,#66527,#66528,#66529,#66530,#66531,#66532,#66533,
#66534,#66535,#66536,#66537,#66538,#66539,#66540,#66541,#66542),
 .UNSPECIFIED.,.F.,.F.,(4,2,2,2,2,2,2,2,2,2,2,2,2,2,2,2,2,4),(-16.997272415308,
-16.974118579872,-16.9161165902415,-16.8564975009602,-16.7995101512218,
-16.7408573501075,-16.6812582779792,-16.6240545216982,-16.5646258893359,
-16.5062147666311,-16.448330624569,-16.388145391231,-16.3309738020301,-16.2724169024022,
-16.2127779950283,-16.155739296564,-16.0965384948368,-16.052121842989),
 .UNSPECIFIED.);
#3250=B_SPLINE_CURVE_WITH_KNOTS('',3,(#66547,#66548,#66549,#66550,#66551,
#66552,#66553,#66554,#66555,#66556,#66557,#66558,#66559,#66560,#66561,#66562,
#66563,#66564,#66565,#66566,#66567,#66568,#66569,#66570,#66571,#66572,#66573,
#66574,#66575,#66576,#66577,#66578,#66579,#66580,#66581,#66582),
 .UNSPECIFIED.,.F.,.F.,(4,2,2,2,2,2,2,2,2,2,2,2,2,2,2,2,2,4),(-12.2980151684053,
-12.2608049534251,-12.2012214180354,-12.1438740189948,-12.0842046319712,
-12.0253980696236,-11.9683912868138,-11.9087094544592,-11.8505531273409,
-11.7927573534416,-11.7330193273245,-11.6755342944868,-11.6158192576419,
-11.5568642629696,-11.4998992163216,-11.4402365277277,-11.3819295252021,
-11.3522871924595),.UNSPECIFIED.);
#3251=B_SPLINE_CURVE_WITH_KNOTS('',3,(#66583,#66584,#66585,#66586,#66587,
#66588,#66589,#66590,#66591,#66592,#66593,#66594,#66595,#66596,#66597,#66598,
#66599,#66600,#66601,#66602,#66603,#66604,#66605,#66606,#66607,#66608,#66609,
#66610,#66611,#66612,#66613,#66614,#66615,#66616,#66617,#66618),
 .UNSPECIFIED.,.F.,.F.,(4,2,2,2,2,2,2,2,2,2,2,2,2,2,2,2,2,4),(-16.052121842989,
-16.0377063442003,-15.9800225041649,-15.9200592855784,-15.8627316418797,
-15.8043778785959,-15.7447638720137,-15.6878306019307,-15.6288305455336,
-15.5694764347843,-15.5119625793001,-15.452188569769,-15.3946092699113,
-15.3364257590099,-15.2768073817686,-15.2198815508401,-15.1610495793805,
-15.1073443691545),.UNSPECIFIED.);
#3252=B_SPLINE_CURVE_WITH_KNOTS('',3,(#66623,#66624,#66625,#66626,#66627,
#66628,#66629,#66630,#66631,#66632,#66633,#66634,#66635,#66636,#66637,#66638,
#66639,#66640,#66641,#66642,#66643,#66644,#66645,#66646,#66647,#66648,#66649,
#66650,#66651,#66652,#66653,#66654,#66655,#66656,#66657,#66658),
 .UNSPECIFIED.,.F.,.F.,(4,2,2,2,2,2,2,2,2,2,2,2,2,2,2,2,2,4),(-13.2436220538442,
-13.1973293402993,-13.1382053560805,-13.0812140676331,-13.0215819437106,
-12.9631029490451,-12.905874761448,-12.8457747640532,-12.787967213325,-12.7293949980337,
-12.670053341907,-12.6128978517491,-12.5532219431716,-12.494522530246,-12.4373888207658,
-12.3770495663262,-12.3190255916381,-12.2980151684053),.UNSPECIFIED.);
#3253=B_SPLINE_CURVE_WITH_KNOTS('',3,(#66659,#66660,#66661,#66662,#66663,
#66664,#66665,#66666,#66667,#66668,#66669,#66670,#66671,#66672,#66673,#66674,
#66675,#66676,#66677,#66678,#66679,#66680,#66681,#66682,#66683,#66684,#66685,
#66686,#66687,#66688,#66689,#66690,#66691,#66692,#66693,#66694,#66695,#66696),
 .UNSPECIFIED.,.F.,.F.,(4,2,2,2,2,2,2,2,2,2,2,2,2,2,2,2,2,2,4),(-15.1073443691545,
-15.1011008892937,-15.0437220848592,-14.9840992717133,-14.926190394778,
-14.8681392181562,-14.8084892686686,-14.7514823595925,-14.6927803091387,
-14.6331489331619,-14.5758985339276,-14.5164203125443,-14.4580324516964,
-14.4001023522461,-14.339867608388,-14.2826884114687,-14.2240848432797,
-14.1644203791933,-14.161791521072),.UNSPECIFIED.);
#3254=B_SPLINE_CURVE_WITH_KNOTS('',3,(#66701,#66702,#66703,#66704,#66705,
#66706,#66707,#66708,#66709,#66710,#66711,#66712,#66713,#66714,#66715,#66716,
#66717,#66718,#66719,#66720,#66721,#66722,#66723,#66724,#66725,#66726,#66727,
#66728,#66729,#66730,#66731,#66732,#66733,#66734,#66735,#66736),
 .UNSPECIFIED.,.F.,.F.,(4,2,2,2,2,2,2,2,2,2,2,2,2,2,2,2,2,4),(-14.1885859699234,
-14.1330844909293,-14.0738030834317,-14.0151322001193,-13.9573780431577,
-13.8973369154889,-13.8400747014035,-13.781649842778,-13.7220284098382,
-13.6650669338426,-13.6061313895152,-13.5492060305576,-13.4895868440872,
-13.4312985326842,-13.3738747554208,-13.3139843572995,-13.2563655957482,
-13.2436220538442),.UNSPECIFIED.);
#3255=B_SPLINE_CURVE_WITH_KNOTS('',3,(#66737,#66738,#66739,#66740,#66741,
#66742,#66743,#66744,#66745,#66746,#66747,#66748,#66749,#66750,#66751,#66752,
#66753,#66754,#66755,#66756,#66757,#66758,#66759,#66760,#66761,#66762,#66763,
#66764,#66765,#66766,#66767,#66768,#66769,#66770,#66771,#66772),
 .UNSPECIFIED.,.F.,.F.,(4,2,2,2,2,2,2,2,2,2,2,2,2,2,2,2,2,4),(-14.161791521072,
-14.1073426685626,-14.0480953063394,-13.9892999039839,-13.9315735440484,
-13.8715645099561,-13.8142414960538,-13.7558447627025,-13.6962089327002,
-13.6392486779599,-13.5802573437773,-13.5233108369954,-13.4636758610349,
-13.4053314288153,-13.3479464458854,-13.2879951425265,-13.2303206406094,
-13.2166062380566),.UNSPECIFIED.);
#3256=B_SPLINE_CURVE_WITH_KNOTS('',3,(#66777,#66778,#66779,#66780,#66781,
#66782,#66783,#66784,#66785,#66786,#66787,#66788,#66789,#66790,#66791,#66792,
#66793,#66794,#66795,#66796,#66797,#66798,#66799,#66800,#66801,#66802,#66803,
#66804,#66805,#66806,#66807,#66808,#66809,#66810,#66811,#66812,#66813,#66814),
 .UNSPECIFIED.,.F.,.F.,(4,2,2,2,2,2,2,2,2,2,2,2,2,2,2,2,2,2,4),(-15.1341561055544,
-15.1269994338561,-15.0695799723091,-15.0099125340775,-14.9520739190766,
-14.8939828445778,-14.8343297519005,-14.7773366004228,-14.7185951213641,
-14.6589576423824,-14.6016713251844,-14.5421535644632,-14.4838629359255,
-14.4258987192761,-14.3656251166082,-14.3084824988271,-14.2498440170218,
-14.1901865832963,-14.1885859699234),.UNSPECIFIED.);
#3257=B_SPLINE_CURVE_WITH_KNOTS('',3,(#66815,#66816,#66817,#66818,#66819,
#66820,#66821,#66822,#66823,#66824,#66825,#66826,#66827,#66828,#66829,#66830,
#66831,#66832,#66833,#66834,#66835,#66836,#66837,#66838,#66839,#66840,#66841,
#66842,#66843,#66844,#66845,#66846,#66847,#66848,#66849,#66850),
 .UNSPECIFIED.,.F.,.F.,(4,2,2,2,2,2,2,2,2,2,2,2,2,2,2,2,2,4),(-13.2166062380566,
-13.1713851979337,-13.1121981319385,-13.0551628296182,-12.9955080421381,
-12.9369655576865,-12.8797535453401,-12.819585289645,-12.761715189623,-12.7032194250943,
-12.6438086463492,-12.586620577358,-12.5270150261763,-12.4683803900242,
-12.4113696886299,-12.35174219741,-12.2937588655423,-12.2712695292436),
 .UNSPECIFIED.);
#3258=B_SPLINE_CURVE_WITH_KNOTS('',3,(#66855,#66856,#66857,#66858,#66859,
#66860,#66861,#66862,#66863,#66864,#66865,#66866,#66867,#66868,#66869,#66870,
#66871,#66872,#66873,#66874,#66875,#66876,#66877,#66878,#66879,#66880,#66881,
#66882,#66883,#66884,#66885,#66886,#66887,#66888,#66889,#66890),
 .UNSPECIFIED.,.F.,.F.,(4,2,2,2,2,2,2,2,2,2,2,2,2,2,2,2,2,4),(-16.0791645683298,
-16.0637629880179,-16.0060223350212,-15.9459969234656,-15.8887024341941,
-15.8302912537239,-15.7706612508563,-15.7136999051047,-15.654642811055,
-15.5954057874932,-15.5378426704977,-15.4780146687669,-15.4204898319656,
-15.3622571133794,-15.3026293793744,-15.2456979578477,-15.1868171504776,
-15.1341561055544),.UNSPECIFIED.);
#3259=B_SPLINE_CURVE_WITH_KNOTS('',3,(#66891,#66892,#66893,#66894,#66895,
#66896,#66897,#66898,#66899,#66900,#66901,#66902,#66903,#66904,#66905,#66906,
#66907,#66908,#66909,#66910,#66911,#66912,#66913,#66914,#66915,#66916,#66917,
#66918,#66919,#66920,#66921,#66922,#66923,#66924,#66925,#66926),
 .UNSPECIFIED.,.F.,.F.,(4,2,2,2,2,2,2,2,2,2,2,2,2,2,2,2,2,4),(-12.2712695292436,
-12.2357754508004,-12.1762270533728,-12.1189170680661,-12.0588176303639,
-12.0000655464483,-11.943159299172,-11.8835712422689,-11.8254678956475,
-11.7678321870858,-11.708145031833,-11.6507114242844,-11.5912213696332,
-11.5323122460786,-11.4754266605439,-11.4158513420701,-11.3575887654668,
-11.3269908932583),.UNSPECIFIED.);
#3260=B_SPLINE_CURVE_WITH_KNOTS('',3,(#66931,#66932,#66933,#66934,#66935,
#66936,#66937,#66938,#66939,#66940,#66941,#66942,#66943,#66944,#66945,#66946,
#66947,#66948,#66949,#66950,#66951,#66952,#66953,#66954,#66955,#66956,#66957,
#66958,#66959,#66960,#66961,#66962,#66963,#66964,#66965,#66966),
 .UNSPECIFIED.,.F.,.F.,(4,2,2,2,2,2,2,2,2,2,2,2,2,2,2,2,2,4),(-17.0247741151702,
-17.0006922494049,-16.942620899042,-16.8829683888398,-16.8259674619989,
-16.7672454552544,-16.7076101234707,-16.6503415003102,-16.590843286514,
-16.5325014804607,-16.4745540351945,-16.4142996421448,-16.357137434069,
-16.2985161360182,-16.2388539992256,-16.1817640975146,-16.1224994016558,
-16.0791645683298),.UNSPECIFIED.);
#3261=B_SPLINE_CURVE_WITH_KNOTS('',3,(#66967,#66968,#66969,#66970,#66971,
#66972,#66973,#66974,#66975,#66976,#66977,#66978,#66979,#66980,#66981,#66982,
#66983,#66984,#66985,#66986,#66987,#66988,#66989,#66990,#66991,#66992,#66993,
#66994,#66995,#66996,#66997,#66998,#66999,#67000,#67001,#67002),
 .UNSPECIFIED.,.F.,.F.,(4,2,2,2,2,2,2,2,2,2,2,2,2,2,2,2,2,4),(-11.3269908932583,
-11.3002304831747,-11.2403651502537,-11.1827717007332,-11.1238285355636,
-11.064728011521,-11.0077668972893,-10.9481757635054,-10.8897195155163,
-10.8325471683827,-10.7724692707686,-10.7146842840278,-10.6561946025542,
-10.5968740051404,-10.5397395269343,-10.4801014814801,-10.4214223488875,
-10.3822526002173),.UNSPECIFIED.);
#3262=B_SPLINE_CURVE_WITH_KNOTS('',3,(#67007,#67008,#67009,#67010,#67011,
#67012,#67013,#67014,#67015,#67016,#67017,#67018,#67019,#67020,#67021,#67022,
#67023,#67024,#67025,#67026,#67027,#67028,#67029,#67030,#67031,#67032,#67033,
#67034,#67035,#67036,#67037,#67038,#67039,#67040,#67041,#67042),
 .UNSPECIFIED.,.F.,.F.,(4,2,2,2,2,2,2,2,2,2,2,2,2,2,2,2,2,4),(-17.9696970255303,
-17.937289370862,-17.8789069021961,-17.8192841522869,-17.7623368372575,
-17.7033082433986,-17.6440100001385,-17.5864714106887,-17.526670356869,
-17.4691167328281,-17.4109085209012,-17.3512845924667,-17.2943555190345,
-17.2354990142404,-17.1756126480208,-17.1182132969445,-17.0585679978772,
-17.0247741151702),.UNSPECIFIED.);
#3263=B_SPLINE_CURVE_WITH_KNOTS('',3,(#67043,#67044,#67045,#67046,#67047,
#67048,#67049,#67050,#67051,#67052,#67053,#67054,#67055,#67056,#67057,#67058,
#67059,#67060,#67061,#67062,#67063,#67064,#67065,#67066,#67067,#67068,#67069,
#67070,#67071,#67072,#67073,#67074,#67075,#67076,#67077,#67078),
 .UNSPECIFIED.,.F.,.F.,(4,2,2,2,2,2,2,2,2,2,2,2,2,2,2,2,2,4),(-10.3822526002173,
-10.3643343540307,-10.3046400968479,-10.246613334744,-10.1885181147052,
-10.128927402479,-10.0715754084394,-10.011325400927,-9.9525347708931,-9.89556195447909,
-9.83591091083034,-9.77776999750488,-9.72003077893023,-9.66030722303232,
-9.60283704872725,-9.54320316116386,-9.48426076178981,-9.43689892858011),
 .UNSPECIFIED.);
#3264=B_SPLINE_CURVE_WITH_KNOTS('',3,(#67083,#67084,#67085,#67086,#67087,
#67088,#67089,#67090,#67091,#67092,#67093,#67094,#67095,#67096,#67097,#67098,
#67099,#67100,#67101,#67102,#67103,#67104,#67105,#67106,#67107,#67108,#67109,
#67110,#67111,#67112,#67113,#67114,#67115,#67116,#67117,#67118),
 .UNSPECIFIED.,.F.,.F.,(4,2,2,2,2,2,2,2,2,2,2,2,2,2,2,2,2,4),(-18.9151145034862,
-18.8743164654268,-18.8156291548377,-18.7560115648048,-18.6987754493173,
-18.6393121439161,-18.5809341256596,-18.5230183981635,-18.4627987144582,
-18.4056311968295,-18.3470421802252,-18.2873910545073,-18.2303271150055,
-18.171094421965,-18.1123080260466,-18.0545957689432,-17.9946015046478,
-17.9696970255303),.UNSPECIFIED.);
#3265=B_SPLINE_CURVE_WITH_KNOTS('',3,(#67119,#67120,#67121,#67122,#67123,
#67124,#67125,#67126,#67127,#67128,#67129,#67130,#67131,#67132,#67133,#67134,
#67135,#67136,#67137,#67138,#67139,#67140,#67141,#67142,#67143,#67144,#67145,
#67146,#67147,#67148,#67149,#67150,#67151,#67152,#67153,#67154),
 .UNSPECIFIED.,.F.,.F.,(4,2,2,2,2,2,2,2,2,2,2,2,2,2,2,2,2,4),(-9.43689892858011,
-9.42732171849391,-9.36768738295302,-9.30939248028644,-9.25194272911408,
-9.19204622378449,-9.13442101602013,-9.07534568068709,-9.01621630273034,
-8.95921594082851,-8.89957004368503,-8.84108593111714,-8.78383634874988,
-8.72373170856049,-8.6659190669351,-8.60731272480359,-8.54796686813959,
-8.49156038630827),.UNSPECIFIED.);
#3266=B_SPLINE_CURVE_WITH_KNOTS('',3,(#67159,#67160,#67161,#67162,#67163,
#67164,#67165,#67166,#67167,#67168,#67169,#67170,#67171,#67172,#67173,#67174,
#67175,#67176,#67177,#67178,#67179,#67180,#67181,#67182,#67183,#67184,#67185,
#67186,#67187,#67188,#67189,#67190,#67191,#67192,#67193,#67194),
 .UNSPECIFIED.,.F.,.F.,(4,2,2,2,2,2,2,2,2,2,2,2,2,2,2,2,2,4),(-19.8597382210236,
-19.810451373043,-19.7514667566491,-19.6921219719675,-19.6346229403372,
-19.5748644342208,-19.5172962645061,-19.4591277252691,-19.3995232496075,
-19.3426105099162,-19.2837936446735,-19.2238539608265,-19.1664896413472,
-19.1068819617647,-19.0489837573588,-18.9909471893313,-18.9313109305834,
-18.9151145034862),.UNSPECIFIED.);
#3267=B_SPLINE_CURVE_WITH_KNOTS('',3,(#67195,#67196,#67197,#67198,#67199,
#67200,#67201,#67202,#67203,#67204,#67205,#67206,#67207,#67208,#67209,#67210,
#67211,#67212,#67213,#67214,#67215,#67216,#67217,#67218,#67219,#67220,#67221,
#67222,#67223,#67224,#67225,#67226,#67227,#67228,#67229,#67230,#67231,#67232),
 .UNSPECIFIED.,.F.,.F.,(4,2,2,2,2,2,2,2,2,2,2,2,2,2,2,2,2,2,4),(-8.49156038630827,
-8.49080675575303,-8.43111857134256,-8.37241526446117,-8.31526501763932,
-8.25492233706489,-8.19689441801019,-8.13864530142174,-8.07905854481672,
-8.02170761683104,-7.96202852596394,-7.9032187975688,-7.84619976450985,
-7.78650760972943,-7.72834831916545,-7.67052935317836,-7.61078895216033,
-7.55330118212272,-7.54539583975842),.UNSPECIFIED.);
#3268=B_SPLINE_CURVE_WITH_KNOTS('',3,(#67237,#67238,#67239,#67240,#67241,
#67242,#67243,#67244,#67245,#67246,#67247,#67248,#67249,#67250,#67251,#67252,
#67253,#67254,#67255,#67256,#67257,#67258,#67259,#67260,#67261,#67262,#67263,
#67264,#67265,#67266,#67267,#67268,#67269,#67270,#67271,#67272,#67273,#67274),
 .UNSPECIFIED.,.F.,.F.,(4,2,2,2,2,2,2,2,2,2,2,2,2,2,2,2,2,2,4),(-20.8047268284554,
-20.8036363389145,-20.7464479008663,-20.6870352594353,-20.6286348915891,
-20.5707661629285,-20.510597073108,-20.4534380889162,-20.3948967931479,
-20.3352722771837,-20.2782483009287,-20.219063232801,-20.1602410153004,
-20.1025723093681,-20.0426249323872,-19.9853090960203,-19.9269706384341,
-19.867370764855,-19.8597382210236),.UNSPECIFIED.);
#3269=B_SPLINE_CURVE_WITH_KNOTS('',3,(#67275,#67276,#67277,#67278,#67279,
#67280,#67281,#67282,#67283,#67284,#67285,#67286,#67287,#67288,#67289,#67290,
#67291,#67292,#67293,#67294,#67295,#67296,#67297,#67298,#67299,#67300,#67301,
#67302,#67303,#67304,#67305,#67306,#67307,#67308,#67309,#67310),
 .UNSPECIFIED.,.F.,.F.,(4,2,2,2,2,2,2,2,2,2,2,2,2,2,2,2,2,4),(-7.54539583975842,
-7.49355110204946,-7.43459460077228,-7.37762115395009,-7.31794932817515,
-7.25964100917192,-7.20212210603924,-7.14221371611197,-7.08457547245393,
-7.02539392871746,-6.96625468515904,-6.90923296876007,-6.84955345859718,
-6.79106019408235,-6.73375428080265,-6.6736419972573,-6.61582024058893,
-6.59962043014718),.UNSPECIFIED.);
#3270=B_SPLINE_CURVE_WITH_KNOTS('',3,(#67315,#67316,#67317,#67318,#67319,
#67320,#67321,#67322,#67323,#67324,#67325,#67326,#67327,#67328,#67329,#67330,
#67331,#67332,#67333,#67334,#67335,#67336,#67337,#67338,#67339,#67340,#67341,
#67342,#67343,#67344,#67345,#67346,#67347,#67348,#67349,#67350),
 .UNSPECIFIED.,.F.,.F.,(4,2,2,2,2,2,2,2,2,2,2,2,2,2,2,2,2,4),(-21.7489046572791,
-21.7392153866495,-21.6817714549229,-21.6220716583751,-21.5645025223573,
-21.5063893301253,-21.4468200256293,-21.3899376073178,-21.3311762213552,
-21.2711970668162,-21.2138831121422,-21.1543289862749,-21.0964221879644,
-21.0384358621701,-20.9788315240901,-20.9218575630073,-20.8632205676017,
-20.8047268284554),.UNSPECIFIED.);
#3271=B_SPLINE_CURVE_WITH_KNOTS('',3,(#67351,#67352,#67353,#67354,#67355,
#67356,#67357,#67358,#67359,#67360,#67361,#67362,#67363,#67364,#67365,#67366,
#67367,#67368,#67369,#67370,#67371,#67372,#67373,#67374,#67375,#67376,#67377,
#67378,#67379,#67380,#67381,#67382,#67383,#67384,#67385,#67386),
 .UNSPECIFIED.,.F.,.F.,(4,2,2,2,2,2,2,2,2,2,2,2,2,2,2,2,2,4),(-6.59962043014718,
-6.55712143056447,-6.49776917806976,-6.44060046014423,-6.3808828825634,
-6.32217397813377,-6.26498116754636,-6.20463437850135,-6.14660066752985,
-6.0882749718812,-6.02868466855325,-5.9713291133043,-5.91162795849117,-5.85281481524407,
-5.79576557777481,-5.73604961995392,-5.67788743624381,-5.65305968192749),
 .UNSPECIFIED.);
#3272=B_SPLINE_CURVE_WITH_KNOTS('',3,(#67391,#67392,#67393,#67394,#67395,
#67396,#67397,#67398,#67399,#67400,#67401,#67402,#67403,#67404,#67405,#67406,
#67407,#67408,#67409,#67410,#67411,#67412,#67413,#67414,#67415,#67416,#67417,
#67418,#67419,#67420,#67421,#67422,#67423,#67424,#67425,#67426),
 .UNSPECIFIED.,.F.,.F.,(4,2,2,2,2,2,2,2,2,2,2,2,2,2,2,2,2,4),(-22.6930944862137,
-22.6750742815793,-22.6172685137948,-22.5571666469156,-22.5000298336195,
-22.4415523883347,-22.3819703093803,-22.3250007752965,-22.2658796385637,
-22.2070346049225,-22.1494252073759,-22.0895411174023,-22.0322350703383,
-21.9739565284333,-21.9143953015877,-21.8575179583935,-21.7985933937003,
-21.7489046572791),.UNSPECIFIED.);
#3273=B_SPLINE_CURVE_WITH_KNOTS('',3,(#67427,#67428,#67429,#67430,#67431,
#67432,#67433,#67434,#67435,#67436,#67437,#67438,#67439,#67440,#67441,#67442,
#67443,#67444,#67445,#67446,#67447,#67448,#67449,#67450,#67451,#67452,#67453,
#67454,#67455,#67456,#67457,#67458,#67459,#67460,#67461,#67462),
 .UNSPECIFIED.,.F.,.F.,(4,2,2,2,2,2,2,2,2,2,2,2,2,2,2,2,2,4),(-5.65305968192749,
-5.62000697109407,-5.56026553634326,-5.50277548740805,-5.4429300395589,
-5.38397497750277,-5.32698226097639,-5.2672900308627,-5.20898363219345,
-5.15141280935565,-5.09150820934248,-5.03387211917237,-4.97460397585247,
-4.91547032791341,-4.8584416373336,-4.79874535977046,-4.74025819094778,
-4.7070192889843),.UNSPECIFIED.);
#3274=B_SPLINE_CURVE_WITH_KNOTS('',3,(#67467,#67468,#67469,#67470,#67471,
#67472,#67473,#67474,#67475,#67476,#67477,#67478,#67479,#67480,#67481,#67482,
#67483,#67484,#67485,#67486,#67487,#67488,#67489,#67490,#67491,#67492,#67493,
#67494,#67495,#67496,#67497,#67498,#67499,#67500,#67501,#67502),
 .UNSPECIFIED.,.F.,.F.,(4,2,2,2,2,2,2,2,2,2,2,2,2,2,2,2,2,4),(-23.6367224740298,
-23.6102009889967,-23.5521597036553,-23.4926417159663,-23.435803856614,
-23.3771146729451,-23.3171085926091,-23.2598611088234,-23.2003772998387,
-23.1424751745089,-23.0845553127723,-23.0249989156642,-22.9680595588619,
-22.9094892557851,-22.8499543793008,-22.7928294928815,-22.7334840265615,
-22.6930944862137),.UNSPECIFIED.);
#3275=B_SPLINE_CURVE_WITH_KNOTS('',3,(#67503,#67504,#67505,#67506,#67507,
#67508,#67509,#67510,#67511,#67512,#67513,#67514,#67515,#67516,#67517,#67518,
#67519,#67520,#67521,#67522,#67523,#67524,#67525,#67526,#67527,#67528,#67529,
#67530,#67531,#67532,#67533,#67534,#67535,#67536,#67537,#67538),
 .UNSPECIFIED.,.F.,.F.,(4,2,2,2,2,2,2,2,2,2,2,2,2,2,2,2,2,4),(-4.7070192889843,
-4.68291221701188,-4.62280788263384,-4.56499211835275,-4.50621920975702,
-4.44687598188547,-4.3897125228076,-4.32998213906469,-4.27128283566224,
-4.21406294394457,-4.15372759490239,-4.09570314650131,-4.03731813708901,
-3.97773968458231,-3.92039439080922,-3.86068740451247,-3.80188610698126,
-3.76030733114506),.UNSPECIFIED.);
#3276=B_SPLINE_CURVE_WITH_KNOTS('',3,(#67543,#67544,#67545,#67546,#67547,
#67548,#67549,#67550,#67551,#67552,#67553,#67554,#67555,#67556,#67557,#67558,
#67559,#67560,#67561,#67562,#67563,#67564,#67565,#67566,#67567,#67568,#67569,
#67570,#67571,#67572,#67573,#67574,#67575,#67576,#67577,#67578),
 .UNSPECIFIED.,.F.,.F.,(4,2,2,2,2,2,2,2,2,2,2,2,2,2,2,2,2,4),(-24.5799045977848,
-24.544864402261,-24.4864680402579,-24.4269448204466,-24.3700449713328,
-24.3110051741305,-24.2521492970098,-24.1946159613695,-24.1348126294181,
-24.0775296073419,-24.0193278864891,-23.9598215850082,-23.9030009070175,
-23.8441534701742,-23.7847543450619,-23.7273819445697,-23.667757974583,
-23.6367224740298),.UNSPECIFIED.);
#3277=B_SPLINE_CURVE_WITH_KNOTS('',3,(#67579,#67580,#67581,#67582,#67583,
#67584,#67585,#67586,#67587,#67588,#67589,#67590,#67591,#67592,#67593,#67594,
#67595,#67596,#67597,#67598,#67599,#67600,#67601,#67602,#67603,#67604,#67605,
#67606,#67607,#67608,#67609,#67610,#67611,#67612,#67613,#67614),
 .UNSPECIFIED.,.F.,.F.,(4,2,2,2,2,2,2,2,2,2,2,2,2,2,2,2,2,4),(-3.76030733114506,
-3.74482173076156,-3.6850983260828,-3.62694832744347,-3.56902286769636,
-3.50929583899485,-3.45181843527126,-3.39189585023894,-3.33295745069471,
-3.27595993809932,-3.21626352613547,-3.15797408399984,-3.1003669659872,
-3.04048156422391,-2.98286252158158,-2.92352507208656,-2.86441225193454,
-2.81422223630842),.UNSPECIFIED.);
#3278=B_SPLINE_CURVE_WITH_KNOTS('',3,(#67619,#67620,#67621,#67622,#67623,
#67624,#67625,#67626,#67627,#67628,#67629,#67630,#67631,#67632,#67633,#67634,
#67635,#67636,#67637,#67638,#67639,#67640,#67641,#67642,#67643,#67644,#67645,
#67646,#67647,#67648,#67649,#67650,#67651,#67652,#67653,#67654),
 .UNSPECIFIED.,.F.,.F.,(4,2,2,2,2,2,2,2,2,2,2,2,2,2,2,2,2,4),(-25.5227587485597,
-25.47965708315,-25.421058174348,-25.361036462416,-25.3038727637219,-25.2444773184052,
-25.1865926949701,-25.128756714116,-25.0692650147963,-25.0123746718861,
-24.9538886316087,-24.8944198504469,-24.8373755091807,-24.7781149174187,
-24.7197080007783,-24.6619822469935,-24.6019654058989,-24.5799045977848),
 .UNSPECIFIED.);
#3279=B_SPLINE_CURVE_WITH_KNOTS('',3,(#67655,#67656,#67657,#67658,#67659,
#67660,#67661,#67662,#67663,#67664,#67665,#67666,#67667,#67668,#67669,#67670,
#67671,#67672,#67673,#67674,#67675,#67676,#67677,#67678,#67679,#67680,#67681,
#67682,#67683,#67684,#67685,#67686,#67687,#67688,#67689,#67690,#67691,#67692),
 .UNSPECIFIED.,.F.,.F.,(4,2,2,2,2,2,2,2,2,2,2,2,2,2,2,2,2,2,4),(-2.81422223630842,
-2.80739059809379,-2.74769363128926,-2.68922759545975,-2.63185666495599,
-2.57177569602702,-2.51398082031509,-2.45515020591261,-2.39583126811454,
-2.3386868262193,-2.27895955966271,-2.22028492138649,-2.16305256653281,
-2.1027441052407,-2.04474383487291,-1.98631516239258,-1.92676386570169,
-1.86944360522889,-1.86759610747369),.UNSPECIFIED.);
#3280=B_SPLINE_CURVE_WITH_KNOTS('',3,(#67697,#67698,#67699,#67700,#67701,
#67702,#67703,#67704,#67705,#67706,#67707,#67708,#67709,#67710,#67711,#67712,
#67713,#67714,#67715,#67716,#67717,#67718,#67719,#67720,#67721,#67722,#67723,
#67724,#67725,#67726,#67727,#67728,#67729,#67730,#67731,#67732),
 .UNSPECIFIED.,.F.,.F.,(4,2,2,2,2,2,2,2,2,2,2,2,2,2,2,2,2,4),(-26.4647006629411,
-26.4128164821547,-26.3538770628634,-26.295021282913,-26.2375822529352,
-26.1778787398139,-26.1206318744523,-26.0625253754812,-26.0030911980923,
-25.9463425849355,-25.8875908503495,-25.8281815100278,-25.7708984260118,
-25.7113688412011,-25.6538368035759,-25.595885334023,-25.5364356344578,
-25.5227587485597),.UNSPECIFIED.);
#3281=B_SPLINE_CURVE_WITH_KNOTS('',3,(#67733,#67734,#67735,#67736,#67737,
#67738,#67739,#67740,#67741,#67742,#67743,#67744,#67745,#67746,#67747,#67748,
#67749,#67750,#67751,#67752,#67753,#67754,#67755,#67756,#67757,#67758,#67759,
#67760,#67761,#67762,#67763,#67764,#67765,#67766,#67767,#67768),
 .UNSPECIFIED.,.F.,.F.,(4,2,2,2,2,2,2,2,2,2,2,2,2,2,2,2,2,4),(-1.86759610747369,
-1.8097465170722,-1.7509722323765,-1.69390716991027,-1.63419213717573,-1.57606932036452,
-1.51811407870063,-1.45841685307261,-1.40096694869804,-1.34098343757821,
-1.28207692999559,-1.22508871615811,-1.16540388332849,-1.10714645181714,
-1.0495176707267,-0.989666932708261,-0.932079853846146,-0.921606618540025),
 .UNSPECIFIED.);
#3282=B_SPLINE_CURVE_WITH_KNOTS('',3,(#67774,#67775,#67776,#67777,#67778,
#67779,#67780,#67781,#67782,#67783,#67784,#67785,#67786,#67787,#67788,#67789,
#67790,#67791,#67792,#67793),.UNSPECIFIED.,.F.,.F.,(4,2,2,2,2,2,2,2,2,4),
(9.99987117032003E-7,0.0282047267175922,0.0500972781633209,0.077222937740314,
0.107624298477487,0.137340418712146,0.157932276880896,0.175135732483776,
0.191462844907497,0.203440126186273),.UNSPECIFIED.);
#3283=B_SPLINE_CURVE_WITH_KNOTS('',3,(#67799,#67800,#67801,#67802,#67803,
#67804,#67805,#67806),.UNSPECIFIED.,.F.,.F.,(4,2,2,4),(21.4315064013737,
21.4634357935859,21.4930318613417,21.5226265917604),.UNSPECIFIED.);
#3284=B_SPLINE_CURVE_WITH_KNOTS('',3,(#67812,#67813,#67814,#67815,#67816,
#67817,#67818,#67819,#67820,#67821,#67822,#67823,#67824,#67825,#67826,#67827,
#67828,#67829,#67830,#67831,#67832,#67833,#67834,#67835,#67836,#67837,#67838,
#67839,#67840,#67841,#67842,#67843,#67844,#67845,#67846,#67847),
 .UNSPECIFIED.,.F.,.F.,(4,2,2,2,2,2,2,2,2,2,2,2,2,2,2,2,2,4),(20.6936878716818,
20.7322285263897,20.7783057175789,20.8227795047066,20.8693557730982,20.9149428892879,
20.9597524851927,21.0065846852777,21.0516438851204,21.0976519395239,21.1438788790039,
21.188432473727,21.2350392941589,21.2807854576605,21.3254925240272,21.3724982892632,
21.417717724476,21.4315064013737),.UNSPECIFIED.);
#3285=B_SPLINE_CURVE_WITH_KNOTS('',3,(#67848,#67849,#67850,#67851,#67852,
#67853,#67854,#67855,#67856,#67857,#67858,#67859,#67860,#67861,#67862,#67863,
#67864,#67865,#67866,#67867,#67868,#67869,#67870,#67871,#67872,#67873,#67874,
#67875,#67876,#67877,#67878,#67879,#67880,#67881,#67882,#67883),
 .UNSPECIFIED.,.F.,.F.,(4,2,2,2,2,2,2,2,2,2,2,2,2,2,2,2,2,4),(9.99999999753597E-7,
0.0364903991492045,0.0742057367939146,0.120984278340417,0.165716260437277,
0.212135354668823,0.258243398942271,0.303486376579508,0.350510827449709,
0.395451299070227,0.441223703670797,0.487964967533294,0.532602258835938,
0.578864855147042,0.625329100321987,0.670440021753448,0.717320863549735,
0.740262878339932),.UNSPECIFIED.);
#3286=B_SPLINE_CURVE_WITH_KNOTS('',3,(#67888,#67889,#67890,#67891,#67892,
#67893,#67894,#67895,#67896,#67897,#67898,#67899,#67900,#67901,#67902,#67903,
#67904,#67905,#67906,#67907,#67908,#67909,#67910,#67911,#67912,#67913,#67914,
#67915,#67916,#67917,#67918,#67919,#67920,#67921,#67922,#67923),
 .UNSPECIFIED.,.F.,.F.,(4,2,2,2,2,2,2,2,2,2,2,2,2,2,2,2,2,4),(19.9559680414516,
20.0008504784901,20.0467368410681,20.0912761832143,20.1378918451635,20.1832739295335,
20.2285046006904,20.275104513086,20.3199511087905,20.366754624975,20.4127173643503,
20.4571887454312,20.5037686894442,20.5492336658488,20.5942218762843,20.6409180608554,
20.6858523218674,20.6936878716818),.UNSPECIFIED.);
#3287=B_SPLINE_CURVE_WITH_KNOTS('',3,(#67924,#67925,#67926,#67927,#67928,
#67929,#67930,#67931,#67932,#67933,#67934,#67935,#67936,#67937,#67938,#67939,
#67940,#67941,#67942,#67943,#67944,#67945,#67946,#67947,#67948,#67949,#67950,
#67951,#67952,#67953,#67954,#67955,#67956,#67957,#67958,#67959),
 .UNSPECIFIED.,.F.,.F.,(4,2,2,2,2,2,2,2,2,2,2,2,2,2,2,2,2,4),(0.740262878339932,
0.762427102215096,0.808069985401053,0.854808846272841,0.899429812570394,
0.945570872042072,0.992454683227221,1.03747065146669,1.08424743869661,1.12958660656193,
1.175138889682,1.22190780149668,1.26658471043468,1.31264188421903,1.35939848501362,
1.4043392205548,1.45103260193205,1.48067239646651),.UNSPECIFIED.);
#3288=B_SPLINE_CURVE_WITH_KNOTS('',3,(#67964,#67965,#67966,#67967,#67968,
#67969,#67970,#67971,#67972,#67973,#67974,#67975,#67976,#67977,#67978,#67979,
#67980,#67981,#67982,#67983,#67984,#67985,#67986,#67987,#67988,#67989,#67990,
#67991,#67992,#67993,#67994,#67995,#67996,#67997,#67998,#67999,#68000,#68001),
 .UNSPECIFIED.,.F.,.F.,(4,2,2,2,2,2,2,2,2,2,2,2,2,2,2,2,2,2,4),(19.2175408288878,
19.2219373965907,19.2685210725085,19.3141891378125,19.3589248216993,19.4058460198647,
19.4509870738391,19.4968133764095,19.5431350504829,19.5877640910998,19.6343990565288,
19.6802461513431,19.72492597093,19.7720411959568,19.8173618084826,19.8629496498953,
19.9094715861334,19.954248068259,19.9559680414516),.UNSPECIFIED.);
#3289=B_SPLINE_CURVE_WITH_KNOTS('',3,(#68002,#68003,#68004,#68005,#68006,
#68007,#68008,#68009,#68010,#68011,#68012,#68013,#68014,#68015,#68016,#68017,
#68018,#68019,#68020,#68021,#68022,#68023,#68024,#68025,#68026,#68027,#68028,
#68029,#68030,#68031,#68032,#68033,#68034,#68035,#68036,#68037),
 .UNSPECIFIED.,.F.,.F.,(4,2,2,2,2,2,2,2,2,2,2,2,2,2,2,2,2,4),(1.48067239646651,
1.49671326012625,1.54219831558785,1.5894859449329,1.63428944893413,1.68030245144421,
1.72708174969527,1.77186789842175,1.81835464146615,1.86425678940839,1.90955548631379,
1.95664189809396,2.00148568453804,2.0473126858144,2.0940334671172,2.13867975719358,
2.18499121801513,2.22108960850334),.UNSPECIFIED.);
#3290=B_SPLINE_CURVE_WITH_KNOTS('',3,(#68042,#68043,#68044,#68045,#68046,
#68047,#68048,#68049,#68050,#68051,#68052,#68053,#68054,#68055,#68056,#68057,
#68058,#68059,#68060,#68061,#68062,#68063,#68064,#68065,#68066,#68067,#68068,
#68069,#68070,#68071,#68072,#68073,#68074,#68075,#68076,#68077),
 .UNSPECIFIED.,.F.,.F.,(4,2,2,2,2,2,2,2,2,2,2,2,2,2,2,2,2,4),(18.4801374015765,
18.4907658335562,18.5373515680576,18.5827705444335,18.6278503823358,18.6744946234866,
18.7193811539994,18.7659288026933,18.8119468369207,18.8564049550709,18.9029730508313,
18.9484975984601,18.9933693854802,19.0401328543241,19.0851285772229,19.1312801323088,
19.1774331204032,19.2175408288878),.UNSPECIFIED.);
#3291=B_SPLINE_CURVE_WITH_KNOTS('',3,(#68078,#68079,#68080,#68081,#68082,
#68083,#68084,#68085,#68086,#68087,#68088,#68089,#68090,#68091,#68092,#68093,
#68094,#68095,#68096,#68097,#68098,#68099,#68100,#68101,#68102,#68103,#68104,
#68105,#68106,#68107,#68108,#68109,#68110,#68111,#68112,#68113),
 .UNSPECIFIED.,.F.,.F.,(4,2,2,2,2,2,2,2,2,2,2,2,2,2,2,2,2,4),(2.22108960850334,
2.23120408655543,2.27635041769103,2.32327161206725,2.368237212408,2.41391337637609,
2.46061197050217,2.50519713949817,2.5513666691862,2.59796482416004,2.64299465171328,
2.68978881476098,2.73495033654449,2.78051325760178,2.82722340804027,2.87182391079689,
2.91788757586549,2.96056667106229),.UNSPECIFIED.);
#3292=B_SPLINE_CURVE_WITH_KNOTS('',3,(#68118,#68119,#68120,#68121,#68122,
#68123,#68124,#68125,#68126,#68127,#68128,#68129,#68130,#68131,#68132,#68133,
#68134,#68135,#68136,#68137,#68138,#68139,#68140,#68141,#68142,#68143,#68144,
#68145,#68146,#68147,#68148,#68149,#68150,#68151,#68152,#68153),
 .UNSPECIFIED.,.F.,.F.,(4,2,2,2,2,2,2,2,2,2,2,2,2,2,2,2,2,4),(17.7416164546727,
17.7581937026132,17.8052897667917,17.8505949548622,17.8963342504639,17.9428341472151,
17.9875910340227,18.0342105180494,18.0800707723051,18.124652551507,18.1712871824617,
18.2166406572815,18.2619848045744,18.3085503929415,18.3533657882032,18.4003592098579,
18.446278791736,18.4801374015765),.UNSPECIFIED.);
#3293=B_SPLINE_CURVE_WITH_KNOTS('',3,(#68154,#68155,#68156,#68157,#68158,
#68159,#68160,#68161,#68162,#68163,#68164,#68165,#68166,#68167,#68168,#68169,
#68170,#68171,#68172,#68173,#68174,#68175,#68176,#68177,#68178,#68179,#68180,
#68181,#68182,#68183,#68184,#68185,#68186,#68187,#68188,#68189,#68190,#68191),
 .UNSPECIFIED.,.F.,.F.,(4,2,2,2,2,2,2,2,2,2,2,2,2,2,2,2,2,2,4),(2.96056667106229,
2.96492507840458,3.00987622748865,3.05658369115965,3.10200096713613,3.14749048109044,
3.19424386894225,3.23892780465305,3.28492439308362,3.33166335864177,3.3765506531,
3.42318675517329,3.46898366970959,3.51441887461108,3.56165143931351,3.60649480370264,
3.65245839321213,3.69924258617203,3.70124435567),.UNSPECIFIED.);
#3294=B_SPLINE_CURVE_WITH_KNOTS('',3,(#68196,#68197,#68198,#68199,#68200,
#68201,#68202,#68203,#68204,#68205,#68206,#68207,#68208,#68209,#68210,#68211,
#68212,#68213,#68214,#68215,#68216,#68217,#68218,#68219,#68220,#68221,#68222,
#68223,#68224,#68225,#68226,#68227,#68228,#68229,#68230,#68231),
 .UNSPECIFIED.,.F.,.F.,(4,2,2,2,2,2,2,2,2,2,2,2,2,2,2,2,2,4),(17.002935008964,
17.0259159067871,17.0726902796453,17.117698909592,17.1640720079207,17.2102290646699,
17.2547667636235,17.301404789293,17.3470724875982,17.391917818806,17.4388344123328,
17.4839738011972,17.5299894371059,17.5763017108472,17.6209316820209,17.6676058954979,
17.7134384045876,17.7416164546727),.UNSPECIFIED.);
#3295=B_SPLINE_CURVE_WITH_KNOTS('',3,(#68232,#68233,#68234,#68235,#68236,
#68237,#68238,#68239,#68240,#68241,#68242,#68243,#68244,#68245,#68246,#68247,
#68248,#68249,#68250,#68251,#68252,#68253,#68254,#68255,#68256,#68257,#68258,
#68259,#68260,#68261,#68262,#68263,#68264,#68265,#68266,#68267),
 .UNSPECIFIED.,.F.,.F.,(4,2,2,2,2,2,2,2,2,2,2,2,2,2,2,2,2,4),(3.70124435567,
3.74399270352421,3.79043516379055,3.83649298289209,3.88175593971899,3.92880219425985,
3.97372113000247,4.01951325018307,4.0662546751028,4.11089815702418,4.15717909203302,
4.20358177465394,4.24870726106109,4.29560414076508,4.34067748019848,4.38633433906348,
4.43306819834531,4.44139309323576),.UNSPECIFIED.);
#3296=B_SPLINE_CURVE_WITH_KNOTS('',3,(#68272,#68273,#68274,#68275,#68276,
#68277,#68278,#68279,#68280,#68281,#68282,#68283,#68284,#68285,#68286,#68287,
#68288,#68289,#68290,#68291,#68292,#68293,#68294,#68295,#68296,#68297,#68298,
#68299,#68300,#68301,#68302,#68303,#68304,#68305,#68306,#68307),
 .UNSPECIFIED.,.F.,.F.,(4,2,2,2,2,2,2,2,2,2,2,2,2,2,2,2,2,4),(16.2641372477882,
16.2938030439013,16.3403922128616,16.3852327649267,16.4318876926505,16.4778418228271,
16.5224230010358,16.5690903677485,16.6145405429621,16.6597873151308,16.7064589317587,
16.7513738187352,16.7981669545333,16.8442036947422,16.8887271733991,16.9353636748532,
16.9809031318305,17.002935008964),.UNSPECIFIED.);
#3297=B_SPLINE_CURVE_WITH_KNOTS('',3,(#68308,#68309,#68310,#68311,#68312,
#68313,#68314,#68315,#68316,#68317,#68318,#68319,#68320,#68321,#68322,#68323,
#68324,#68325,#68326,#68327,#68328,#68329,#68330,#68331,#68332,#68333,#68334,
#68335,#68336,#68337,#68338,#68339,#68340,#68341,#68342,#68343),
 .UNSPECIFIED.,.F.,.F.,(4,2,2,2,2,2,2,2,2,2,2,2,2,2,2,2,2,4),(4.44139309323576,
4.47768369479005,4.52383758291686,4.57065155177945,4.61567630686354,4.66246297203597,
4.70776020748785,4.7533204420323,4.80007956137218,4.8447406734777,4.8908048094463,
4.93755248955131,4.98249808878681,5.02919719884178,5.0748218415068,5.12031038865077,
5.16760288129374,5.1818539671131),.UNSPECIFIED.);
#3298=B_SPLINE_CURVE_WITH_KNOTS('',3,(#68348,#68349,#68350,#68351,#68352,
#68353,#68354,#68355,#68356,#68357,#68358,#68359,#68360,#68361,#68362,#68363,
#68364,#68365,#68366,#68367,#68368,#68369,#68370,#68371,#68372,#68373,#68374,
#68375,#68376,#68377,#68378,#68379,#68380,#68381,#68382,#68383),
 .UNSPECIFIED.,.F.,.F.,(4,2,2,2,2,2,2,2,2,2,2,2,2,2,2,2,2,4),(15.5253008226521,
15.5614208712953,15.6076307463169,15.6521806514462,15.6988024510405,15.7445285973342,
15.7892808885852,15.8362633798431,15.8814623032694,15.9272761463232,15.9736600003967,
16.0183472154503,16.0650263145743,16.1109370835491,16.1556467547297,16.2028290254408,
16.2482129532865,16.2641372477882),.UNSPECIFIED.);
#3299=B_SPLINE_CURVE_WITH_KNOTS('',3,(#68384,#68385,#68386,#68387,#68388,
#68389,#68390,#68391,#68392,#68393,#68394,#68395,#68396,#68397,#68398,#68399,
#68400,#68401,#68402,#68403,#68404,#68405,#68406,#68407,#68408,#68409,#68410,
#68411,#68412,#68413,#68414,#68415,#68416,#68417,#68418,#68419),
 .UNSPECIFIED.,.F.,.F.,(4,2,2,2,2,2,2,2,2,2,2,2,2,2,2,2,2,4),(5.1818539671131,
5.21237880454505,5.258394968262,5.30515700825967,5.34994371692685,5.39643143835995,
5.44226233196025,5.48755936077848,5.53464520113254,5.57944804045745,5.62527291369698,
5.67197040786348,5.71660500923211,5.76291244064308,5.80904038797896,5.85417959966551,
5.90109443452282,5.92163532828753),.UNSPECIFIED.);
#3300=B_SPLINE_CURVE_WITH_KNOTS('',3,(#68424,#68425,#68426,#68427,#68428,
#68429,#68430,#68431,#68432,#68433,#68434,#68435,#68436,#68437,#68438,#68439,
#68440,#68441,#68442,#68443,#68444,#68445,#68446,#68447,#68448,#68449,#68450,
#68451,#68452,#68453,#68454,#68455,#68456,#68457,#68458,#68459),
 .UNSPECIFIED.,.F.,.F.,(4,2,2,2,2,2,2,2,2,2,2,2,2,2,2,2,2,4),(14.7873695620709,
14.8300506862385,14.8760153817406,14.9205240016754,14.9671371535707,15.0126019576596,
15.0576755801971,15.1043686547149,15.149301357282,15.1958140370104,15.2418832855322,
15.286374482974,15.3329751561295,15.3785518380475,15.4234279626835,15.4702466599603,
15.5152945505239,15.5253008226521),.UNSPECIFIED.);
#3301=B_SPLINE_CURVE_WITH_KNOTS('',3,(#68460,#68461,#68462,#68463,#68464,
#68465,#68466,#68467,#68468,#68469,#68470,#68471,#68472,#68473,#68474,#68475,
#68476,#68477,#68478,#68479,#68480,#68481,#68482,#68483,#68484,#68485,#68486,
#68487,#68488,#68489,#68490,#68491,#68492,#68493,#68494,#68495),
 .UNSPECIFIED.,.F.,.F.,(4,2,2,2,2,2,2,2,2,2,2,2,2,2,2,2,2,4),(5.92163532828753,
5.94600637034905,5.99167472503286,6.03834442621258,6.08290534138804,6.12906543193699,
6.17556776582538,6.22058468374404,6.26736631647045,6.31246290290152,6.358011917132,
6.40468792773244,6.44925237282631,6.4953007135921,6.54223498706927,6.58716711269207,
6.63385553062737,6.66068791027176),.UNSPECIFIED.);
#3302=B_SPLINE_CURVE_WITH_KNOTS('',3,(#68500,#68501,#68502,#68503,#68504,
#68505,#68506,#68507,#68508,#68509,#68510,#68511,#68512,#68513,#68514,#68515,
#68516,#68517,#68518,#68519,#68520,#68521,#68522,#68523,#68524,#68525,#68526,
#68527,#68528,#68529,#68530,#68531,#68532,#68533,#68534,#68535,#68536,#68537),
 .UNSPECIFIED.,.F.,.F.,(4,2,2,2,2,2,2,2,2,2,2,2,2,2,2,2,2,2,4),(14.0482100339955,
14.0502949245492,14.096984232057,14.142851009537,14.1876060347159,14.2347388331608,
14.2800782706825,14.3257899974572,14.3723273782223,14.41711976203,14.463762437258,
14.5096613573186,14.55425504223,14.6009122351073,14.6463049690835,14.6916352778898,
14.7382430334376,14.7830983471007,14.7873695620709),.UNSPECIFIED.);
#3303=B_SPLINE_CURVE_WITH_KNOTS('',3,(#68538,#68539,#68540,#68541,#68542,
#68543,#68544,#68545,#68546,#68547,#68548,#68549,#68550,#68551,#68552,#68553,
#68554,#68555,#68556,#68557,#68558,#68559,#68560,#68561,#68562,#68563,#68564,
#68565,#68566,#68567,#68568,#68569,#68570,#68571,#68572,#68573),
 .UNSPECIFIED.,.F.,.F.,(4,2,2,2,2,2,2,2,2,2,2,2,2,2,2,2,2,4),(6.66068791027176,
6.67919937428358,6.72466854077273,6.77138281680808,6.8160205136328,6.86199546468963,
6.90869606620136,6.95356006101863,7.00017259357045,7.04588152905359,7.09129151458587,
7.13849904618301,7.1832836822818,7.22922137847032,7.27595882272717,7.32067836819823,
7.3670926336791,7.40074313214862),.UNSPECIFIED.);
#3304=B_SPLINE_CURVE_WITH_KNOTS('',3,(#68578,#68579,#68580,#68581,#68582,
#68583,#68584,#68585,#68586,#68587,#68588,#68589,#68590,#68591,#68592,#68593,
#68594,#68595,#68596,#68597,#68598,#68599,#68600,#68601,#68602,#68603,#68604,
#68605,#68606,#68607,#68608,#68609,#68610,#68611,#68612,#68613),
 .UNSPECIFIED.,.F.,.F.,(4,2,2,2,2,2,2,2,2,2,2,2,2,2,2,2,2,4),(13.3095464675158,
13.3179418806692,13.3645829204745,13.4101456027589,13.4551345123131,13.5019343594699,
13.5469666402861,13.5932875705783,13.6394722908042,13.6840250076321,13.7306726518614,
13.7763692796775,13.8212020202917,13.8681498816812,13.9133183606713,13.9592929931832,
14.0056379903772,14.0482100339955),.UNSPECIFIED.);
#3305=B_SPLINE_CURVE_WITH_KNOTS('',3,(#68614,#68615,#68616,#68617,#68618,
#68619,#68620,#68621,#68622,#68623,#68624,#68625,#68626,#68627,#68628,#68629,
#68630,#68631,#68632,#68633,#68634,#68635,#68636,#68637,#68638,#68639,#68640,
#68641,#68642,#68643,#68644,#68645,#68646,#68647,#68648,#68649),
 .UNSPECIFIED.,.F.,.F.,(4,2,2,2,2,2,2,2,2,2,2,2,2,2,2,2,2,4),(7.40074313214862,
7.41304791193527,7.45828058796883,7.50529645981043,7.55014367964178,7.59590467610001,
7.64259365979734,7.68719438829927,7.73344217485688,7.77972977945611,7.82481959518803,
7.87168035903332,7.91667006179515,7.96229014337893,8.00896624300127,8.05352690669973,
8.09964223179755,8.13994719566162),.UNSPECIFIED.);
#3306=B_SPLINE_CURVE_WITH_KNOTS('',3,(#68654,#68655,#68656,#68657,#68658,
#68659,#68660,#68661,#68662,#68663,#68664,#68665,#68666,#68667,#68668,#68669,
#68670,#68671,#68672,#68673,#68674,#68675,#68676,#68677,#68678,#68679,#68680,
#68681,#68682,#68683,#68684,#68685,#68686,#68687,#68688,#68689),
 .UNSPECIFIED.,.F.,.F.,(4,2,2,2,2,2,2,2,2,2,2,2,2,2,2,2,2,4),(12.5705412100685,
12.5848546363202,12.6320513419363,12.6774479779185,12.7229914291377,12.7695957874756,
12.8144503148156,12.8611058709474,12.9070763074098,12.951650697705,12.9983178350321,
13.0437851961517,13.0889992823918,13.1356902587469,13.1806230630583,13.2273560115123,
13.2734149408359,13.3095464675158),.UNSPECIFIED.);
#3307=B_SPLINE_CURVE_WITH_KNOTS('',3,(#68690,#68691,#68692,#68693,#68694,
#68695,#68696,#68697,#68698,#68699,#68700,#68701,#68702,#68703,#68704,#68705,
#68706,#68707,#68708,#68709,#68710,#68711,#68712,#68713,#68714,#68715,#68716,
#68717,#68718,#68719,#68720,#68721,#68722,#68723,#68724,#68725,#68726,#68727),
 .UNSPECIFIED.,.F.,.F.,(4,2,2,2,2,2,2,2,2,2,2,2,2,2,2,2,2,2,4),(8.13994719566162,
8.1463316268328,8.19131496388372,8.2380593874591,8.28326280667136,8.33020598996195,
8.37537161294956,8.42146167930536,8.46779890512908,8.51245656585315,8.55916791039741,
8.60502388501555,8.64982522039719,8.69694438308839,8.7422725099988,8.78807715134522,
8.83459899420235,8.87937738670119,8.87958134265245),.UNSPECIFIED.);
#3308=B_SPLINE_CURVE_WITH_KNOTS('',3,(#68732,#68733,#68734,#68735,#68736,
#68737,#68738,#68739,#68740,#68741,#68742,#68743,#68744,#68745,#68746,#68747,
#68748,#68749,#68750,#68751,#68752,#68753,#68754,#68755,#68756,#68757,#68758,
#68759,#68760,#68761,#68762,#68763,#68764,#68765,#68766,#68767),
 .UNSPECIFIED.,.F.,.F.,(4,2,2,2,2,2,2,2,2,2,2,2,2,2,2,2,2,4),(11.8321815561307,
11.8527802750529,11.8996021687833,11.9446521456017,11.9907033317147,12.0369186139489,
12.0814657613186,12.1280739153687,12.1738072480122,12.2185277557899,12.2655192350349,
12.3107256977114,12.3564778448273,12.4028721237148,12.4475687949672,12.4942402335744,
12.5401634891127,12.5705412100685),.UNSPECIFIED.);
#3309=B_SPLINE_CURVE_WITH_KNOTS('',3,(#68768,#68769,#68770,#68771,#68772,
#68773,#68774,#68775,#68776,#68777,#68778,#68779,#68780,#68781,#68782,#68783,
#68784,#68785,#68786,#68787,#68788,#68789,#68790,#68791,#68792,#68793,#68794,
#68795,#68796,#68797,#68798,#68799,#68800,#68801,#68802,#68803),
 .UNSPECIFIED.,.F.,.F.,(4,2,2,2,2,2,2,2,2,2,2,2,2,2,2,2,2,4),(8.87958134265245,
8.92602852613987,8.97190922554665,9.01652860508801,9.06319528540556,9.10856829663463,
9.15396816684055,9.20055253946269,9.24538645185148,9.29245567553163,9.33839133852289,
9.38290947461184,9.42952391977244,9.47495799934766,9.52008834525836,9.56674688093536,
9.6116477128901,9.61793661341104),.UNSPECIFIED.);
#3310=B_SPLINE_CURVE_WITH_KNOTS('',3,(#68808,#68809,#68810,#68811,#68812,
#68813,#68814,#68815,#68816,#68817,#68818,#68819,#68820,#68821,#68822,#68823,
#68824,#68825,#68826,#68827,#68828,#68829,#68830,#68831,#68832,#68833,#68834,
#68835,#68836,#68837,#68838,#68839,#68840,#68841,#68842,#68843),
 .UNSPECIFIED.,.F.,.F.,(4,2,2,2,2,2,2,2,2,2,2,2,2,2,2,2,2,4),(11.0945157929649,
11.1213867420797,11.1679850354348,11.212830558321,11.2596899586864,11.3056487691199,
11.3501304725593,11.3967192229775,11.4421794409724,11.4871976310158,11.5338877382452,
11.5788167443302,11.6252436424475,11.6713128846608,11.7157888443594,11.7623703136435,
11.8079484981885,11.8321815561307),.UNSPECIFIED.);
#3311=B_SPLINE_CURVE_WITH_KNOTS('',3,(#68844,#68845,#68846,#68847,#68848,
#68849,#68850,#68851,#68852,#68853,#68854,#68855,#68856,#68857,#68858,#68859,
#68860,#68861,#68862,#68863,#68864,#68865,#68866,#68867,#68868,#68869,#68870,
#68871,#68872,#68873,#68874,#68875,#68876,#68877,#68878,#68879),
 .UNSPECIFIED.,.F.,.F.,(4,2,2,2,2,2,2,2,2,2,2,2,2,2,2,2,2,4),(9.61793661341104,
9.65826687912693,9.70429689093938,9.74877836477337,9.79537166131895,9.84090708321871,
9.88582218876157,9.93259567749554,9.97760169196064,10.0238180381891,10.0699792278232,
10.1144983947581,10.1611035398683,10.2067785301348,10.2515491657397,10.2984763720027,
10.3436239452287,10.3558181882677),.UNSPECIFIED.);
#3312=B_SPLINE_CURVE_WITH_KNOTS('',3,(#68884,#68885,#68886,#68887,#68888,
#68889,#68890,#68891,#68892,#68893,#68894,#68895,#68896,#68897,#68898,#68899,
#68900,#68901,#68902,#68903,#68904,#68905,#68906,#68907,#68908,#68909,#68910,
#68911,#68912,#68913,#68914,#68915,#68916,#68917,#68918,#68919),
 .UNSPECIFIED.,.F.,.F.,(4,2,2,2,2,2,2,2,2,2,2,2,2,2,2,2,2,4),(10.3558181865992,
10.3895062288278,10.4358326314552,10.4804680791543,10.5271205064737,10.5729708577389,
10.6176765737363,10.6647940480184,10.710117621532,10.7557512885806,10.8022746889798,
10.8470530120057,10.8936670905081,10.9395538338801,10.9841105681321,11.0307384394129,
11.0761201700909,11.0945157929649),.UNSPECIFIED.);
#3313=B_SPLINE_CURVE_WITH_KNOTS('',3,(#68920,#68921,#68922,#68923,#68924,
#68925,#68926,#68927,#68928,#68929,#68930,#68931,#68932,#68933,#68934,#68935,
#68936,#68937,#68938,#68939,#68940,#68941,#68942,#68943,#68944,#68945,#68946,
#68947,#68948,#68949,#68950,#68951,#68952,#68953,#68954,#68955),
 .UNSPECIFIED.,.F.,.F.,(4,2,2,2,2,2,2,2,2,2,2,2,2,2,2,2,2,4),(10.3558181882677,
10.3895062304569,10.4358326331012,10.4804680808162,10.5271205081509,10.572970859433,
10.6176765754436,10.6647940497431,10.7101176232735,10.7557512903329,10.8022746907493,
10.8470530137919,10.8936670923103,10.9395538356998,10.9841105699663,11.0307384412633,
11.0761201719588,11.0945157948807),.UNSPECIFIED.);
#3314=B_SPLINE_CURVE_WITH_KNOTS('',3,(#68960,#68961,#68962,#68963,#68964,
#68965,#68966,#68967,#68968,#68969,#68970,#68971,#68972,#68973,#68974,#68975,
#68976,#68977,#68978,#68979,#68980,#68981,#68982,#68983,#68984,#68985,#68986,
#68987,#68988,#68989,#68990,#68991,#68992,#68993,#68994,#68995),
 .UNSPECIFIED.,.F.,.F.,(4,2,2,2,2,2,2,2,2,2,2,2,2,2,2,2,2,4),(9.61793661197057,
9.65826687772365,9.7042968895204,9.74877836334091,9.79537165987244,9.84090708175655,
9.88582218728856,9.93259567600637,9.977601690456,10.0238180366761,10.069979226294,
10.1144983932143,10.16110353831,10.2067785285603,10.2515491641532,10.2984763703993,
10.3436239436092,10.3558181865992),.UNSPECIFIED.);
#3315=B_SPLINE_CURVE_WITH_KNOTS('',3,(#68996,#68997,#68998,#68999,#69000,
#69001,#69002,#69003,#69004,#69005,#69006,#69007,#69008,#69009,#69010,#69011,
#69012,#69013,#69014,#69015,#69016,#69017,#69018,#69019,#69020,#69021,#69022,
#69023,#69024,#69025,#69026,#69027,#69028,#69029,#69030,#69031),
 .UNSPECIFIED.,.F.,.F.,(4,2,2,2,2,2,2,2,2,2,2,2,2,2,2,2,2,4),(11.0945157948807,
11.1213867439599,11.1679850373331,11.2128305602366,11.2596899606121,11.3056487710637,
11.3501304745185,11.3967192249533,11.4421794429662,11.4871976330225,11.5338877402705,
11.5788167463733,11.625243644501,11.6713128867326,11.7157888464474,11.762370315748,
11.8079485003112,11.8321815583089),.UNSPECIFIED.);
#3316=B_SPLINE_CURVE_WITH_KNOTS('',3,(#69036,#69037,#69038,#69039,#69040,
#69041,#69042,#69043,#69044,#69045,#69046,#69047,#69048,#69049,#69050,#69051,
#69052,#69053,#69054,#69055,#69056,#69057,#69058,#69059,#69060,#69061,#69062,
#69063,#69064,#69065,#69066,#69067,#69068,#69069,#69070,#69071),
 .UNSPECIFIED.,.F.,.F.,(4,2,2,2,2,2,2,2,2,2,2,2,2,2,2,2,2,4),(8.87958134142251,
8.92602852493827,8.97190922433066,9.01652860386053,9.06319528416507,9.10856829537987,
9.15396816557657,9.20055253818396,9.24538645055861,9.29245567423173,9.33839133720815,
9.38290947328484,9.42952391843202,9.47495799799238,9.5200883438932,9.56674687955462,
9.61164771149445,9.61793661197057),.UNSPECIFIED.);
#3317=B_SPLINE_CURVE_WITH_KNOTS('',3,(#69072,#69073,#69074,#69075,#69076,
#69077,#69078,#69079,#69080,#69081,#69082,#69083,#69084,#69085,#69086,#69087,
#69088,#69089,#69090,#69091,#69092,#69093,#69094,#69095,#69096,#69097,#69098,
#69099,#69100,#69101,#69102,#69103,#69104,#69105,#69106,#69107),
 .UNSPECIFIED.,.F.,.F.,(4,2,2,2,2,2,2,2,2,2,2,2,2,2,2,2,2,4),(11.8321815583089,
11.8527802771891,11.8996021709384,11.9446521477749,11.9907033338989,12.0369186161519,
12.0814657635389,12.128073917606,12.1738072502682,12.2185277580605,12.2655192373249,
12.31072570002,12.3564778471481,12.402872126055,12.4475687973262,12.4942402359512,
12.5401634915089,12.5705412125212),.UNSPECIFIED.);
#3318=B_SPLINE_CURVE_WITH_KNOTS('',3,(#69112,#69113,#69114,#69115,#69116,
#69117,#69118,#69119,#69120,#69121,#69122,#69123,#69124,#69125,#69126,#69127,
#69128,#69129,#69130,#69131,#69132,#69133,#69134,#69135,#69136,#69137,#69138,
#69139,#69140,#69141,#69142,#69143,#69144,#69145,#69146,#69147,#69148,#69149),
 .UNSPECIFIED.,.F.,.F.,(4,2,2,2,2,2,2,2,2,2,2,2,2,2,2,2,2,2,4),(8.13994719462425,
8.14633162583834,8.19131496287961,8.23805938644507,8.28326280564246,8.33020598891935,
8.37537161189387,8.42146167824292,8.46779890405304,8.51245656476452,8.55916790929672,
8.60502388390122,8.64982521927269,8.69694438194964,8.74227250884644,8.78807715018487,
8.83459899302762,8.87937738551268,8.87958134142251),.UNSPECIFIED.);
#3319=B_SPLINE_CURVE_WITH_KNOTS('',3,(#69150,#69151,#69152,#69153,#69154,
#69155,#69156,#69157,#69158,#69159,#69160,#69161,#69162,#69163,#69164,#69165,
#69166,#69167,#69168,#69169,#69170,#69171,#69172,#69173,#69174,#69175,#69176,
#69177,#69178,#69179,#69180,#69181,#69182,#69183,#69184,#69185),
 .UNSPECIFIED.,.F.,.F.,(4,2,2,2,2,2,2,2,2,2,2,2,2,2,2,2,2,4),(12.5705412125212,
12.5848546387325,12.6320513443688,12.6774479803703,12.7229914316032,12.7695957899609,
12.81445031732,12.8611058734703,12.9070763099523,12.9516507002645,12.99831783761,
13.0437851987491,13.0889992850039,13.1356902613794,13.1806230657103,13.2273560141773,
13.2734149435215,13.3095464702606),.UNSPECIFIED.);
#3320=B_SPLINE_CURVE_WITH_KNOTS('',3,(#69190,#69191,#69192,#69193,#69194,
#69195,#69196,#69197,#69198,#69199,#69200,#69201,#69202,#69203,#69204,#69205,
#69206,#69207,#69208,#69209,#69210,#69211,#69212,#69213,#69214,#69215,#69216,
#69217,#69218,#69219,#69220,#69221,#69222,#69223,#69224,#69225),
 .UNSPECIFIED.,.F.,.F.,(4,2,2,2,2,2,2,2,2,2,2,2,2,2,2,2,2,4),(7.4007431312885,
7.41304791111891,7.45828058714382,7.50529645897655,7.55014367879521,7.59590467524459,
7.64259365893083,7.68719438742294,7.73344217397141,7.7797297785534,7.82481959427612,
7.87168035811193,7.91667006085986,7.96229014243438,8.00896624204524,8.05352690573283,
8.09964223082121,8.13994719462425),.UNSPECIFIED.);
#3321=B_SPLINE_CURVE_WITH_KNOTS('',3,(#69226,#69227,#69228,#69229,#69230,
#69231,#69232,#69233,#69234,#69235,#69236,#69237,#69238,#69239,#69240,#69241,
#69242,#69243,#69244,#69245,#69246,#69247,#69248,#69249,#69250,#69251,#69252,
#69253,#69254,#69255,#69256,#69257,#69258,#69259,#69260,#69261),
 .UNSPECIFIED.,.F.,.F.,(4,2,2,2,2,2,2,2,2,2,2,2,2,2,2,2,2,4),(13.3095464702606,
13.317941883373,13.3645829231975,13.4101456055024,13.4551345150724,13.5019343622502,
13.5469666430868,13.5932875733925,13.6394722936394,13.6840250104865,13.7306726547352,
13.7763692825722,13.8212020232032,13.8681498846145,13.9133183636254,13.9592929961519,
14.0056379933677,14.0482100370503),.UNSPECIFIED.);
#3322=B_SPLINE_CURVE_WITH_KNOTS('',3,(#69266,#69267,#69268,#69269,#69270,
#69271,#69272,#69273,#69274,#69275,#69276,#69277,#69278,#69279,#69280,#69281,
#69282,#69283,#69284,#69285,#69286,#69287,#69288,#69289,#69290,#69291,#69292,
#69293,#69294,#69295,#69296,#69297,#69298,#69299,#69300,#69301),
 .UNSPECIFIED.,.F.,.F.,(4,2,2,2,2,2,2,2,2,2,2,2,2,2,2,2,2,4),(6.66068790957161,
6.67919937362265,6.72466854010414,6.77138281612983,6.81602051294445,6.86199546399339,
6.90869606549543,6.95356006030469,7.00017259284827,7.04588152831696,7.09129151384102,
7.13849904542972,7.18328368151711,7.22922137769738,7.27595882194379,7.32067836740631,
7.36709263287862,7.4007431312885),.UNSPECIFIED.);
#3323=B_SPLINE_CURVE_WITH_KNOTS('',3,(#69302,#69303,#69304,#69305,#69306,
#69307,#69308,#69309,#69310,#69311,#69312,#69313,#69314,#69315,#69316,#69317,
#69318,#69319,#69320,#69321,#69322,#69323,#69324,#69325,#69326,#69327,#69328,
#69329,#69330,#69331,#69332,#69333,#69334,#69335,#69336,#69337,#69338,#69339),
 .UNSPECIFIED.,.F.,.F.,(4,2,2,2,2,2,2,2,2,2,2,2,2,2,2,2,2,2,4),(14.0482100370503,
14.0502949275604,14.0969842350884,14.1428510125903,14.1876060377872,14.2347388362546,
14.2800782737978,14.3257900005883,14.3723273813755,14.4171197652046,14.4637624404534,
14.5096613605359,14.5542550454664,14.6009122383646,14.6463049723626,14.6916352811859,
14.7382430367566,14.7830983504416,14.7873695654535),.UNSPECIFIED.);
#3324=B_SPLINE_CURVE_WITH_KNOTS('',3,(#69344,#69345,#69346,#69347,#69348,
#69349,#69350,#69351,#69352,#69353,#69354,#69355,#69356,#69357,#69358,#69359,
#69360,#69361,#69362,#69363,#69364,#69365,#69366,#69367,#69368,#69369,#69370,
#69371,#69372,#69373,#69374,#69375,#69376,#69377,#69378,#69379),
 .UNSPECIFIED.,.F.,.F.,(4,2,2,2,2,2,2,2,2,2,2,2,2,2,2,2,2,4),(5.92163532773223,
5.94600636983764,5.99167472451486,6.03834442568581,6.08290534085326,6.12906543139539,
6.17556776526837,6.22058468317993,6.26736631589905,6.31246290231792,6.35801191654115,
6.40468792713218,6.44925237221679,6.49530071297518,6.5422349864363,6.58716711205166,
6.6338555299793,6.66068790957161),.UNSPECIFIED.);
#3325=B_SPLINE_CURVE_WITH_KNOTS('',3,(#69380,#69381,#69382,#69383,#69384,
#69385,#69386,#69387,#69388,#69389,#69390,#69391,#69392,#69393,#69394,#69395,
#69396,#69397,#69398,#69399,#69400,#69401,#69402,#69403,#69404,#69405,#69406,
#69407,#69408,#69409,#69410,#69411,#69412,#69413,#69414,#69415),
 .UNSPECIFIED.,.F.,.F.,(4,2,2,2,2,2,2,2,2,2,2,2,2,2,2,2,2,4),(14.7873695654535,
14.8300506895943,14.8760153851188,14.9205240050731,14.9671371569893,15.0126019611003,
15.057675583655,15.1043686581955,15.1493013607845,15.1958140405279,15.2418832890724,
15.2863744865348,15.3329751597116,15.3785518416522,15.4234279663063,15.4702466636066,
15.5152945541928,15.52530082637),.UNSPECIFIED.);
#3326=B_SPLINE_CURVE_WITH_KNOTS('',3,(#69420,#69421,#69422,#69423,#69424,
#69425,#69426,#69427,#69428,#69429,#69430,#69431,#69432,#69433,#69434,#69435,
#69436,#69437,#69438,#69439,#69440,#69441,#69442,#69443,#69444,#69445,#69446,
#69447,#69448,#69449,#69450,#69451,#69452,#69453,#69454,#69455),
 .UNSPECIFIED.,.F.,.F.,(4,2,2,2,2,2,2,2,2,2,2,2,2,2,2,2,2,4),(5.18185396668694,
5.21237880416024,5.25839496787151,5.30515700786141,5.34994371652288,5.39643143795004,
5.44226233153737,5.48755936034949,5.53464520069729,5.57944804001234,5.62527291324563,
5.6719704074037,5.71660500876536,5.76291244016987,5.80904038749152,5.85417959917163,
5.90109443402236,5.92163532773223),.UNSPECIFIED.);
#3327=B_SPLINE_CURVE_WITH_KNOTS('',3,(#69456,#69457,#69458,#69459,#69460,
#69461,#69462,#69463,#69464,#69465,#69466,#69467,#69468,#69469,#69470,#69471,
#69472,#69473,#69474,#69475,#69476,#69477,#69478,#69479,#69480,#69481,#69482,
#69483,#69484,#69485,#69486,#69487,#69488,#69489,#69490,#69491),
 .UNSPECIFIED.,.F.,.F.,(4,2,2,2,2,2,2,2,2,2,2,2,2,2,2,2,2,4),(15.52530082637,
15.5614208749801,15.6076307500252,15.6521806551763,15.6988024547926,15.7445286011097,
15.7892808923799,15.8362633836619,15.8814623071114,15.927276150182,15.9736600042795,
16.0183472193562,16.0650263185026,16.1109370875013,16.1556467587023,16.2028290294383,
16.2482129573077,16.2641372518591),.UNSPECIFIED.);
#3328=B_SPLINE_CURVE_WITH_KNOTS('',3,(#69496,#69497,#69498,#69499,#69500,
#69501,#69502,#69503,#69504,#69505,#69506,#69507,#69508,#69509,#69510,#69511,
#69512,#69513,#69514,#69515,#69516,#69517,#69518,#69519,#69520,#69521,#69522,
#69523,#69524,#69525,#69526,#69527,#69528,#69529,#69530,#69531),
 .UNSPECIFIED.,.F.,.F.,(4,2,2,2,2,2,2,2,2,2,2,2,2,2,2,2,2,4),(4.44139309291887,
4.4776836945143,4.52383758263681,4.5706515514869,4.61567630656631,4.66246297173395,
4.70776020717613,4.75332044171567,4.80007956104877,4.84474067314722,4.89080480911077,
4.93755248920882,4.9824980884388,5.02919719848812,5.0748218411417,5.12031038828011,
5.16760288091741,5.18185396668694),.UNSPECIFIED.);
#3329=B_SPLINE_CURVE_WITH_KNOTS('',3,(#69532,#69533,#69534,#69535,#69536,
#69537,#69538,#69539,#69540,#69541,#69542,#69543,#69544,#69545,#69546,#69547,
#69548,#69549,#69550,#69551,#69552,#69553,#69554,#69555,#69556,#69557,#69558,
#69559,#69560,#69561,#69562,#69563,#69564,#69565,#69566,#69567),
 .UNSPECIFIED.,.F.,.F.,(4,2,2,2,2,2,2,2,2,2,2,2,2,2,2,2,2,4),(16.2641372518591,
16.2938030479407,16.3403922169256,16.3852327690144,16.4318876967614,16.4778418269624,
16.5224230051924,16.5690903719281,16.6145405471659,16.6597873193538,16.7064589360066,
16.7513738230071,16.7981669588227,16.8442036990566,16.8887271777361,16.9353636792139,
16.9809031362162,17.002935013404),.UNSPECIFIED.);
#3330=B_SPLINE_CURVE_WITH_KNOTS('',3,(#69572,#69573,#69574,#69575,#69576,
#69577,#69578,#69579,#69580,#69581,#69582,#69583,#69584,#69585,#69586,#69587,
#69588,#69589,#69590,#69591,#69592,#69593,#69594,#69595,#69596,#69597,#69598,
#69599,#69600,#69601,#69602,#69603,#69604,#69605,#69606,#69607),
 .UNSPECIFIED.,.F.,.F.,(4,2,2,2,2,2,2,2,2,2,2,2,2,2,2,2,2,4),(3.70124435544509,
3.74399270334172,3.79043516360456,3.83649298269546,3.88175593951858,3.92880219405563,
3.97372112979052,4.0195132499672,4.06625467488101,4.11089815679736,4.15717909180209,
4.20358177441128,4.24870726081431,4.29560414051408,4.34067747993884,4.38633433879972,
4.43306819807542,4.44139309291887),.UNSPECIFIED.);
#3331=B_SPLINE_CURVE_WITH_KNOTS('',3,(#69608,#69609,#69610,#69611,#69612,
#69613,#69614,#69615,#69616,#69617,#69618,#69619,#69620,#69621,#69622,#69623,
#69624,#69625,#69626,#69627,#69628,#69629,#69630,#69631,#69632,#69633,#69634,
#69635,#69636,#69637,#69638,#69639,#69640,#69641,#69642,#69643),
 .UNSPECIFIED.,.F.,.F.,(4,2,2,2,2,2,2,2,2,2,2,2,2,2,2,2,2,4),(17.002935013404,
17.025915911193,17.072690284077,17.1176989140485,17.1640720123954,17.2102290691703,
17.2547667681474,17.3014047938411,17.3470724921718,17.3919178234011,17.4388344169549,
17.4839738058451,17.5299894417733,17.576301715541,17.6209316867396,17.6676059002416,
17.7134384093576,17.7416164595014),.UNSPECIFIED.);
#3332=B_SPLINE_CURVE_WITH_KNOTS('',3,(#69648,#69649,#69650,#69651,#69652,
#69653,#69654,#69655,#69656,#69657,#69658,#69659,#69660,#69661,#69662,#69663,
#69664,#69665,#69666,#69667,#69668,#69669,#69670,#69671,#69672,#69673,#69674,
#69675,#69676,#69677,#69678,#69679,#69680,#69681,#69682,#69683,#69684,#69685),
 .UNSPECIFIED.,.F.,.F.,(4,2,2,2,2,2,2,2,2,2,2,2,2,2,2,2,2,2,4),(2.96056667091537,
2.96492507829847,3.00987622737974,3.05658369104791,3.10200096701632,3.14749048096761,
3.19424386881459,3.23892780451988,3.28492439294727,3.33166335850067,3.37655065295563,
3.42318675502558,3.46898366955253,3.51441887445073,3.56165143914983,3.60649480353247,
3.65245839303867,3.69924258599329,3.70124435544509),.UNSPECIFIED.);
#3333=B_SPLINE_CURVE_WITH_KNOTS('',3,(#69686,#69687,#69688,#69689,#69690,
#69691,#69692,#69693,#69694,#69695,#69696,#69697,#69698,#69699,#69700,#69701,
#69702,#69703,#69704,#69705,#69706,#69707,#69708,#69709,#69710,#69711,#69712,
#69713,#69714,#69715,#69716,#69717,#69718,#69719,#69720,#69721),
 .UNSPECIFIED.,.F.,.F.,(4,2,2,2,2,2,2,2,2,2,2,2,2,2,2,2,2,4),(17.7416164595014,
17.7581937074056,17.8052897716113,17.8505949597077,17.8963342553297,17.9428341521077,
17.9875910389412,18.0342105229933,18.0800707772756,18.1246525565008,18.1712871874809,
18.216640662327,18.2619848096412,18.3085503980356,18.3533657933236,18.400359214998,
18.4462787969036,18.4801374068086),.UNSPECIFIED.);
#3334=B_SPLINE_CURVE_WITH_KNOTS('',3,(#69726,#69727,#69728,#69729,#69730,
#69731,#69732,#69733,#69734,#69735,#69736,#69737,#69738,#69739,#69740,#69741,
#69742,#69743,#69744,#69745,#69746,#69747,#69748,#69749,#69750,#69751,#69752,
#69753,#69754,#69755,#69756,#69757,#69758,#69759,#69760,#69761),
 .UNSPECIFIED.,.F.,.F.,(4,2,2,2,2,2,2,2,2,2,2,2,2,2,2,2,2,4),(2.22108960842022,
2.23120408651738,2.27635041765121,2.32327161202571,2.36823721236016,2.41391337632635,
2.46061197044848,2.50519713944098,2.5513666691269,2.59796482409036,2.64299465164124,
2.68978881468655,2.73495033646277,2.78051325751773,2.82722340795193,2.87182391070409,
2.91788757577027,2.96056667091537),.UNSPECIFIED.);
#3335=B_SPLINE_CURVE_WITH_KNOTS('',3,(#69762,#69763,#69764,#69765,#69766,
#69767,#69768,#69769,#69770,#69771,#69772,#69773,#69774,#69775,#69776,#69777,
#69778,#69779,#69780,#69781,#69782,#69783,#69784,#69785,#69786,#69787,#69788,
#69789,#69790,#69791,#69792,#69793,#69794,#69795,#69796,#69797),
 .UNSPECIFIED.,.F.,.F.,(4,2,2,2,2,2,2,2,2,2,2,2,2,2,2,2,2,4),(18.4801374068086,
18.4907658387484,18.5373515732759,18.5827705496792,18.6278503876037,18.6744946287827,
18.7193811593225,18.7659288080364,18.8119468422919,18.8564049604675,18.9029730562544,
18.9484976039111,18.9933693909541,19.040132859827,19.0851285827534,19.1312801378602,
19.1774331259836,19.2175408345414),.UNSPECIFIED.);
#3336=B_SPLINE_CURVE_WITH_KNOTS('',3,(#69802,#69803,#69804,#69805,#69806,
#69807,#69808,#69809,#69810,#69811,#69812,#69813,#69814,#69815,#69816,#69817,
#69818,#69819,#69820,#69821,#69822,#69823,#69824,#69825,#69826,#69827,#69828,
#69829,#69830,#69831,#69832,#69833,#69834,#69835,#69836,#69837),
 .UNSPECIFIED.,.F.,.F.,(4,2,2,2,2,2,2,2,2,2,2,2,2,2,2,2,2,4),(1.48067239643092,
1.4967132601331,1.54219831559389,1.58948594493822,1.63428944893559,1.68030245144475,
1.72708174969294,1.77186789841824,1.81835464146151,1.86425678939566,1.90955548629973,
1.95664189807863,2.00148568451759,2.04731268579268,2.09403346709215,2.13867975716629,
2.18499121798638,2.22108960842022),.UNSPECIFIED.);
#3337=B_SPLINE_CURVE_WITH_KNOTS('',3,(#69838,#69839,#69840,#69841,#69842,
#69843,#69844,#69845,#69846,#69847,#69848,#69849,#69850,#69851,#69852,#69853,
#69854,#69855,#69856,#69857,#69858,#69859,#69860,#69861,#69862,#69863,#69864,
#69865,#69866,#69867,#69868,#69869,#69870,#69871,#69872,#69873,#69874,#69875),
 .UNSPECIFIED.,.F.,.F.,(4,2,2,2,2,2,2,2,2,2,2,2,2,2,2,2,2,2,4),(19.2175408345414,
19.221937402198,19.2685210781433,19.3141891434761,19.3589248273872,19.4058460255822,
19.4509870795851,19.4968133821774,19.5431350562803,19.5877640969252,19.634399062382,
19.6802461572256,19.724925976838,19.7720412018952,19.81736181445,19.862949655886,
19.9094715921544,19.954248074309,19.955968047547),.UNSPECIFIED.);
#3338=B_SPLINE_CURVE_WITH_KNOTS('',3,(#69880,#69881,#69882,#69883,#69884,
#69885,#69886,#69887,#69888,#69889,#69890,#69891,#69892,#69893,#69894,#69895,
#69896,#69897,#69898,#69899,#69900,#69901,#69902,#69903,#69904,#69905,#69906,
#69907,#69908,#69909,#69910,#69911,#69912,#69913,#69914,#69915),
 .UNSPECIFIED.,.F.,.F.,(4,2,2,2,2,2,2,2,2,2,2,2,2,2,2,2,2,4),(0.740262878330326,
0.76242710224918,0.808069985435835,0.854808846306471,0.899429812602798,
0.94557087207502,0.992454683252572,1.03747065149212,1.08424743872217,1.12958660658263,
1.17513888970271,1.22190780151563,1.26658471045133,1.31264188423565,1.35939848502835,
1.40433922056887,1.45103260194552,1.48067239643092),.UNSPECIFIED.);
#3339=B_SPLINE_CURVE_WITH_KNOTS('',3,(#69916,#69917,#69918,#69919,#69920,
#69921,#69922,#69923,#69924,#69925,#69926,#69927,#69928,#69929,#69930,#69931,
#69932,#69933,#69934,#69935,#69936,#69937,#69938,#69939,#69940,#69941,#69942,
#69943,#69944,#69945,#69946,#69947,#69948,#69949,#69950,#69951),
 .UNSPECIFIED.,.F.,.F.,(4,2,2,2,2,2,2,2,2,2,2,2,2,2,2,2,2,4),(19.955968047547,
20.000850484569,20.0467368471769,20.0912761893499,20.1378918513278,20.1832739357276,
20.2285046069091,20.2751045193351,20.3199511150685,20.3667546312751,20.4127173706803,
20.4571887517883,20.5037686958299,20.5492336722642,20.5942218827244,20.6409180673264,
20.685852328368,20.6936878782319),.UNSPECIFIED.);
#3340=B_SPLINE_CURVE_WITH_KNOTS('',3,(#69956,#69957,#69958,#69959,#69960,
#69961,#69962,#69963,#69964,#69965,#69966,#69967,#69968,#69969,#69970,#69971,
#69972,#69973,#69974,#69975,#69976,#69977,#69978,#69979,#69980,#69981,#69982,
#69983,#69984,#69985,#69986,#69987,#69988,#69989,#69990,#69991),
 .UNSPECIFIED.,.F.,.F.,(4,2,2,2,2,2,2,2,2,2,2,2,2,2,2,2,2,4),(1.00000014275486E-6,
0.0364903991724837,0.0742057368406976,0.120984278386942,0.16571626048475,
0.212135354717781,0.258243398985401,0.303486376623694,0.350510827495094,
0.395451299112592,0.441223703714196,0.487964967575798,0.532602258878132,
0.578864855190162,0.62532910035835,0.67044002179057,0.717320863587734,0.740262878330326),
 .UNSPECIFIED.);
#3341=B_SPLINE_CURVE_WITH_KNOTS('',3,(#69992,#69993,#69994,#69995,#69996,
#69997,#69998,#69999,#70000,#70001,#70002,#70003,#70004,#70005,#70006,#70007,
#70008,#70009,#70010,#70011,#70012,#70013,#70014,#70015,#70016,#70017,#70018,
#70019,#70020,#70021,#70022,#70023,#70024,#70025,#70026,#70027),
 .UNSPECIFIED.,.F.,.F.,(4,2,2,2,2,2,2,2,2,2,2,2,2,2,2,2,2,4),(20.6936878782319,
20.732228532913,20.778305724133,20.8227795112891,20.8693557797099,20.9149428959302,
20.9597524918607,21.0065846919771,21.0516438918501,21.0976519462771,21.1438788857884,
21.188432480541,21.2350393010027,21.2807854645354,21.325492530929,21.3724982961973,
21.417717731441,21.4315064083924),.UNSPECIFIED.);
#3342=B_SPLINE_CURVE_WITH_KNOTS('',3,(#70030,#70031,#70032,#70033,#70034,
#70035,#70036,#70037),.UNSPECIFIED.,.F.,.F.,(4,2,2,4),(21.4315064083924,
21.4634358005757,21.493031868375,21.522626598838),.UNSPECIFIED.);
#3343=B_SPLINE_CURVE_WITH_KNOTS('',3,(#70042,#70043,#70044,#70045,#70046,
#70047,#70048,#70049,#70050,#70051,#70052,#70053),.UNSPECIFIED.,.F.,.F.,
(4,2,2,2,2,4),(-0.220493779628296,-0.188155373461082,-0.153829429857051,
-0.103952453260852,-0.0536656706932583,-1.00000014990886E-6),
 .UNSPECIFIED.);
#3344=B_SPLINE_CURVE_WITH_KNOTS('',3,(#70056,#70057,#70058,#70059,#70060,
#70061,#70062,#70063,#70064,#70065,#70066,#70067,#70068,#70069,#70070,#70071,
#70072,#70073,#70074,#70075,#70076,#70077),.UNSPECIFIED.,.F.,.F.,(4,2,2,
2,2,2,2,2,2,2,4),(0.203440126186273,0.213167596868103,0.241856386112924,
0.272211919544501,0.305118112000406,0.341399456620154,0.378879659132554,
0.40534149334872,0.429291364608543,0.44378295238274,0.459192789470913),
 .UNSPECIFIED.);
#3345=B_SPLINE_CURVE_WITH_KNOTS('',3,(#70079,#70080,#70081,#70082,#70083,
#70084,#70085,#70086,#70087,#70088,#70089,#70090,#70091,#70092,#70093,#70094,
#70095,#70096,#70097,#70098,#70099,#70100,#70101,#70102,#70103,#70104,#70105,
#70106,#70107,#70108,#70109,#70110,#70111,#70112),.UNSPECIFIED.,.F.,.F.,
(4,2,2,2,2,2,2,2,2,2,2,2,2,2,2,2,4),(-0.921606618540025,-0.872688627355351,
-0.813612023857313,-0.756611351546357,-0.69692945872276,-0.638499761548747,
-0.581118209737007,-0.521076231967445,-0.463317306881228,-0.4044438926574,
-0.345164740388026,-0.288053249414949,-0.228344796882901,-0.169710130792356,
-0.112479424024743,-0.0563089256119929,-9.99999990258793E-7),
 .UNSPECIFIED.);
#3346=B_SPLINE_CURVE_WITH_KNOTS('',3,(#70113,#70114,#70115,#70116,#70117,
#70118,#70119,#70120,#70121,#70122,#70123,#70124,#70125,#70126,#70127,#70128,
#70129,#70130,#70131,#70132,#70133,#70134,#70135,#70136,#70137,#70138,#70139,
#70140,#70141,#70142,#70143,#70144),.UNSPECIFIED.,.F.,.F.,(4,2,2,2,2,2,
2,2,2,2,2,2,2,2,2,4),(-27.2675995337344,-27.2205810783644,-27.1716030839864,
-27.1114524980469,-27.0544959346273,-26.9959799991961,-26.9364896777515,
-26.8795127522937,-26.8203565510693,-26.7619639947482,-26.7043369916545,
-26.6444247756288,-26.5873734790364,-26.5290771329393,-26.4696302887724,
-26.4647006629411),.UNSPECIFIED.);
#3347=B_SPLINE_CURVE_WITH_KNOTS('',3,(#70321,#70322,#70323,#70324,#70325,
#70326,#70327,#70328),.UNSPECIFIED.,.F.,.F.,(4,2,2,4),(-0.00426615559741139,
-0.00353262795509977,-0.00302253710286643,-0.00251244625063308),
 .UNSPECIFIED.);
#3348=B_SPLINE_CURVE_WITH_KNOTS('',3,(#71242,#71243,#71244,#71245,#71246,
#71247,#71248,#71249),.UNSPECIFIED.,.F.,.F.,(4,2,2,4),(-0.00251244625063308,
-0.00200235539839974,-0.0014922645461664,-0.000758736903856822),
 .UNSPECIFIED.);
#3349=B_SPLINE_CURVE_WITH_KNOTS('',3,(#71254,#71255,#71256,#71257,#71258,
#71259,#71260,#71261),.UNSPECIFIED.,.F.,.F.,(4,2,2,4),(-0.00932716297425779,
-0.00859363533194745,-0.0080835444797141,-0.00757345362748076),
 .UNSPECIFIED.);
#3350=B_SPLINE_CURVE_WITH_KNOTS('',3,(#72175,#72176,#72177,#72178,#72179,
#72180,#72181,#72182),.UNSPECIFIED.,.F.,.F.,(4,2,2,4),(-0.00757345362748076,
-0.00706336277524741,-0.00655327192301407,-0.00581974428070595),
 .UNSPECIFIED.);
#3351=B_SPLINE_CURVE_WITH_KNOTS('',3,(#74178,#74179,#74180,#74181,#74182,
#74183,#74184,#74185,#74186,#74187,#74188,#74189,#74190,#74191,#74192,#74193,
#74194,#74195,#74196,#74197,#74198,#74199,#74200,#74201,#74202,#74203,#74204,
#74205),.UNSPECIFIED.,.F.,.F.,(4,2,2,2,2,2,2,2,2,2,2,2,2,4),(1.00000052656661E-6,
0.0405527857266322,0.0799421814660319,0.1262631587317,0.186952165234641,
0.270820823781497,0.348937293245129,0.459507052180891,0.623823282878412,
0.790896670749941,0.927459468885873,1.05843758188768,1.16179395572833,1.24835467272154),
 .UNSPECIFIED.);
#3352=SPHERICAL_SURFACE('',#32135,6.);
#3353=SPHERICAL_SURFACE('',#32138,6.);
#3354=SPHERICAL_SURFACE('',#32141,6.);
#3355=SHAPE_REPRESENTATION_RELATIONSHIP('SRR','None',#75368,#3363);
#3356=SHAPE_REPRESENTATION_RELATIONSHIP('SRR','None',#75369,#3364);
#3357=SHAPE_REPRESENTATION_RELATIONSHIP('SRR','None',#75370,#3365);
#3358=SHAPE_REPRESENTATION_RELATIONSHIP('SRR','None',#75371,#3366);
#3359=SHAPE_REPRESENTATION_RELATIONSHIP('SRR','None',#75372,#3367);
#3360=SHAPE_REPRESENTATION_RELATIONSHIP('SRR','None',#75373,#3368);
#3361=SHAPE_REPRESENTATION_RELATIONSHIP('SRR','None',#75374,#3369);
#3362=SHAPE_REPRESENTATION_RELATIONSHIP('SRR','None',#75375,#3370);
#3363=ADVANCED_BREP_SHAPE_REPRESENTATION('',(#3379),#75328);
#3364=ADVANCED_BREP_SHAPE_REPRESENTATION('',(#3380),#75329);
#3365=ADVANCED_BREP_SHAPE_REPRESENTATION('',(#3381),#75330);
#3366=ADVANCED_BREP_SHAPE_REPRESENTATION('',(#3382),#75331);
#3367=ADVANCED_BREP_SHAPE_REPRESENTATION('',(#3383),#75332);
#3368=ADVANCED_BREP_SHAPE_REPRESENTATION('',(#3384),#75333);
#3369=ADVANCED_BREP_SHAPE_REPRESENTATION('',(#3385),#75334);
#3370=ADVANCED_BREP_SHAPE_REPRESENTATION('',(#3386),#75335);
#3371=STYLED_ITEM('',(#75417),#3379);
#3372=STYLED_ITEM('',(#75418),#3380);
#3373=STYLED_ITEM('',(#75418),#3381);
#3374=STYLED_ITEM('',(#75418),#3382);
#3375=STYLED_ITEM('',(#75417),#3383);
#3376=STYLED_ITEM('',(#75419),#3384);
#3377=STYLED_ITEM('',(#75419),#3385);
#3378=STYLED_ITEM('',(#75419),#3386);
#3379=MANIFOLD_SOLID_BREP('Body1',#32021);
#3380=MANIFOLD_SOLID_BREP('Body1',#32022);
#3381=MANIFOLD_SOLID_BREP('Body1',#32023);
#3382=MANIFOLD_SOLID_BREP('Body1',#32024);
#3383=MANIFOLD_SOLID_BREP('Body1',#32025);
#3384=MANIFOLD_SOLID_BREP('Body1',#32026);
#3385=MANIFOLD_SOLID_BREP('Body1',#32027);
#3386=MANIFOLD_SOLID_BREP('Body1',#32028);
#3387=FACE_BOUND('',#6872,.T.);
#3388=FACE_BOUND('',#6889,.T.);
#3389=FACE_BOUND('',#6890,.T.);
#3390=FACE_BOUND('',#6891,.T.);
#3391=FACE_BOUND('',#6903,.T.);
#3392=FACE_BOUND('',#6904,.T.);
#3393=FACE_BOUND('',#6905,.T.);
#3394=FACE_BOUND('',#7230,.T.);
#3395=FACE_BOUND('',#7235,.T.);
#3396=FACE_BOUND('',#7795,.T.);
#3397=FACE_BOUND('',#7800,.T.);
#3398=FACE_BOUND('',#8360,.T.);
#3399=FACE_BOUND('',#8365,.T.);
#3400=CIRCLE('',#32130,40.);
#3401=CIRCLE('',#32131,40.);
#3402=CIRCLE('',#32136,6.);
#3403=CIRCLE('',#32139,6.);
#3404=CIRCLE('',#32142,6.);
#3405=CIRCLE('',#32145,1.5);
#3406=CIRCLE('',#32146,1.5);
#3407=CIRCLE('',#32148,1.5);
#3408=CIRCLE('',#32149,1.5);
#3409=CIRCLE('',#32151,1.5);
#3410=CIRCLE('',#32152,1.5);
#3411=CIRCLE('',#32154,5.);
#3412=CIRCLE('',#32155,5.);
#3413=CIRCLE('',#32158,5.);
#3414=CIRCLE('',#32159,5.);
#3415=CIRCLE('',#32162,5.);
#3416=CIRCLE('',#32163,5.);
#3417=CIRCLE('',#32166,5.);
#3418=CIRCLE('',#32167,5.);
#3419=CIRCLE('',#32169,40.);
#3420=CIRCLE('',#32170,40.);
#3421=CIRCLE('',#32172,5.);
#3422=CIRCLE('',#32173,40.);
#3423=CIRCLE('',#32174,5.);
#3424=CIRCLE('',#32175,5.);
#3425=CIRCLE('',#32176,40.);
#3426=CIRCLE('',#32177,5.);
#3427=CIRCLE('',#32178,5.);
#3428=CIRCLE('',#32180,5.);
#3429=CIRCLE('',#32182,40.);
#3430=CIRCLE('',#32184,5.);
#3431=CIRCLE('',#32186,5.);
#3432=CIRCLE('',#32188,5.);
#3433=CIRCLE('',#32190,5.);
#3434=CIRCLE('',#32193,40.);
#3435=CIRCLE('',#32199,1.5);
#3436=CIRCLE('',#32200,1.5);
#3437=CIRCLE('',#32229,1.17524047358084);
#3438=CIRCLE('',#32231,1.17524047358084);
#3439=CIRCLE('',#32262,1.1752404735812);
#3440=CIRCLE('',#32264,1.17524047358084);
#3441=CIRCLE('',#32265,1.5);
#3442=CIRCLE('',#32313,1.55162884844711);
#3443=CIRCLE('',#32315,2.61372936963188);
#3444=CIRCLE('',#32316,0.0468749999999982);
#3445=CIRCLE('',#32317,2.58058373926377);
#3446=CIRCLE('',#32319,2.73627063036812);
#3447=CIRCLE('',#32321,2.73627063036812);
#3448=CIRCLE('',#32323,2.73627063036812);
#3449=CIRCLE('',#32325,2.73627063036812);
#3450=CIRCLE('',#32327,2.73627063036812);
#3451=CIRCLE('',#32329,2.73627063036812);
#3452=CIRCLE('',#32331,2.73627063036812);
#3453=CIRCLE('',#32333,2.73627063036812);
#3454=CIRCLE('',#32335,2.73627063036812);
#3455=CIRCLE('',#32337,2.73627063036812);
#3456=CIRCLE('',#32339,2.73627063036812);
#3457=CIRCLE('',#32341,2.73627063036812);
#3458=CIRCLE('',#32343,2.73627063036812);
#3459=CIRCLE('',#32345,2.73627063036812);
#3460=CIRCLE('',#32347,2.73627063036812);
#3461=CIRCLE('',#32349,2.73627063036812);
#3462=CIRCLE('',#32351,2.73627063036812);
#3463=CIRCLE('',#32353,2.73627063036812);
#3464=CIRCLE('',#32355,2.73627063036812);
#3465=CIRCLE('',#32357,2.73627063036812);
#3466=CIRCLE('',#32359,2.73627063036812);
#3467=CIRCLE('',#32361,2.73627063036812);
#3468=CIRCLE('',#32363,2.73627063036812);
#3469=CIRCLE('',#32365,2.73627063036812);
#3470=CIRCLE('',#32367,2.73627063036812);
#3471=CIRCLE('',#32369,2.73627063036812);
#3472=CIRCLE('',#32371,2.73627063036812);
#3473=CIRCLE('',#32373,2.73627063036812);
#3474=CIRCLE('',#32375,2.73627063036812);
#3475=CIRCLE('',#32377,2.73627063036812);
#3476=CIRCLE('',#32379,2.73627063036812);
#3477=CIRCLE('',#32381,2.73627063036812);
#3478=CIRCLE('',#32383,2.73627063036812);
#3479=CIRCLE('',#32385,2.73627063036812);
#3480=CIRCLE('',#32387,2.73627063036812);
#3481=CIRCLE('',#32389,2.73627063036812);
#3482=CIRCLE('',#32391,2.73627063036812);
#3483=CIRCLE('',#32393,2.73627063036812);
#3484=CIRCLE('',#32395,2.73627063036812);
#3485=CIRCLE('',#32397,2.73627063036812);
#3486=CIRCLE('',#32399,2.73627063036812);
#3487=CIRCLE('',#32401,2.73627063036812);
#3488=CIRCLE('',#32403,2.73627063036812);
#3489=CIRCLE('',#32405,2.73627063036812);
#3490=CIRCLE('',#32407,2.73627063036812);
#3491=CIRCLE('',#32409,2.73627063036812);
#3492=CIRCLE('',#32410,2.73627063036812);
#3493=CIRCLE('',#32411,2.73627063036812);
#3494=CIRCLE('',#32412,2.73627063036812);
#3495=CIRCLE('',#32413,2.73627063036812);
#3496=CIRCLE('',#32414,2.73627063036812);
#3497=CIRCLE('',#32415,2.73627063036812);
#3498=CIRCLE('',#32416,2.73627063036812);
#3499=CIRCLE('',#32417,2.73627063036812);
#3500=CIRCLE('',#32418,2.73627063036812);
#3501=CIRCLE('',#32419,2.73627063036812);
#3502=CIRCLE('',#32420,2.73627063036812);
#3503=CIRCLE('',#32421,2.73627063036812);
#3504=CIRCLE('',#32422,2.73627063036812);
#3505=CIRCLE('',#32423,2.73627063036812);
#3506=CIRCLE('',#32424,2.73627063036812);
#3507=CIRCLE('',#32426,2.73627063036812);
#3508=CIRCLE('',#32428,2.73627063036812);
#3509=CIRCLE('',#32430,2.73627063036812);
#3510=CIRCLE('',#32432,2.73627063036812);
#3511=CIRCLE('',#32434,2.73627063036812);
#3512=CIRCLE('',#32436,2.73627063036812);
#3513=CIRCLE('',#32438,2.73627063036812);
#3514=CIRCLE('',#32440,2.73627063036812);
#3515=CIRCLE('',#32442,2.73627063036812);
#3516=CIRCLE('',#32444,2.73627063036812);
#3517=CIRCLE('',#32446,2.73627063036812);
#3518=CIRCLE('',#32448,2.73627063036812);
#3519=CIRCLE('',#32450,2.73627063036812);
#3520=CIRCLE('',#32452,2.73627063036812);
#3521=CIRCLE('',#32454,2.73627063036812);
#3522=CIRCLE('',#32456,2.73627063036812);
#3523=CIRCLE('',#32458,2.73627063036812);
#3524=CIRCLE('',#32460,2.73627063036812);
#3525=CIRCLE('',#32462,2.73627063036812);
#3526=CIRCLE('',#32464,2.73627063036812);
#3527=CIRCLE('',#32466,2.73627063036812);
#3528=CIRCLE('',#32468,2.73627063036812);
#3529=CIRCLE('',#32470,2.73627063036812);
#3530=CIRCLE('',#32472,2.73627063036812);
#3531=CIRCLE('',#32474,2.73627063036812);
#3532=CIRCLE('',#32476,2.73627063036812);
#3533=CIRCLE('',#32478,2.73627063036812);
#3534=CIRCLE('',#32480,2.73627063036812);
#3535=CIRCLE('',#32482,2.73627063036812);
#3536=CIRCLE('',#32484,2.73627063036812);
#3537=CIRCLE('',#32486,2.73627063036812);
#3538=CIRCLE('',#32488,2.73627063036812);
#3539=CIRCLE('',#32490,2.73627063036812);
#3540=CIRCLE('',#32492,2.73627063036812);
#3541=CIRCLE('',#32494,2.73627063036812);
#3542=CIRCLE('',#32496,2.73627063036812);
#3543=CIRCLE('',#32498,2.73627063036812);
#3544=CIRCLE('',#32500,2.73627063036812);
#3545=CIRCLE('',#32502,2.73627063036812);
#3546=CIRCLE('',#32504,2.73627063036812);
#3547=CIRCLE('',#32506,2.73627063036812);
#3548=CIRCLE('',#32508,2.73627063036812);
#3549=CIRCLE('',#32510,2.73627063036812);
#3550=CIRCLE('',#32512,2.73627063036812);
#3551=CIRCLE('',#32514,2.73627063036812);
#3552=CIRCLE('',#32516,2.73627063036812);
#3553=CIRCLE('',#32518,2.73627063036812);
#3554=CIRCLE('',#32520,2.73627063036812);
#3555=CIRCLE('',#32522,2.73627063036812);
#3556=CIRCLE('',#32524,2.73627063036812);
#3557=CIRCLE('',#32526,2.73627063036812);
#3558=CIRCLE('',#32528,2.73627063036812);
#3559=CIRCLE('',#32530,2.73627063036812);
#3560=CIRCLE('',#32532,2.73627063036812);
#3561=CIRCLE('',#32534,2.73627063036812);
#3562=CIRCLE('',#32536,2.73627063036812);
#3563=CIRCLE('',#32538,2.73627063036812);
#3564=CIRCLE('',#32540,2.73627063036812);
#3565=CIRCLE('',#32542,2.73627063036812);
#3566=CIRCLE('',#32544,2.73627063036812);
#3567=CIRCLE('',#32546,2.73627063036812);
#3568=CIRCLE('',#32548,2.73627063036812);
#3569=CIRCLE('',#32550,2.73627063036812);
#3570=CIRCLE('',#32552,2.73627063036812);
#3571=CIRCLE('',#32554,2.73627063036812);
#3572=CIRCLE('',#32556,2.73627063036812);
#3573=CIRCLE('',#32558,2.73627063036812);
#3574=CIRCLE('',#32560,2.73627063036812);
#3575=CIRCLE('',#32562,2.73627063036812);
#3576=CIRCLE('',#32564,2.73627063036812);
#3577=CIRCLE('',#32566,2.73627063036812);
#3578=CIRCLE('',#32568,2.73627063036812);
#3579=CIRCLE('',#32570,2.73627063036812);
#3580=CIRCLE('',#32572,2.73627063036812);
#3581=CIRCLE('',#32574,2.73627063036812);
#3582=CIRCLE('',#32576,2.73627063036812);
#3583=CIRCLE('',#32578,2.73627063036812);
#3584=CIRCLE('',#32580,2.73627063036812);
#3585=CIRCLE('',#32582,2.73627063036812);
#3586=CIRCLE('',#32583,2.73627063036812);
#3587=CIRCLE('',#32584,2.73627063036812);
#3588=CIRCLE('',#32585,2.73627063036812);
#3589=CIRCLE('',#32586,2.73627063036812);
#3590=CIRCLE('',#32587,2.73627063036812);
#3591=CIRCLE('',#32588,2.73627063036812);
#3592=CIRCLE('',#32589,2.73627063036812);
#3593=CIRCLE('',#32590,2.73627063036812);
#3594=CIRCLE('',#32591,2.73627063036812);
#3595=CIRCLE('',#32592,2.73627063036812);
#3596=CIRCLE('',#32593,2.73627063036812);
#3597=CIRCLE('',#32594,2.73627063036812);
#3598=CIRCLE('',#32595,2.73627063036812);
#3599=CIRCLE('',#32596,2.73627063036812);
#3600=CIRCLE('',#32597,2.73627063036812);
#3601=CIRCLE('',#32599,2.73627063036812);
#3602=CIRCLE('',#32601,2.73627063036812);
#3603=CIRCLE('',#32603,2.73627063036812);
#3604=CIRCLE('',#32605,2.73627063036812);
#3605=CIRCLE('',#32607,2.73627063036812);
#3606=CIRCLE('',#32608,2.68872936963188);
#3607=CIRCLE('',#32609,2.68872936963188);
#3608=CIRCLE('',#32611,2.675);
#3609=CIRCLE('',#32612,0.0468749999999996);
#3610=CIRCLE('',#32614,2.675);
#3611=CIRCLE('',#32616,2.60625);
#3612=CIRCLE('',#32617,0.0687500000000002);
#3613=CIRCLE('',#32619,0.15);
#3614=CIRCLE('',#32620,1.65);
#3615=CIRCLE('',#32623,2.75);
#3616=CIRCLE('',#32628,2.75);
#3617=CIRCLE('',#32632,2.75);
#3618=CIRCLE('',#32636,2.75);
#3619=CIRCLE('',#32640,2.75);
#3620=CIRCLE('',#32644,2.75);
#3621=CIRCLE('',#32648,2.75);
#3622=CIRCLE('',#32652,2.75);
#3623=CIRCLE('',#32656,2.75);
#3624=CIRCLE('',#32660,2.75);
#3625=CIRCLE('',#32664,2.75);
#3626=CIRCLE('',#32668,2.75);
#3627=CIRCLE('',#32672,2.75);
#3628=CIRCLE('',#32676,2.75);
#3629=CIRCLE('',#32680,2.75);
#3630=CIRCLE('',#32684,2.75);
#3631=CIRCLE('',#32688,2.75);
#3632=CIRCLE('',#32692,2.75);
#3633=CIRCLE('',#32696,2.75);
#3634=CIRCLE('',#32700,2.75);
#3635=CIRCLE('',#32704,2.75);
#3636=CIRCLE('',#32708,2.75);
#3637=CIRCLE('',#32712,2.75);
#3638=CIRCLE('',#32716,2.75);
#3639=CIRCLE('',#32720,2.75);
#3640=CIRCLE('',#32724,2.75);
#3641=CIRCLE('',#32728,2.75);
#3642=CIRCLE('',#32732,2.75);
#3643=CIRCLE('',#32736,2.75);
#3644=CIRCLE('',#32740,2.75);
#3645=CIRCLE('',#32744,2.75);
#3646=CIRCLE('',#32748,2.75);
#3647=CIRCLE('',#32752,2.75);
#3648=CIRCLE('',#32756,2.75);
#3649=CIRCLE('',#32760,2.75);
#3650=CIRCLE('',#32764,2.75);
#3651=CIRCLE('',#32768,2.75);
#3652=CIRCLE('',#32772,2.75);
#3653=CIRCLE('',#32776,2.75);
#3654=CIRCLE('',#32780,2.75);
#3655=CIRCLE('',#32784,2.75);
#3656=CIRCLE('',#32788,2.75);
#3657=CIRCLE('',#32792,2.75);
#3658=CIRCLE('',#32796,2.75);
#3659=CIRCLE('',#32800,2.75);
#3660=CIRCLE('',#32804,2.75);
#3661=CIRCLE('',#32808,2.75);
#3662=CIRCLE('',#32812,2.75);
#3663=CIRCLE('',#32816,2.75);
#3664=CIRCLE('',#32820,2.75);
#3665=CIRCLE('',#32824,2.75);
#3666=CIRCLE('',#32828,2.75);
#3667=CIRCLE('',#32832,2.75);
#3668=CIRCLE('',#32836,2.75);
#3669=CIRCLE('',#32840,2.75);
#3670=CIRCLE('',#32844,2.75);
#3671=CIRCLE('',#32848,2.75);
#3672=CIRCLE('',#32852,2.75);
#3673=CIRCLE('',#32856,2.75);
#3674=CIRCLE('',#32860,2.75);
#3675=CIRCLE('',#32864,2.75);
#3676=CIRCLE('',#32868,2.75);
#3677=CIRCLE('',#32872,2.75);
#3678=CIRCLE('',#32876,2.75);
#3679=CIRCLE('',#32879,2.75);
#3680=CIRCLE('',#32883,2.75);
#3681=CIRCLE('',#32887,2.75);
#3682=CIRCLE('',#32891,2.75);
#3683=CIRCLE('',#32895,2.75);
#3684=CIRCLE('',#32899,2.75);
#3685=CIRCLE('',#32903,2.75);
#3686=CIRCLE('',#32907,2.75);
#3687=CIRCLE('',#32911,2.75);
#3688=CIRCLE('',#32915,2.75);
#3689=CIRCLE('',#32919,2.75);
#3690=CIRCLE('',#32923,2.75);
#3691=CIRCLE('',#32927,2.75);
#3692=CIRCLE('',#32931,2.75);
#3693=CIRCLE('',#32936,2.75);
#3694=CIRCLE('',#32938,2.75);
#3695=CIRCLE('',#32940,2.75);
#3696=CIRCLE('',#32942,2.75);
#3697=CIRCLE('',#32944,2.75);
#3698=CIRCLE('',#32946,2.75);
#3699=CIRCLE('',#32948,2.75);
#3700=CIRCLE('',#32950,2.75);
#3701=CIRCLE('',#32952,2.75);
#3702=CIRCLE('',#32954,2.75);
#3703=CIRCLE('',#32956,2.75);
#3704=CIRCLE('',#32958,2.75);
#3705=CIRCLE('',#32960,2.75);
#3706=CIRCLE('',#32962,2.75);
#3707=CIRCLE('',#32964,2.75);
#3708=CIRCLE('',#32966,2.75);
#3709=CIRCLE('',#32968,2.75);
#3710=CIRCLE('',#32970,2.75);
#3711=CIRCLE('',#32972,2.75);
#3712=CIRCLE('',#32974,2.75);
#3713=CIRCLE('',#32976,2.75);
#3714=CIRCLE('',#32978,2.75);
#3715=CIRCLE('',#32980,2.75);
#3716=CIRCLE('',#32982,2.75);
#3717=CIRCLE('',#32984,2.75);
#3718=CIRCLE('',#32986,2.75);
#3719=CIRCLE('',#32988,2.75);
#3720=CIRCLE('',#32990,2.75);
#3721=CIRCLE('',#32992,2.75);
#3722=CIRCLE('',#32994,2.75);
#3723=CIRCLE('',#32996,2.75);
#3724=CIRCLE('',#32998,2.75);
#3725=CIRCLE('',#33000,2.75);
#3726=CIRCLE('',#33002,2.75);
#3727=CIRCLE('',#33004,2.75);
#3728=CIRCLE('',#33006,2.75);
#3729=CIRCLE('',#33008,2.75);
#3730=CIRCLE('',#33010,2.75);
#3731=CIRCLE('',#33012,2.75);
#3732=CIRCLE('',#33014,2.75);
#3733=CIRCLE('',#33016,2.75);
#3734=CIRCLE('',#33018,2.75);
#3735=CIRCLE('',#33020,2.75);
#3736=CIRCLE('',#33022,2.75);
#3737=CIRCLE('',#33024,2.75);
#3738=CIRCLE('',#33026,2.75);
#3739=CIRCLE('',#33028,2.75);
#3740=CIRCLE('',#33030,2.75);
#3741=CIRCLE('',#33032,2.75);
#3742=CIRCLE('',#33034,2.75);
#3743=CIRCLE('',#33036,2.75);
#3744=CIRCLE('',#33038,2.75);
#3745=CIRCLE('',#33040,2.75);
#3746=CIRCLE('',#33042,2.75);
#3747=CIRCLE('',#33044,2.75);
#3748=CIRCLE('',#33046,2.75);
#3749=CIRCLE('',#33048,2.75);
#3750=CIRCLE('',#33050,2.75);
#3751=CIRCLE('',#33052,2.75);
#3752=CIRCLE('',#33054,2.75);
#3753=CIRCLE('',#33056,2.75);
#3754=CIRCLE('',#33058,2.75);
#3755=CIRCLE('',#33060,2.75);
#3756=CIRCLE('',#33062,2.75);
#3757=CIRCLE('',#33064,2.75);
#3758=CIRCLE('',#33066,2.75);
#3759=CIRCLE('',#33068,2.75);
#3760=CIRCLE('',#33070,2.75);
#3761=CIRCLE('',#33072,2.75);
#3762=CIRCLE('',#33074,2.75);
#3763=CIRCLE('',#33076,2.75);
#3764=CIRCLE('',#33078,2.75);
#3765=CIRCLE('',#33080,2.75);
#3766=CIRCLE('',#33082,2.75);
#3767=CIRCLE('',#33084,2.75);
#3768=CIRCLE('',#33086,2.75);
#3769=CIRCLE('',#33088,2.75);
#3770=CIRCLE('',#33090,2.75);
#3771=CIRCLE('',#33092,2.75);
#3772=CIRCLE('',#33094,2.75);
#3773=CIRCLE('',#33337,2.75);
#3774=CIRCLE('',#33339,2.75);
#3775=CIRCLE('',#33579,1.5);
#3776=CIRCLE('',#33580,1.5);
#3777=CIRCLE('',#33609,1.17524047358084);
#3778=CIRCLE('',#33611,1.17524047358084);
#3779=CIRCLE('',#33642,1.1752404735812);
#3780=CIRCLE('',#33644,1.17524047358084);
#3781=CIRCLE('',#33645,1.5);
#3782=CIRCLE('',#33693,1.55162884844711);
#3783=CIRCLE('',#33695,2.61372936963188);
#3784=CIRCLE('',#33696,0.0468749999999982);
#3785=CIRCLE('',#33697,2.58058373926377);
#3786=CIRCLE('',#33699,2.73627063036812);
#3787=CIRCLE('',#33701,2.73627063036812);
#3788=CIRCLE('',#33703,2.73627063036812);
#3789=CIRCLE('',#33705,2.73627063036812);
#3790=CIRCLE('',#33707,2.73627063036812);
#3791=CIRCLE('',#33709,2.73627063036812);
#3792=CIRCLE('',#33711,2.73627063036812);
#3793=CIRCLE('',#33713,2.73627063036812);
#3794=CIRCLE('',#33715,2.73627063036812);
#3795=CIRCLE('',#33717,2.73627063036812);
#3796=CIRCLE('',#33719,2.73627063036812);
#3797=CIRCLE('',#33721,2.73627063036812);
#3798=CIRCLE('',#33723,2.73627063036812);
#3799=CIRCLE('',#33725,2.73627063036812);
#3800=CIRCLE('',#33727,2.73627063036812);
#3801=CIRCLE('',#33729,2.73627063036812);
#3802=CIRCLE('',#33731,2.73627063036812);
#3803=CIRCLE('',#33733,2.73627063036812);
#3804=CIRCLE('',#33735,2.73627063036812);
#3805=CIRCLE('',#33737,2.73627063036812);
#3806=CIRCLE('',#33739,2.73627063036812);
#3807=CIRCLE('',#33741,2.73627063036812);
#3808=CIRCLE('',#33743,2.73627063036812);
#3809=CIRCLE('',#33745,2.73627063036812);
#3810=CIRCLE('',#33747,2.73627063036812);
#3811=CIRCLE('',#33749,2.73627063036812);
#3812=CIRCLE('',#33751,2.73627063036812);
#3813=CIRCLE('',#33753,2.73627063036812);
#3814=CIRCLE('',#33755,2.73627063036812);
#3815=CIRCLE('',#33757,2.73627063036812);
#3816=CIRCLE('',#33759,2.73627063036812);
#3817=CIRCLE('',#33761,2.73627063036812);
#3818=CIRCLE('',#33763,2.73627063036812);
#3819=CIRCLE('',#33765,2.73627063036812);
#3820=CIRCLE('',#33767,2.73627063036812);
#3821=CIRCLE('',#33769,2.73627063036812);
#3822=CIRCLE('',#33771,2.73627063036812);
#3823=CIRCLE('',#33773,2.73627063036812);
#3824=CIRCLE('',#33775,2.73627063036812);
#3825=CIRCLE('',#33777,2.73627063036812);
#3826=CIRCLE('',#33779,2.73627063036812);
#3827=CIRCLE('',#33781,2.73627063036812);
#3828=CIRCLE('',#33783,2.73627063036812);
#3829=CIRCLE('',#33785,2.73627063036812);
#3830=CIRCLE('',#33787,2.73627063036812);
#3831=CIRCLE('',#33789,2.73627063036812);
#3832=CIRCLE('',#33790,2.73627063036812);
#3833=CIRCLE('',#33791,2.73627063036812);
#3834=CIRCLE('',#33792,2.73627063036812);
#3835=CIRCLE('',#33793,2.73627063036812);
#3836=CIRCLE('',#33794,2.73627063036812);
#3837=CIRCLE('',#33795,2.73627063036812);
#3838=CIRCLE('',#33796,2.73627063036812);
#3839=CIRCLE('',#33797,2.73627063036812);
#3840=CIRCLE('',#33798,2.73627063036812);
#3841=CIRCLE('',#33799,2.73627063036812);
#3842=CIRCLE('',#33800,2.73627063036812);
#3843=CIRCLE('',#33801,2.73627063036812);
#3844=CIRCLE('',#33802,2.73627063036812);
#3845=CIRCLE('',#33803,2.73627063036812);
#3846=CIRCLE('',#33804,2.73627063036812);
#3847=CIRCLE('',#33806,2.73627063036812);
#3848=CIRCLE('',#33808,2.73627063036812);
#3849=CIRCLE('',#33810,2.73627063036812);
#3850=CIRCLE('',#33812,2.73627063036812);
#3851=CIRCLE('',#33814,2.73627063036812);
#3852=CIRCLE('',#33816,2.73627063036812);
#3853=CIRCLE('',#33818,2.73627063036812);
#3854=CIRCLE('',#33820,2.73627063036812);
#3855=CIRCLE('',#33822,2.73627063036812);
#3856=CIRCLE('',#33824,2.73627063036812);
#3857=CIRCLE('',#33826,2.73627063036812);
#3858=CIRCLE('',#33828,2.73627063036812);
#3859=CIRCLE('',#33830,2.73627063036812);
#3860=CIRCLE('',#33832,2.73627063036812);
#3861=CIRCLE('',#33834,2.73627063036812);
#3862=CIRCLE('',#33836,2.73627063036812);
#3863=CIRCLE('',#33838,2.73627063036812);
#3864=CIRCLE('',#33840,2.73627063036812);
#3865=CIRCLE('',#33842,2.73627063036812);
#3866=CIRCLE('',#33844,2.73627063036812);
#3867=CIRCLE('',#33846,2.73627063036812);
#3868=CIRCLE('',#33848,2.73627063036812);
#3869=CIRCLE('',#33850,2.73627063036812);
#3870=CIRCLE('',#33852,2.73627063036812);
#3871=CIRCLE('',#33854,2.73627063036812);
#3872=CIRCLE('',#33856,2.73627063036812);
#3873=CIRCLE('',#33858,2.73627063036812);
#3874=CIRCLE('',#33860,2.73627063036812);
#3875=CIRCLE('',#33862,2.73627063036812);
#3876=CIRCLE('',#33864,2.73627063036812);
#3877=CIRCLE('',#33866,2.73627063036812);
#3878=CIRCLE('',#33868,2.73627063036812);
#3879=CIRCLE('',#33870,2.73627063036812);
#3880=CIRCLE('',#33872,2.73627063036812);
#3881=CIRCLE('',#33874,2.73627063036812);
#3882=CIRCLE('',#33876,2.73627063036812);
#3883=CIRCLE('',#33878,2.73627063036812);
#3884=CIRCLE('',#33880,2.73627063036812);
#3885=CIRCLE('',#33882,2.73627063036812);
#3886=CIRCLE('',#33884,2.73627063036812);
#3887=CIRCLE('',#33886,2.73627063036812);
#3888=CIRCLE('',#33888,2.73627063036812);
#3889=CIRCLE('',#33890,2.73627063036812);
#3890=CIRCLE('',#33892,2.73627063036812);
#3891=CIRCLE('',#33894,2.73627063036812);
#3892=CIRCLE('',#33896,2.73627063036812);
#3893=CIRCLE('',#33898,2.73627063036812);
#3894=CIRCLE('',#33900,2.73627063036812);
#3895=CIRCLE('',#33902,2.73627063036812);
#3896=CIRCLE('',#33904,2.73627063036812);
#3897=CIRCLE('',#33906,2.73627063036812);
#3898=CIRCLE('',#33908,2.73627063036812);
#3899=CIRCLE('',#33910,2.73627063036812);
#3900=CIRCLE('',#33912,2.73627063036812);
#3901=CIRCLE('',#33914,2.73627063036812);
#3902=CIRCLE('',#33916,2.73627063036812);
#3903=CIRCLE('',#33918,2.73627063036812);
#3904=CIRCLE('',#33920,2.73627063036812);
#3905=CIRCLE('',#33922,2.73627063036812);
#3906=CIRCLE('',#33924,2.73627063036812);
#3907=CIRCLE('',#33926,2.73627063036812);
#3908=CIRCLE('',#33928,2.73627063036812);
#3909=CIRCLE('',#33930,2.73627063036812);
#3910=CIRCLE('',#33932,2.73627063036812);
#3911=CIRCLE('',#33934,2.73627063036812);
#3912=CIRCLE('',#33936,2.73627063036812);
#3913=CIRCLE('',#33938,2.73627063036812);
#3914=CIRCLE('',#33940,2.73627063036812);
#3915=CIRCLE('',#33942,2.73627063036812);
#3916=CIRCLE('',#33944,2.73627063036812);
#3917=CIRCLE('',#33946,2.73627063036812);
#3918=CIRCLE('',#33948,2.73627063036812);
#3919=CIRCLE('',#33950,2.73627063036812);
#3920=CIRCLE('',#33952,2.73627063036812);
#3921=CIRCLE('',#33954,2.73627063036812);
#3922=CIRCLE('',#33956,2.73627063036812);
#3923=CIRCLE('',#33958,2.73627063036812);
#3924=CIRCLE('',#33960,2.73627063036812);
#3925=CIRCLE('',#33962,2.73627063036812);
#3926=CIRCLE('',#33963,2.73627063036812);
#3927=CIRCLE('',#33964,2.73627063036812);
#3928=CIRCLE('',#33965,2.73627063036812);
#3929=CIRCLE('',#33966,2.73627063036812);
#3930=CIRCLE('',#33967,2.73627063036812);
#3931=CIRCLE('',#33968,2.73627063036812);
#3932=CIRCLE('',#33969,2.73627063036812);
#3933=CIRCLE('',#33970,2.73627063036812);
#3934=CIRCLE('',#33971,2.73627063036812);
#3935=CIRCLE('',#33972,2.73627063036812);
#3936=CIRCLE('',#33973,2.73627063036812);
#3937=CIRCLE('',#33974,2.73627063036812);
#3938=CIRCLE('',#33975,2.73627063036812);
#3939=CIRCLE('',#33976,2.73627063036812);
#3940=CIRCLE('',#33977,2.73627063036812);
#3941=CIRCLE('',#33979,2.73627063036812);
#3942=CIRCLE('',#33981,2.73627063036812);
#3943=CIRCLE('',#33983,2.73627063036812);
#3944=CIRCLE('',#33985,2.73627063036812);
#3945=CIRCLE('',#33987,2.73627063036812);
#3946=CIRCLE('',#33988,2.68872936963188);
#3947=CIRCLE('',#33989,2.68872936963188);
#3948=CIRCLE('',#33991,2.675);
#3949=CIRCLE('',#33992,0.0468749999999996);
#3950=CIRCLE('',#33994,2.675);
#3951=CIRCLE('',#33996,2.60625);
#3952=CIRCLE('',#33997,0.0687500000000002);
#3953=CIRCLE('',#33999,0.15);
#3954=CIRCLE('',#34000,1.65);
#3955=CIRCLE('',#34003,2.75);
#3956=CIRCLE('',#34008,2.75);
#3957=CIRCLE('',#34012,2.75);
#3958=CIRCLE('',#34016,2.75);
#3959=CIRCLE('',#34020,2.75);
#3960=CIRCLE('',#34024,2.75);
#3961=CIRCLE('',#34028,2.75);
#3962=CIRCLE('',#34032,2.75);
#3963=CIRCLE('',#34036,2.75);
#3964=CIRCLE('',#34040,2.75);
#3965=CIRCLE('',#34044,2.75);
#3966=CIRCLE('',#34048,2.75);
#3967=CIRCLE('',#34052,2.75);
#3968=CIRCLE('',#34056,2.75);
#3969=CIRCLE('',#34060,2.75);
#3970=CIRCLE('',#34064,2.75);
#3971=CIRCLE('',#34068,2.75);
#3972=CIRCLE('',#34072,2.75);
#3973=CIRCLE('',#34076,2.75);
#3974=CIRCLE('',#34080,2.75);
#3975=CIRCLE('',#34084,2.75);
#3976=CIRCLE('',#34088,2.75);
#3977=CIRCLE('',#34092,2.75);
#3978=CIRCLE('',#34096,2.75);
#3979=CIRCLE('',#34100,2.75);
#3980=CIRCLE('',#34104,2.75);
#3981=CIRCLE('',#34108,2.75);
#3982=CIRCLE('',#34112,2.75);
#3983=CIRCLE('',#34116,2.75);
#3984=CIRCLE('',#34120,2.75);
#3985=CIRCLE('',#34124,2.75);
#3986=CIRCLE('',#34128,2.75);
#3987=CIRCLE('',#34132,2.75);
#3988=CIRCLE('',#34136,2.75);
#3989=CIRCLE('',#34140,2.75);
#3990=CIRCLE('',#34144,2.75);
#3991=CIRCLE('',#34148,2.75);
#3992=CIRCLE('',#34152,2.75);
#3993=CIRCLE('',#34156,2.75);
#3994=CIRCLE('',#34160,2.75);
#3995=CIRCLE('',#34164,2.75);
#3996=CIRCLE('',#34168,2.75);
#3997=CIRCLE('',#34172,2.75);
#3998=CIRCLE('',#34176,2.75);
#3999=CIRCLE('',#34180,2.75);
#4000=CIRCLE('',#34184,2.75);
#4001=CIRCLE('',#34188,2.75);
#4002=CIRCLE('',#34192,2.75);
#4003=CIRCLE('',#34196,2.75);
#4004=CIRCLE('',#34200,2.75);
#4005=CIRCLE('',#34204,2.75);
#4006=CIRCLE('',#34208,2.75);
#4007=CIRCLE('',#34212,2.75);
#4008=CIRCLE('',#34216,2.75);
#4009=CIRCLE('',#34220,2.75);
#4010=CIRCLE('',#34224,2.75);
#4011=CIRCLE('',#34228,2.75);
#4012=CIRCLE('',#34232,2.75);
#4013=CIRCLE('',#34236,2.75);
#4014=CIRCLE('',#34240,2.75);
#4015=CIRCLE('',#34244,2.75);
#4016=CIRCLE('',#34248,2.75);
#4017=CIRCLE('',#34252,2.75);
#4018=CIRCLE('',#34256,2.75);
#4019=CIRCLE('',#34259,2.75);
#4020=CIRCLE('',#34263,2.75);
#4021=CIRCLE('',#34267,2.75);
#4022=CIRCLE('',#34271,2.75);
#4023=CIRCLE('',#34275,2.75);
#4024=CIRCLE('',#34279,2.75);
#4025=CIRCLE('',#34283,2.75);
#4026=CIRCLE('',#34287,2.75);
#4027=CIRCLE('',#34291,2.75);
#4028=CIRCLE('',#34295,2.75);
#4029=CIRCLE('',#34299,2.75);
#4030=CIRCLE('',#34303,2.75);
#4031=CIRCLE('',#34307,2.75);
#4032=CIRCLE('',#34311,2.75);
#4033=CIRCLE('',#34316,2.75);
#4034=CIRCLE('',#34318,2.75);
#4035=CIRCLE('',#34320,2.75);
#4036=CIRCLE('',#34322,2.75);
#4037=CIRCLE('',#34324,2.75);
#4038=CIRCLE('',#34326,2.75);
#4039=CIRCLE('',#34328,2.75);
#4040=CIRCLE('',#34330,2.75);
#4041=CIRCLE('',#34332,2.75);
#4042=CIRCLE('',#34334,2.75);
#4043=CIRCLE('',#34336,2.75);
#4044=CIRCLE('',#34338,2.75);
#4045=CIRCLE('',#34340,2.75);
#4046=CIRCLE('',#34342,2.75);
#4047=CIRCLE('',#34344,2.75);
#4048=CIRCLE('',#34346,2.75);
#4049=CIRCLE('',#34348,2.75);
#4050=CIRCLE('',#34350,2.75);
#4051=CIRCLE('',#34352,2.75);
#4052=CIRCLE('',#34354,2.75);
#4053=CIRCLE('',#34356,2.75);
#4054=CIRCLE('',#34358,2.75);
#4055=CIRCLE('',#34360,2.75);
#4056=CIRCLE('',#34362,2.75);
#4057=CIRCLE('',#34364,2.75);
#4058=CIRCLE('',#34366,2.75);
#4059=CIRCLE('',#34368,2.75);
#4060=CIRCLE('',#34370,2.75);
#4061=CIRCLE('',#34372,2.75);
#4062=CIRCLE('',#34374,2.75);
#4063=CIRCLE('',#34376,2.75);
#4064=CIRCLE('',#34378,2.75);
#4065=CIRCLE('',#34380,2.75);
#4066=CIRCLE('',#34382,2.75);
#4067=CIRCLE('',#34384,2.75);
#4068=CIRCLE('',#34386,2.75);
#4069=CIRCLE('',#34388,2.75);
#4070=CIRCLE('',#34390,2.75);
#4071=CIRCLE('',#34392,2.75);
#4072=CIRCLE('',#34394,2.75);
#4073=CIRCLE('',#34396,2.75);
#4074=CIRCLE('',#34398,2.75);
#4075=CIRCLE('',#34400,2.75);
#4076=CIRCLE('',#34402,2.75);
#4077=CIRCLE('',#34404,2.75);
#4078=CIRCLE('',#34406,2.75);
#4079=CIRCLE('',#34408,2.75);
#4080=CIRCLE('',#34410,2.75);
#4081=CIRCLE('',#34412,2.75);
#4082=CIRCLE('',#34414,2.75);
#4083=CIRCLE('',#34416,2.75);
#4084=CIRCLE('',#34418,2.75);
#4085=CIRCLE('',#34420,2.75);
#4086=CIRCLE('',#34422,2.75);
#4087=CIRCLE('',#34424,2.75);
#4088=CIRCLE('',#34426,2.75);
#4089=CIRCLE('',#34428,2.75);
#4090=CIRCLE('',#34430,2.75);
#4091=CIRCLE('',#34432,2.75);
#4092=CIRCLE('',#34434,2.75);
#4093=CIRCLE('',#34436,2.75);
#4094=CIRCLE('',#34438,2.75);
#4095=CIRCLE('',#34440,2.75);
#4096=CIRCLE('',#34442,2.75);
#4097=CIRCLE('',#34444,2.75);
#4098=CIRCLE('',#34446,2.75);
#4099=CIRCLE('',#34448,2.75);
#4100=CIRCLE('',#34450,2.75);
#4101=CIRCLE('',#34452,2.75);
#4102=CIRCLE('',#34454,2.75);
#4103=CIRCLE('',#34456,2.75);
#4104=CIRCLE('',#34458,2.75);
#4105=CIRCLE('',#34460,2.75);
#4106=CIRCLE('',#34462,2.75);
#4107=CIRCLE('',#34464,2.75);
#4108=CIRCLE('',#34466,2.75);
#4109=CIRCLE('',#34468,2.75);
#4110=CIRCLE('',#34470,2.75);
#4111=CIRCLE('',#34472,2.75);
#4112=CIRCLE('',#34474,2.75);
#4113=CIRCLE('',#34717,2.75);
#4114=CIRCLE('',#34719,2.75);
#4115=CIRCLE('',#34959,1.5);
#4116=CIRCLE('',#34960,1.5);
#4117=CIRCLE('',#34989,1.17524047358084);
#4118=CIRCLE('',#34991,1.17524047358084);
#4119=CIRCLE('',#35022,1.1752404735812);
#4120=CIRCLE('',#35024,1.17524047358084);
#4121=CIRCLE('',#35025,1.5);
#4122=CIRCLE('',#35073,1.55162884844711);
#4123=CIRCLE('',#35075,2.61372936963188);
#4124=CIRCLE('',#35076,0.0468749999999982);
#4125=CIRCLE('',#35077,2.58058373926377);
#4126=CIRCLE('',#35079,2.73627063036812);
#4127=CIRCLE('',#35081,2.73627063036812);
#4128=CIRCLE('',#35083,2.73627063036812);
#4129=CIRCLE('',#35085,2.73627063036812);
#4130=CIRCLE('',#35087,2.73627063036812);
#4131=CIRCLE('',#35089,2.73627063036812);
#4132=CIRCLE('',#35091,2.73627063036812);
#4133=CIRCLE('',#35093,2.73627063036812);
#4134=CIRCLE('',#35095,2.73627063036812);
#4135=CIRCLE('',#35097,2.73627063036812);
#4136=CIRCLE('',#35099,2.73627063036812);
#4137=CIRCLE('',#35101,2.73627063036812);
#4138=CIRCLE('',#35103,2.73627063036812);
#4139=CIRCLE('',#35105,2.73627063036812);
#4140=CIRCLE('',#35107,2.73627063036812);
#4141=CIRCLE('',#35109,2.73627063036812);
#4142=CIRCLE('',#35111,2.73627063036812);
#4143=CIRCLE('',#35113,2.73627063036812);
#4144=CIRCLE('',#35115,2.73627063036812);
#4145=CIRCLE('',#35117,2.73627063036812);
#4146=CIRCLE('',#35119,2.73627063036812);
#4147=CIRCLE('',#35121,2.73627063036812);
#4148=CIRCLE('',#35123,2.73627063036812);
#4149=CIRCLE('',#35125,2.73627063036812);
#4150=CIRCLE('',#35127,2.73627063036812);
#4151=CIRCLE('',#35129,2.73627063036812);
#4152=CIRCLE('',#35131,2.73627063036812);
#4153=CIRCLE('',#35133,2.73627063036812);
#4154=CIRCLE('',#35135,2.73627063036812);
#4155=CIRCLE('',#35137,2.73627063036812);
#4156=CIRCLE('',#35139,2.73627063036812);
#4157=CIRCLE('',#35141,2.73627063036812);
#4158=CIRCLE('',#35143,2.73627063036812);
#4159=CIRCLE('',#35145,2.73627063036812);
#4160=CIRCLE('',#35147,2.73627063036812);
#4161=CIRCLE('',#35149,2.73627063036812);
#4162=CIRCLE('',#35151,2.73627063036812);
#4163=CIRCLE('',#35153,2.73627063036812);
#4164=CIRCLE('',#35155,2.73627063036812);
#4165=CIRCLE('',#35157,2.73627063036812);
#4166=CIRCLE('',#35159,2.73627063036812);
#4167=CIRCLE('',#35161,2.73627063036812);
#4168=CIRCLE('',#35163,2.73627063036812);
#4169=CIRCLE('',#35165,2.73627063036812);
#4170=CIRCLE('',#35167,2.73627063036812);
#4171=CIRCLE('',#35169,2.73627063036812);
#4172=CIRCLE('',#35170,2.73627063036812);
#4173=CIRCLE('',#35171,2.73627063036812);
#4174=CIRCLE('',#35172,2.73627063036812);
#4175=CIRCLE('',#35173,2.73627063036812);
#4176=CIRCLE('',#35174,2.73627063036812);
#4177=CIRCLE('',#35175,2.73627063036812);
#4178=CIRCLE('',#35176,2.73627063036812);
#4179=CIRCLE('',#35177,2.73627063036812);
#4180=CIRCLE('',#35178,2.73627063036812);
#4181=CIRCLE('',#35179,2.73627063036812);
#4182=CIRCLE('',#35180,2.73627063036812);
#4183=CIRCLE('',#35181,2.73627063036812);
#4184=CIRCLE('',#35182,2.73627063036812);
#4185=CIRCLE('',#35183,2.73627063036812);
#4186=CIRCLE('',#35184,2.73627063036812);
#4187=CIRCLE('',#35186,2.73627063036812);
#4188=CIRCLE('',#35188,2.73627063036812);
#4189=CIRCLE('',#35190,2.73627063036812);
#4190=CIRCLE('',#35192,2.73627063036812);
#4191=CIRCLE('',#35194,2.73627063036812);
#4192=CIRCLE('',#35196,2.73627063036812);
#4193=CIRCLE('',#35198,2.73627063036812);
#4194=CIRCLE('',#35200,2.73627063036812);
#4195=CIRCLE('',#35202,2.73627063036812);
#4196=CIRCLE('',#35204,2.73627063036812);
#4197=CIRCLE('',#35206,2.73627063036812);
#4198=CIRCLE('',#35208,2.73627063036812);
#4199=CIRCLE('',#35210,2.73627063036812);
#4200=CIRCLE('',#35212,2.73627063036812);
#4201=CIRCLE('',#35214,2.73627063036812);
#4202=CIRCLE('',#35216,2.73627063036812);
#4203=CIRCLE('',#35218,2.73627063036812);
#4204=CIRCLE('',#35220,2.73627063036812);
#4205=CIRCLE('',#35222,2.73627063036812);
#4206=CIRCLE('',#35224,2.73627063036812);
#4207=CIRCLE('',#35226,2.73627063036812);
#4208=CIRCLE('',#35228,2.73627063036812);
#4209=CIRCLE('',#35230,2.73627063036812);
#4210=CIRCLE('',#35232,2.73627063036812);
#4211=CIRCLE('',#35234,2.73627063036812);
#4212=CIRCLE('',#35236,2.73627063036812);
#4213=CIRCLE('',#35238,2.73627063036812);
#4214=CIRCLE('',#35240,2.73627063036812);
#4215=CIRCLE('',#35242,2.73627063036812);
#4216=CIRCLE('',#35244,2.73627063036812);
#4217=CIRCLE('',#35246,2.73627063036812);
#4218=CIRCLE('',#35248,2.73627063036812);
#4219=CIRCLE('',#35250,2.73627063036812);
#4220=CIRCLE('',#35252,2.73627063036812);
#4221=CIRCLE('',#35254,2.73627063036812);
#4222=CIRCLE('',#35256,2.73627063036812);
#4223=CIRCLE('',#35258,2.73627063036812);
#4224=CIRCLE('',#35260,2.73627063036812);
#4225=CIRCLE('',#35262,2.73627063036812);
#4226=CIRCLE('',#35264,2.73627063036812);
#4227=CIRCLE('',#35266,2.73627063036812);
#4228=CIRCLE('',#35268,2.73627063036812);
#4229=CIRCLE('',#35270,2.73627063036812);
#4230=CIRCLE('',#35272,2.73627063036812);
#4231=CIRCLE('',#35274,2.73627063036812);
#4232=CIRCLE('',#35276,2.73627063036812);
#4233=CIRCLE('',#35278,2.73627063036812);
#4234=CIRCLE('',#35280,2.73627063036812);
#4235=CIRCLE('',#35282,2.73627063036812);
#4236=CIRCLE('',#35284,2.73627063036812);
#4237=CIRCLE('',#35286,2.73627063036812);
#4238=CIRCLE('',#35288,2.73627063036812);
#4239=CIRCLE('',#35290,2.73627063036812);
#4240=CIRCLE('',#35292,2.73627063036812);
#4241=CIRCLE('',#35294,2.73627063036812);
#4242=CIRCLE('',#35296,2.73627063036812);
#4243=CIRCLE('',#35298,2.73627063036812);
#4244=CIRCLE('',#35300,2.73627063036812);
#4245=CIRCLE('',#35302,2.73627063036812);
#4246=CIRCLE('',#35304,2.73627063036812);
#4247=CIRCLE('',#35306,2.73627063036812);
#4248=CIRCLE('',#35308,2.73627063036812);
#4249=CIRCLE('',#35310,2.73627063036812);
#4250=CIRCLE('',#35312,2.73627063036812);
#4251=CIRCLE('',#35314,2.73627063036812);
#4252=CIRCLE('',#35316,2.73627063036812);
#4253=CIRCLE('',#35318,2.73627063036812);
#4254=CIRCLE('',#35320,2.73627063036812);
#4255=CIRCLE('',#35322,2.73627063036812);
#4256=CIRCLE('',#35324,2.73627063036812);
#4257=CIRCLE('',#35326,2.73627063036812);
#4258=CIRCLE('',#35328,2.73627063036812);
#4259=CIRCLE('',#35330,2.73627063036812);
#4260=CIRCLE('',#35332,2.73627063036812);
#4261=CIRCLE('',#35334,2.73627063036812);
#4262=CIRCLE('',#35336,2.73627063036812);
#4263=CIRCLE('',#35338,2.73627063036812);
#4264=CIRCLE('',#35340,2.73627063036812);
#4265=CIRCLE('',#35342,2.73627063036812);
#4266=CIRCLE('',#35343,2.73627063036812);
#4267=CIRCLE('',#35344,2.73627063036812);
#4268=CIRCLE('',#35345,2.73627063036812);
#4269=CIRCLE('',#35346,2.73627063036812);
#4270=CIRCLE('',#35347,2.73627063036812);
#4271=CIRCLE('',#35348,2.73627063036812);
#4272=CIRCLE('',#35349,2.73627063036812);
#4273=CIRCLE('',#35350,2.73627063036812);
#4274=CIRCLE('',#35351,2.73627063036812);
#4275=CIRCLE('',#35352,2.73627063036812);
#4276=CIRCLE('',#35353,2.73627063036812);
#4277=CIRCLE('',#35354,2.73627063036812);
#4278=CIRCLE('',#35355,2.73627063036812);
#4279=CIRCLE('',#35356,2.73627063036812);
#4280=CIRCLE('',#35357,2.73627063036812);
#4281=CIRCLE('',#35359,2.73627063036812);
#4282=CIRCLE('',#35361,2.73627063036812);
#4283=CIRCLE('',#35363,2.73627063036812);
#4284=CIRCLE('',#35365,2.73627063036812);
#4285=CIRCLE('',#35367,2.73627063036812);
#4286=CIRCLE('',#35368,2.68872936963188);
#4287=CIRCLE('',#35369,2.68872936963188);
#4288=CIRCLE('',#35371,2.675);
#4289=CIRCLE('',#35372,0.0468749999999996);
#4290=CIRCLE('',#35374,2.675);
#4291=CIRCLE('',#35376,2.60625);
#4292=CIRCLE('',#35377,0.0687500000000002);
#4293=CIRCLE('',#35379,0.15);
#4294=CIRCLE('',#35380,1.65);
#4295=CIRCLE('',#35383,2.75);
#4296=CIRCLE('',#35388,2.75);
#4297=CIRCLE('',#35392,2.75);
#4298=CIRCLE('',#35396,2.75);
#4299=CIRCLE('',#35400,2.75);
#4300=CIRCLE('',#35404,2.75);
#4301=CIRCLE('',#35408,2.75);
#4302=CIRCLE('',#35412,2.75);
#4303=CIRCLE('',#35416,2.75);
#4304=CIRCLE('',#35420,2.75);
#4305=CIRCLE('',#35424,2.75);
#4306=CIRCLE('',#35428,2.75);
#4307=CIRCLE('',#35432,2.75);
#4308=CIRCLE('',#35436,2.75);
#4309=CIRCLE('',#35440,2.75);
#4310=CIRCLE('',#35444,2.75);
#4311=CIRCLE('',#35448,2.75);
#4312=CIRCLE('',#35452,2.75);
#4313=CIRCLE('',#35456,2.75);
#4314=CIRCLE('',#35460,2.75);
#4315=CIRCLE('',#35464,2.75);
#4316=CIRCLE('',#35468,2.75);
#4317=CIRCLE('',#35472,2.75);
#4318=CIRCLE('',#35476,2.75);
#4319=CIRCLE('',#35480,2.75);
#4320=CIRCLE('',#35484,2.75);
#4321=CIRCLE('',#35488,2.75);
#4322=CIRCLE('',#35492,2.75);
#4323=CIRCLE('',#35496,2.75);
#4324=CIRCLE('',#35500,2.75);
#4325=CIRCLE('',#35504,2.75);
#4326=CIRCLE('',#35508,2.75);
#4327=CIRCLE('',#35512,2.75);
#4328=CIRCLE('',#35516,2.75);
#4329=CIRCLE('',#35520,2.75);
#4330=CIRCLE('',#35524,2.75);
#4331=CIRCLE('',#35528,2.75);
#4332=CIRCLE('',#35532,2.75);
#4333=CIRCLE('',#35536,2.75);
#4334=CIRCLE('',#35540,2.75);
#4335=CIRCLE('',#35544,2.75);
#4336=CIRCLE('',#35548,2.75);
#4337=CIRCLE('',#35552,2.75);
#4338=CIRCLE('',#35556,2.75);
#4339=CIRCLE('',#35560,2.75);
#4340=CIRCLE('',#35564,2.75);
#4341=CIRCLE('',#35568,2.75);
#4342=CIRCLE('',#35572,2.75);
#4343=CIRCLE('',#35576,2.75);
#4344=CIRCLE('',#35580,2.75);
#4345=CIRCLE('',#35584,2.75);
#4346=CIRCLE('',#35588,2.75);
#4347=CIRCLE('',#35592,2.75);
#4348=CIRCLE('',#35596,2.75);
#4349=CIRCLE('',#35600,2.75);
#4350=CIRCLE('',#35604,2.75);
#4351=CIRCLE('',#35608,2.75);
#4352=CIRCLE('',#35612,2.75);
#4353=CIRCLE('',#35616,2.75);
#4354=CIRCLE('',#35620,2.75);
#4355=CIRCLE('',#35624,2.75);
#4356=CIRCLE('',#35628,2.75);
#4357=CIRCLE('',#35632,2.75);
#4358=CIRCLE('',#35636,2.75);
#4359=CIRCLE('',#35639,2.75);
#4360=CIRCLE('',#35643,2.75);
#4361=CIRCLE('',#35647,2.75);
#4362=CIRCLE('',#35651,2.75);
#4363=CIRCLE('',#35655,2.75);
#4364=CIRCLE('',#35659,2.75);
#4365=CIRCLE('',#35663,2.75);
#4366=CIRCLE('',#35667,2.75);
#4367=CIRCLE('',#35671,2.75);
#4368=CIRCLE('',#35675,2.75);
#4369=CIRCLE('',#35679,2.75);
#4370=CIRCLE('',#35683,2.75);
#4371=CIRCLE('',#35687,2.75);
#4372=CIRCLE('',#35691,2.75);
#4373=CIRCLE('',#35696,2.75);
#4374=CIRCLE('',#35698,2.75);
#4375=CIRCLE('',#35700,2.75);
#4376=CIRCLE('',#35702,2.75);
#4377=CIRCLE('',#35704,2.75);
#4378=CIRCLE('',#35706,2.75);
#4379=CIRCLE('',#35708,2.75);
#4380=CIRCLE('',#35710,2.75);
#4381=CIRCLE('',#35712,2.75);
#4382=CIRCLE('',#35714,2.75);
#4383=CIRCLE('',#35716,2.75);
#4384=CIRCLE('',#35718,2.75);
#4385=CIRCLE('',#35720,2.75);
#4386=CIRCLE('',#35722,2.75);
#4387=CIRCLE('',#35724,2.75);
#4388=CIRCLE('',#35726,2.75);
#4389=CIRCLE('',#35728,2.75);
#4390=CIRCLE('',#35730,2.75);
#4391=CIRCLE('',#35732,2.75);
#4392=CIRCLE('',#35734,2.75);
#4393=CIRCLE('',#35736,2.75);
#4394=CIRCLE('',#35738,2.75);
#4395=CIRCLE('',#35740,2.75);
#4396=CIRCLE('',#35742,2.75);
#4397=CIRCLE('',#35744,2.75);
#4398=CIRCLE('',#35746,2.75);
#4399=CIRCLE('',#35748,2.75);
#4400=CIRCLE('',#35750,2.75);
#4401=CIRCLE('',#35752,2.75);
#4402=CIRCLE('',#35754,2.75);
#4403=CIRCLE('',#35756,2.75);
#4404=CIRCLE('',#35758,2.75);
#4405=CIRCLE('',#35760,2.75);
#4406=CIRCLE('',#35762,2.75);
#4407=CIRCLE('',#35764,2.75);
#4408=CIRCLE('',#35766,2.75);
#4409=CIRCLE('',#35768,2.75);
#4410=CIRCLE('',#35770,2.75);
#4411=CIRCLE('',#35772,2.75);
#4412=CIRCLE('',#35774,2.75);
#4413=CIRCLE('',#35776,2.75);
#4414=CIRCLE('',#35778,2.75);
#4415=CIRCLE('',#35780,2.75);
#4416=CIRCLE('',#35782,2.75);
#4417=CIRCLE('',#35784,2.75);
#4418=CIRCLE('',#35786,2.75);
#4419=CIRCLE('',#35788,2.75);
#4420=CIRCLE('',#35790,2.75);
#4421=CIRCLE('',#35792,2.75);
#4422=CIRCLE('',#35794,2.75);
#4423=CIRCLE('',#35796,2.75);
#4424=CIRCLE('',#35798,2.75);
#4425=CIRCLE('',#35800,2.75);
#4426=CIRCLE('',#35802,2.75);
#4427=CIRCLE('',#35804,2.75);
#4428=CIRCLE('',#35806,2.75);
#4429=CIRCLE('',#35808,2.75);
#4430=CIRCLE('',#35810,2.75);
#4431=CIRCLE('',#35812,2.75);
#4432=CIRCLE('',#35814,2.75);
#4433=CIRCLE('',#35816,2.75);
#4434=CIRCLE('',#35818,2.75);
#4435=CIRCLE('',#35820,2.75);
#4436=CIRCLE('',#35822,2.75);
#4437=CIRCLE('',#35824,2.75);
#4438=CIRCLE('',#35826,2.75);
#4439=CIRCLE('',#35828,2.75);
#4440=CIRCLE('',#35830,2.75);
#4441=CIRCLE('',#35832,2.75);
#4442=CIRCLE('',#35834,2.75);
#4443=CIRCLE('',#35836,2.75);
#4444=CIRCLE('',#35838,2.75);
#4445=CIRCLE('',#35840,2.75);
#4446=CIRCLE('',#35842,2.75);
#4447=CIRCLE('',#35844,2.75);
#4448=CIRCLE('',#35846,2.75);
#4449=CIRCLE('',#35848,2.75);
#4450=CIRCLE('',#35850,2.75);
#4451=CIRCLE('',#35852,2.75);
#4452=CIRCLE('',#35854,2.75);
#4453=CIRCLE('',#36097,2.75);
#4454=CIRCLE('',#36099,2.75);
#4455=CYLINDRICAL_SURFACE('',#32129,40.);
#4456=CYLINDRICAL_SURFACE('',#32144,1.5);
#4457=CYLINDRICAL_SURFACE('',#32147,1.5);
#4458=CYLINDRICAL_SURFACE('',#32150,1.5);
#4459=CYLINDRICAL_SURFACE('',#32153,5.);
#4460=CYLINDRICAL_SURFACE('',#32157,5.);
#4461=CYLINDRICAL_SURFACE('',#32161,5.);
#4462=CYLINDRICAL_SURFACE('',#32165,5.);
#4463=CYLINDRICAL_SURFACE('',#32168,40.);
#4464=CYLINDRICAL_SURFACE('',#32179,5.);
#4465=CYLINDRICAL_SURFACE('',#32181,40.);
#4466=CYLINDRICAL_SURFACE('',#32183,5.);
#4467=CYLINDRICAL_SURFACE('',#32185,5.);
#4468=CYLINDRICAL_SURFACE('',#32187,5.);
#4469=CYLINDRICAL_SURFACE('',#32189,5.);
#4470=CYLINDRICAL_SURFACE('',#32192,40.);
#4471=CYLINDRICAL_SURFACE('',#32198,1.5);
#4472=CYLINDRICAL_SURFACE('',#32201,1.5);
#4473=CYLINDRICAL_SURFACE('',#32202,1.5);
#4474=CYLINDRICAL_SURFACE('',#32203,1.5);
#4475=CYLINDRICAL_SURFACE('',#32204,1.5);
#4476=CYLINDRICAL_SURFACE('',#32205,1.5);
#4477=CYLINDRICAL_SURFACE('',#32206,1.5);
#4478=CYLINDRICAL_SURFACE('',#32207,1.5);
#4479=CYLINDRICAL_SURFACE('',#32208,1.5);
#4480=CYLINDRICAL_SURFACE('',#32209,1.5);
#4481=CYLINDRICAL_SURFACE('',#32210,1.5);
#4482=CYLINDRICAL_SURFACE('',#32211,1.5);
#4483=CYLINDRICAL_SURFACE('',#32212,1.5);
#4484=CYLINDRICAL_SURFACE('',#32213,1.5);
#4485=CYLINDRICAL_SURFACE('',#32214,1.5);
#4486=CYLINDRICAL_SURFACE('',#32215,1.5);
#4487=CYLINDRICAL_SURFACE('',#32216,1.5);
#4488=CYLINDRICAL_SURFACE('',#32217,1.5);
#4489=CYLINDRICAL_SURFACE('',#32218,1.5);
#4490=CYLINDRICAL_SURFACE('',#32219,1.5);
#4491=CYLINDRICAL_SURFACE('',#32220,1.5);
#4492=CYLINDRICAL_SURFACE('',#32221,1.5);
#4493=CYLINDRICAL_SURFACE('',#32222,1.5);
#4494=CYLINDRICAL_SURFACE('',#32223,1.5);
#4495=CYLINDRICAL_SURFACE('',#32224,1.5);
#4496=CYLINDRICAL_SURFACE('',#32225,1.5);
#4497=CYLINDRICAL_SURFACE('',#32226,1.5);
#4498=CYLINDRICAL_SURFACE('',#32227,1.5);
#4499=CYLINDRICAL_SURFACE('',#32230,1.17524047358084);
#4500=CYLINDRICAL_SURFACE('',#32232,1.17524047358084);
#4501=CYLINDRICAL_SURFACE('',#32233,1.17524047358084);
#4502=CYLINDRICAL_SURFACE('',#32234,1.17524047358084);
#4503=CYLINDRICAL_SURFACE('',#32235,1.17524047358084);
#4504=CYLINDRICAL_SURFACE('',#32236,1.17524047358084);
#4505=CYLINDRICAL_SURFACE('',#32237,1.17524047358084);
#4506=CYLINDRICAL_SURFACE('',#32238,1.17524047358084);
#4507=CYLINDRICAL_SURFACE('',#32239,1.17524047358084);
#4508=CYLINDRICAL_SURFACE('',#32240,1.17524047358084);
#4509=CYLINDRICAL_SURFACE('',#32241,1.17524047358084);
#4510=CYLINDRICAL_SURFACE('',#32242,1.17524047358084);
#4511=CYLINDRICAL_SURFACE('',#32243,1.17524047358084);
#4512=CYLINDRICAL_SURFACE('',#32244,1.17524047358084);
#4513=CYLINDRICAL_SURFACE('',#32245,1.17524047358084);
#4514=CYLINDRICAL_SURFACE('',#32246,1.17524047358084);
#4515=CYLINDRICAL_SURFACE('',#32247,1.17524047358084);
#4516=CYLINDRICAL_SURFACE('',#32248,1.17524047358084);
#4517=CYLINDRICAL_SURFACE('',#32249,1.17524047358084);
#4518=CYLINDRICAL_SURFACE('',#32250,1.17524047358084);
#4519=CYLINDRICAL_SURFACE('',#32251,1.17524047358084);
#4520=CYLINDRICAL_SURFACE('',#32252,1.17524047358084);
#4521=CYLINDRICAL_SURFACE('',#32253,1.17524047358084);
#4522=CYLINDRICAL_SURFACE('',#32254,1.17524047358084);
#4523=CYLINDRICAL_SURFACE('',#32255,1.17524047358084);
#4524=CYLINDRICAL_SURFACE('',#32256,1.17524047358084);
#4525=CYLINDRICAL_SURFACE('',#32257,1.17524047358084);
#4526=CYLINDRICAL_SURFACE('',#32258,1.17524047358084);
#4527=CYLINDRICAL_SURFACE('',#32259,1.17524047358084);
#4528=CYLINDRICAL_SURFACE('',#32260,1.17524047358084);
#4529=CYLINDRICAL_SURFACE('',#32261,1.17524047358084);
#4530=CYLINDRICAL_SURFACE('',#32266,1.5);
#4531=CYLINDRICAL_SURFACE('',#32267,0.0137499999999999);
#4532=CYLINDRICAL_SURFACE('',#32270,0.0137499999999999);
#4533=CYLINDRICAL_SURFACE('',#32273,0.0137499999999999);
#4534=CYLINDRICAL_SURFACE('',#32276,0.0137499999999999);
#4535=CYLINDRICAL_SURFACE('',#32279,0.0137499999999999);
#4536=CYLINDRICAL_SURFACE('',#32282,0.0137499999999999);
#4537=CYLINDRICAL_SURFACE('',#32285,0.0137499999999999);
#4538=CYLINDRICAL_SURFACE('',#32288,0.0137499999999999);
#4539=CYLINDRICAL_SURFACE('',#32291,0.0137499999999999);
#4540=CYLINDRICAL_SURFACE('',#32294,0.0137499999999999);
#4541=CYLINDRICAL_SURFACE('',#32297,0.0137499999999997);
#4542=CYLINDRICAL_SURFACE('',#32300,0.0137499999999997);
#4543=CYLINDRICAL_SURFACE('',#32303,0.0137499999999997);
#4544=CYLINDRICAL_SURFACE('',#32306,0.0137499999999997);
#4545=CYLINDRICAL_SURFACE('',#32309,0.0137499999999997);
#4546=CYLINDRICAL_SURFACE('',#32613,2.675);
#4547=CYLINDRICAL_SURFACE('',#32937,2.75);
#4548=CYLINDRICAL_SURFACE('',#32939,2.75);
#4549=CYLINDRICAL_SURFACE('',#32941,2.75);
#4550=CYLINDRICAL_SURFACE('',#32943,2.75);
#4551=CYLINDRICAL_SURFACE('',#32945,2.75);
#4552=CYLINDRICAL_SURFACE('',#32947,2.75);
#4553=CYLINDRICAL_SURFACE('',#32949,2.75);
#4554=CYLINDRICAL_SURFACE('',#32951,2.75);
#4555=CYLINDRICAL_SURFACE('',#32953,2.75);
#4556=CYLINDRICAL_SURFACE('',#32955,2.75);
#4557=CYLINDRICAL_SURFACE('',#32957,2.75);
#4558=CYLINDRICAL_SURFACE('',#32959,2.75);
#4559=CYLINDRICAL_SURFACE('',#32961,2.75);
#4560=CYLINDRICAL_SURFACE('',#32963,2.75);
#4561=CYLINDRICAL_SURFACE('',#32965,2.75);
#4562=CYLINDRICAL_SURFACE('',#32967,2.75);
#4563=CYLINDRICAL_SURFACE('',#32969,2.75);
#4564=CYLINDRICAL_SURFACE('',#32971,2.75);
#4565=CYLINDRICAL_SURFACE('',#32973,2.75);
#4566=CYLINDRICAL_SURFACE('',#32975,2.75);
#4567=CYLINDRICAL_SURFACE('',#32977,2.75);
#4568=CYLINDRICAL_SURFACE('',#32979,2.75);
#4569=CYLINDRICAL_SURFACE('',#32981,2.75);
#4570=CYLINDRICAL_SURFACE('',#32983,2.75);
#4571=CYLINDRICAL_SURFACE('',#32985,2.75);
#4572=CYLINDRICAL_SURFACE('',#32987,2.75);
#4573=CYLINDRICAL_SURFACE('',#32989,2.75);
#4574=CYLINDRICAL_SURFACE('',#32991,2.75);
#4575=CYLINDRICAL_SURFACE('',#32993,2.75);
#4576=CYLINDRICAL_SURFACE('',#32995,2.75);
#4577=CYLINDRICAL_SURFACE('',#32997,2.75);
#4578=CYLINDRICAL_SURFACE('',#32999,2.75);
#4579=CYLINDRICAL_SURFACE('',#33001,2.75);
#4580=CYLINDRICAL_SURFACE('',#33003,2.75);
#4581=CYLINDRICAL_SURFACE('',#33005,2.75);
#4582=CYLINDRICAL_SURFACE('',#33007,2.75);
#4583=CYLINDRICAL_SURFACE('',#33009,2.75);
#4584=CYLINDRICAL_SURFACE('',#33011,2.75);
#4585=CYLINDRICAL_SURFACE('',#33013,2.75);
#4586=CYLINDRICAL_SURFACE('',#33015,2.75);
#4587=CYLINDRICAL_SURFACE('',#33017,2.75);
#4588=CYLINDRICAL_SURFACE('',#33019,2.75);
#4589=CYLINDRICAL_SURFACE('',#33021,2.75);
#4590=CYLINDRICAL_SURFACE('',#33023,2.75);
#4591=CYLINDRICAL_SURFACE('',#33025,2.75);
#4592=CYLINDRICAL_SURFACE('',#33027,2.75);
#4593=CYLINDRICAL_SURFACE('',#33029,2.75);
#4594=CYLINDRICAL_SURFACE('',#33031,2.75);
#4595=CYLINDRICAL_SURFACE('',#33033,2.75);
#4596=CYLINDRICAL_SURFACE('',#33035,2.75);
#4597=CYLINDRICAL_SURFACE('',#33037,2.75);
#4598=CYLINDRICAL_SURFACE('',#33039,2.75);
#4599=CYLINDRICAL_SURFACE('',#33041,2.75);
#4600=CYLINDRICAL_SURFACE('',#33043,2.75);
#4601=CYLINDRICAL_SURFACE('',#33045,2.75);
#4602=CYLINDRICAL_SURFACE('',#33047,2.75);
#4603=CYLINDRICAL_SURFACE('',#33049,2.75);
#4604=CYLINDRICAL_SURFACE('',#33051,2.75);
#4605=CYLINDRICAL_SURFACE('',#33053,2.75);
#4606=CYLINDRICAL_SURFACE('',#33055,2.75);
#4607=CYLINDRICAL_SURFACE('',#33057,2.75);
#4608=CYLINDRICAL_SURFACE('',#33059,2.75);
#4609=CYLINDRICAL_SURFACE('',#33061,2.75);
#4610=CYLINDRICAL_SURFACE('',#33063,2.75);
#4611=CYLINDRICAL_SURFACE('',#33065,2.75);
#4612=CYLINDRICAL_SURFACE('',#33067,2.75);
#4613=CYLINDRICAL_SURFACE('',#33069,2.75);
#4614=CYLINDRICAL_SURFACE('',#33071,2.75);
#4615=CYLINDRICAL_SURFACE('',#33073,2.75);
#4616=CYLINDRICAL_SURFACE('',#33075,2.75);
#4617=CYLINDRICAL_SURFACE('',#33077,2.75);
#4618=CYLINDRICAL_SURFACE('',#33079,2.75);
#4619=CYLINDRICAL_SURFACE('',#33081,2.75);
#4620=CYLINDRICAL_SURFACE('',#33083,2.75);
#4621=CYLINDRICAL_SURFACE('',#33085,2.75);
#4622=CYLINDRICAL_SURFACE('',#33087,2.75);
#4623=CYLINDRICAL_SURFACE('',#33089,2.75);
#4624=CYLINDRICAL_SURFACE('',#33091,2.75);
#4625=CYLINDRICAL_SURFACE('',#33093,2.75);
#4626=CYLINDRICAL_SURFACE('',#33338,2.75);
#4627=CYLINDRICAL_SURFACE('',#33353,0.0137499999999997);
#4628=CYLINDRICAL_SURFACE('',#33356,0.0137499999999997);
#4629=CYLINDRICAL_SURFACE('',#33359,0.0137499999999997);
#4630=CYLINDRICAL_SURFACE('',#33362,0.0137499999999997);
#4631=CYLINDRICAL_SURFACE('',#33365,0.0137499999999998);
#4632=CYLINDRICAL_SURFACE('',#33368,0.0137499999999998);
#4633=CYLINDRICAL_SURFACE('',#33371,0.0137499999999997);
#4634=CYLINDRICAL_SURFACE('',#33392,0.0137499999999997);
#4635=CYLINDRICAL_SURFACE('',#33395,0.0137499999999998);
#4636=CYLINDRICAL_SURFACE('',#33398,0.0137499999999998);
#4637=CYLINDRICAL_SURFACE('',#33401,0.0137499999999997);
#4638=CYLINDRICAL_SURFACE('',#33404,0.0137499999999997);
#4639=CYLINDRICAL_SURFACE('',#33407,0.0137499999999997);
#4640=CYLINDRICAL_SURFACE('',#33410,0.0137499999999997);
#4641=CYLINDRICAL_SURFACE('',#33413,0.0137499999999997);
#4642=CYLINDRICAL_SURFACE('',#33416,0.0137499999999997);
#4643=CYLINDRICAL_SURFACE('',#33419,0.0137499999999999);
#4644=CYLINDRICAL_SURFACE('',#33422,0.0137499999999999);
#4645=CYLINDRICAL_SURFACE('',#33425,0.0137499999999999);
#4646=CYLINDRICAL_SURFACE('',#33428,0.0137499999999999);
#4647=CYLINDRICAL_SURFACE('',#33431,0.0137499999999999);
#4648=CYLINDRICAL_SURFACE('',#33434,0.0137499999999999);
#4649=CYLINDRICAL_SURFACE('',#33437,0.0137499999999999);
#4650=CYLINDRICAL_SURFACE('',#33440,0.0137499999999999);
#4651=CYLINDRICAL_SURFACE('',#33443,0.0137499999999999);
#4652=CYLINDRICAL_SURFACE('',#33446,0.0137499999999997);
#4653=CYLINDRICAL_SURFACE('',#33449,0.0137499999999997);
#4654=CYLINDRICAL_SURFACE('',#33452,0.0137499999999997);
#4655=CYLINDRICAL_SURFACE('',#33455,0.0137499999999998);
#4656=CYLINDRICAL_SURFACE('',#33458,0.0137499999999998);
#4657=CYLINDRICAL_SURFACE('',#33461,0.0137499999999997);
#4658=CYLINDRICAL_SURFACE('',#33464,0.0137499999999997);
#4659=CYLINDRICAL_SURFACE('',#33467,0.0137499999999997);
#4660=CYLINDRICAL_SURFACE('',#33470,0.0137499999999997);
#4661=CYLINDRICAL_SURFACE('',#33473,0.0137499999999997);
#4662=CYLINDRICAL_SURFACE('',#33476,0.0137499999999997);
#4663=CYLINDRICAL_SURFACE('',#33479,0.0137499999999999);
#4664=CYLINDRICAL_SURFACE('',#33482,0.0137499999999999);
#4665=CYLINDRICAL_SURFACE('',#33485,0.0137499999999999);
#4666=CYLINDRICAL_SURFACE('',#33488,0.0137499999999999);
#4667=CYLINDRICAL_SURFACE('',#33491,0.0137499999999999);
#4668=CYLINDRICAL_SURFACE('',#33494,0.0137499999999999);
#4669=CYLINDRICAL_SURFACE('',#33497,0.0137499999999999);
#4670=CYLINDRICAL_SURFACE('',#33500,0.0137499999999999);
#4671=CYLINDRICAL_SURFACE('',#33503,0.0137499999999999);
#4672=CYLINDRICAL_SURFACE('',#33506,0.0137499999999999);
#4673=CYLINDRICAL_SURFACE('',#33509,0.0137499999999999);
#4674=CYLINDRICAL_SURFACE('',#33512,0.0137499999999999);
#4675=CYLINDRICAL_SURFACE('',#33515,0.0137499999999999);
#4676=CYLINDRICAL_SURFACE('',#33518,0.0137499999999999);
#4677=CYLINDRICAL_SURFACE('',#33521,0.0137499999999999);
#4678=CYLINDRICAL_SURFACE('',#33524,0.0137499999999999);
#4679=CYLINDRICAL_SURFACE('',#33527,0.0137499999999999);
#4680=CYLINDRICAL_SURFACE('',#33530,0.0137499999999999);
#4681=CYLINDRICAL_SURFACE('',#33533,0.0137499999999999);
#4682=CYLINDRICAL_SURFACE('',#33536,0.0137499999999997);
#4683=CYLINDRICAL_SURFACE('',#33539,0.0137499999999997);
#4684=CYLINDRICAL_SURFACE('',#33542,0.0137499999999997);
#4685=CYLINDRICAL_SURFACE('',#33545,0.0137499999999997);
#4686=CYLINDRICAL_SURFACE('',#33548,0.0137499999999997);
#4687=CYLINDRICAL_SURFACE('',#33551,0.0137499999999997);
#4688=CYLINDRICAL_SURFACE('',#33554,0.0137499999999998);
#4689=CYLINDRICAL_SURFACE('',#33557,0.0137499999999998);
#4690=CYLINDRICAL_SURFACE('',#33560,0.0137499999999997);
#4691=CYLINDRICAL_SURFACE('',#33563,0.0137499999999997);
#4692=CYLINDRICAL_SURFACE('',#33578,1.5);
#4693=CYLINDRICAL_SURFACE('',#33581,1.5);
#4694=CYLINDRICAL_SURFACE('',#33582,1.5);
#4695=CYLINDRICAL_SURFACE('',#33583,1.5);
#4696=CYLINDRICAL_SURFACE('',#33584,1.5);
#4697=CYLINDRICAL_SURFACE('',#33585,1.5);
#4698=CYLINDRICAL_SURFACE('',#33586,1.5);
#4699=CYLINDRICAL_SURFACE('',#33587,1.5);
#4700=CYLINDRICAL_SURFACE('',#33588,1.5);
#4701=CYLINDRICAL_SURFACE('',#33589,1.5);
#4702=CYLINDRICAL_SURFACE('',#33590,1.5);
#4703=CYLINDRICAL_SURFACE('',#33591,1.5);
#4704=CYLINDRICAL_SURFACE('',#33592,1.5);
#4705=CYLINDRICAL_SURFACE('',#33593,1.5);
#4706=CYLINDRICAL_SURFACE('',#33594,1.5);
#4707=CYLINDRICAL_SURFACE('',#33595,1.5);
#4708=CYLINDRICAL_SURFACE('',#33596,1.5);
#4709=CYLINDRICAL_SURFACE('',#33597,1.5);
#4710=CYLINDRICAL_SURFACE('',#33598,1.5);
#4711=CYLINDRICAL_SURFACE('',#33599,1.5);
#4712=CYLINDRICAL_SURFACE('',#33600,1.5);
#4713=CYLINDRICAL_SURFACE('',#33601,1.5);
#4714=CYLINDRICAL_SURFACE('',#33602,1.5);
#4715=CYLINDRICAL_SURFACE('',#33603,1.5);
#4716=CYLINDRICAL_SURFACE('',#33604,1.5);
#4717=CYLINDRICAL_SURFACE('',#33605,1.5);
#4718=CYLINDRICAL_SURFACE('',#33606,1.5);
#4719=CYLINDRICAL_SURFACE('',#33607,1.5);
#4720=CYLINDRICAL_SURFACE('',#33610,1.17524047358084);
#4721=CYLINDRICAL_SURFACE('',#33612,1.17524047358084);
#4722=CYLINDRICAL_SURFACE('',#33613,1.17524047358084);
#4723=CYLINDRICAL_SURFACE('',#33614,1.17524047358084);
#4724=CYLINDRICAL_SURFACE('',#33615,1.17524047358084);
#4725=CYLINDRICAL_SURFACE('',#33616,1.17524047358084);
#4726=CYLINDRICAL_SURFACE('',#33617,1.17524047358084);
#4727=CYLINDRICAL_SURFACE('',#33618,1.17524047358084);
#4728=CYLINDRICAL_SURFACE('',#33619,1.17524047358084);
#4729=CYLINDRICAL_SURFACE('',#33620,1.17524047358084);
#4730=CYLINDRICAL_SURFACE('',#33621,1.17524047358084);
#4731=CYLINDRICAL_SURFACE('',#33622,1.17524047358084);
#4732=CYLINDRICAL_SURFACE('',#33623,1.17524047358084);
#4733=CYLINDRICAL_SURFACE('',#33624,1.17524047358084);
#4734=CYLINDRICAL_SURFACE('',#33625,1.17524047358084);
#4735=CYLINDRICAL_SURFACE('',#33626,1.17524047358084);
#4736=CYLINDRICAL_SURFACE('',#33627,1.17524047358084);
#4737=CYLINDRICAL_SURFACE('',#33628,1.17524047358084);
#4738=CYLINDRICAL_SURFACE('',#33629,1.17524047358084);
#4739=CYLINDRICAL_SURFACE('',#33630,1.17524047358084);
#4740=CYLINDRICAL_SURFACE('',#33631,1.17524047358084);
#4741=CYLINDRICAL_SURFACE('',#33632,1.17524047358084);
#4742=CYLINDRICAL_SURFACE('',#33633,1.17524047358084);
#4743=CYLINDRICAL_SURFACE('',#33634,1.17524047358084);
#4744=CYLINDRICAL_SURFACE('',#33635,1.17524047358084);
#4745=CYLINDRICAL_SURFACE('',#33636,1.17524047358084);
#4746=CYLINDRICAL_SURFACE('',#33637,1.17524047358084);
#4747=CYLINDRICAL_SURFACE('',#33638,1.17524047358084);
#4748=CYLINDRICAL_SURFACE('',#33639,1.17524047358084);
#4749=CYLINDRICAL_SURFACE('',#33640,1.17524047358084);
#4750=CYLINDRICAL_SURFACE('',#33641,1.17524047358084);
#4751=CYLINDRICAL_SURFACE('',#33646,1.5);
#4752=CYLINDRICAL_SURFACE('',#33647,0.0137499999999999);
#4753=CYLINDRICAL_SURFACE('',#33650,0.0137499999999999);
#4754=CYLINDRICAL_SURFACE('',#33653,0.0137499999999999);
#4755=CYLINDRICAL_SURFACE('',#33656,0.0137499999999999);
#4756=CYLINDRICAL_SURFACE('',#33659,0.0137499999999999);
#4757=CYLINDRICAL_SURFACE('',#33662,0.0137499999999999);
#4758=CYLINDRICAL_SURFACE('',#33665,0.0137499999999999);
#4759=CYLINDRICAL_SURFACE('',#33668,0.0137499999999999);
#4760=CYLINDRICAL_SURFACE('',#33671,0.0137499999999999);
#4761=CYLINDRICAL_SURFACE('',#33674,0.0137499999999999);
#4762=CYLINDRICAL_SURFACE('',#33677,0.0137499999999997);
#4763=CYLINDRICAL_SURFACE('',#33680,0.0137499999999997);
#4764=CYLINDRICAL_SURFACE('',#33683,0.0137499999999997);
#4765=CYLINDRICAL_SURFACE('',#33686,0.0137499999999997);
#4766=CYLINDRICAL_SURFACE('',#33689,0.0137499999999997);
#4767=CYLINDRICAL_SURFACE('',#33993,2.675);
#4768=CYLINDRICAL_SURFACE('',#34317,2.75);
#4769=CYLINDRICAL_SURFACE('',#34319,2.75);
#4770=CYLINDRICAL_SURFACE('',#34321,2.75);
#4771=CYLINDRICAL_SURFACE('',#34323,2.75);
#4772=CYLINDRICAL_SURFACE('',#34325,2.75);
#4773=CYLINDRICAL_SURFACE('',#34327,2.75);
#4774=CYLINDRICAL_SURFACE('',#34329,2.75);
#4775=CYLINDRICAL_SURFACE('',#34331,2.75);
#4776=CYLINDRICAL_SURFACE('',#34333,2.75);
#4777=CYLINDRICAL_SURFACE('',#34335,2.75);
#4778=CYLINDRICAL_SURFACE('',#34337,2.75);
#4779=CYLINDRICAL_SURFACE('',#34339,2.75);
#4780=CYLINDRICAL_SURFACE('',#34341,2.75);
#4781=CYLINDRICAL_SURFACE('',#34343,2.75);
#4782=CYLINDRICAL_SURFACE('',#34345,2.75);
#4783=CYLINDRICAL_SURFACE('',#34347,2.75);
#4784=CYLINDRICAL_SURFACE('',#34349,2.75);
#4785=CYLINDRICAL_SURFACE('',#34351,2.75);
#4786=CYLINDRICAL_SURFACE('',#34353,2.75);
#4787=CYLINDRICAL_SURFACE('',#34355,2.75);
#4788=CYLINDRICAL_SURFACE('',#34357,2.75);
#4789=CYLINDRICAL_SURFACE('',#34359,2.75);
#4790=CYLINDRICAL_SURFACE('',#34361,2.75);
#4791=CYLINDRICAL_SURFACE('',#34363,2.75);
#4792=CYLINDRICAL_SURFACE('',#34365,2.75);
#4793=CYLINDRICAL_SURFACE('',#34367,2.75);
#4794=CYLINDRICAL_SURFACE('',#34369,2.75);
#4795=CYLINDRICAL_SURFACE('',#34371,2.75);
#4796=CYLINDRICAL_SURFACE('',#34373,2.75);
#4797=CYLINDRICAL_SURFACE('',#34375,2.75);
#4798=CYLINDRICAL_SURFACE('',#34377,2.75);
#4799=CYLINDRICAL_SURFACE('',#34379,2.75);
#4800=CYLINDRICAL_SURFACE('',#34381,2.75);
#4801=CYLINDRICAL_SURFACE('',#34383,2.75);
#4802=CYLINDRICAL_SURFACE('',#34385,2.75);
#4803=CYLINDRICAL_SURFACE('',#34387,2.75);
#4804=CYLINDRICAL_SURFACE('',#34389,2.75);
#4805=CYLINDRICAL_SURFACE('',#34391,2.75);
#4806=CYLINDRICAL_SURFACE('',#34393,2.75);
#4807=CYLINDRICAL_SURFACE('',#34395,2.75);
#4808=CYLINDRICAL_SURFACE('',#34397,2.75);
#4809=CYLINDRICAL_SURFACE('',#34399,2.75);
#4810=CYLINDRICAL_SURFACE('',#34401,2.75);
#4811=CYLINDRICAL_SURFACE('',#34403,2.75);
#4812=CYLINDRICAL_SURFACE('',#34405,2.75);
#4813=CYLINDRICAL_SURFACE('',#34407,2.75);
#4814=CYLINDRICAL_SURFACE('',#34409,2.75);
#4815=CYLINDRICAL_SURFACE('',#34411,2.75);
#4816=CYLINDRICAL_SURFACE('',#34413,2.75);
#4817=CYLINDRICAL_SURFACE('',#34415,2.75);
#4818=CYLINDRICAL_SURFACE('',#34417,2.75);
#4819=CYLINDRICAL_SURFACE('',#34419,2.75);
#4820=CYLINDRICAL_SURFACE('',#34421,2.75);
#4821=CYLINDRICAL_SURFACE('',#34423,2.75);
#4822=CYLINDRICAL_SURFACE('',#34425,2.75);
#4823=CYLINDRICAL_SURFACE('',#34427,2.75);
#4824=CYLINDRICAL_SURFACE('',#34429,2.75);
#4825=CYLINDRICAL_SURFACE('',#34431,2.75);
#4826=CYLINDRICAL_SURFACE('',#34433,2.75);
#4827=CYLINDRICAL_SURFACE('',#34435,2.75);
#4828=CYLINDRICAL_SURFACE('',#34437,2.75);
#4829=CYLINDRICAL_SURFACE('',#34439,2.75);
#4830=CYLINDRICAL_SURFACE('',#34441,2.75);
#4831=CYLINDRICAL_SURFACE('',#34443,2.75);
#4832=CYLINDRICAL_SURFACE('',#34445,2.75);
#4833=CYLINDRICAL_SURFACE('',#34447,2.75);
#4834=CYLINDRICAL_SURFACE('',#34449,2.75);
#4835=CYLINDRICAL_SURFACE('',#34451,2.75);
#4836=CYLINDRICAL_SURFACE('',#34453,2.75);
#4837=CYLINDRICAL_SURFACE('',#34455,2.75);
#4838=CYLINDRICAL_SURFACE('',#34457,2.75);
#4839=CYLINDRICAL_SURFACE('',#34459,2.75);
#4840=CYLINDRICAL_SURFACE('',#34461,2.75);
#4841=CYLINDRICAL_SURFACE('',#34463,2.75);
#4842=CYLINDRICAL_SURFACE('',#34465,2.75);
#4843=CYLINDRICAL_SURFACE('',#34467,2.75);
#4844=CYLINDRICAL_SURFACE('',#34469,2.75);
#4845=CYLINDRICAL_SURFACE('',#34471,2.75);
#4846=CYLINDRICAL_SURFACE('',#34473,2.75);
#4847=CYLINDRICAL_SURFACE('',#34718,2.75);
#4848=CYLINDRICAL_SURFACE('',#34733,0.0137499999999997);
#4849=CYLINDRICAL_SURFACE('',#34736,0.0137499999999997);
#4850=CYLINDRICAL_SURFACE('',#34739,0.0137499999999997);
#4851=CYLINDRICAL_SURFACE('',#34742,0.0137499999999997);
#4852=CYLINDRICAL_SURFACE('',#34745,0.0137499999999998);
#4853=CYLINDRICAL_SURFACE('',#34748,0.0137499999999998);
#4854=CYLINDRICAL_SURFACE('',#34751,0.0137499999999997);
#4855=CYLINDRICAL_SURFACE('',#34772,0.0137499999999997);
#4856=CYLINDRICAL_SURFACE('',#34775,0.0137499999999998);
#4857=CYLINDRICAL_SURFACE('',#34778,0.0137499999999998);
#4858=CYLINDRICAL_SURFACE('',#34781,0.0137499999999997);
#4859=CYLINDRICAL_SURFACE('',#34784,0.0137499999999997);
#4860=CYLINDRICAL_SURFACE('',#34787,0.0137499999999997);
#4861=CYLINDRICAL_SURFACE('',#34790,0.0137499999999997);
#4862=CYLINDRICAL_SURFACE('',#34793,0.0137499999999997);
#4863=CYLINDRICAL_SURFACE('',#34796,0.0137499999999997);
#4864=CYLINDRICAL_SURFACE('',#34799,0.0137499999999999);
#4865=CYLINDRICAL_SURFACE('',#34802,0.0137499999999999);
#4866=CYLINDRICAL_SURFACE('',#34805,0.0137499999999999);
#4867=CYLINDRICAL_SURFACE('',#34808,0.0137499999999999);
#4868=CYLINDRICAL_SURFACE('',#34811,0.0137499999999999);
#4869=CYLINDRICAL_SURFACE('',#34814,0.0137499999999999);
#4870=CYLINDRICAL_SURFACE('',#34817,0.0137499999999999);
#4871=CYLINDRICAL_SURFACE('',#34820,0.0137499999999999);
#4872=CYLINDRICAL_SURFACE('',#34823,0.0137499999999999);
#4873=CYLINDRICAL_SURFACE('',#34826,0.0137499999999997);
#4874=CYLINDRICAL_SURFACE('',#34829,0.0137499999999997);
#4875=CYLINDRICAL_SURFACE('',#34832,0.0137499999999997);
#4876=CYLINDRICAL_SURFACE('',#34835,0.0137499999999998);
#4877=CYLINDRICAL_SURFACE('',#34838,0.0137499999999998);
#4878=CYLINDRICAL_SURFACE('',#34841,0.0137499999999997);
#4879=CYLINDRICAL_SURFACE('',#34844,0.0137499999999997);
#4880=CYLINDRICAL_SURFACE('',#34847,0.0137499999999997);
#4881=CYLINDRICAL_SURFACE('',#34850,0.0137499999999997);
#4882=CYLINDRICAL_SURFACE('',#34853,0.0137499999999997);
#4883=CYLINDRICAL_SURFACE('',#34856,0.0137499999999997);
#4884=CYLINDRICAL_SURFACE('',#34859,0.0137499999999999);
#4885=CYLINDRICAL_SURFACE('',#34862,0.0137499999999999);
#4886=CYLINDRICAL_SURFACE('',#34865,0.0137499999999999);
#4887=CYLINDRICAL_SURFACE('',#34868,0.0137499999999999);
#4888=CYLINDRICAL_SURFACE('',#34871,0.0137499999999999);
#4889=CYLINDRICAL_SURFACE('',#34874,0.0137499999999999);
#4890=CYLINDRICAL_SURFACE('',#34877,0.0137499999999999);
#4891=CYLINDRICAL_SURFACE('',#34880,0.0137499999999999);
#4892=CYLINDRICAL_SURFACE('',#34883,0.0137499999999999);
#4893=CYLINDRICAL_SURFACE('',#34886,0.0137499999999999);
#4894=CYLINDRICAL_SURFACE('',#34889,0.0137499999999999);
#4895=CYLINDRICAL_SURFACE('',#34892,0.0137499999999999);
#4896=CYLINDRICAL_SURFACE('',#34895,0.0137499999999999);
#4897=CYLINDRICAL_SURFACE('',#34898,0.0137499999999999);
#4898=CYLINDRICAL_SURFACE('',#34901,0.0137499999999999);
#4899=CYLINDRICAL_SURFACE('',#34904,0.0137499999999999);
#4900=CYLINDRICAL_SURFACE('',#34907,0.0137499999999999);
#4901=CYLINDRICAL_SURFACE('',#34910,0.0137499999999999);
#4902=CYLINDRICAL_SURFACE('',#34913,0.0137499999999999);
#4903=CYLINDRICAL_SURFACE('',#34916,0.0137499999999997);
#4904=CYLINDRICAL_SURFACE('',#34919,0.0137499999999997);
#4905=CYLINDRICAL_SURFACE('',#34922,0.0137499999999997);
#4906=CYLINDRICAL_SURFACE('',#34925,0.0137499999999997);
#4907=CYLINDRICAL_SURFACE('',#34928,0.0137499999999997);
#4908=CYLINDRICAL_SURFACE('',#34931,0.0137499999999997);
#4909=CYLINDRICAL_SURFACE('',#34934,0.0137499999999998);
#4910=CYLINDRICAL_SURFACE('',#34937,0.0137499999999998);
#4911=CYLINDRICAL_SURFACE('',#34940,0.0137499999999997);
#4912=CYLINDRICAL_SURFACE('',#34943,0.0137499999999997);
#4913=CYLINDRICAL_SURFACE('',#34958,1.5);
#4914=CYLINDRICAL_SURFACE('',#34961,1.5);
#4915=CYLINDRICAL_SURFACE('',#34962,1.5);
#4916=CYLINDRICAL_SURFACE('',#34963,1.5);
#4917=CYLINDRICAL_SURFACE('',#34964,1.5);
#4918=CYLINDRICAL_SURFACE('',#34965,1.5);
#4919=CYLINDRICAL_SURFACE('',#34966,1.5);
#4920=CYLINDRICAL_SURFACE('',#34967,1.5);
#4921=CYLINDRICAL_SURFACE('',#34968,1.5);
#4922=CYLINDRICAL_SURFACE('',#34969,1.5);
#4923=CYLINDRICAL_SURFACE('',#34970,1.5);
#4924=CYLINDRICAL_SURFACE('',#34971,1.5);
#4925=CYLINDRICAL_SURFACE('',#34972,1.5);
#4926=CYLINDRICAL_SURFACE('',#34973,1.5);
#4927=CYLINDRICAL_SURFACE('',#34974,1.5);
#4928=CYLINDRICAL_SURFACE('',#34975,1.5);
#4929=CYLINDRICAL_SURFACE('',#34976,1.5);
#4930=CYLINDRICAL_SURFACE('',#34977,1.5);
#4931=CYLINDRICAL_SURFACE('',#34978,1.5);
#4932=CYLINDRICAL_SURFACE('',#34979,1.5);
#4933=CYLINDRICAL_SURFACE('',#34980,1.5);
#4934=CYLINDRICAL_SURFACE('',#34981,1.5);
#4935=CYLINDRICAL_SURFACE('',#34982,1.5);
#4936=CYLINDRICAL_SURFACE('',#34983,1.5);
#4937=CYLINDRICAL_SURFACE('',#34984,1.5);
#4938=CYLINDRICAL_SURFACE('',#34985,1.5);
#4939=CYLINDRICAL_SURFACE('',#34986,1.5);
#4940=CYLINDRICAL_SURFACE('',#34987,1.5);
#4941=CYLINDRICAL_SURFACE('',#34990,1.17524047358084);
#4942=CYLINDRICAL_SURFACE('',#34992,1.17524047358084);
#4943=CYLINDRICAL_SURFACE('',#34993,1.17524047358084);
#4944=CYLINDRICAL_SURFACE('',#34994,1.17524047358084);
#4945=CYLINDRICAL_SURFACE('',#34995,1.17524047358084);
#4946=CYLINDRICAL_SURFACE('',#34996,1.17524047358084);
#4947=CYLINDRICAL_SURFACE('',#34997,1.17524047358084);
#4948=CYLINDRICAL_SURFACE('',#34998,1.17524047358084);
#4949=CYLINDRICAL_SURFACE('',#34999,1.17524047358084);
#4950=CYLINDRICAL_SURFACE('',#35000,1.17524047358084);
#4951=CYLINDRICAL_SURFACE('',#35001,1.17524047358084);
#4952=CYLINDRICAL_SURFACE('',#35002,1.17524047358084);
#4953=CYLINDRICAL_SURFACE('',#35003,1.17524047358084);
#4954=CYLINDRICAL_SURFACE('',#35004,1.17524047358084);
#4955=CYLINDRICAL_SURFACE('',#35005,1.17524047358084);
#4956=CYLINDRICAL_SURFACE('',#35006,1.17524047358084);
#4957=CYLINDRICAL_SURFACE('',#35007,1.17524047358084);
#4958=CYLINDRICAL_SURFACE('',#35008,1.17524047358084);
#4959=CYLINDRICAL_SURFACE('',#35009,1.17524047358084);
#4960=CYLINDRICAL_SURFACE('',#35010,1.17524047358084);
#4961=CYLINDRICAL_SURFACE('',#35011,1.17524047358084);
#4962=CYLINDRICAL_SURFACE('',#35012,1.17524047358084);
#4963=CYLINDRICAL_SURFACE('',#35013,1.17524047358084);
#4964=CYLINDRICAL_SURFACE('',#35014,1.17524047358084);
#4965=CYLINDRICAL_SURFACE('',#35015,1.17524047358084);
#4966=CYLINDRICAL_SURFACE('',#35016,1.17524047358084);
#4967=CYLINDRICAL_SURFACE('',#35017,1.17524047358084);
#4968=CYLINDRICAL_SURFACE('',#35018,1.17524047358084);
#4969=CYLINDRICAL_SURFACE('',#35019,1.17524047358084);
#4970=CYLINDRICAL_SURFACE('',#35020,1.17524047358084);
#4971=CYLINDRICAL_SURFACE('',#35021,1.17524047358084);
#4972=CYLINDRICAL_SURFACE('',#35026,1.5);
#4973=CYLINDRICAL_SURFACE('',#35027,0.0137499999999999);
#4974=CYLINDRICAL_SURFACE('',#35030,0.0137499999999999);
#4975=CYLINDRICAL_SURFACE('',#35033,0.0137499999999999);
#4976=CYLINDRICAL_SURFACE('',#35036,0.0137499999999999);
#4977=CYLINDRICAL_SURFACE('',#35039,0.0137499999999999);
#4978=CYLINDRICAL_SURFACE('',#35042,0.0137499999999999);
#4979=CYLINDRICAL_SURFACE('',#35045,0.0137499999999999);
#4980=CYLINDRICAL_SURFACE('',#35048,0.0137499999999999);
#4981=CYLINDRICAL_SURFACE('',#35051,0.0137499999999999);
#4982=CYLINDRICAL_SURFACE('',#35054,0.0137499999999999);
#4983=CYLINDRICAL_SURFACE('',#35057,0.0137499999999997);
#4984=CYLINDRICAL_SURFACE('',#35060,0.0137499999999997);
#4985=CYLINDRICAL_SURFACE('',#35063,0.0137499999999997);
#4986=CYLINDRICAL_SURFACE('',#35066,0.0137499999999997);
#4987=CYLINDRICAL_SURFACE('',#35069,0.0137499999999997);
#4988=CYLINDRICAL_SURFACE('',#35373,2.675);
#4989=CYLINDRICAL_SURFACE('',#35697,2.75);
#4990=CYLINDRICAL_SURFACE('',#35699,2.75);
#4991=CYLINDRICAL_SURFACE('',#35701,2.75);
#4992=CYLINDRICAL_SURFACE('',#35703,2.75);
#4993=CYLINDRICAL_SURFACE('',#35705,2.75);
#4994=CYLINDRICAL_SURFACE('',#35707,2.75);
#4995=CYLINDRICAL_SURFACE('',#35709,2.75);
#4996=CYLINDRICAL_SURFACE('',#35711,2.75);
#4997=CYLINDRICAL_SURFACE('',#35713,2.75);
#4998=CYLINDRICAL_SURFACE('',#35715,2.75);
#4999=CYLINDRICAL_SURFACE('',#35717,2.75);
#5000=CYLINDRICAL_SURFACE('',#35719,2.75);
#5001=CYLINDRICAL_SURFACE('',#35721,2.75);
#5002=CYLINDRICAL_SURFACE('',#35723,2.75);
#5003=CYLINDRICAL_SURFACE('',#35725,2.75);
#5004=CYLINDRICAL_SURFACE('',#35727,2.75);
#5005=CYLINDRICAL_SURFACE('',#35729,2.75);
#5006=CYLINDRICAL_SURFACE('',#35731,2.75);
#5007=CYLINDRICAL_SURFACE('',#35733,2.75);
#5008=CYLINDRICAL_SURFACE('',#35735,2.75);
#5009=CYLINDRICAL_SURFACE('',#35737,2.75);
#5010=CYLINDRICAL_SURFACE('',#35739,2.75);
#5011=CYLINDRICAL_SURFACE('',#35741,2.75);
#5012=CYLINDRICAL_SURFACE('',#35743,2.75);
#5013=CYLINDRICAL_SURFACE('',#35745,2.75);
#5014=CYLINDRICAL_SURFACE('',#35747,2.75);
#5015=CYLINDRICAL_SURFACE('',#35749,2.75);
#5016=CYLINDRICAL_SURFACE('',#35751,2.75);
#5017=CYLINDRICAL_SURFACE('',#35753,2.75);
#5018=CYLINDRICAL_SURFACE('',#35755,2.75);
#5019=CYLINDRICAL_SURFACE('',#35757,2.75);
#5020=CYLINDRICAL_SURFACE('',#35759,2.75);
#5021=CYLINDRICAL_SURFACE('',#35761,2.75);
#5022=CYLINDRICAL_SURFACE('',#35763,2.75);
#5023=CYLINDRICAL_SURFACE('',#35765,2.75);
#5024=CYLINDRICAL_SURFACE('',#35767,2.75);
#5025=CYLINDRICAL_SURFACE('',#35769,2.75);
#5026=CYLINDRICAL_SURFACE('',#35771,2.75);
#5027=CYLINDRICAL_SURFACE('',#35773,2.75);
#5028=CYLINDRICAL_SURFACE('',#35775,2.75);
#5029=CYLINDRICAL_SURFACE('',#35777,2.75);
#5030=CYLINDRICAL_SURFACE('',#35779,2.75);
#5031=CYLINDRICAL_SURFACE('',#35781,2.75);
#5032=CYLINDRICAL_SURFACE('',#35783,2.75);
#5033=CYLINDRICAL_SURFACE('',#35785,2.75);
#5034=CYLINDRICAL_SURFACE('',#35787,2.75);
#5035=CYLINDRICAL_SURFACE('',#35789,2.75);
#5036=CYLINDRICAL_SURFACE('',#35791,2.75);
#5037=CYLINDRICAL_SURFACE('',#35793,2.75);
#5038=CYLINDRICAL_SURFACE('',#35795,2.75);
#5039=CYLINDRICAL_SURFACE('',#35797,2.75);
#5040=CYLINDRICAL_SURFACE('',#35799,2.75);
#5041=CYLINDRICAL_SURFACE('',#35801,2.75);
#5042=CYLINDRICAL_SURFACE('',#35803,2.75);
#5043=CYLINDRICAL_SURFACE('',#35805,2.75);
#5044=CYLINDRICAL_SURFACE('',#35807,2.75);
#5045=CYLINDRICAL_SURFACE('',#35809,2.75);
#5046=CYLINDRICAL_SURFACE('',#35811,2.75);
#5047=CYLINDRICAL_SURFACE('',#35813,2.75);
#5048=CYLINDRICAL_SURFACE('',#35815,2.75);
#5049=CYLINDRICAL_SURFACE('',#35817,2.75);
#5050=CYLINDRICAL_SURFACE('',#35819,2.75);
#5051=CYLINDRICAL_SURFACE('',#35821,2.75);
#5052=CYLINDRICAL_SURFACE('',#35823,2.75);
#5053=CYLINDRICAL_SURFACE('',#35825,2.75);
#5054=CYLINDRICAL_SURFACE('',#35827,2.75);
#5055=CYLINDRICAL_SURFACE('',#35829,2.75);
#5056=CYLINDRICAL_SURFACE('',#35831,2.75);
#5057=CYLINDRICAL_SURFACE('',#35833,2.75);
#5058=CYLINDRICAL_SURFACE('',#35835,2.75);
#5059=CYLINDRICAL_SURFACE('',#35837,2.75);
#5060=CYLINDRICAL_SURFACE('',#35839,2.75);
#5061=CYLINDRICAL_SURFACE('',#35841,2.75);
#5062=CYLINDRICAL_SURFACE('',#35843,2.75);
#5063=CYLINDRICAL_SURFACE('',#35845,2.75);
#5064=CYLINDRICAL_SURFACE('',#35847,2.75);
#5065=CYLINDRICAL_SURFACE('',#35849,2.75);
#5066=CYLINDRICAL_SURFACE('',#35851,2.75);
#5067=CYLINDRICAL_SURFACE('',#35853,2.75);
#5068=CYLINDRICAL_SURFACE('',#36098,2.75);
#5069=CYLINDRICAL_SURFACE('',#36113,0.0137499999999997);
#5070=CYLINDRICAL_SURFACE('',#36116,0.0137499999999997);
#5071=CYLINDRICAL_SURFACE('',#36119,0.0137499999999997);
#5072=CYLINDRICAL_SURFACE('',#36122,0.0137499999999997);
#5073=CYLINDRICAL_SURFACE('',#36125,0.0137499999999998);
#5074=CYLINDRICAL_SURFACE('',#36128,0.0137499999999998);
#5075=CYLINDRICAL_SURFACE('',#36131,0.0137499999999997);
#5076=CYLINDRICAL_SURFACE('',#36152,0.0137499999999997);
#5077=CYLINDRICAL_SURFACE('',#36155,0.0137499999999998);
#5078=CYLINDRICAL_SURFACE('',#36158,0.0137499999999998);
#5079=CYLINDRICAL_SURFACE('',#36161,0.0137499999999997);
#5080=CYLINDRICAL_SURFACE('',#36164,0.0137499999999997);
#5081=CYLINDRICAL_SURFACE('',#36167,0.0137499999999997);
#5082=CYLINDRICAL_SURFACE('',#36170,0.0137499999999997);
#5083=CYLINDRICAL_SURFACE('',#36173,0.0137499999999997);
#5084=CYLINDRICAL_SURFACE('',#36176,0.0137499999999997);
#5085=CYLINDRICAL_SURFACE('',#36179,0.0137499999999999);
#5086=CYLINDRICAL_SURFACE('',#36182,0.0137499999999999);
#5087=CYLINDRICAL_SURFACE('',#36185,0.0137499999999999);
#5088=CYLINDRICAL_SURFACE('',#36188,0.0137499999999999);
#5089=CYLINDRICAL_SURFACE('',#36191,0.0137499999999999);
#5090=CYLINDRICAL_SURFACE('',#36194,0.0137499999999999);
#5091=CYLINDRICAL_SURFACE('',#36197,0.0137499999999999);
#5092=CYLINDRICAL_SURFACE('',#36200,0.0137499999999999);
#5093=CYLINDRICAL_SURFACE('',#36203,0.0137499999999999);
#5094=CYLINDRICAL_SURFACE('',#36206,0.0137499999999997);
#5095=CYLINDRICAL_SURFACE('',#36209,0.0137499999999997);
#5096=CYLINDRICAL_SURFACE('',#36212,0.0137499999999997);
#5097=CYLINDRICAL_SURFACE('',#36215,0.0137499999999998);
#5098=CYLINDRICAL_SURFACE('',#36218,0.0137499999999998);
#5099=CYLINDRICAL_SURFACE('',#36221,0.0137499999999997);
#5100=CYLINDRICAL_SURFACE('',#36224,0.0137499999999997);
#5101=CYLINDRICAL_SURFACE('',#36227,0.0137499999999997);
#5102=CYLINDRICAL_SURFACE('',#36230,0.0137499999999997);
#5103=CYLINDRICAL_SURFACE('',#36233,0.0137499999999997);
#5104=CYLINDRICAL_SURFACE('',#36236,0.0137499999999997);
#5105=CYLINDRICAL_SURFACE('',#36239,0.0137499999999999);
#5106=CYLINDRICAL_SURFACE('',#36242,0.0137499999999999);
#5107=CYLINDRICAL_SURFACE('',#36245,0.0137499999999999);
#5108=CYLINDRICAL_SURFACE('',#36248,0.0137499999999999);
#5109=CYLINDRICAL_SURFACE('',#36251,0.0137499999999999);
#5110=CYLINDRICAL_SURFACE('',#36254,0.0137499999999999);
#5111=CYLINDRICAL_SURFACE('',#36257,0.0137499999999999);
#5112=CYLINDRICAL_SURFACE('',#36260,0.0137499999999999);
#5113=CYLINDRICAL_SURFACE('',#36263,0.0137499999999999);
#5114=CYLINDRICAL_SURFACE('',#36266,0.0137499999999999);
#5115=CYLINDRICAL_SURFACE('',#36269,0.0137499999999999);
#5116=CYLINDRICAL_SURFACE('',#36272,0.0137499999999999);
#5117=CYLINDRICAL_SURFACE('',#36275,0.0137499999999999);
#5118=CYLINDRICAL_SURFACE('',#36278,0.0137499999999999);
#5119=CYLINDRICAL_SURFACE('',#36281,0.0137499999999999);
#5120=CYLINDRICAL_SURFACE('',#36284,0.0137499999999999);
#5121=CYLINDRICAL_SURFACE('',#36287,0.0137499999999999);
#5122=CYLINDRICAL_SURFACE('',#36290,0.0137499999999999);
#5123=CYLINDRICAL_SURFACE('',#36293,0.0137499999999999);
#5124=CYLINDRICAL_SURFACE('',#36296,0.0137499999999997);
#5125=CYLINDRICAL_SURFACE('',#36299,0.0137499999999997);
#5126=CYLINDRICAL_SURFACE('',#36302,0.0137499999999997);
#5127=CYLINDRICAL_SURFACE('',#36305,0.0137499999999997);
#5128=CYLINDRICAL_SURFACE('',#36308,0.0137499999999997);
#5129=CYLINDRICAL_SURFACE('',#36311,0.0137499999999997);
#5130=CYLINDRICAL_SURFACE('',#36314,0.0137499999999998);
#5131=CYLINDRICAL_SURFACE('',#36317,0.0137499999999998);
#5132=CYLINDRICAL_SURFACE('',#36320,0.0137499999999997);
#5133=CYLINDRICAL_SURFACE('',#36323,0.0137499999999997);
#5134=FACE_OUTER_BOUND('',#6861,.T.);
#5135=FACE_OUTER_BOUND('',#6862,.T.);
#5136=FACE_OUTER_BOUND('',#6863,.T.);
#5137=FACE_OUTER_BOUND('',#6864,.T.);
#5138=FACE_OUTER_BOUND('',#6865,.T.);
#5139=FACE_OUTER_BOUND('',#6866,.T.);
#5140=FACE_OUTER_BOUND('',#6867,.T.);
#5141=FACE_OUTER_BOUND('',#6868,.T.);
#5142=FACE_OUTER_BOUND('',#6869,.T.);
#5143=FACE_OUTER_BOUND('',#6870,.T.);
#5144=FACE_OUTER_BOUND('',#6871,.T.);
#5145=FACE_OUTER_BOUND('',#6873,.T.);
#5146=FACE_OUTER_BOUND('',#6874,.T.);
#5147=FACE_OUTER_BOUND('',#6875,.T.);
#5148=FACE_OUTER_BOUND('',#6876,.T.);
#5149=FACE_OUTER_BOUND('',#6877,.T.);
#5150=FACE_OUTER_BOUND('',#6878,.T.);
#5151=FACE_OUTER_BOUND('',#6879,.T.);
#5152=FACE_OUTER_BOUND('',#6880,.T.);
#5153=FACE_OUTER_BOUND('',#6881,.T.);
#5154=FACE_OUTER_BOUND('',#6882,.T.);
#5155=FACE_OUTER_BOUND('',#6883,.T.);
#5156=FACE_OUTER_BOUND('',#6884,.T.);
#5157=FACE_OUTER_BOUND('',#6885,.T.);
#5158=FACE_OUTER_BOUND('',#6886,.T.);
#5159=FACE_OUTER_BOUND('',#6887,.T.);
#5160=FACE_OUTER_BOUND('',#6888,.T.);
#5161=FACE_OUTER_BOUND('',#6892,.T.);
#5162=FACE_OUTER_BOUND('',#6893,.T.);
#5163=FACE_OUTER_BOUND('',#6894,.T.);
#5164=FACE_OUTER_BOUND('',#6895,.T.);
#5165=FACE_OUTER_BOUND('',#6896,.T.);
#5166=FACE_OUTER_BOUND('',#6897,.T.);
#5167=FACE_OUTER_BOUND('',#6898,.T.);
#5168=FACE_OUTER_BOUND('',#6899,.T.);
#5169=FACE_OUTER_BOUND('',#6900,.T.);
#5170=FACE_OUTER_BOUND('',#6901,.T.);
#5171=FACE_OUTER_BOUND('',#6902,.T.);
#5172=FACE_OUTER_BOUND('',#6906,.T.);
#5173=FACE_OUTER_BOUND('',#6907,.T.);
#5174=FACE_OUTER_BOUND('',#6908,.T.);
#5175=FACE_OUTER_BOUND('',#6909,.T.);
#5176=FACE_OUTER_BOUND('',#6910,.T.);
#5177=FACE_OUTER_BOUND('',#6911,.T.);
#5178=FACE_OUTER_BOUND('',#6912,.T.);
#5179=FACE_OUTER_BOUND('',#6913,.T.);
#5180=FACE_OUTER_BOUND('',#6914,.T.);
#5181=FACE_OUTER_BOUND('',#6915,.T.);
#5182=FACE_OUTER_BOUND('',#6916,.T.);
#5183=FACE_OUTER_BOUND('',#6917,.T.);
#5184=FACE_OUTER_BOUND('',#6918,.T.);
#5185=FACE_OUTER_BOUND('',#6919,.T.);
#5186=FACE_OUTER_BOUND('',#6920,.T.);
#5187=FACE_OUTER_BOUND('',#6921,.T.);
#5188=FACE_OUTER_BOUND('',#6922,.T.);
#5189=FACE_OUTER_BOUND('',#6923,.T.);
#5190=FACE_OUTER_BOUND('',#6924,.T.);
#5191=FACE_OUTER_BOUND('',#6925,.T.);
#5192=FACE_OUTER_BOUND('',#6926,.T.);
#5193=FACE_OUTER_BOUND('',#6927,.T.);
#5194=FACE_OUTER_BOUND('',#6928,.T.);
#5195=FACE_OUTER_BOUND('',#6929,.T.);
#5196=FACE_OUTER_BOUND('',#6930,.T.);
#5197=FACE_OUTER_BOUND('',#6931,.T.);
#5198=FACE_OUTER_BOUND('',#6932,.T.);
#5199=FACE_OUTER_BOUND('',#6933,.T.);
#5200=FACE_OUTER_BOUND('',#6934,.T.);
#5201=FACE_OUTER_BOUND('',#6935,.T.);
#5202=FACE_OUTER_BOUND('',#6936,.T.);
#5203=FACE_OUTER_BOUND('',#6937,.T.);
#5204=FACE_OUTER_BOUND('',#6938,.T.);
#5205=FACE_OUTER_BOUND('',#6939,.T.);
#5206=FACE_OUTER_BOUND('',#6940,.T.);
#5207=FACE_OUTER_BOUND('',#6941,.T.);
#5208=FACE_OUTER_BOUND('',#6942,.T.);
#5209=FACE_OUTER_BOUND('',#6943,.T.);
#5210=FACE_OUTER_BOUND('',#6944,.T.);
#5211=FACE_OUTER_BOUND('',#6945,.T.);
#5212=FACE_OUTER_BOUND('',#6946,.T.);
#5213=FACE_OUTER_BOUND('',#6947,.T.);
#5214=FACE_OUTER_BOUND('',#6948,.T.);
#5215=FACE_OUTER_BOUND('',#6949,.T.);
#5216=FACE_OUTER_BOUND('',#6950,.T.);
#5217=FACE_OUTER_BOUND('',#6951,.T.);
#5218=FACE_OUTER_BOUND('',#6952,.T.);
#5219=FACE_OUTER_BOUND('',#6953,.T.);
#5220=FACE_OUTER_BOUND('',#6954,.T.);
#5221=FACE_OUTER_BOUND('',#6955,.T.);
#5222=FACE_OUTER_BOUND('',#6956,.T.);
#5223=FACE_OUTER_BOUND('',#6957,.T.);
#5224=FACE_OUTER_BOUND('',#6958,.T.);
#5225=FACE_OUTER_BOUND('',#6959,.T.);
#5226=FACE_OUTER_BOUND('',#6960,.T.);
#5227=FACE_OUTER_BOUND('',#6961,.T.);
#5228=FACE_OUTER_BOUND('',#6962,.T.);
#5229=FACE_OUTER_BOUND('',#6963,.T.);
#5230=FACE_OUTER_BOUND('',#6964,.T.);
#5231=FACE_OUTER_BOUND('',#6965,.T.);
#5232=FACE_OUTER_BOUND('',#6966,.T.);
#5233=FACE_OUTER_BOUND('',#6967,.T.);
#5234=FACE_OUTER_BOUND('',#6968,.T.);
#5235=FACE_OUTER_BOUND('',#6969,.T.);
#5236=FACE_OUTER_BOUND('',#6970,.T.);
#5237=FACE_OUTER_BOUND('',#6971,.T.);
#5238=FACE_OUTER_BOUND('',#6972,.T.);
#5239=FACE_OUTER_BOUND('',#6973,.T.);
#5240=FACE_OUTER_BOUND('',#6974,.T.);
#5241=FACE_OUTER_BOUND('',#6975,.T.);
#5242=FACE_OUTER_BOUND('',#6976,.T.);
#5243=FACE_OUTER_BOUND('',#6977,.T.);
#5244=FACE_OUTER_BOUND('',#6978,.T.);
#5245=FACE_OUTER_BOUND('',#6979,.T.);
#5246=FACE_OUTER_BOUND('',#6980,.T.);
#5247=FACE_OUTER_BOUND('',#6981,.T.);
#5248=FACE_OUTER_BOUND('',#6982,.T.);
#5249=FACE_OUTER_BOUND('',#6983,.T.);
#5250=FACE_OUTER_BOUND('',#6984,.T.);
#5251=FACE_OUTER_BOUND('',#6985,.T.);
#5252=FACE_OUTER_BOUND('',#6986,.T.);
#5253=FACE_OUTER_BOUND('',#6987,.T.);
#5254=FACE_OUTER_BOUND('',#6988,.T.);
#5255=FACE_OUTER_BOUND('',#6989,.T.);
#5256=FACE_OUTER_BOUND('',#6990,.T.);
#5257=FACE_OUTER_BOUND('',#6991,.T.);
#5258=FACE_OUTER_BOUND('',#6992,.T.);
#5259=FACE_OUTER_BOUND('',#6993,.T.);
#5260=FACE_OUTER_BOUND('',#6994,.T.);
#5261=FACE_OUTER_BOUND('',#6995,.T.);
#5262=FACE_OUTER_BOUND('',#6996,.T.);
#5263=FACE_OUTER_BOUND('',#6997,.T.);
#5264=FACE_OUTER_BOUND('',#6998,.T.);
#5265=FACE_OUTER_BOUND('',#6999,.T.);
#5266=FACE_OUTER_BOUND('',#7000,.T.);
#5267=FACE_OUTER_BOUND('',#7001,.T.);
#5268=FACE_OUTER_BOUND('',#7002,.T.);
#5269=FACE_OUTER_BOUND('',#7003,.T.);
#5270=FACE_OUTER_BOUND('',#7004,.T.);
#5271=FACE_OUTER_BOUND('',#7005,.T.);
#5272=FACE_OUTER_BOUND('',#7006,.T.);
#5273=FACE_OUTER_BOUND('',#7007,.T.);
#5274=FACE_OUTER_BOUND('',#7008,.T.);
#5275=FACE_OUTER_BOUND('',#7009,.T.);
#5276=FACE_OUTER_BOUND('',#7010,.T.);
#5277=FACE_OUTER_BOUND('',#7011,.T.);
#5278=FACE_OUTER_BOUND('',#7012,.T.);
#5279=FACE_OUTER_BOUND('',#7013,.T.);
#5280=FACE_OUTER_BOUND('',#7014,.T.);
#5281=FACE_OUTER_BOUND('',#7015,.T.);
#5282=FACE_OUTER_BOUND('',#7016,.T.);
#5283=FACE_OUTER_BOUND('',#7017,.T.);
#5284=FACE_OUTER_BOUND('',#7018,.T.);
#5285=FACE_OUTER_BOUND('',#7019,.T.);
#5286=FACE_OUTER_BOUND('',#7020,.T.);
#5287=FACE_OUTER_BOUND('',#7021,.T.);
#5288=FACE_OUTER_BOUND('',#7022,.T.);
#5289=FACE_OUTER_BOUND('',#7023,.T.);
#5290=FACE_OUTER_BOUND('',#7024,.T.);
#5291=FACE_OUTER_BOUND('',#7025,.T.);
#5292=FACE_OUTER_BOUND('',#7026,.T.);
#5293=FACE_OUTER_BOUND('',#7027,.T.);
#5294=FACE_OUTER_BOUND('',#7028,.T.);
#5295=FACE_OUTER_BOUND('',#7029,.T.);
#5296=FACE_OUTER_BOUND('',#7030,.T.);
#5297=FACE_OUTER_BOUND('',#7031,.T.);
#5298=FACE_OUTER_BOUND('',#7032,.T.);
#5299=FACE_OUTER_BOUND('',#7033,.T.);
#5300=FACE_OUTER_BOUND('',#7034,.T.);
#5301=FACE_OUTER_BOUND('',#7035,.T.);
#5302=FACE_OUTER_BOUND('',#7036,.T.);
#5303=FACE_OUTER_BOUND('',#7037,.T.);
#5304=FACE_OUTER_BOUND('',#7038,.T.);
#5305=FACE_OUTER_BOUND('',#7039,.T.);
#5306=FACE_OUTER_BOUND('',#7040,.T.);
#5307=FACE_OUTER_BOUND('',#7041,.T.);
#5308=FACE_OUTER_BOUND('',#7042,.T.);
#5309=FACE_OUTER_BOUND('',#7043,.T.);
#5310=FACE_OUTER_BOUND('',#7044,.T.);
#5311=FACE_OUTER_BOUND('',#7045,.T.);
#5312=FACE_OUTER_BOUND('',#7046,.T.);
#5313=FACE_OUTER_BOUND('',#7047,.T.);
#5314=FACE_OUTER_BOUND('',#7048,.T.);
#5315=FACE_OUTER_BOUND('',#7049,.T.);
#5316=FACE_OUTER_BOUND('',#7050,.T.);
#5317=FACE_OUTER_BOUND('',#7051,.T.);
#5318=FACE_OUTER_BOUND('',#7052,.T.);
#5319=FACE_OUTER_BOUND('',#7053,.T.);
#5320=FACE_OUTER_BOUND('',#7054,.T.);
#5321=FACE_OUTER_BOUND('',#7055,.T.);
#5322=FACE_OUTER_BOUND('',#7056,.T.);
#5323=FACE_OUTER_BOUND('',#7057,.T.);
#5324=FACE_OUTER_BOUND('',#7058,.T.);
#5325=FACE_OUTER_BOUND('',#7059,.T.);
#5326=FACE_OUTER_BOUND('',#7060,.T.);
#5327=FACE_OUTER_BOUND('',#7061,.T.);
#5328=FACE_OUTER_BOUND('',#7062,.T.);
#5329=FACE_OUTER_BOUND('',#7063,.T.);
#5330=FACE_OUTER_BOUND('',#7064,.T.);
#5331=FACE_OUTER_BOUND('',#7065,.T.);
#5332=FACE_OUTER_BOUND('',#7066,.T.);
#5333=FACE_OUTER_BOUND('',#7067,.T.);
#5334=FACE_OUTER_BOUND('',#7068,.T.);
#5335=FACE_OUTER_BOUND('',#7069,.T.);
#5336=FACE_OUTER_BOUND('',#7070,.T.);
#5337=FACE_OUTER_BOUND('',#7071,.T.);
#5338=FACE_OUTER_BOUND('',#7072,.T.);
#5339=FACE_OUTER_BOUND('',#7073,.T.);
#5340=FACE_OUTER_BOUND('',#7074,.T.);
#5341=FACE_OUTER_BOUND('',#7075,.T.);
#5342=FACE_OUTER_BOUND('',#7076,.T.);
#5343=FACE_OUTER_BOUND('',#7077,.T.);
#5344=FACE_OUTER_BOUND('',#7078,.T.);
#5345=FACE_OUTER_BOUND('',#7079,.T.);
#5346=FACE_OUTER_BOUND('',#7080,.T.);
#5347=FACE_OUTER_BOUND('',#7081,.T.);
#5348=FACE_OUTER_BOUND('',#7082,.T.);
#5349=FACE_OUTER_BOUND('',#7083,.T.);
#5350=FACE_OUTER_BOUND('',#7084,.T.);
#5351=FACE_OUTER_BOUND('',#7085,.T.);
#5352=FACE_OUTER_BOUND('',#7086,.T.);
#5353=FACE_OUTER_BOUND('',#7087,.T.);
#5354=FACE_OUTER_BOUND('',#7088,.T.);
#5355=FACE_OUTER_BOUND('',#7089,.T.);
#5356=FACE_OUTER_BOUND('',#7090,.T.);
#5357=FACE_OUTER_BOUND('',#7091,.T.);
#5358=FACE_OUTER_BOUND('',#7092,.T.);
#5359=FACE_OUTER_BOUND('',#7093,.T.);
#5360=FACE_OUTER_BOUND('',#7094,.T.);
#5361=FACE_OUTER_BOUND('',#7095,.T.);
#5362=FACE_OUTER_BOUND('',#7096,.T.);
#5363=FACE_OUTER_BOUND('',#7097,.T.);
#5364=FACE_OUTER_BOUND('',#7098,.T.);
#5365=FACE_OUTER_BOUND('',#7099,.T.);
#5366=FACE_OUTER_BOUND('',#7100,.T.);
#5367=FACE_OUTER_BOUND('',#7101,.T.);
#5368=FACE_OUTER_BOUND('',#7102,.T.);
#5369=FACE_OUTER_BOUND('',#7103,.T.);
#5370=FACE_OUTER_BOUND('',#7104,.T.);
#5371=FACE_OUTER_BOUND('',#7105,.T.);
#5372=FACE_OUTER_BOUND('',#7106,.T.);
#5373=FACE_OUTER_BOUND('',#7107,.T.);
#5374=FACE_OUTER_BOUND('',#7108,.T.);
#5375=FACE_OUTER_BOUND('',#7109,.T.);
#5376=FACE_OUTER_BOUND('',#7110,.T.);
#5377=FACE_OUTER_BOUND('',#7111,.T.);
#5378=FACE_OUTER_BOUND('',#7112,.T.);
#5379=FACE_OUTER_BOUND('',#7113,.T.);
#5380=FACE_OUTER_BOUND('',#7114,.T.);
#5381=FACE_OUTER_BOUND('',#7115,.T.);
#5382=FACE_OUTER_BOUND('',#7116,.T.);
#5383=FACE_OUTER_BOUND('',#7117,.T.);
#5384=FACE_OUTER_BOUND('',#7118,.T.);
#5385=FACE_OUTER_BOUND('',#7119,.T.);
#5386=FACE_OUTER_BOUND('',#7120,.T.);
#5387=FACE_OUTER_BOUND('',#7121,.T.);
#5388=FACE_OUTER_BOUND('',#7122,.T.);
#5389=FACE_OUTER_BOUND('',#7123,.T.);
#5390=FACE_OUTER_BOUND('',#7124,.T.);
#5391=FACE_OUTER_BOUND('',#7125,.T.);
#5392=FACE_OUTER_BOUND('',#7126,.T.);
#5393=FACE_OUTER_BOUND('',#7127,.T.);
#5394=FACE_OUTER_BOUND('',#7128,.T.);
#5395=FACE_OUTER_BOUND('',#7129,.T.);
#5396=FACE_OUTER_BOUND('',#7130,.T.);
#5397=FACE_OUTER_BOUND('',#7131,.T.);
#5398=FACE_OUTER_BOUND('',#7132,.T.);
#5399=FACE_OUTER_BOUND('',#7133,.T.);
#5400=FACE_OUTER_BOUND('',#7134,.T.);
#5401=FACE_OUTER_BOUND('',#7135,.T.);
#5402=FACE_OUTER_BOUND('',#7136,.T.);
#5403=FACE_OUTER_BOUND('',#7137,.T.);
#5404=FACE_OUTER_BOUND('',#7138,.T.);
#5405=FACE_OUTER_BOUND('',#7139,.T.);
#5406=FACE_OUTER_BOUND('',#7140,.T.);
#5407=FACE_OUTER_BOUND('',#7141,.T.);
#5408=FACE_OUTER_BOUND('',#7142,.T.);
#5409=FACE_OUTER_BOUND('',#7143,.T.);
#5410=FACE_OUTER_BOUND('',#7144,.T.);
#5411=FACE_OUTER_BOUND('',#7145,.T.);
#5412=FACE_OUTER_BOUND('',#7146,.T.);
#5413=FACE_OUTER_BOUND('',#7147,.T.);
#5414=FACE_OUTER_BOUND('',#7148,.T.);
#5415=FACE_OUTER_BOUND('',#7149,.T.);
#5416=FACE_OUTER_BOUND('',#7150,.T.);
#5417=FACE_OUTER_BOUND('',#7151,.T.);
#5418=FACE_OUTER_BOUND('',#7152,.T.);
#5419=FACE_OUTER_BOUND('',#7153,.T.);
#5420=FACE_OUTER_BOUND('',#7154,.T.);
#5421=FACE_OUTER_BOUND('',#7155,.T.);
#5422=FACE_OUTER_BOUND('',#7156,.T.);
#5423=FACE_OUTER_BOUND('',#7157,.T.);
#5424=FACE_OUTER_BOUND('',#7158,.T.);
#5425=FACE_OUTER_BOUND('',#7159,.T.);
#5426=FACE_OUTER_BOUND('',#7160,.T.);
#5427=FACE_OUTER_BOUND('',#7161,.T.);
#5428=FACE_OUTER_BOUND('',#7162,.T.);
#5429=FACE_OUTER_BOUND('',#7163,.T.);
#5430=FACE_OUTER_BOUND('',#7164,.T.);
#5431=FACE_OUTER_BOUND('',#7165,.T.);
#5432=FACE_OUTER_BOUND('',#7166,.T.);
#5433=FACE_OUTER_BOUND('',#7167,.T.);
#5434=FACE_OUTER_BOUND('',#7168,.T.);
#5435=FACE_OUTER_BOUND('',#7169,.T.);
#5436=FACE_OUTER_BOUND('',#7170,.T.);
#5437=FACE_OUTER_BOUND('',#7171,.T.);
#5438=FACE_OUTER_BOUND('',#7172,.T.);
#5439=FACE_OUTER_BOUND('',#7173,.T.);
#5440=FACE_OUTER_BOUND('',#7174,.T.);
#5441=FACE_OUTER_BOUND('',#7175,.T.);
#5442=FACE_OUTER_BOUND('',#7176,.T.);
#5443=FACE_OUTER_BOUND('',#7177,.T.);
#5444=FACE_OUTER_BOUND('',#7178,.T.);
#5445=FACE_OUTER_BOUND('',#7179,.T.);
#5446=FACE_OUTER_BOUND('',#7180,.T.);
#5447=FACE_OUTER_BOUND('',#7181,.T.);
#5448=FACE_OUTER_BOUND('',#7182,.T.);
#5449=FACE_OUTER_BOUND('',#7183,.T.);
#5450=FACE_OUTER_BOUND('',#7184,.T.);
#5451=FACE_OUTER_BOUND('',#7185,.T.);
#5452=FACE_OUTER_BOUND('',#7186,.T.);
#5453=FACE_OUTER_BOUND('',#7187,.T.);
#5454=FACE_OUTER_BOUND('',#7188,.T.);
#5455=FACE_OUTER_BOUND('',#7189,.T.);
#5456=FACE_OUTER_BOUND('',#7190,.T.);
#5457=FACE_OUTER_BOUND('',#7191,.T.);
#5458=FACE_OUTER_BOUND('',#7192,.T.);
#5459=FACE_OUTER_BOUND('',#7193,.T.);
#5460=FACE_OUTER_BOUND('',#7194,.T.);
#5461=FACE_OUTER_BOUND('',#7195,.T.);
#5462=FACE_OUTER_BOUND('',#7196,.T.);
#5463=FACE_OUTER_BOUND('',#7197,.T.);
#5464=FACE_OUTER_BOUND('',#7198,.T.);
#5465=FACE_OUTER_BOUND('',#7199,.T.);
#5466=FACE_OUTER_BOUND('',#7200,.T.);
#5467=FACE_OUTER_BOUND('',#7201,.T.);
#5468=FACE_OUTER_BOUND('',#7202,.T.);
#5469=FACE_OUTER_BOUND('',#7203,.T.);
#5470=FACE_OUTER_BOUND('',#7204,.T.);
#5471=FACE_OUTER_BOUND('',#7205,.T.);
#5472=FACE_OUTER_BOUND('',#7206,.T.);
#5473=FACE_OUTER_BOUND('',#7207,.T.);
#5474=FACE_OUTER_BOUND('',#7208,.T.);
#5475=FACE_OUTER_BOUND('',#7209,.T.);
#5476=FACE_OUTER_BOUND('',#7210,.T.);
#5477=FACE_OUTER_BOUND('',#7211,.T.);
#5478=FACE_OUTER_BOUND('',#7212,.T.);
#5479=FACE_OUTER_BOUND('',#7213,.T.);
#5480=FACE_OUTER_BOUND('',#7214,.T.);
#5481=FACE_OUTER_BOUND('',#7215,.T.);
#5482=FACE_OUTER_BOUND('',#7216,.T.);
#5483=FACE_OUTER_BOUND('',#7217,.T.);
#5484=FACE_OUTER_BOUND('',#7218,.T.);
#5485=FACE_OUTER_BOUND('',#7219,.T.);
#5486=FACE_OUTER_BOUND('',#7220,.T.);
#5487=FACE_OUTER_BOUND('',#7221,.T.);
#5488=FACE_OUTER_BOUND('',#7222,.T.);
#5489=FACE_OUTER_BOUND('',#7223,.T.);
#5490=FACE_OUTER_BOUND('',#7224,.T.);
#5491=FACE_OUTER_BOUND('',#7225,.T.);
#5492=FACE_OUTER_BOUND('',#7226,.T.);
#5493=FACE_OUTER_BOUND('',#7227,.T.);
#5494=FACE_OUTER_BOUND('',#7228,.T.);
#5495=FACE_OUTER_BOUND('',#7229,.T.);
#5496=FACE_OUTER_BOUND('',#7231,.T.);
#5497=FACE_OUTER_BOUND('',#7232,.T.);
#5498=FACE_OUTER_BOUND('',#7233,.T.);
#5499=FACE_OUTER_BOUND('',#7234,.T.);
#5500=FACE_OUTER_BOUND('',#7236,.T.);
#5501=FACE_OUTER_BOUND('',#7237,.T.);
#5502=FACE_OUTER_BOUND('',#7238,.T.);
#5503=FACE_OUTER_BOUND('',#7239,.T.);
#5504=FACE_OUTER_BOUND('',#7240,.T.);
#5505=FACE_OUTER_BOUND('',#7241,.T.);
#5506=FACE_OUTER_BOUND('',#7242,.T.);
#5507=FACE_OUTER_BOUND('',#7243,.T.);
#5508=FACE_OUTER_BOUND('',#7244,.T.);
#5509=FACE_OUTER_BOUND('',#7245,.T.);
#5510=FACE_OUTER_BOUND('',#7246,.T.);
#5511=FACE_OUTER_BOUND('',#7247,.T.);
#5512=FACE_OUTER_BOUND('',#7248,.T.);
#5513=FACE_OUTER_BOUND('',#7249,.T.);
#5514=FACE_OUTER_BOUND('',#7250,.T.);
#5515=FACE_OUTER_BOUND('',#7251,.T.);
#5516=FACE_OUTER_BOUND('',#7252,.T.);
#5517=FACE_OUTER_BOUND('',#7253,.T.);
#5518=FACE_OUTER_BOUND('',#7254,.T.);
#5519=FACE_OUTER_BOUND('',#7255,.T.);
#5520=FACE_OUTER_BOUND('',#7256,.T.);
#5521=FACE_OUTER_BOUND('',#7257,.T.);
#5522=FACE_OUTER_BOUND('',#7258,.T.);
#5523=FACE_OUTER_BOUND('',#7259,.T.);
#5524=FACE_OUTER_BOUND('',#7260,.T.);
#5525=FACE_OUTER_BOUND('',#7261,.T.);
#5526=FACE_OUTER_BOUND('',#7262,.T.);
#5527=FACE_OUTER_BOUND('',#7263,.T.);
#5528=FACE_OUTER_BOUND('',#7264,.T.);
#5529=FACE_OUTER_BOUND('',#7265,.T.);
#5530=FACE_OUTER_BOUND('',#7266,.T.);
#5531=FACE_OUTER_BOUND('',#7267,.T.);
#5532=FACE_OUTER_BOUND('',#7268,.T.);
#5533=FACE_OUTER_BOUND('',#7269,.T.);
#5534=FACE_OUTER_BOUND('',#7270,.T.);
#5535=FACE_OUTER_BOUND('',#7271,.T.);
#5536=FACE_OUTER_BOUND('',#7272,.T.);
#5537=FACE_OUTER_BOUND('',#7273,.T.);
#5538=FACE_OUTER_BOUND('',#7274,.T.);
#5539=FACE_OUTER_BOUND('',#7275,.T.);
#5540=FACE_OUTER_BOUND('',#7276,.T.);
#5541=FACE_OUTER_BOUND('',#7277,.T.);
#5542=FACE_OUTER_BOUND('',#7278,.T.);
#5543=FACE_OUTER_BOUND('',#7279,.T.);
#5544=FACE_OUTER_BOUND('',#7280,.T.);
#5545=FACE_OUTER_BOUND('',#7281,.T.);
#5546=FACE_OUTER_BOUND('',#7282,.T.);
#5547=FACE_OUTER_BOUND('',#7283,.T.);
#5548=FACE_OUTER_BOUND('',#7284,.T.);
#5549=FACE_OUTER_BOUND('',#7285,.T.);
#5550=FACE_OUTER_BOUND('',#7286,.T.);
#5551=FACE_OUTER_BOUND('',#7287,.T.);
#5552=FACE_OUTER_BOUND('',#7288,.T.);
#5553=FACE_OUTER_BOUND('',#7289,.T.);
#5554=FACE_OUTER_BOUND('',#7290,.T.);
#5555=FACE_OUTER_BOUND('',#7291,.T.);
#5556=FACE_OUTER_BOUND('',#7292,.T.);
#5557=FACE_OUTER_BOUND('',#7293,.T.);
#5558=FACE_OUTER_BOUND('',#7294,.T.);
#5559=FACE_OUTER_BOUND('',#7295,.T.);
#5560=FACE_OUTER_BOUND('',#7296,.T.);
#5561=FACE_OUTER_BOUND('',#7297,.T.);
#5562=FACE_OUTER_BOUND('',#7298,.T.);
#5563=FACE_OUTER_BOUND('',#7299,.T.);
#5564=FACE_OUTER_BOUND('',#7300,.T.);
#5565=FACE_OUTER_BOUND('',#7301,.T.);
#5566=FACE_OUTER_BOUND('',#7302,.T.);
#5567=FACE_OUTER_BOUND('',#7303,.T.);
#5568=FACE_OUTER_BOUND('',#7304,.T.);
#5569=FACE_OUTER_BOUND('',#7305,.T.);
#5570=FACE_OUTER_BOUND('',#7306,.T.);
#5571=FACE_OUTER_BOUND('',#7307,.T.);
#5572=FACE_OUTER_BOUND('',#7308,.T.);
#5573=FACE_OUTER_BOUND('',#7309,.T.);
#5574=FACE_OUTER_BOUND('',#7310,.T.);
#5575=FACE_OUTER_BOUND('',#7311,.T.);
#5576=FACE_OUTER_BOUND('',#7312,.T.);
#5577=FACE_OUTER_BOUND('',#7313,.T.);
#5578=FACE_OUTER_BOUND('',#7314,.T.);
#5579=FACE_OUTER_BOUND('',#7315,.T.);
#5580=FACE_OUTER_BOUND('',#7316,.T.);
#5581=FACE_OUTER_BOUND('',#7317,.T.);
#5582=FACE_OUTER_BOUND('',#7318,.T.);
#5583=FACE_OUTER_BOUND('',#7319,.T.);
#5584=FACE_OUTER_BOUND('',#7320,.T.);
#5585=FACE_OUTER_BOUND('',#7321,.T.);
#5586=FACE_OUTER_BOUND('',#7322,.T.);
#5587=FACE_OUTER_BOUND('',#7323,.T.);
#5588=FACE_OUTER_BOUND('',#7324,.T.);
#5589=FACE_OUTER_BOUND('',#7325,.T.);
#5590=FACE_OUTER_BOUND('',#7326,.T.);
#5591=FACE_OUTER_BOUND('',#7327,.T.);
#5592=FACE_OUTER_BOUND('',#7328,.T.);
#5593=FACE_OUTER_BOUND('',#7329,.T.);
#5594=FACE_OUTER_BOUND('',#7330,.T.);
#5595=FACE_OUTER_BOUND('',#7331,.T.);
#5596=FACE_OUTER_BOUND('',#7332,.T.);
#5597=FACE_OUTER_BOUND('',#7333,.T.);
#5598=FACE_OUTER_BOUND('',#7334,.T.);
#5599=FACE_OUTER_BOUND('',#7335,.T.);
#5600=FACE_OUTER_BOUND('',#7336,.T.);
#5601=FACE_OUTER_BOUND('',#7337,.T.);
#5602=FACE_OUTER_BOUND('',#7338,.T.);
#5603=FACE_OUTER_BOUND('',#7339,.T.);
#5604=FACE_OUTER_BOUND('',#7340,.T.);
#5605=FACE_OUTER_BOUND('',#7341,.T.);
#5606=FACE_OUTER_BOUND('',#7342,.T.);
#5607=FACE_OUTER_BOUND('',#7343,.T.);
#5608=FACE_OUTER_BOUND('',#7344,.T.);
#5609=FACE_OUTER_BOUND('',#7345,.T.);
#5610=FACE_OUTER_BOUND('',#7346,.T.);
#5611=FACE_OUTER_BOUND('',#7347,.T.);
#5612=FACE_OUTER_BOUND('',#7348,.T.);
#5613=FACE_OUTER_BOUND('',#7349,.T.);
#5614=FACE_OUTER_BOUND('',#7350,.T.);
#5615=FACE_OUTER_BOUND('',#7351,.T.);
#5616=FACE_OUTER_BOUND('',#7352,.T.);
#5617=FACE_OUTER_BOUND('',#7353,.T.);
#5618=FACE_OUTER_BOUND('',#7354,.T.);
#5619=FACE_OUTER_BOUND('',#7355,.T.);
#5620=FACE_OUTER_BOUND('',#7356,.T.);
#5621=FACE_OUTER_BOUND('',#7357,.T.);
#5622=FACE_OUTER_BOUND('',#7358,.T.);
#5623=FACE_OUTER_BOUND('',#7359,.T.);
#5624=FACE_OUTER_BOUND('',#7360,.T.);
#5625=FACE_OUTER_BOUND('',#7361,.T.);
#5626=FACE_OUTER_BOUND('',#7362,.T.);
#5627=FACE_OUTER_BOUND('',#7363,.T.);
#5628=FACE_OUTER_BOUND('',#7364,.T.);
#5629=FACE_OUTER_BOUND('',#7365,.T.);
#5630=FACE_OUTER_BOUND('',#7366,.T.);
#5631=FACE_OUTER_BOUND('',#7367,.T.);
#5632=FACE_OUTER_BOUND('',#7368,.T.);
#5633=FACE_OUTER_BOUND('',#7369,.T.);
#5634=FACE_OUTER_BOUND('',#7370,.T.);
#5635=FACE_OUTER_BOUND('',#7371,.T.);
#5636=FACE_OUTER_BOUND('',#7372,.T.);
#5637=FACE_OUTER_BOUND('',#7373,.T.);
#5638=FACE_OUTER_BOUND('',#7374,.T.);
#5639=FACE_OUTER_BOUND('',#7375,.T.);
#5640=FACE_OUTER_BOUND('',#7376,.T.);
#5641=FACE_OUTER_BOUND('',#7377,.T.);
#5642=FACE_OUTER_BOUND('',#7378,.T.);
#5643=FACE_OUTER_BOUND('',#7379,.T.);
#5644=FACE_OUTER_BOUND('',#7380,.T.);
#5645=FACE_OUTER_BOUND('',#7381,.T.);
#5646=FACE_OUTER_BOUND('',#7382,.T.);
#5647=FACE_OUTER_BOUND('',#7383,.T.);
#5648=FACE_OUTER_BOUND('',#7384,.T.);
#5649=FACE_OUTER_BOUND('',#7385,.T.);
#5650=FACE_OUTER_BOUND('',#7386,.T.);
#5651=FACE_OUTER_BOUND('',#7387,.T.);
#5652=FACE_OUTER_BOUND('',#7388,.T.);
#5653=FACE_OUTER_BOUND('',#7389,.T.);
#5654=FACE_OUTER_BOUND('',#7390,.T.);
#5655=FACE_OUTER_BOUND('',#7391,.T.);
#5656=FACE_OUTER_BOUND('',#7392,.T.);
#5657=FACE_OUTER_BOUND('',#7393,.T.);
#5658=FACE_OUTER_BOUND('',#7394,.T.);
#5659=FACE_OUTER_BOUND('',#7395,.T.);
#5660=FACE_OUTER_BOUND('',#7396,.T.);
#5661=FACE_OUTER_BOUND('',#7397,.T.);
#5662=FACE_OUTER_BOUND('',#7398,.T.);
#5663=FACE_OUTER_BOUND('',#7399,.T.);
#5664=FACE_OUTER_BOUND('',#7400,.T.);
#5665=FACE_OUTER_BOUND('',#7401,.T.);
#5666=FACE_OUTER_BOUND('',#7402,.T.);
#5667=FACE_OUTER_BOUND('',#7403,.T.);
#5668=FACE_OUTER_BOUND('',#7404,.T.);
#5669=FACE_OUTER_BOUND('',#7405,.T.);
#5670=FACE_OUTER_BOUND('',#7406,.T.);
#5671=FACE_OUTER_BOUND('',#7407,.T.);
#5672=FACE_OUTER_BOUND('',#7408,.T.);
#5673=FACE_OUTER_BOUND('',#7409,.T.);
#5674=FACE_OUTER_BOUND('',#7410,.T.);
#5675=FACE_OUTER_BOUND('',#7411,.T.);
#5676=FACE_OUTER_BOUND('',#7412,.T.);
#5677=FACE_OUTER_BOUND('',#7413,.T.);
#5678=FACE_OUTER_BOUND('',#7414,.T.);
#5679=FACE_OUTER_BOUND('',#7415,.T.);
#5680=FACE_OUTER_BOUND('',#7416,.T.);
#5681=FACE_OUTER_BOUND('',#7417,.T.);
#5682=FACE_OUTER_BOUND('',#7418,.T.);
#5683=FACE_OUTER_BOUND('',#7419,.T.);
#5684=FACE_OUTER_BOUND('',#7420,.T.);
#5685=FACE_OUTER_BOUND('',#7421,.T.);
#5686=FACE_OUTER_BOUND('',#7422,.T.);
#5687=FACE_OUTER_BOUND('',#7423,.T.);
#5688=FACE_OUTER_BOUND('',#7424,.T.);
#5689=FACE_OUTER_BOUND('',#7425,.T.);
#5690=FACE_OUTER_BOUND('',#7426,.T.);
#5691=FACE_OUTER_BOUND('',#7427,.T.);
#5692=FACE_OUTER_BOUND('',#7428,.T.);
#5693=FACE_OUTER_BOUND('',#7429,.T.);
#5694=FACE_OUTER_BOUND('',#7430,.T.);
#5695=FACE_OUTER_BOUND('',#7431,.T.);
#5696=FACE_OUTER_BOUND('',#7432,.T.);
#5697=FACE_OUTER_BOUND('',#7433,.T.);
#5698=FACE_OUTER_BOUND('',#7434,.T.);
#5699=FACE_OUTER_BOUND('',#7435,.T.);
#5700=FACE_OUTER_BOUND('',#7436,.T.);
#5701=FACE_OUTER_BOUND('',#7437,.T.);
#5702=FACE_OUTER_BOUND('',#7438,.T.);
#5703=FACE_OUTER_BOUND('',#7439,.T.);
#5704=FACE_OUTER_BOUND('',#7440,.T.);
#5705=FACE_OUTER_BOUND('',#7441,.T.);
#5706=FACE_OUTER_BOUND('',#7442,.T.);
#5707=FACE_OUTER_BOUND('',#7443,.T.);
#5708=FACE_OUTER_BOUND('',#7444,.T.);
#5709=FACE_OUTER_BOUND('',#7445,.T.);
#5710=FACE_OUTER_BOUND('',#7446,.T.);
#5711=FACE_OUTER_BOUND('',#7447,.T.);
#5712=FACE_OUTER_BOUND('',#7448,.T.);
#5713=FACE_OUTER_BOUND('',#7449,.T.);
#5714=FACE_OUTER_BOUND('',#7450,.T.);
#5715=FACE_OUTER_BOUND('',#7451,.T.);
#5716=FACE_OUTER_BOUND('',#7452,.T.);
#5717=FACE_OUTER_BOUND('',#7453,.T.);
#5718=FACE_OUTER_BOUND('',#7454,.T.);
#5719=FACE_OUTER_BOUND('',#7455,.T.);
#5720=FACE_OUTER_BOUND('',#7456,.T.);
#5721=FACE_OUTER_BOUND('',#7457,.T.);
#5722=FACE_OUTER_BOUND('',#7458,.T.);
#5723=FACE_OUTER_BOUND('',#7459,.T.);
#5724=FACE_OUTER_BOUND('',#7460,.T.);
#5725=FACE_OUTER_BOUND('',#7461,.T.);
#5726=FACE_OUTER_BOUND('',#7462,.T.);
#5727=FACE_OUTER_BOUND('',#7463,.T.);
#5728=FACE_OUTER_BOUND('',#7464,.T.);
#5729=FACE_OUTER_BOUND('',#7465,.T.);
#5730=FACE_OUTER_BOUND('',#7466,.T.);
#5731=FACE_OUTER_BOUND('',#7467,.T.);
#5732=FACE_OUTER_BOUND('',#7468,.T.);
#5733=FACE_OUTER_BOUND('',#7469,.T.);
#5734=FACE_OUTER_BOUND('',#7470,.T.);
#5735=FACE_OUTER_BOUND('',#7471,.T.);
#5736=FACE_OUTER_BOUND('',#7472,.T.);
#5737=FACE_OUTER_BOUND('',#7473,.T.);
#5738=FACE_OUTER_BOUND('',#7474,.T.);
#5739=FACE_OUTER_BOUND('',#7475,.T.);
#5740=FACE_OUTER_BOUND('',#7476,.T.);
#5741=FACE_OUTER_BOUND('',#7477,.T.);
#5742=FACE_OUTER_BOUND('',#7478,.T.);
#5743=FACE_OUTER_BOUND('',#7479,.T.);
#5744=FACE_OUTER_BOUND('',#7480,.T.);
#5745=FACE_OUTER_BOUND('',#7481,.T.);
#5746=FACE_OUTER_BOUND('',#7482,.T.);
#5747=FACE_OUTER_BOUND('',#7483,.T.);
#5748=FACE_OUTER_BOUND('',#7484,.T.);
#5749=FACE_OUTER_BOUND('',#7485,.T.);
#5750=FACE_OUTER_BOUND('',#7486,.T.);
#5751=FACE_OUTER_BOUND('',#7487,.T.);
#5752=FACE_OUTER_BOUND('',#7488,.T.);
#5753=FACE_OUTER_BOUND('',#7489,.T.);
#5754=FACE_OUTER_BOUND('',#7490,.T.);
#5755=FACE_OUTER_BOUND('',#7491,.T.);
#5756=FACE_OUTER_BOUND('',#7492,.T.);
#5757=FACE_OUTER_BOUND('',#7493,.T.);
#5758=FACE_OUTER_BOUND('',#7494,.T.);
#5759=FACE_OUTER_BOUND('',#7495,.T.);
#5760=FACE_OUTER_BOUND('',#7496,.T.);
#5761=FACE_OUTER_BOUND('',#7497,.T.);
#5762=FACE_OUTER_BOUND('',#7498,.T.);
#5763=FACE_OUTER_BOUND('',#7499,.T.);
#5764=FACE_OUTER_BOUND('',#7500,.T.);
#5765=FACE_OUTER_BOUND('',#7501,.T.);
#5766=FACE_OUTER_BOUND('',#7502,.T.);
#5767=FACE_OUTER_BOUND('',#7503,.T.);
#5768=FACE_OUTER_BOUND('',#7504,.T.);
#5769=FACE_OUTER_BOUND('',#7505,.T.);
#5770=FACE_OUTER_BOUND('',#7506,.T.);
#5771=FACE_OUTER_BOUND('',#7507,.T.);
#5772=FACE_OUTER_BOUND('',#7508,.T.);
#5773=FACE_OUTER_BOUND('',#7509,.T.);
#5774=FACE_OUTER_BOUND('',#7510,.T.);
#5775=FACE_OUTER_BOUND('',#7511,.T.);
#5776=FACE_OUTER_BOUND('',#7512,.T.);
#5777=FACE_OUTER_BOUND('',#7513,.T.);
#5778=FACE_OUTER_BOUND('',#7514,.T.);
#5779=FACE_OUTER_BOUND('',#7515,.T.);
#5780=FACE_OUTER_BOUND('',#7516,.T.);
#5781=FACE_OUTER_BOUND('',#7517,.T.);
#5782=FACE_OUTER_BOUND('',#7518,.T.);
#5783=FACE_OUTER_BOUND('',#7519,.T.);
#5784=FACE_OUTER_BOUND('',#7520,.T.);
#5785=FACE_OUTER_BOUND('',#7521,.T.);
#5786=FACE_OUTER_BOUND('',#7522,.T.);
#5787=FACE_OUTER_BOUND('',#7523,.T.);
#5788=FACE_OUTER_BOUND('',#7524,.T.);
#5789=FACE_OUTER_BOUND('',#7525,.T.);
#5790=FACE_OUTER_BOUND('',#7526,.T.);
#5791=FACE_OUTER_BOUND('',#7527,.T.);
#5792=FACE_OUTER_BOUND('',#7528,.T.);
#5793=FACE_OUTER_BOUND('',#7529,.T.);
#5794=FACE_OUTER_BOUND('',#7530,.T.);
#5795=FACE_OUTER_BOUND('',#7531,.T.);
#5796=FACE_OUTER_BOUND('',#7532,.T.);
#5797=FACE_OUTER_BOUND('',#7533,.T.);
#5798=FACE_OUTER_BOUND('',#7534,.T.);
#5799=FACE_OUTER_BOUND('',#7535,.T.);
#5800=FACE_OUTER_BOUND('',#7536,.T.);
#5801=FACE_OUTER_BOUND('',#7537,.T.);
#5802=FACE_OUTER_BOUND('',#7538,.T.);
#5803=FACE_OUTER_BOUND('',#7539,.T.);
#5804=FACE_OUTER_BOUND('',#7540,.T.);
#5805=FACE_OUTER_BOUND('',#7541,.T.);
#5806=FACE_OUTER_BOUND('',#7542,.T.);
#5807=FACE_OUTER_BOUND('',#7543,.T.);
#5808=FACE_OUTER_BOUND('',#7544,.T.);
#5809=FACE_OUTER_BOUND('',#7545,.T.);
#5810=FACE_OUTER_BOUND('',#7546,.T.);
#5811=FACE_OUTER_BOUND('',#7547,.T.);
#5812=FACE_OUTER_BOUND('',#7548,.T.);
#5813=FACE_OUTER_BOUND('',#7549,.T.);
#5814=FACE_OUTER_BOUND('',#7550,.T.);
#5815=FACE_OUTER_BOUND('',#7551,.T.);
#5816=FACE_OUTER_BOUND('',#7552,.T.);
#5817=FACE_OUTER_BOUND('',#7553,.T.);
#5818=FACE_OUTER_BOUND('',#7554,.T.);
#5819=FACE_OUTER_BOUND('',#7555,.T.);
#5820=FACE_OUTER_BOUND('',#7556,.T.);
#5821=FACE_OUTER_BOUND('',#7557,.T.);
#5822=FACE_OUTER_BOUND('',#7558,.T.);
#5823=FACE_OUTER_BOUND('',#7559,.T.);
#5824=FACE_OUTER_BOUND('',#7560,.T.);
#5825=FACE_OUTER_BOUND('',#7561,.T.);
#5826=FACE_OUTER_BOUND('',#7562,.T.);
#5827=FACE_OUTER_BOUND('',#7563,.T.);
#5828=FACE_OUTER_BOUND('',#7564,.T.);
#5829=FACE_OUTER_BOUND('',#7565,.T.);
#5830=FACE_OUTER_BOUND('',#7566,.T.);
#5831=FACE_OUTER_BOUND('',#7567,.T.);
#5832=FACE_OUTER_BOUND('',#7568,.T.);
#5833=FACE_OUTER_BOUND('',#7569,.T.);
#5834=FACE_OUTER_BOUND('',#7570,.T.);
#5835=FACE_OUTER_BOUND('',#7571,.T.);
#5836=FACE_OUTER_BOUND('',#7572,.T.);
#5837=FACE_OUTER_BOUND('',#7573,.T.);
#5838=FACE_OUTER_BOUND('',#7574,.T.);
#5839=FACE_OUTER_BOUND('',#7575,.T.);
#5840=FACE_OUTER_BOUND('',#7576,.T.);
#5841=FACE_OUTER_BOUND('',#7577,.T.);
#5842=FACE_OUTER_BOUND('',#7578,.T.);
#5843=FACE_OUTER_BOUND('',#7579,.T.);
#5844=FACE_OUTER_BOUND('',#7580,.T.);
#5845=FACE_OUTER_BOUND('',#7581,.T.);
#5846=FACE_OUTER_BOUND('',#7582,.T.);
#5847=FACE_OUTER_BOUND('',#7583,.T.);
#5848=FACE_OUTER_BOUND('',#7584,.T.);
#5849=FACE_OUTER_BOUND('',#7585,.T.);
#5850=FACE_OUTER_BOUND('',#7586,.T.);
#5851=FACE_OUTER_BOUND('',#7587,.T.);
#5852=FACE_OUTER_BOUND('',#7588,.T.);
#5853=FACE_OUTER_BOUND('',#7589,.T.);
#5854=FACE_OUTER_BOUND('',#7590,.T.);
#5855=FACE_OUTER_BOUND('',#7591,.T.);
#5856=FACE_OUTER_BOUND('',#7592,.T.);
#5857=FACE_OUTER_BOUND('',#7593,.T.);
#5858=FACE_OUTER_BOUND('',#7594,.T.);
#5859=FACE_OUTER_BOUND('',#7595,.T.);
#5860=FACE_OUTER_BOUND('',#7596,.T.);
#5861=FACE_OUTER_BOUND('',#7597,.T.);
#5862=FACE_OUTER_BOUND('',#7598,.T.);
#5863=FACE_OUTER_BOUND('',#7599,.T.);
#5864=FACE_OUTER_BOUND('',#7600,.T.);
#5865=FACE_OUTER_BOUND('',#7601,.T.);
#5866=FACE_OUTER_BOUND('',#7602,.T.);
#5867=FACE_OUTER_BOUND('',#7603,.T.);
#5868=FACE_OUTER_BOUND('',#7604,.T.);
#5869=FACE_OUTER_BOUND('',#7605,.T.);
#5870=FACE_OUTER_BOUND('',#7606,.T.);
#5871=FACE_OUTER_BOUND('',#7607,.T.);
#5872=FACE_OUTER_BOUND('',#7608,.T.);
#5873=FACE_OUTER_BOUND('',#7609,.T.);
#5874=FACE_OUTER_BOUND('',#7610,.T.);
#5875=FACE_OUTER_BOUND('',#7611,.T.);
#5876=FACE_OUTER_BOUND('',#7612,.T.);
#5877=FACE_OUTER_BOUND('',#7613,.T.);
#5878=FACE_OUTER_BOUND('',#7614,.T.);
#5879=FACE_OUTER_BOUND('',#7615,.T.);
#5880=FACE_OUTER_BOUND('',#7616,.T.);
#5881=FACE_OUTER_BOUND('',#7617,.T.);
#5882=FACE_OUTER_BOUND('',#7618,.T.);
#5883=FACE_OUTER_BOUND('',#7619,.T.);
#5884=FACE_OUTER_BOUND('',#7620,.T.);
#5885=FACE_OUTER_BOUND('',#7621,.T.);
#5886=FACE_OUTER_BOUND('',#7622,.T.);
#5887=FACE_OUTER_BOUND('',#7623,.T.);
#5888=FACE_OUTER_BOUND('',#7624,.T.);
#5889=FACE_OUTER_BOUND('',#7625,.T.);
#5890=FACE_OUTER_BOUND('',#7626,.T.);
#5891=FACE_OUTER_BOUND('',#7627,.T.);
#5892=FACE_OUTER_BOUND('',#7628,.T.);
#5893=FACE_OUTER_BOUND('',#7629,.T.);
#5894=FACE_OUTER_BOUND('',#7630,.T.);
#5895=FACE_OUTER_BOUND('',#7631,.T.);
#5896=FACE_OUTER_BOUND('',#7632,.T.);
#5897=FACE_OUTER_BOUND('',#7633,.T.);
#5898=FACE_OUTER_BOUND('',#7634,.T.);
#5899=FACE_OUTER_BOUND('',#7635,.T.);
#5900=FACE_OUTER_BOUND('',#7636,.T.);
#5901=FACE_OUTER_BOUND('',#7637,.T.);
#5902=FACE_OUTER_BOUND('',#7638,.T.);
#5903=FACE_OUTER_BOUND('',#7639,.T.);
#5904=FACE_OUTER_BOUND('',#7640,.T.);
#5905=FACE_OUTER_BOUND('',#7641,.T.);
#5906=FACE_OUTER_BOUND('',#7642,.T.);
#5907=FACE_OUTER_BOUND('',#7643,.T.);
#5908=FACE_OUTER_BOUND('',#7644,.T.);
#5909=FACE_OUTER_BOUND('',#7645,.T.);
#5910=FACE_OUTER_BOUND('',#7646,.T.);
#5911=FACE_OUTER_BOUND('',#7647,.T.);
#5912=FACE_OUTER_BOUND('',#7648,.T.);
#5913=FACE_OUTER_BOUND('',#7649,.T.);
#5914=FACE_OUTER_BOUND('',#7650,.T.);
#5915=FACE_OUTER_BOUND('',#7651,.T.);
#5916=FACE_OUTER_BOUND('',#7652,.T.);
#5917=FACE_OUTER_BOUND('',#7653,.T.);
#5918=FACE_OUTER_BOUND('',#7654,.T.);
#5919=FACE_OUTER_BOUND('',#7655,.T.);
#5920=FACE_OUTER_BOUND('',#7656,.T.);
#5921=FACE_OUTER_BOUND('',#7657,.T.);
#5922=FACE_OUTER_BOUND('',#7658,.T.);
#5923=FACE_OUTER_BOUND('',#7659,.T.);
#5924=FACE_OUTER_BOUND('',#7660,.T.);
#5925=FACE_OUTER_BOUND('',#7661,.T.);
#5926=FACE_OUTER_BOUND('',#7662,.T.);
#5927=FACE_OUTER_BOUND('',#7663,.T.);
#5928=FACE_OUTER_BOUND('',#7664,.T.);
#5929=FACE_OUTER_BOUND('',#7665,.T.);
#5930=FACE_OUTER_BOUND('',#7666,.T.);
#5931=FACE_OUTER_BOUND('',#7667,.T.);
#5932=FACE_OUTER_BOUND('',#7668,.T.);
#5933=FACE_OUTER_BOUND('',#7669,.T.);
#5934=FACE_OUTER_BOUND('',#7670,.T.);
#5935=FACE_OUTER_BOUND('',#7671,.T.);
#5936=FACE_OUTER_BOUND('',#7672,.T.);
#5937=FACE_OUTER_BOUND('',#7673,.T.);
#5938=FACE_OUTER_BOUND('',#7674,.T.);
#5939=FACE_OUTER_BOUND('',#7675,.T.);
#5940=FACE_OUTER_BOUND('',#7676,.T.);
#5941=FACE_OUTER_BOUND('',#7677,.T.);
#5942=FACE_OUTER_BOUND('',#7678,.T.);
#5943=FACE_OUTER_BOUND('',#7679,.T.);
#5944=FACE_OUTER_BOUND('',#7680,.T.);
#5945=FACE_OUTER_BOUND('',#7681,.T.);
#5946=FACE_OUTER_BOUND('',#7682,.T.);
#5947=FACE_OUTER_BOUND('',#7683,.T.);
#5948=FACE_OUTER_BOUND('',#7684,.T.);
#5949=FACE_OUTER_BOUND('',#7685,.T.);
#5950=FACE_OUTER_BOUND('',#7686,.T.);
#5951=FACE_OUTER_BOUND('',#7687,.T.);
#5952=FACE_OUTER_BOUND('',#7688,.T.);
#5953=FACE_OUTER_BOUND('',#7689,.T.);
#5954=FACE_OUTER_BOUND('',#7690,.T.);
#5955=FACE_OUTER_BOUND('',#7691,.T.);
#5956=FACE_OUTER_BOUND('',#7692,.T.);
#5957=FACE_OUTER_BOUND('',#7693,.T.);
#5958=FACE_OUTER_BOUND('',#7694,.T.);
#5959=FACE_OUTER_BOUND('',#7695,.T.);
#5960=FACE_OUTER_BOUND('',#7696,.T.);
#5961=FACE_OUTER_BOUND('',#7697,.T.);
#5962=FACE_OUTER_BOUND('',#7698,.T.);
#5963=FACE_OUTER_BOUND('',#7699,.T.);
#5964=FACE_OUTER_BOUND('',#7700,.T.);
#5965=FACE_OUTER_BOUND('',#7701,.T.);
#5966=FACE_OUTER_BOUND('',#7702,.T.);
#5967=FACE_OUTER_BOUND('',#7703,.T.);
#5968=FACE_OUTER_BOUND('',#7704,.T.);
#5969=FACE_OUTER_BOUND('',#7705,.T.);
#5970=FACE_OUTER_BOUND('',#7706,.T.);
#5971=FACE_OUTER_BOUND('',#7707,.T.);
#5972=FACE_OUTER_BOUND('',#7708,.T.);
#5973=FACE_OUTER_BOUND('',#7709,.T.);
#5974=FACE_OUTER_BOUND('',#7710,.T.);
#5975=FACE_OUTER_BOUND('',#7711,.T.);
#5976=FACE_OUTER_BOUND('',#7712,.T.);
#5977=FACE_OUTER_BOUND('',#7713,.T.);
#5978=FACE_OUTER_BOUND('',#7714,.T.);
#5979=FACE_OUTER_BOUND('',#7715,.T.);
#5980=FACE_OUTER_BOUND('',#7716,.T.);
#5981=FACE_OUTER_BOUND('',#7717,.T.);
#5982=FACE_OUTER_BOUND('',#7718,.T.);
#5983=FACE_OUTER_BOUND('',#7719,.T.);
#5984=FACE_OUTER_BOUND('',#7720,.T.);
#5985=FACE_OUTER_BOUND('',#7721,.T.);
#5986=FACE_OUTER_BOUND('',#7722,.T.);
#5987=FACE_OUTER_BOUND('',#7723,.T.);
#5988=FACE_OUTER_BOUND('',#7724,.T.);
#5989=FACE_OUTER_BOUND('',#7725,.T.);
#5990=FACE_OUTER_BOUND('',#7726,.T.);
#5991=FACE_OUTER_BOUND('',#7727,.T.);
#5992=FACE_OUTER_BOUND('',#7728,.T.);
#5993=FACE_OUTER_BOUND('',#7729,.T.);
#5994=FACE_OUTER_BOUND('',#7730,.T.);
#5995=FACE_OUTER_BOUND('',#7731,.T.);
#5996=FACE_OUTER_BOUND('',#7732,.T.);
#5997=FACE_OUTER_BOUND('',#7733,.T.);
#5998=FACE_OUTER_BOUND('',#7734,.T.);
#5999=FACE_OUTER_BOUND('',#7735,.T.);
#6000=FACE_OUTER_BOUND('',#7736,.T.);
#6001=FACE_OUTER_BOUND('',#7737,.T.);
#6002=FACE_OUTER_BOUND('',#7738,.T.);
#6003=FACE_OUTER_BOUND('',#7739,.T.);
#6004=FACE_OUTER_BOUND('',#7740,.T.);
#6005=FACE_OUTER_BOUND('',#7741,.T.);
#6006=FACE_OUTER_BOUND('',#7742,.T.);
#6007=FACE_OUTER_BOUND('',#7743,.T.);
#6008=FACE_OUTER_BOUND('',#7744,.T.);
#6009=FACE_OUTER_BOUND('',#7745,.T.);
#6010=FACE_OUTER_BOUND('',#7746,.T.);
#6011=FACE_OUTER_BOUND('',#7747,.T.);
#6012=FACE_OUTER_BOUND('',#7748,.T.);
#6013=FACE_OUTER_BOUND('',#7749,.T.);
#6014=FACE_OUTER_BOUND('',#7750,.T.);
#6015=FACE_OUTER_BOUND('',#7751,.T.);
#6016=FACE_OUTER_BOUND('',#7752,.T.);
#6017=FACE_OUTER_BOUND('',#7753,.T.);
#6018=FACE_OUTER_BOUND('',#7754,.T.);
#6019=FACE_OUTER_BOUND('',#7755,.T.);
#6020=FACE_OUTER_BOUND('',#7756,.T.);
#6021=FACE_OUTER_BOUND('',#7757,.T.);
#6022=FACE_OUTER_BOUND('',#7758,.T.);
#6023=FACE_OUTER_BOUND('',#7759,.T.);
#6024=FACE_OUTER_BOUND('',#7760,.T.);
#6025=FACE_OUTER_BOUND('',#7761,.T.);
#6026=FACE_OUTER_BOUND('',#7762,.T.);
#6027=FACE_OUTER_BOUND('',#7763,.T.);
#6028=FACE_OUTER_BOUND('',#7764,.T.);
#6029=FACE_OUTER_BOUND('',#7765,.T.);
#6030=FACE_OUTER_BOUND('',#7766,.T.);
#6031=FACE_OUTER_BOUND('',#7767,.T.);
#6032=FACE_OUTER_BOUND('',#7768,.T.);
#6033=FACE_OUTER_BOUND('',#7769,.T.);
#6034=FACE_OUTER_BOUND('',#7770,.T.);
#6035=FACE_OUTER_BOUND('',#7771,.T.);
#6036=FACE_OUTER_BOUND('',#7772,.T.);
#6037=FACE_OUTER_BOUND('',#7773,.T.);
#6038=FACE_OUTER_BOUND('',#7774,.T.);
#6039=FACE_OUTER_BOUND('',#7775,.T.);
#6040=FACE_OUTER_BOUND('',#7776,.T.);
#6041=FACE_OUTER_BOUND('',#7777,.T.);
#6042=FACE_OUTER_BOUND('',#7778,.T.);
#6043=FACE_OUTER_BOUND('',#7779,.T.);
#6044=FACE_OUTER_BOUND('',#7780,.T.);
#6045=FACE_OUTER_BOUND('',#7781,.T.);
#6046=FACE_OUTER_BOUND('',#7782,.T.);
#6047=FACE_OUTER_BOUND('',#7783,.T.);
#6048=FACE_OUTER_BOUND('',#7784,.T.);
#6049=FACE_OUTER_BOUND('',#7785,.T.);
#6050=FACE_OUTER_BOUND('',#7786,.T.);
#6051=FACE_OUTER_BOUND('',#7787,.T.);
#6052=FACE_OUTER_BOUND('',#7788,.T.);
#6053=FACE_OUTER_BOUND('',#7789,.T.);
#6054=FACE_OUTER_BOUND('',#7790,.T.);
#6055=FACE_OUTER_BOUND('',#7791,.T.);
#6056=FACE_OUTER_BOUND('',#7792,.T.);
#6057=FACE_OUTER_BOUND('',#7793,.T.);
#6058=FACE_OUTER_BOUND('',#7794,.T.);
#6059=FACE_OUTER_BOUND('',#7796,.T.);
#6060=FACE_OUTER_BOUND('',#7797,.T.);
#6061=FACE_OUTER_BOUND('',#7798,.T.);
#6062=FACE_OUTER_BOUND('',#7799,.T.);
#6063=FACE_OUTER_BOUND('',#7801,.T.);
#6064=FACE_OUTER_BOUND('',#7802,.T.);
#6065=FACE_OUTER_BOUND('',#7803,.T.);
#6066=FACE_OUTER_BOUND('',#7804,.T.);
#6067=FACE_OUTER_BOUND('',#7805,.T.);
#6068=FACE_OUTER_BOUND('',#7806,.T.);
#6069=FACE_OUTER_BOUND('',#7807,.T.);
#6070=FACE_OUTER_BOUND('',#7808,.T.);
#6071=FACE_OUTER_BOUND('',#7809,.T.);
#6072=FACE_OUTER_BOUND('',#7810,.T.);
#6073=FACE_OUTER_BOUND('',#7811,.T.);
#6074=FACE_OUTER_BOUND('',#7812,.T.);
#6075=FACE_OUTER_BOUND('',#7813,.T.);
#6076=FACE_OUTER_BOUND('',#7814,.T.);
#6077=FACE_OUTER_BOUND('',#7815,.T.);
#6078=FACE_OUTER_BOUND('',#7816,.T.);
#6079=FACE_OUTER_BOUND('',#7817,.T.);
#6080=FACE_OUTER_BOUND('',#7818,.T.);
#6081=FACE_OUTER_BOUND('',#7819,.T.);
#6082=FACE_OUTER_BOUND('',#7820,.T.);
#6083=FACE_OUTER_BOUND('',#7821,.T.);
#6084=FACE_OUTER_BOUND('',#7822,.T.);
#6085=FACE_OUTER_BOUND('',#7823,.T.);
#6086=FACE_OUTER_BOUND('',#7824,.T.);
#6087=FACE_OUTER_BOUND('',#7825,.T.);
#6088=FACE_OUTER_BOUND('',#7826,.T.);
#6089=FACE_OUTER_BOUND('',#7827,.T.);
#6090=FACE_OUTER_BOUND('',#7828,.T.);
#6091=FACE_OUTER_BOUND('',#7829,.T.);
#6092=FACE_OUTER_BOUND('',#7830,.T.);
#6093=FACE_OUTER_BOUND('',#7831,.T.);
#6094=FACE_OUTER_BOUND('',#7832,.T.);
#6095=FACE_OUTER_BOUND('',#7833,.T.);
#6096=FACE_OUTER_BOUND('',#7834,.T.);
#6097=FACE_OUTER_BOUND('',#7835,.T.);
#6098=FACE_OUTER_BOUND('',#7836,.T.);
#6099=FACE_OUTER_BOUND('',#7837,.T.);
#6100=FACE_OUTER_BOUND('',#7838,.T.);
#6101=FACE_OUTER_BOUND('',#7839,.T.);
#6102=FACE_OUTER_BOUND('',#7840,.T.);
#6103=FACE_OUTER_BOUND('',#7841,.T.);
#6104=FACE_OUTER_BOUND('',#7842,.T.);
#6105=FACE_OUTER_BOUND('',#7843,.T.);
#6106=FACE_OUTER_BOUND('',#7844,.T.);
#6107=FACE_OUTER_BOUND('',#7845,.T.);
#6108=FACE_OUTER_BOUND('',#7846,.T.);
#6109=FACE_OUTER_BOUND('',#7847,.T.);
#6110=FACE_OUTER_BOUND('',#7848,.T.);
#6111=FACE_OUTER_BOUND('',#7849,.T.);
#6112=FACE_OUTER_BOUND('',#7850,.T.);
#6113=FACE_OUTER_BOUND('',#7851,.T.);
#6114=FACE_OUTER_BOUND('',#7852,.T.);
#6115=FACE_OUTER_BOUND('',#7853,.T.);
#6116=FACE_OUTER_BOUND('',#7854,.T.);
#6117=FACE_OUTER_BOUND('',#7855,.T.);
#6118=FACE_OUTER_BOUND('',#7856,.T.);
#6119=FACE_OUTER_BOUND('',#7857,.T.);
#6120=FACE_OUTER_BOUND('',#7858,.T.);
#6121=FACE_OUTER_BOUND('',#7859,.T.);
#6122=FACE_OUTER_BOUND('',#7860,.T.);
#6123=FACE_OUTER_BOUND('',#7861,.T.);
#6124=FACE_OUTER_BOUND('',#7862,.T.);
#6125=FACE_OUTER_BOUND('',#7863,.T.);
#6126=FACE_OUTER_BOUND('',#7864,.T.);
#6127=FACE_OUTER_BOUND('',#7865,.T.);
#6128=FACE_OUTER_BOUND('',#7866,.T.);
#6129=FACE_OUTER_BOUND('',#7867,.T.);
#6130=FACE_OUTER_BOUND('',#7868,.T.);
#6131=FACE_OUTER_BOUND('',#7869,.T.);
#6132=FACE_OUTER_BOUND('',#7870,.T.);
#6133=FACE_OUTER_BOUND('',#7871,.T.);
#6134=FACE_OUTER_BOUND('',#7872,.T.);
#6135=FACE_OUTER_BOUND('',#7873,.T.);
#6136=FACE_OUTER_BOUND('',#7874,.T.);
#6137=FACE_OUTER_BOUND('',#7875,.T.);
#6138=FACE_OUTER_BOUND('',#7876,.T.);
#6139=FACE_OUTER_BOUND('',#7877,.T.);
#6140=FACE_OUTER_BOUND('',#7878,.T.);
#6141=FACE_OUTER_BOUND('',#7879,.T.);
#6142=FACE_OUTER_BOUND('',#7880,.T.);
#6143=FACE_OUTER_BOUND('',#7881,.T.);
#6144=FACE_OUTER_BOUND('',#7882,.T.);
#6145=FACE_OUTER_BOUND('',#7883,.T.);
#6146=FACE_OUTER_BOUND('',#7884,.T.);
#6147=FACE_OUTER_BOUND('',#7885,.T.);
#6148=FACE_OUTER_BOUND('',#7886,.T.);
#6149=FACE_OUTER_BOUND('',#7887,.T.);
#6150=FACE_OUTER_BOUND('',#7888,.T.);
#6151=FACE_OUTER_BOUND('',#7889,.T.);
#6152=FACE_OUTER_BOUND('',#7890,.T.);
#6153=FACE_OUTER_BOUND('',#7891,.T.);
#6154=FACE_OUTER_BOUND('',#7892,.T.);
#6155=FACE_OUTER_BOUND('',#7893,.T.);
#6156=FACE_OUTER_BOUND('',#7894,.T.);
#6157=FACE_OUTER_BOUND('',#7895,.T.);
#6158=FACE_OUTER_BOUND('',#7896,.T.);
#6159=FACE_OUTER_BOUND('',#7897,.T.);
#6160=FACE_OUTER_BOUND('',#7898,.T.);
#6161=FACE_OUTER_BOUND('',#7899,.T.);
#6162=FACE_OUTER_BOUND('',#7900,.T.);
#6163=FACE_OUTER_BOUND('',#7901,.T.);
#6164=FACE_OUTER_BOUND('',#7902,.T.);
#6165=FACE_OUTER_BOUND('',#7903,.T.);
#6166=FACE_OUTER_BOUND('',#7904,.T.);
#6167=FACE_OUTER_BOUND('',#7905,.T.);
#6168=FACE_OUTER_BOUND('',#7906,.T.);
#6169=FACE_OUTER_BOUND('',#7907,.T.);
#6170=FACE_OUTER_BOUND('',#7908,.T.);
#6171=FACE_OUTER_BOUND('',#7909,.T.);
#6172=FACE_OUTER_BOUND('',#7910,.T.);
#6173=FACE_OUTER_BOUND('',#7911,.T.);
#6174=FACE_OUTER_BOUND('',#7912,.T.);
#6175=FACE_OUTER_BOUND('',#7913,.T.);
#6176=FACE_OUTER_BOUND('',#7914,.T.);
#6177=FACE_OUTER_BOUND('',#7915,.T.);
#6178=FACE_OUTER_BOUND('',#7916,.T.);
#6179=FACE_OUTER_BOUND('',#7917,.T.);
#6180=FACE_OUTER_BOUND('',#7918,.T.);
#6181=FACE_OUTER_BOUND('',#7919,.T.);
#6182=FACE_OUTER_BOUND('',#7920,.T.);
#6183=FACE_OUTER_BOUND('',#7921,.T.);
#6184=FACE_OUTER_BOUND('',#7922,.T.);
#6185=FACE_OUTER_BOUND('',#7923,.T.);
#6186=FACE_OUTER_BOUND('',#7924,.T.);
#6187=FACE_OUTER_BOUND('',#7925,.T.);
#6188=FACE_OUTER_BOUND('',#7926,.T.);
#6189=FACE_OUTER_BOUND('',#7927,.T.);
#6190=FACE_OUTER_BOUND('',#7928,.T.);
#6191=FACE_OUTER_BOUND('',#7929,.T.);
#6192=FACE_OUTER_BOUND('',#7930,.T.);
#6193=FACE_OUTER_BOUND('',#7931,.T.);
#6194=FACE_OUTER_BOUND('',#7932,.T.);
#6195=FACE_OUTER_BOUND('',#7933,.T.);
#6196=FACE_OUTER_BOUND('',#7934,.T.);
#6197=FACE_OUTER_BOUND('',#7935,.T.);
#6198=FACE_OUTER_BOUND('',#7936,.T.);
#6199=FACE_OUTER_BOUND('',#7937,.T.);
#6200=FACE_OUTER_BOUND('',#7938,.T.);
#6201=FACE_OUTER_BOUND('',#7939,.T.);
#6202=FACE_OUTER_BOUND('',#7940,.T.);
#6203=FACE_OUTER_BOUND('',#7941,.T.);
#6204=FACE_OUTER_BOUND('',#7942,.T.);
#6205=FACE_OUTER_BOUND('',#7943,.T.);
#6206=FACE_OUTER_BOUND('',#7944,.T.);
#6207=FACE_OUTER_BOUND('',#7945,.T.);
#6208=FACE_OUTER_BOUND('',#7946,.T.);
#6209=FACE_OUTER_BOUND('',#7947,.T.);
#6210=FACE_OUTER_BOUND('',#7948,.T.);
#6211=FACE_OUTER_BOUND('',#7949,.T.);
#6212=FACE_OUTER_BOUND('',#7950,.T.);
#6213=FACE_OUTER_BOUND('',#7951,.T.);
#6214=FACE_OUTER_BOUND('',#7952,.T.);
#6215=FACE_OUTER_BOUND('',#7953,.T.);
#6216=FACE_OUTER_BOUND('',#7954,.T.);
#6217=FACE_OUTER_BOUND('',#7955,.T.);
#6218=FACE_OUTER_BOUND('',#7956,.T.);
#6219=FACE_OUTER_BOUND('',#7957,.T.);
#6220=FACE_OUTER_BOUND('',#7958,.T.);
#6221=FACE_OUTER_BOUND('',#7959,.T.);
#6222=FACE_OUTER_BOUND('',#7960,.T.);
#6223=FACE_OUTER_BOUND('',#7961,.T.);
#6224=FACE_OUTER_BOUND('',#7962,.T.);
#6225=FACE_OUTER_BOUND('',#7963,.T.);
#6226=FACE_OUTER_BOUND('',#7964,.T.);
#6227=FACE_OUTER_BOUND('',#7965,.T.);
#6228=FACE_OUTER_BOUND('',#7966,.T.);
#6229=FACE_OUTER_BOUND('',#7967,.T.);
#6230=FACE_OUTER_BOUND('',#7968,.T.);
#6231=FACE_OUTER_BOUND('',#7969,.T.);
#6232=FACE_OUTER_BOUND('',#7970,.T.);
#6233=FACE_OUTER_BOUND('',#7971,.T.);
#6234=FACE_OUTER_BOUND('',#7972,.T.);
#6235=FACE_OUTER_BOUND('',#7973,.T.);
#6236=FACE_OUTER_BOUND('',#7974,.T.);
#6237=FACE_OUTER_BOUND('',#7975,.T.);
#6238=FACE_OUTER_BOUND('',#7976,.T.);
#6239=FACE_OUTER_BOUND('',#7977,.T.);
#6240=FACE_OUTER_BOUND('',#7978,.T.);
#6241=FACE_OUTER_BOUND('',#7979,.T.);
#6242=FACE_OUTER_BOUND('',#7980,.T.);
#6243=FACE_OUTER_BOUND('',#7981,.T.);
#6244=FACE_OUTER_BOUND('',#7982,.T.);
#6245=FACE_OUTER_BOUND('',#7983,.T.);
#6246=FACE_OUTER_BOUND('',#7984,.T.);
#6247=FACE_OUTER_BOUND('',#7985,.T.);
#6248=FACE_OUTER_BOUND('',#7986,.T.);
#6249=FACE_OUTER_BOUND('',#7987,.T.);
#6250=FACE_OUTER_BOUND('',#7988,.T.);
#6251=FACE_OUTER_BOUND('',#7989,.T.);
#6252=FACE_OUTER_BOUND('',#7990,.T.);
#6253=FACE_OUTER_BOUND('',#7991,.T.);
#6254=FACE_OUTER_BOUND('',#7992,.T.);
#6255=FACE_OUTER_BOUND('',#7993,.T.);
#6256=FACE_OUTER_BOUND('',#7994,.T.);
#6257=FACE_OUTER_BOUND('',#7995,.T.);
#6258=FACE_OUTER_BOUND('',#7996,.T.);
#6259=FACE_OUTER_BOUND('',#7997,.T.);
#6260=FACE_OUTER_BOUND('',#7998,.T.);
#6261=FACE_OUTER_BOUND('',#7999,.T.);
#6262=FACE_OUTER_BOUND('',#8000,.T.);
#6263=FACE_OUTER_BOUND('',#8001,.T.);
#6264=FACE_OUTER_BOUND('',#8002,.T.);
#6265=FACE_OUTER_BOUND('',#8003,.T.);
#6266=FACE_OUTER_BOUND('',#8004,.T.);
#6267=FACE_OUTER_BOUND('',#8005,.T.);
#6268=FACE_OUTER_BOUND('',#8006,.T.);
#6269=FACE_OUTER_BOUND('',#8007,.T.);
#6270=FACE_OUTER_BOUND('',#8008,.T.);
#6271=FACE_OUTER_BOUND('',#8009,.T.);
#6272=FACE_OUTER_BOUND('',#8010,.T.);
#6273=FACE_OUTER_BOUND('',#8011,.T.);
#6274=FACE_OUTER_BOUND('',#8012,.T.);
#6275=FACE_OUTER_BOUND('',#8013,.T.);
#6276=FACE_OUTER_BOUND('',#8014,.T.);
#6277=FACE_OUTER_BOUND('',#8015,.T.);
#6278=FACE_OUTER_BOUND('',#8016,.T.);
#6279=FACE_OUTER_BOUND('',#8017,.T.);
#6280=FACE_OUTER_BOUND('',#8018,.T.);
#6281=FACE_OUTER_BOUND('',#8019,.T.);
#6282=FACE_OUTER_BOUND('',#8020,.T.);
#6283=FACE_OUTER_BOUND('',#8021,.T.);
#6284=FACE_OUTER_BOUND('',#8022,.T.);
#6285=FACE_OUTER_BOUND('',#8023,.T.);
#6286=FACE_OUTER_BOUND('',#8024,.T.);
#6287=FACE_OUTER_BOUND('',#8025,.T.);
#6288=FACE_OUTER_BOUND('',#8026,.T.);
#6289=FACE_OUTER_BOUND('',#8027,.T.);
#6290=FACE_OUTER_BOUND('',#8028,.T.);
#6291=FACE_OUTER_BOUND('',#8029,.T.);
#6292=FACE_OUTER_BOUND('',#8030,.T.);
#6293=FACE_OUTER_BOUND('',#8031,.T.);
#6294=FACE_OUTER_BOUND('',#8032,.T.);
#6295=FACE_OUTER_BOUND('',#8033,.T.);
#6296=FACE_OUTER_BOUND('',#8034,.T.);
#6297=FACE_OUTER_BOUND('',#8035,.T.);
#6298=FACE_OUTER_BOUND('',#8036,.T.);
#6299=FACE_OUTER_BOUND('',#8037,.T.);
#6300=FACE_OUTER_BOUND('',#8038,.T.);
#6301=FACE_OUTER_BOUND('',#8039,.T.);
#6302=FACE_OUTER_BOUND('',#8040,.T.);
#6303=FACE_OUTER_BOUND('',#8041,.T.);
#6304=FACE_OUTER_BOUND('',#8042,.T.);
#6305=FACE_OUTER_BOUND('',#8043,.T.);
#6306=FACE_OUTER_BOUND('',#8044,.T.);
#6307=FACE_OUTER_BOUND('',#8045,.T.);
#6308=FACE_OUTER_BOUND('',#8046,.T.);
#6309=FACE_OUTER_BOUND('',#8047,.T.);
#6310=FACE_OUTER_BOUND('',#8048,.T.);
#6311=FACE_OUTER_BOUND('',#8049,.T.);
#6312=FACE_OUTER_BOUND('',#8050,.T.);
#6313=FACE_OUTER_BOUND('',#8051,.T.);
#6314=FACE_OUTER_BOUND('',#8052,.T.);
#6315=FACE_OUTER_BOUND('',#8053,.T.);
#6316=FACE_OUTER_BOUND('',#8054,.T.);
#6317=FACE_OUTER_BOUND('',#8055,.T.);
#6318=FACE_OUTER_BOUND('',#8056,.T.);
#6319=FACE_OUTER_BOUND('',#8057,.T.);
#6320=FACE_OUTER_BOUND('',#8058,.T.);
#6321=FACE_OUTER_BOUND('',#8059,.T.);
#6322=FACE_OUTER_BOUND('',#8060,.T.);
#6323=FACE_OUTER_BOUND('',#8061,.T.);
#6324=FACE_OUTER_BOUND('',#8062,.T.);
#6325=FACE_OUTER_BOUND('',#8063,.T.);
#6326=FACE_OUTER_BOUND('',#8064,.T.);
#6327=FACE_OUTER_BOUND('',#8065,.T.);
#6328=FACE_OUTER_BOUND('',#8066,.T.);
#6329=FACE_OUTER_BOUND('',#8067,.T.);
#6330=FACE_OUTER_BOUND('',#8068,.T.);
#6331=FACE_OUTER_BOUND('',#8069,.T.);
#6332=FACE_OUTER_BOUND('',#8070,.T.);
#6333=FACE_OUTER_BOUND('',#8071,.T.);
#6334=FACE_OUTER_BOUND('',#8072,.T.);
#6335=FACE_OUTER_BOUND('',#8073,.T.);
#6336=FACE_OUTER_BOUND('',#8074,.T.);
#6337=FACE_OUTER_BOUND('',#8075,.T.);
#6338=FACE_OUTER_BOUND('',#8076,.T.);
#6339=FACE_OUTER_BOUND('',#8077,.T.);
#6340=FACE_OUTER_BOUND('',#8078,.T.);
#6341=FACE_OUTER_BOUND('',#8079,.T.);
#6342=FACE_OUTER_BOUND('',#8080,.T.);
#6343=FACE_OUTER_BOUND('',#8081,.T.);
#6344=FACE_OUTER_BOUND('',#8082,.T.);
#6345=FACE_OUTER_BOUND('',#8083,.T.);
#6346=FACE_OUTER_BOUND('',#8084,.T.);
#6347=FACE_OUTER_BOUND('',#8085,.T.);
#6348=FACE_OUTER_BOUND('',#8086,.T.);
#6349=FACE_OUTER_BOUND('',#8087,.T.);
#6350=FACE_OUTER_BOUND('',#8088,.T.);
#6351=FACE_OUTER_BOUND('',#8089,.T.);
#6352=FACE_OUTER_BOUND('',#8090,.T.);
#6353=FACE_OUTER_BOUND('',#8091,.T.);
#6354=FACE_OUTER_BOUND('',#8092,.T.);
#6355=FACE_OUTER_BOUND('',#8093,.T.);
#6356=FACE_OUTER_BOUND('',#8094,.T.);
#6357=FACE_OUTER_BOUND('',#8095,.T.);
#6358=FACE_OUTER_BOUND('',#8096,.T.);
#6359=FACE_OUTER_BOUND('',#8097,.T.);
#6360=FACE_OUTER_BOUND('',#8098,.T.);
#6361=FACE_OUTER_BOUND('',#8099,.T.);
#6362=FACE_OUTER_BOUND('',#8100,.T.);
#6363=FACE_OUTER_BOUND('',#8101,.T.);
#6364=FACE_OUTER_BOUND('',#8102,.T.);
#6365=FACE_OUTER_BOUND('',#8103,.T.);
#6366=FACE_OUTER_BOUND('',#8104,.T.);
#6367=FACE_OUTER_BOUND('',#8105,.T.);
#6368=FACE_OUTER_BOUND('',#8106,.T.);
#6369=FACE_OUTER_BOUND('',#8107,.T.);
#6370=FACE_OUTER_BOUND('',#8108,.T.);
#6371=FACE_OUTER_BOUND('',#8109,.T.);
#6372=FACE_OUTER_BOUND('',#8110,.T.);
#6373=FACE_OUTER_BOUND('',#8111,.T.);
#6374=FACE_OUTER_BOUND('',#8112,.T.);
#6375=FACE_OUTER_BOUND('',#8113,.T.);
#6376=FACE_OUTER_BOUND('',#8114,.T.);
#6377=FACE_OUTER_BOUND('',#8115,.T.);
#6378=FACE_OUTER_BOUND('',#8116,.T.);
#6379=FACE_OUTER_BOUND('',#8117,.T.);
#6380=FACE_OUTER_BOUND('',#8118,.T.);
#6381=FACE_OUTER_BOUND('',#8119,.T.);
#6382=FACE_OUTER_BOUND('',#8120,.T.);
#6383=FACE_OUTER_BOUND('',#8121,.T.);
#6384=FACE_OUTER_BOUND('',#8122,.T.);
#6385=FACE_OUTER_BOUND('',#8123,.T.);
#6386=FACE_OUTER_BOUND('',#8124,.T.);
#6387=FACE_OUTER_BOUND('',#8125,.T.);
#6388=FACE_OUTER_BOUND('',#8126,.T.);
#6389=FACE_OUTER_BOUND('',#8127,.T.);
#6390=FACE_OUTER_BOUND('',#8128,.T.);
#6391=FACE_OUTER_BOUND('',#8129,.T.);
#6392=FACE_OUTER_BOUND('',#8130,.T.);
#6393=FACE_OUTER_BOUND('',#8131,.T.);
#6394=FACE_OUTER_BOUND('',#8132,.T.);
#6395=FACE_OUTER_BOUND('',#8133,.T.);
#6396=FACE_OUTER_BOUND('',#8134,.T.);
#6397=FACE_OUTER_BOUND('',#8135,.T.);
#6398=FACE_OUTER_BOUND('',#8136,.T.);
#6399=FACE_OUTER_BOUND('',#8137,.T.);
#6400=FACE_OUTER_BOUND('',#8138,.T.);
#6401=FACE_OUTER_BOUND('',#8139,.T.);
#6402=FACE_OUTER_BOUND('',#8140,.T.);
#6403=FACE_OUTER_BOUND('',#8141,.T.);
#6404=FACE_OUTER_BOUND('',#8142,.T.);
#6405=FACE_OUTER_BOUND('',#8143,.T.);
#6406=FACE_OUTER_BOUND('',#8144,.T.);
#6407=FACE_OUTER_BOUND('',#8145,.T.);
#6408=FACE_OUTER_BOUND('',#8146,.T.);
#6409=FACE_OUTER_BOUND('',#8147,.T.);
#6410=FACE_OUTER_BOUND('',#8148,.T.);
#6411=FACE_OUTER_BOUND('',#8149,.T.);
#6412=FACE_OUTER_BOUND('',#8150,.T.);
#6413=FACE_OUTER_BOUND('',#8151,.T.);
#6414=FACE_OUTER_BOUND('',#8152,.T.);
#6415=FACE_OUTER_BOUND('',#8153,.T.);
#6416=FACE_OUTER_BOUND('',#8154,.T.);
#6417=FACE_OUTER_BOUND('',#8155,.T.);
#6418=FACE_OUTER_BOUND('',#8156,.T.);
#6419=FACE_OUTER_BOUND('',#8157,.T.);
#6420=FACE_OUTER_BOUND('',#8158,.T.);
#6421=FACE_OUTER_BOUND('',#8159,.T.);
#6422=FACE_OUTER_BOUND('',#8160,.T.);
#6423=FACE_OUTER_BOUND('',#8161,.T.);
#6424=FACE_OUTER_BOUND('',#8162,.T.);
#6425=FACE_OUTER_BOUND('',#8163,.T.);
#6426=FACE_OUTER_BOUND('',#8164,.T.);
#6427=FACE_OUTER_BOUND('',#8165,.T.);
#6428=FACE_OUTER_BOUND('',#8166,.T.);
#6429=FACE_OUTER_BOUND('',#8167,.T.);
#6430=FACE_OUTER_BOUND('',#8168,.T.);
#6431=FACE_OUTER_BOUND('',#8169,.T.);
#6432=FACE_OUTER_BOUND('',#8170,.T.);
#6433=FACE_OUTER_BOUND('',#8171,.T.);
#6434=FACE_OUTER_BOUND('',#8172,.T.);
#6435=FACE_OUTER_BOUND('',#8173,.T.);
#6436=FACE_OUTER_BOUND('',#8174,.T.);
#6437=FACE_OUTER_BOUND('',#8175,.T.);
#6438=FACE_OUTER_BOUND('',#8176,.T.);
#6439=FACE_OUTER_BOUND('',#8177,.T.);
#6440=FACE_OUTER_BOUND('',#8178,.T.);
#6441=FACE_OUTER_BOUND('',#8179,.T.);
#6442=FACE_OUTER_BOUND('',#8180,.T.);
#6443=FACE_OUTER_BOUND('',#8181,.T.);
#6444=FACE_OUTER_BOUND('',#8182,.T.);
#6445=FACE_OUTER_BOUND('',#8183,.T.);
#6446=FACE_OUTER_BOUND('',#8184,.T.);
#6447=FACE_OUTER_BOUND('',#8185,.T.);
#6448=FACE_OUTER_BOUND('',#8186,.T.);
#6449=FACE_OUTER_BOUND('',#8187,.T.);
#6450=FACE_OUTER_BOUND('',#8188,.T.);
#6451=FACE_OUTER_BOUND('',#8189,.T.);
#6452=FACE_OUTER_BOUND('',#8190,.T.);
#6453=FACE_OUTER_BOUND('',#8191,.T.);
#6454=FACE_OUTER_BOUND('',#8192,.T.);
#6455=FACE_OUTER_BOUND('',#8193,.T.);
#6456=FACE_OUTER_BOUND('',#8194,.T.);
#6457=FACE_OUTER_BOUND('',#8195,.T.);
#6458=FACE_OUTER_BOUND('',#8196,.T.);
#6459=FACE_OUTER_BOUND('',#8197,.T.);
#6460=FACE_OUTER_BOUND('',#8198,.T.);
#6461=FACE_OUTER_BOUND('',#8199,.T.);
#6462=FACE_OUTER_BOUND('',#8200,.T.);
#6463=FACE_OUTER_BOUND('',#8201,.T.);
#6464=FACE_OUTER_BOUND('',#8202,.T.);
#6465=FACE_OUTER_BOUND('',#8203,.T.);
#6466=FACE_OUTER_BOUND('',#8204,.T.);
#6467=FACE_OUTER_BOUND('',#8205,.T.);
#6468=FACE_OUTER_BOUND('',#8206,.T.);
#6469=FACE_OUTER_BOUND('',#8207,.T.);
#6470=FACE_OUTER_BOUND('',#8208,.T.);
#6471=FACE_OUTER_BOUND('',#8209,.T.);
#6472=FACE_OUTER_BOUND('',#8210,.T.);
#6473=FACE_OUTER_BOUND('',#8211,.T.);
#6474=FACE_OUTER_BOUND('',#8212,.T.);
#6475=FACE_OUTER_BOUND('',#8213,.T.);
#6476=FACE_OUTER_BOUND('',#8214,.T.);
#6477=FACE_OUTER_BOUND('',#8215,.T.);
#6478=FACE_OUTER_BOUND('',#8216,.T.);
#6479=FACE_OUTER_BOUND('',#8217,.T.);
#6480=FACE_OUTER_BOUND('',#8218,.T.);
#6481=FACE_OUTER_BOUND('',#8219,.T.);
#6482=FACE_OUTER_BOUND('',#8220,.T.);
#6483=FACE_OUTER_BOUND('',#8221,.T.);
#6484=FACE_OUTER_BOUND('',#8222,.T.);
#6485=FACE_OUTER_BOUND('',#8223,.T.);
#6486=FACE_OUTER_BOUND('',#8224,.T.);
#6487=FACE_OUTER_BOUND('',#8225,.T.);
#6488=FACE_OUTER_BOUND('',#8226,.T.);
#6489=FACE_OUTER_BOUND('',#8227,.T.);
#6490=FACE_OUTER_BOUND('',#8228,.T.);
#6491=FACE_OUTER_BOUND('',#8229,.T.);
#6492=FACE_OUTER_BOUND('',#8230,.T.);
#6493=FACE_OUTER_BOUND('',#8231,.T.);
#6494=FACE_OUTER_BOUND('',#8232,.T.);
#6495=FACE_OUTER_BOUND('',#8233,.T.);
#6496=FACE_OUTER_BOUND('',#8234,.T.);
#6497=FACE_OUTER_BOUND('',#8235,.T.);
#6498=FACE_OUTER_BOUND('',#8236,.T.);
#6499=FACE_OUTER_BOUND('',#8237,.T.);
#6500=FACE_OUTER_BOUND('',#8238,.T.);
#6501=FACE_OUTER_BOUND('',#8239,.T.);
#6502=FACE_OUTER_BOUND('',#8240,.T.);
#6503=FACE_OUTER_BOUND('',#8241,.T.);
#6504=FACE_OUTER_BOUND('',#8242,.T.);
#6505=FACE_OUTER_BOUND('',#8243,.T.);
#6506=FACE_OUTER_BOUND('',#8244,.T.);
#6507=FACE_OUTER_BOUND('',#8245,.T.);
#6508=FACE_OUTER_BOUND('',#8246,.T.);
#6509=FACE_OUTER_BOUND('',#8247,.T.);
#6510=FACE_OUTER_BOUND('',#8248,.T.);
#6511=FACE_OUTER_BOUND('',#8249,.T.);
#6512=FACE_OUTER_BOUND('',#8250,.T.);
#6513=FACE_OUTER_BOUND('',#8251,.T.);
#6514=FACE_OUTER_BOUND('',#8252,.T.);
#6515=FACE_OUTER_BOUND('',#8253,.T.);
#6516=FACE_OUTER_BOUND('',#8254,.T.);
#6517=FACE_OUTER_BOUND('',#8255,.T.);
#6518=FACE_OUTER_BOUND('',#8256,.T.);
#6519=FACE_OUTER_BOUND('',#8257,.T.);
#6520=FACE_OUTER_BOUND('',#8258,.T.);
#6521=FACE_OUTER_BOUND('',#8259,.T.);
#6522=FACE_OUTER_BOUND('',#8260,.T.);
#6523=FACE_OUTER_BOUND('',#8261,.T.);
#6524=FACE_OUTER_BOUND('',#8262,.T.);
#6525=FACE_OUTER_BOUND('',#8263,.T.);
#6526=FACE_OUTER_BOUND('',#8264,.T.);
#6527=FACE_OUTER_BOUND('',#8265,.T.);
#6528=FACE_OUTER_BOUND('',#8266,.T.);
#6529=FACE_OUTER_BOUND('',#8267,.T.);
#6530=FACE_OUTER_BOUND('',#8268,.T.);
#6531=FACE_OUTER_BOUND('',#8269,.T.);
#6532=FACE_OUTER_BOUND('',#8270,.T.);
#6533=FACE_OUTER_BOUND('',#8271,.T.);
#6534=FACE_OUTER_BOUND('',#8272,.T.);
#6535=FACE_OUTER_BOUND('',#8273,.T.);
#6536=FACE_OUTER_BOUND('',#8274,.T.);
#6537=FACE_OUTER_BOUND('',#8275,.T.);
#6538=FACE_OUTER_BOUND('',#8276,.T.);
#6539=FACE_OUTER_BOUND('',#8277,.T.);
#6540=FACE_OUTER_BOUND('',#8278,.T.);
#6541=FACE_OUTER_BOUND('',#8279,.T.);
#6542=FACE_OUTER_BOUND('',#8280,.T.);
#6543=FACE_OUTER_BOUND('',#8281,.T.);
#6544=FACE_OUTER_BOUND('',#8282,.T.);
#6545=FACE_OUTER_BOUND('',#8283,.T.);
#6546=FACE_OUTER_BOUND('',#8284,.T.);
#6547=FACE_OUTER_BOUND('',#8285,.T.);
#6548=FACE_OUTER_BOUND('',#8286,.T.);
#6549=FACE_OUTER_BOUND('',#8287,.T.);
#6550=FACE_OUTER_BOUND('',#8288,.T.);
#6551=FACE_OUTER_BOUND('',#8289,.T.);
#6552=FACE_OUTER_BOUND('',#8290,.T.);
#6553=FACE_OUTER_BOUND('',#8291,.T.);
#6554=FACE_OUTER_BOUND('',#8292,.T.);
#6555=FACE_OUTER_BOUND('',#8293,.T.);
#6556=FACE_OUTER_BOUND('',#8294,.T.);
#6557=FACE_OUTER_BOUND('',#8295,.T.);
#6558=FACE_OUTER_BOUND('',#8296,.T.);
#6559=FACE_OUTER_BOUND('',#8297,.T.);
#6560=FACE_OUTER_BOUND('',#8298,.T.);
#6561=FACE_OUTER_BOUND('',#8299,.T.);
#6562=FACE_OUTER_BOUND('',#8300,.T.);
#6563=FACE_OUTER_BOUND('',#8301,.T.);
#6564=FACE_OUTER_BOUND('',#8302,.T.);
#6565=FACE_OUTER_BOUND('',#8303,.T.);
#6566=FACE_OUTER_BOUND('',#8304,.T.);
#6567=FACE_OUTER_BOUND('',#8305,.T.);
#6568=FACE_OUTER_BOUND('',#8306,.T.);
#6569=FACE_OUTER_BOUND('',#8307,.T.);
#6570=FACE_OUTER_BOUND('',#8308,.T.);
#6571=FACE_OUTER_BOUND('',#8309,.T.);
#6572=FACE_OUTER_BOUND('',#8310,.T.);
#6573=FACE_OUTER_BOUND('',#8311,.T.);
#6574=FACE_OUTER_BOUND('',#8312,.T.);
#6575=FACE_OUTER_BOUND('',#8313,.T.);
#6576=FACE_OUTER_BOUND('',#8314,.T.);
#6577=FACE_OUTER_BOUND('',#8315,.T.);
#6578=FACE_OUTER_BOUND('',#8316,.T.);
#6579=FACE_OUTER_BOUND('',#8317,.T.);
#6580=FACE_OUTER_BOUND('',#8318,.T.);
#6581=FACE_OUTER_BOUND('',#8319,.T.);
#6582=FACE_OUTER_BOUND('',#8320,.T.);
#6583=FACE_OUTER_BOUND('',#8321,.T.);
#6584=FACE_OUTER_BOUND('',#8322,.T.);
#6585=FACE_OUTER_BOUND('',#8323,.T.);
#6586=FACE_OUTER_BOUND('',#8324,.T.);
#6587=FACE_OUTER_BOUND('',#8325,.T.);
#6588=FACE_OUTER_BOUND('',#8326,.T.);
#6589=FACE_OUTER_BOUND('',#8327,.T.);
#6590=FACE_OUTER_BOUND('',#8328,.T.);
#6591=FACE_OUTER_BOUND('',#8329,.T.);
#6592=FACE_OUTER_BOUND('',#8330,.T.);
#6593=FACE_OUTER_BOUND('',#8331,.T.);
#6594=FACE_OUTER_BOUND('',#8332,.T.);
#6595=FACE_OUTER_BOUND('',#8333,.T.);
#6596=FACE_OUTER_BOUND('',#8334,.T.);
#6597=FACE_OUTER_BOUND('',#8335,.T.);
#6598=FACE_OUTER_BOUND('',#8336,.T.);
#6599=FACE_OUTER_BOUND('',#8337,.T.);
#6600=FACE_OUTER_BOUND('',#8338,.T.);
#6601=FACE_OUTER_BOUND('',#8339,.T.);
#6602=FACE_OUTER_BOUND('',#8340,.T.);
#6603=FACE_OUTER_BOUND('',#8341,.T.);
#6604=FACE_OUTER_BOUND('',#8342,.T.);
#6605=FACE_OUTER_BOUND('',#8343,.T.);
#6606=FACE_OUTER_BOUND('',#8344,.T.);
#6607=FACE_OUTER_BOUND('',#8345,.T.);
#6608=FACE_OUTER_BOUND('',#8346,.T.);
#6609=FACE_OUTER_BOUND('',#8347,.T.);
#6610=FACE_OUTER_BOUND('',#8348,.T.);
#6611=FACE_OUTER_BOUND('',#8349,.T.);
#6612=FACE_OUTER_BOUND('',#8350,.T.);
#6613=FACE_OUTER_BOUND('',#8351,.T.);
#6614=FACE_OUTER_BOUND('',#8352,.T.);
#6615=FACE_OUTER_BOUND('',#8353,.T.);
#6616=FACE_OUTER_BOUND('',#8354,.T.);
#6617=FACE_OUTER_BOUND('',#8355,.T.);
#6618=FACE_OUTER_BOUND('',#8356,.T.);
#6619=FACE_OUTER_BOUND('',#8357,.T.);
#6620=FACE_OUTER_BOUND('',#8358,.T.);
#6621=FACE_OUTER_BOUND('',#8359,.T.);
#6622=FACE_OUTER_BOUND('',#8361,.T.);
#6623=FACE_OUTER_BOUND('',#8362,.T.);
#6624=FACE_OUTER_BOUND('',#8363,.T.);
#6625=FACE_OUTER_BOUND('',#8364,.T.);
#6626=FACE_OUTER_BOUND('',#8366,.T.);
#6627=FACE_OUTER_BOUND('',#8367,.T.);
#6628=FACE_OUTER_BOUND('',#8368,.T.);
#6629=FACE_OUTER_BOUND('',#8369,.T.);
#6630=FACE_OUTER_BOUND('',#8370,.T.);
#6631=FACE_OUTER_BOUND('',#8371,.T.);
#6632=FACE_OUTER_BOUND('',#8372,.T.);
#6633=FACE_OUTER_BOUND('',#8373,.T.);
#6634=FACE_OUTER_BOUND('',#8374,.T.);
#6635=FACE_OUTER_BOUND('',#8375,.T.);
#6636=FACE_OUTER_BOUND('',#8376,.T.);
#6637=FACE_OUTER_BOUND('',#8377,.T.);
#6638=FACE_OUTER_BOUND('',#8378,.T.);
#6639=FACE_OUTER_BOUND('',#8379,.T.);
#6640=FACE_OUTER_BOUND('',#8380,.T.);
#6641=FACE_OUTER_BOUND('',#8381,.T.);
#6642=FACE_OUTER_BOUND('',#8382,.T.);
#6643=FACE_OUTER_BOUND('',#8383,.T.);
#6644=FACE_OUTER_BOUND('',#8384,.T.);
#6645=FACE_OUTER_BOUND('',#8385,.T.);
#6646=FACE_OUTER_BOUND('',#8386,.T.);
#6647=FACE_OUTER_BOUND('',#8387,.T.);
#6648=FACE_OUTER_BOUND('',#8388,.T.);
#6649=FACE_OUTER_BOUND('',#8389,.T.);
#6650=FACE_OUTER_BOUND('',#8390,.T.);
#6651=FACE_OUTER_BOUND('',#8391,.T.);
#6652=FACE_OUTER_BOUND('',#8392,.T.);
#6653=FACE_OUTER_BOUND('',#8393,.T.);
#6654=FACE_OUTER_BOUND('',#8394,.T.);
#6655=FACE_OUTER_BOUND('',#8395,.T.);
#6656=FACE_OUTER_BOUND('',#8396,.T.);
#6657=FACE_OUTER_BOUND('',#8397,.T.);
#6658=FACE_OUTER_BOUND('',#8398,.T.);
#6659=FACE_OUTER_BOUND('',#8399,.T.);
#6660=FACE_OUTER_BOUND('',#8400,.T.);
#6661=FACE_OUTER_BOUND('',#8401,.T.);
#6662=FACE_OUTER_BOUND('',#8402,.T.);
#6663=FACE_OUTER_BOUND('',#8403,.T.);
#6664=FACE_OUTER_BOUND('',#8404,.T.);
#6665=FACE_OUTER_BOUND('',#8405,.T.);
#6666=FACE_OUTER_BOUND('',#8406,.T.);
#6667=FACE_OUTER_BOUND('',#8407,.T.);
#6668=FACE_OUTER_BOUND('',#8408,.T.);
#6669=FACE_OUTER_BOUND('',#8409,.T.);
#6670=FACE_OUTER_BOUND('',#8410,.T.);
#6671=FACE_OUTER_BOUND('',#8411,.T.);
#6672=FACE_OUTER_BOUND('',#8412,.T.);
#6673=FACE_OUTER_BOUND('',#8413,.T.);
#6674=FACE_OUTER_BOUND('',#8414,.T.);
#6675=FACE_OUTER_BOUND('',#8415,.T.);
#6676=FACE_OUTER_BOUND('',#8416,.T.);
#6677=FACE_OUTER_BOUND('',#8417,.T.);
#6678=FACE_OUTER_BOUND('',#8418,.T.);
#6679=FACE_OUTER_BOUND('',#8419,.T.);
#6680=FACE_OUTER_BOUND('',#8420,.T.);
#6681=FACE_OUTER_BOUND('',#8421,.T.);
#6682=FACE_OUTER_BOUND('',#8422,.T.);
#6683=FACE_OUTER_BOUND('',#8423,.T.);
#6684=FACE_OUTER_BOUND('',#8424,.T.);
#6685=FACE_OUTER_BOUND('',#8425,.T.);
#6686=FACE_OUTER_BOUND('',#8426,.T.);
#6687=FACE_OUTER_BOUND('',#8427,.T.);
#6688=FACE_OUTER_BOUND('',#8428,.T.);
#6689=FACE_OUTER_BOUND('',#8429,.T.);
#6690=FACE_OUTER_BOUND('',#8430,.T.);
#6691=FACE_OUTER_BOUND('',#8431,.T.);
#6692=FACE_OUTER_BOUND('',#8432,.T.);
#6693=FACE_OUTER_BOUND('',#8433,.T.);
#6694=FACE_OUTER_BOUND('',#8434,.T.);
#6695=FACE_OUTER_BOUND('',#8435,.T.);
#6696=FACE_OUTER_BOUND('',#8436,.T.);
#6697=FACE_OUTER_BOUND('',#8437,.T.);
#6698=FACE_OUTER_BOUND('',#8438,.T.);
#6699=FACE_OUTER_BOUND('',#8439,.T.);
#6700=FACE_OUTER_BOUND('',#8440,.T.);
#6701=FACE_OUTER_BOUND('',#8441,.T.);
#6702=FACE_OUTER_BOUND('',#8442,.T.);
#6703=FACE_OUTER_BOUND('',#8443,.T.);
#6704=FACE_OUTER_BOUND('',#8444,.T.);
#6705=FACE_OUTER_BOUND('',#8445,.T.);
#6706=FACE_OUTER_BOUND('',#8446,.T.);
#6707=FACE_OUTER_BOUND('',#8447,.T.);
#6708=FACE_OUTER_BOUND('',#8448,.T.);
#6709=FACE_OUTER_BOUND('',#8449,.T.);
#6710=FACE_OUTER_BOUND('',#8450,.T.);
#6711=FACE_OUTER_BOUND('',#8451,.T.);
#6712=FACE_OUTER_BOUND('',#8452,.T.);
#6713=FACE_OUTER_BOUND('',#8453,.T.);
#6714=FACE_OUTER_BOUND('',#8454,.T.);
#6715=FACE_OUTER_BOUND('',#8455,.T.);
#6716=FACE_OUTER_BOUND('',#8456,.T.);
#6717=FACE_OUTER_BOUND('',#8457,.T.);
#6718=FACE_OUTER_BOUND('',#8458,.T.);
#6719=FACE_OUTER_BOUND('',#8459,.T.);
#6720=FACE_OUTER_BOUND('',#8460,.T.);
#6721=FACE_OUTER_BOUND('',#8461,.T.);
#6722=FACE_OUTER_BOUND('',#8462,.T.);
#6723=FACE_OUTER_BOUND('',#8463,.T.);
#6724=FACE_OUTER_BOUND('',#8464,.T.);
#6725=FACE_OUTER_BOUND('',#8465,.T.);
#6726=FACE_OUTER_BOUND('',#8466,.T.);
#6727=FACE_OUTER_BOUND('',#8467,.T.);
#6728=FACE_OUTER_BOUND('',#8468,.T.);
#6729=FACE_OUTER_BOUND('',#8469,.T.);
#6730=FACE_OUTER_BOUND('',#8470,.T.);
#6731=FACE_OUTER_BOUND('',#8471,.T.);
#6732=FACE_OUTER_BOUND('',#8472,.T.);
#6733=FACE_OUTER_BOUND('',#8473,.T.);
#6734=FACE_OUTER_BOUND('',#8474,.T.);
#6735=FACE_OUTER_BOUND('',#8475,.T.);
#6736=FACE_OUTER_BOUND('',#8476,.T.);
#6737=FACE_OUTER_BOUND('',#8477,.T.);
#6738=FACE_OUTER_BOUND('',#8478,.T.);
#6739=FACE_OUTER_BOUND('',#8479,.T.);
#6740=FACE_OUTER_BOUND('',#8480,.T.);
#6741=FACE_OUTER_BOUND('',#8481,.T.);
#6742=FACE_OUTER_BOUND('',#8482,.T.);
#6743=FACE_OUTER_BOUND('',#8483,.T.);
#6744=FACE_OUTER_BOUND('',#8484,.T.);
#6745=FACE_OUTER_BOUND('',#8485,.T.);
#6746=FACE_OUTER_BOUND('',#8486,.T.);
#6747=FACE_OUTER_BOUND('',#8487,.T.);
#6748=FACE_OUTER_BOUND('',#8488,.T.);
#6749=FACE_OUTER_BOUND('',#8489,.T.);
#6750=FACE_OUTER_BOUND('',#8490,.T.);
#6751=FACE_OUTER_BOUND('',#8491,.T.);
#6752=FACE_OUTER_BOUND('',#8492,.T.);
#6753=FACE_OUTER_BOUND('',#8493,.T.);
#6754=FACE_OUTER_BOUND('',#8494,.T.);
#6755=FACE_OUTER_BOUND('',#8495,.T.);
#6756=FACE_OUTER_BOUND('',#8496,.T.);
#6757=FACE_OUTER_BOUND('',#8497,.T.);
#6758=FACE_OUTER_BOUND('',#8498,.T.);
#6759=FACE_OUTER_BOUND('',#8499,.T.);
#6760=FACE_OUTER_BOUND('',#8500,.T.);
#6761=FACE_OUTER_BOUND('',#8501,.T.);
#6762=FACE_OUTER_BOUND('',#8502,.T.);
#6763=FACE_OUTER_BOUND('',#8503,.T.);
#6764=FACE_OUTER_BOUND('',#8504,.T.);
#6765=FACE_OUTER_BOUND('',#8505,.T.);
#6766=FACE_OUTER_BOUND('',#8506,.T.);
#6767=FACE_OUTER_BOUND('',#8507,.T.);
#6768=FACE_OUTER_BOUND('',#8508,.T.);
#6769=FACE_OUTER_BOUND('',#8509,.T.);
#6770=FACE_OUTER_BOUND('',#8510,.T.);
#6771=FACE_OUTER_BOUND('',#8511,.T.);
#6772=FACE_OUTER_BOUND('',#8512,.T.);
#6773=FACE_OUTER_BOUND('',#8513,.T.);
#6774=FACE_OUTER_BOUND('',#8514,.T.);
#6775=FACE_OUTER_BOUND('',#8515,.T.);
#6776=FACE_OUTER_BOUND('',#8516,.T.);
#6777=FACE_OUTER_BOUND('',#8517,.T.);
#6778=FACE_OUTER_BOUND('',#8518,.T.);
#6779=FACE_OUTER_BOUND('',#8519,.T.);
#6780=FACE_OUTER_BOUND('',#8520,.T.);
#6781=FACE_OUTER_BOUND('',#8521,.T.);
#6782=FACE_OUTER_BOUND('',#8522,.T.);
#6783=FACE_OUTER_BOUND('',#8523,.T.);
#6784=FACE_OUTER_BOUND('',#8524,.T.);
#6785=FACE_OUTER_BOUND('',#8525,.T.);
#6786=FACE_OUTER_BOUND('',#8526,.T.);
#6787=FACE_OUTER_BOUND('',#8527,.T.);
#6788=FACE_OUTER_BOUND('',#8528,.T.);
#6789=FACE_OUTER_BOUND('',#8529,.T.);
#6790=FACE_OUTER_BOUND('',#8530,.T.);
#6791=FACE_OUTER_BOUND('',#8531,.T.);
#6792=FACE_OUTER_BOUND('',#8532,.T.);
#6793=FACE_OUTER_BOUND('',#8533,.T.);
#6794=FACE_OUTER_BOUND('',#8534,.T.);
#6795=FACE_OUTER_BOUND('',#8535,.T.);
#6796=FACE_OUTER_BOUND('',#8536,.T.);
#6797=FACE_OUTER_BOUND('',#8537,.T.);
#6798=FACE_OUTER_BOUND('',#8538,.T.);
#6799=FACE_OUTER_BOUND('',#8539,.T.);
#6800=FACE_OUTER_BOUND('',#8540,.T.);
#6801=FACE_OUTER_BOUND('',#8541,.T.);
#6802=FACE_OUTER_BOUND('',#8542,.T.);
#6803=FACE_OUTER_BOUND('',#8543,.T.);
#6804=FACE_OUTER_BOUND('',#8544,.T.);
#6805=FACE_OUTER_BOUND('',#8545,.T.);
#6806=FACE_OUTER_BOUND('',#8546,.T.);
#6807=FACE_OUTER_BOUND('',#8547,.T.);
#6808=FACE_OUTER_BOUND('',#8548,.T.);
#6809=FACE_OUTER_BOUND('',#8549,.T.);
#6810=FACE_OUTER_BOUND('',#8550,.T.);
#6811=FACE_OUTER_BOUND('',#8551,.T.);
#6812=FACE_OUTER_BOUND('',#8552,.T.);
#6813=FACE_OUTER_BOUND('',#8553,.T.);
#6814=FACE_OUTER_BOUND('',#8554,.T.);
#6815=FACE_OUTER_BOUND('',#8555,.T.);
#6816=FACE_OUTER_BOUND('',#8556,.T.);
#6817=FACE_OUTER_BOUND('',#8557,.T.);
#6818=FACE_OUTER_BOUND('',#8558,.T.);
#6819=FACE_OUTER_BOUND('',#8559,.T.);
#6820=FACE_OUTER_BOUND('',#8560,.T.);
#6821=FACE_OUTER_BOUND('',#8561,.T.);
#6822=FACE_OUTER_BOUND('',#8562,.T.);
#6823=FACE_OUTER_BOUND('',#8563,.T.);
#6824=FACE_OUTER_BOUND('',#8564,.T.);
#6825=FACE_OUTER_BOUND('',#8565,.T.);
#6826=FACE_OUTER_BOUND('',#8566,.T.);
#6827=FACE_OUTER_BOUND('',#8567,.T.);
#6828=FACE_OUTER_BOUND('',#8568,.T.);
#6829=FACE_OUTER_BOUND('',#8569,.T.);
#6830=FACE_OUTER_BOUND('',#8570,.T.);
#6831=FACE_OUTER_BOUND('',#8571,.T.);
#6832=FACE_OUTER_BOUND('',#8572,.T.);
#6833=FACE_OUTER_BOUND('',#8573,.T.);
#6834=FACE_OUTER_BOUND('',#8574,.T.);
#6835=FACE_OUTER_BOUND('',#8575,.T.);
#6836=FACE_OUTER_BOUND('',#8576,.T.);
#6837=FACE_OUTER_BOUND('',#8577,.T.);
#6838=FACE_OUTER_BOUND('',#8578,.T.);
#6839=FACE_OUTER_BOUND('',#8579,.T.);
#6840=FACE_OUTER_BOUND('',#8580,.T.);
#6841=FACE_OUTER_BOUND('',#8581,.T.);
#6842=FACE_OUTER_BOUND('',#8582,.T.);
#6843=FACE_OUTER_BOUND('',#8583,.T.);
#6844=FACE_OUTER_BOUND('',#8584,.T.);
#6845=FACE_OUTER_BOUND('',#8585,.T.);
#6846=FACE_OUTER_BOUND('',#8586,.T.);
#6847=FACE_OUTER_BOUND('',#8587,.T.);
#6848=FACE_OUTER_BOUND('',#8588,.T.);
#6849=FACE_OUTER_BOUND('',#8589,.T.);
#6850=FACE_OUTER_BOUND('',#8590,.T.);
#6851=FACE_OUTER_BOUND('',#8591,.T.);
#6852=FACE_OUTER_BOUND('',#8592,.T.);
#6853=FACE_OUTER_BOUND('',#8593,.T.);
#6854=FACE_OUTER_BOUND('',#8594,.T.);
#6855=FACE_OUTER_BOUND('',#8595,.T.);
#6856=FACE_OUTER_BOUND('',#8596,.T.);
#6857=FACE_OUTER_BOUND('',#8597,.T.);
#6858=FACE_OUTER_BOUND('',#8598,.T.);
#6859=FACE_OUTER_BOUND('',#8599,.T.);
#6860=FACE_OUTER_BOUND('',#8600,.T.);
#6861=EDGE_LOOP('',(#19577,#19578,#19579,#19580));
#6862=EDGE_LOOP('',(#19581,#19582,#19583,#19584));
#6863=EDGE_LOOP('',(#19585,#19586,#19587,#19588));
#6864=EDGE_LOOP('',(#19589,#19590,#19591));
#6865=EDGE_LOOP('',(#19592,#19593,#19594,#19595));
#6866=EDGE_LOOP('',(#19596,#19597,#19598));
#6867=EDGE_LOOP('',(#19599,#19600,#19601,#19602));
#6868=EDGE_LOOP('',(#19603,#19604,#19605,#19606));
#6869=EDGE_LOOP('',(#19607,#19608,#19609));
#6870=EDGE_LOOP('',(#19610,#19611,#19612,#19613));
#6871=EDGE_LOOP('',(#19614));
#6872=EDGE_LOOP('',(#19615,#19616,#19617,#19618,#19619,#19620,#19621,#19622,
#19623));
#6873=EDGE_LOOP('',(#19624));
#6874=EDGE_LOOP('',(#19625,#19626));
#6875=EDGE_LOOP('',(#19627,#19628));
#6876=EDGE_LOOP('',(#19629,#19630));
#6877=EDGE_LOOP('',(#19631,#19632,#19633,#19634));
#6878=EDGE_LOOP('',(#19635,#19636,#19637,#19638));
#6879=EDGE_LOOP('',(#19639,#19640,#19641,#19642));
#6880=EDGE_LOOP('',(#19643,#19644,#19645,#19646));
#6881=EDGE_LOOP('',(#19647,#19648,#19649,#19650));
#6882=EDGE_LOOP('',(#19651,#19652,#19653,#19654));
#6883=EDGE_LOOP('',(#19655,#19656,#19657,#19658));
#6884=EDGE_LOOP('',(#19659,#19660,#19661,#19662));
#6885=EDGE_LOOP('',(#19663,#19664,#19665,#19666));
#6886=EDGE_LOOP('',(#19667,#19668,#19669,#19670));
#6887=EDGE_LOOP('',(#19671,#19672,#19673,#19674));
#6888=EDGE_LOOP('',(#19675,#19676,#19677,#19678,#19679,#19680,#19681,#19682,
#19683,#19684,#19685,#19686,#19687,#19688,#19689,#19690,#19691,#19692));
#6889=EDGE_LOOP('',(#19693));
#6890=EDGE_LOOP('',(#19694));
#6891=EDGE_LOOP('',(#19695));
#6892=EDGE_LOOP('',(#19696,#19697,#19698,#19699));
#6893=EDGE_LOOP('',(#19700,#19701,#19702,#19703));
#6894=EDGE_LOOP('',(#19704,#19705,#19706,#19707));
#6895=EDGE_LOOP('',(#19708,#19709,#19710,#19711));
#6896=EDGE_LOOP('',(#19712,#19713,#19714,#19715));
#6897=EDGE_LOOP('',(#19716,#19717,#19718,#19719));
#6898=EDGE_LOOP('',(#19720,#19721,#19722,#19723));
#6899=EDGE_LOOP('',(#19724,#19725,#19726,#19727));
#6900=EDGE_LOOP('',(#19728,#19729,#19730,#19731));
#6901=EDGE_LOOP('',(#19732,#19733,#19734,#19735));
#6902=EDGE_LOOP('',(#19736,#19737,#19738,#19739,#19740,#19741,#19742,#19743,
#19744,#19745,#19746,#19747,#19748,#19749,#19750,#19751,#19752,#19753));
#6903=EDGE_LOOP('',(#19754));
#6904=EDGE_LOOP('',(#19755));
#6905=EDGE_LOOP('',(#19756));
#6906=EDGE_LOOP('',(#19757,#19758,#19759,#19760,#19761,#19762,#19763));
#6907=EDGE_LOOP('',(#19764,#19765,#19766,#19767));
#6908=EDGE_LOOP('',(#19768,#19769,#19770,#19771));
#6909=EDGE_LOOP('',(#19772,#19773,#19774,#19775));
#6910=EDGE_LOOP('',(#19776,#19777,#19778,#19779));
#6911=EDGE_LOOP('',(#19780,#19781,#19782,#19783));
#6912=EDGE_LOOP('',(#19784,#19785,#19786,#19787));
#6913=EDGE_LOOP('',(#19788,#19789,#19790,#19791));
#6914=EDGE_LOOP('',(#19792,#19793,#19794,#19795));
#6915=EDGE_LOOP('',(#19796,#19797,#19798,#19799));
#6916=EDGE_LOOP('',(#19800,#19801,#19802,#19803));
#6917=EDGE_LOOP('',(#19804,#19805,#19806,#19807));
#6918=EDGE_LOOP('',(#19808,#19809,#19810,#19811));
#6919=EDGE_LOOP('',(#19812,#19813,#19814,#19815));
#6920=EDGE_LOOP('',(#19816,#19817,#19818,#19819));
#6921=EDGE_LOOP('',(#19820,#19821,#19822,#19823));
#6922=EDGE_LOOP('',(#19824,#19825,#19826,#19827));
#6923=EDGE_LOOP('',(#19828,#19829,#19830,#19831));
#6924=EDGE_LOOP('',(#19832,#19833,#19834,#19835));
#6925=EDGE_LOOP('',(#19836,#19837,#19838,#19839));
#6926=EDGE_LOOP('',(#19840,#19841,#19842,#19843));
#6927=EDGE_LOOP('',(#19844,#19845,#19846,#19847));
#6928=EDGE_LOOP('',(#19848,#19849,#19850,#19851));
#6929=EDGE_LOOP('',(#19852,#19853,#19854,#19855));
#6930=EDGE_LOOP('',(#19856,#19857,#19858,#19859));
#6931=EDGE_LOOP('',(#19860,#19861,#19862,#19863));
#6932=EDGE_LOOP('',(#19864,#19865,#19866,#19867));
#6933=EDGE_LOOP('',(#19868,#19869,#19870,#19871));
#6934=EDGE_LOOP('',(#19872,#19873,#19874));
#6935=EDGE_LOOP('',(#19875,#19876,#19877));
#6936=EDGE_LOOP('',(#19878,#19879,#19880,#19881));
#6937=EDGE_LOOP('',(#19882,#19883,#19884,#19885));
#6938=EDGE_LOOP('',(#19886,#19887,#19888,#19889));
#6939=EDGE_LOOP('',(#19890,#19891,#19892,#19893));
#6940=EDGE_LOOP('',(#19894,#19895,#19896,#19897));
#6941=EDGE_LOOP('',(#19898,#19899,#19900,#19901));
#6942=EDGE_LOOP('',(#19902,#19903,#19904,#19905));
#6943=EDGE_LOOP('',(#19906,#19907,#19908,#19909));
#6944=EDGE_LOOP('',(#19910,#19911,#19912,#19913));
#6945=EDGE_LOOP('',(#19914,#19915,#19916,#19917));
#6946=EDGE_LOOP('',(#19918,#19919,#19920,#19921));
#6947=EDGE_LOOP('',(#19922,#19923,#19924,#19925));
#6948=EDGE_LOOP('',(#19926,#19927,#19928,#19929));
#6949=EDGE_LOOP('',(#19930,#19931,#19932,#19933));
#6950=EDGE_LOOP('',(#19934,#19935,#19936,#19937));
#6951=EDGE_LOOP('',(#19938,#19939,#19940,#19941));
#6952=EDGE_LOOP('',(#19942,#19943,#19944,#19945));
#6953=EDGE_LOOP('',(#19946,#19947,#19948,#19949));
#6954=EDGE_LOOP('',(#19950,#19951,#19952,#19953));
#6955=EDGE_LOOP('',(#19954,#19955,#19956,#19957));
#6956=EDGE_LOOP('',(#19958,#19959,#19960,#19961));
#6957=EDGE_LOOP('',(#19962,#19963,#19964,#19965));
#6958=EDGE_LOOP('',(#19966,#19967,#19968,#19969));
#6959=EDGE_LOOP('',(#19970,#19971,#19972,#19973));
#6960=EDGE_LOOP('',(#19974,#19975,#19976,#19977));
#6961=EDGE_LOOP('',(#19978,#19979,#19980,#19981));
#6962=EDGE_LOOP('',(#19982,#19983,#19984,#19985));
#6963=EDGE_LOOP('',(#19986,#19987,#19988,#19989));
#6964=EDGE_LOOP('',(#19990,#19991,#19992,#19993));
#6965=EDGE_LOOP('',(#19994,#19995,#19996));
#6966=EDGE_LOOP('',(#19997,#19998,#19999,#20000,#20001));
#6967=EDGE_LOOP('',(#20002,#20003,#20004,#20005));
#6968=EDGE_LOOP('',(#20006,#20007,#20008,#20009));
#6969=EDGE_LOOP('',(#20010,#20011,#20012,#20013));
#6970=EDGE_LOOP('',(#20014,#20015,#20016,#20017));
#6971=EDGE_LOOP('',(#20018,#20019,#20020,#20021));
#6972=EDGE_LOOP('',(#20022,#20023,#20024,#20025));
#6973=EDGE_LOOP('',(#20026,#20027,#20028,#20029));
#6974=EDGE_LOOP('',(#20030,#20031,#20032,#20033));
#6975=EDGE_LOOP('',(#20034,#20035,#20036,#20037));
#6976=EDGE_LOOP('',(#20038,#20039,#20040,#20041));
#6977=EDGE_LOOP('',(#20042,#20043,#20044,#20045));
#6978=EDGE_LOOP('',(#20046,#20047,#20048,#20049));
#6979=EDGE_LOOP('',(#20050,#20051,#20052,#20053));
#6980=EDGE_LOOP('',(#20054,#20055,#20056,#20057));
#6981=EDGE_LOOP('',(#20058,#20059,#20060,#20061));
#6982=EDGE_LOOP('',(#20062,#20063,#20064,#20065));
#6983=EDGE_LOOP('',(#20066,#20067,#20068,#20069,#20070,#20071,#20072,#20073,
#20074,#20075));
#6984=EDGE_LOOP('',(#20076,#20077,#20078,#20079));
#6985=EDGE_LOOP('',(#20080,#20081,#20082,#20083,#20084,#20085,#20086,#20087,
#20088,#20089,#20090,#20091,#20092,#20093,#20094,#20095,#20096,#20097,#20098,
#20099,#20100,#20101,#20102,#20103,#20104,#20105,#20106,#20107,#20108,#20109,
#20110,#20111,#20112,#20113,#20114,#20115,#20116,#20117,#20118,#20119,#20120,
#20121,#20122,#20123,#20124,#20125,#20126,#20127,#20128,#20129,#20130,#20131,
#20132,#20133,#20134,#20135,#20136,#20137,#20138,#20139,#20140,#20141,#20142,
#20143,#20144,#20145,#20146,#20147,#20148,#20149,#20150,#20151,#20152,#20153,
#20154,#20155,#20156,#20157,#20158,#20159,#20160,#20161,#20162,#20163,#20164,
#20165,#20166,#20167,#20168,#20169,#20170,#20171,#20172,#20173,#20174,#20175,
#20176,#20177,#20178,#20179,#20180,#20181,#20182,#20183,#20184,#20185,#20186,
#20187,#20188,#20189,#20190,#20191,#20192,#20193,#20194,#20195,#20196,#20197,
#20198,#20199,#20200,#20201,#20202,#20203,#20204,#20205,#20206,#20207,#20208,
#20209,#20210,#20211,#20212,#20213,#20214,#20215,#20216,#20217,#20218,#20219,
#20220,#20221,#20222,#20223,#20224,#20225,#20226,#20227,#20228,#20229,#20230,
#20231,#20232,#20233,#20234,#20235,#20236,#20237,#20238,#20239,#20240,#20241,
#20242,#20243,#20244,#20245,#20246,#20247,#20248,#20249,#20250,#20251,#20252,
#20253,#20254,#20255,#20256,#20257,#20258,#20259,#20260,#20261,#20262,#20263,
#20264,#20265,#20266,#20267,#20268,#20269,#20270,#20271,#20272,#20273,#20274,
#20275,#20276,#20277,#20278,#20279,#20280,#20281,#20282,#20283,#20284,#20285,
#20286,#20287,#20288,#20289,#20290,#20291,#20292,#20293,#20294,#20295,#20296,
#20297,#20298,#20299,#20300,#20301,#20302,#20303,#20304,#20305,#20306,#20307,
#20308,#20309,#20310,#20311,#20312,#20313,#20314,#20315,#20316,#20317,#20318,
#20319,#20320,#20321,#20322,#20323,#20324,#20325,#20326,#20327,#20328,#20329,
#20330,#20331,#20332,#20333,#20334,#20335,#20336,#20337,#20338,#20339,#20340,
#20341,#20342,#20343,#20344,#20345,#20346,#20347,#20348,#20349,#20350,#20351,
#20352,#20353,#20354,#20355,#20356,#20357,#20358,#20359,#20360,#20361,#20362,
#20363,#20364,#20365,#20366,#20367,#20368,#20369,#20370,#20371,#20372,#20373,
#20374,#20375,#20376,#20377,#20378,#20379,#20380,#20381,#20382,#20383,#20384,
#20385,#20386,#20387,#20388,#20389,#20390,#20391,#20392,#20393,#20394,#20395,
#20396,#20397,#20398,#20399,#20400,#20401,#20402,#20403));
#6986=EDGE_LOOP('',(#20404,#20405,#20406,#20407,#20408,#20409,#20410,#20411,
#20412,#20413,#20414,#20415,#20416,#20417,#20418,#20419,#20420,#20421,#20422,
#20423,#20424,#20425,#20426,#20427,#20428,#20429,#20430,#20431,#20432,#20433,
#20434,#20435,#20436,#20437,#20438,#20439,#20440,#20441,#20442,#20443,#20444,
#20445,#20446,#20447,#20448,#20449,#20450,#20451,#20452,#20453,#20454,#20455,
#20456,#20457,#20458,#20459,#20460,#20461,#20462,#20463,#20464,#20465,#20466,
#20467,#20468,#20469,#20470,#20471,#20472,#20473,#20474,#20475,#20476,#20477,
#20478,#20479,#20480,#20481,#20482,#20483,#20484,#20485,#20486,#20487,#20488,
#20489,#20490,#20491,#20492,#20493,#20494,#20495,#20496,#20497,#20498,#20499,
#20500,#20501,#20502,#20503,#20504,#20505,#20506,#20507,#20508,#20509,#20510,
#20511,#20512,#20513,#20514,#20515,#20516,#20517,#20518,#20519,#20520,#20521,
#20522,#20523,#20524,#20525,#20526,#20527,#20528,#20529,#20530,#20531,#20532,
#20533,#20534,#20535,#20536,#20537,#20538,#20539,#20540,#20541,#20542,#20543,
#20544,#20545,#20546,#20547,#20548,#20549,#20550,#20551,#20552,#20553,#20554,
#20555,#20556,#20557,#20558,#20559,#20560,#20561,#20562,#20563,#20564,#20565,
#20566,#20567,#20568,#20569,#20570,#20571,#20572,#20573,#20574,#20575,#20576,
#20577,#20578,#20579,#20580,#20581,#20582,#20583,#20584,#20585,#20586,#20587,
#20588,#20589,#20590,#20591,#20592,#20593,#20594,#20595,#20596,#20597,#20598,
#20599,#20600,#20601,#20602,#20603,#20604,#20605,#20606,#20607,#20608,#20609,
#20610,#20611,#20612,#20613,#20614,#20615,#20616,#20617,#20618,#20619,#20620,
#20621,#20622,#20623,#20624,#20625,#20626,#20627,#20628,#20629,#20630,#20631,
#20632,#20633,#20634,#20635,#20636,#20637,#20638,#20639,#20640,#20641,#20642,
#20643,#20644,#20645,#20646,#20647,#20648,#20649,#20650,#20651,#20652,#20653,
#20654,#20655,#20656,#20657,#20658,#20659,#20660,#20661,#20662,#20663,#20664,
#20665,#20666,#20667,#20668,#20669,#20670,#20671,#20672,#20673,#20674,#20675,
#20676,#20677,#20678,#20679,#20680,#20681,#20682,#20683,#20684,#20685,#20686,
#20687,#20688,#20689,#20690,#20691,#20692,#20693,#20694,#20695,#20696,#20697,
#20698,#20699,#20700,#20701,#20702,#20703,#20704,#20705,#20706,#20707,#20708,
#20709,#20710,#20711,#20712,#20713,#20714,#20715,#20716,#20717,#20718,#20719,
#20720,#20721,#20722,#20723,#20724,#20725,#20726,#20727,#20728));
#6987=EDGE_LOOP('',(#20729,#20730,#20731,#20732,#20733));
#6988=EDGE_LOOP('',(#20734,#20735,#20736,#20737));
#6989=EDGE_LOOP('',(#20738,#20739,#20740,#20741));
#6990=EDGE_LOOP('',(#20742,#20743,#20744,#20745));
#6991=EDGE_LOOP('',(#20746,#20747,#20748,#20749));
#6992=EDGE_LOOP('',(#20750,#20751,#20752,#20753));
#6993=EDGE_LOOP('',(#20754,#20755,#20756,#20757));
#6994=EDGE_LOOP('',(#20758,#20759,#20760,#20761));
#6995=EDGE_LOOP('',(#20762,#20763,#20764,#20765));
#6996=EDGE_LOOP('',(#20766,#20767,#20768,#20769));
#6997=EDGE_LOOP('',(#20770,#20771,#20772,#20773));
#6998=EDGE_LOOP('',(#20774,#20775,#20776,#20777));
#6999=EDGE_LOOP('',(#20778,#20779,#20780,#20781));
#7000=EDGE_LOOP('',(#20782,#20783,#20784,#20785));
#7001=EDGE_LOOP('',(#20786,#20787,#20788,#20789));
#7002=EDGE_LOOP('',(#20790,#20791,#20792,#20793));
#7003=EDGE_LOOP('',(#20794,#20795,#20796,#20797));
#7004=EDGE_LOOP('',(#20798,#20799,#20800,#20801));
#7005=EDGE_LOOP('',(#20802,#20803,#20804,#20805));
#7006=EDGE_LOOP('',(#20806,#20807,#20808,#20809));
#7007=EDGE_LOOP('',(#20810,#20811,#20812,#20813));
#7008=EDGE_LOOP('',(#20814,#20815,#20816,#20817));
#7009=EDGE_LOOP('',(#20818,#20819,#20820,#20821));
#7010=EDGE_LOOP('',(#20822,#20823,#20824,#20825));
#7011=EDGE_LOOP('',(#20826,#20827,#20828,#20829));
#7012=EDGE_LOOP('',(#20830,#20831,#20832,#20833));
#7013=EDGE_LOOP('',(#20834,#20835,#20836,#20837));
#7014=EDGE_LOOP('',(#20838,#20839,#20840,#20841));
#7015=EDGE_LOOP('',(#20842,#20843,#20844,#20845));
#7016=EDGE_LOOP('',(#20846,#20847,#20848,#20849));
#7017=EDGE_LOOP('',(#20850,#20851,#20852,#20853));
#7018=EDGE_LOOP('',(#20854,#20855,#20856,#20857));
#7019=EDGE_LOOP('',(#20858,#20859,#20860,#20861));
#7020=EDGE_LOOP('',(#20862,#20863,#20864,#20865));
#7021=EDGE_LOOP('',(#20866,#20867,#20868,#20869));
#7022=EDGE_LOOP('',(#20870,#20871,#20872,#20873));
#7023=EDGE_LOOP('',(#20874,#20875,#20876,#20877));
#7024=EDGE_LOOP('',(#20878,#20879,#20880,#20881));
#7025=EDGE_LOOP('',(#20882,#20883,#20884,#20885));
#7026=EDGE_LOOP('',(#20886,#20887,#20888,#20889));
#7027=EDGE_LOOP('',(#20890,#20891,#20892,#20893));
#7028=EDGE_LOOP('',(#20894,#20895,#20896,#20897));
#7029=EDGE_LOOP('',(#20898,#20899,#20900,#20901));
#7030=EDGE_LOOP('',(#20902,#20903,#20904,#20905));
#7031=EDGE_LOOP('',(#20906,#20907,#20908,#20909));
#7032=EDGE_LOOP('',(#20910,#20911,#20912,#20913));
#7033=EDGE_LOOP('',(#20914,#20915,#20916,#20917));
#7034=EDGE_LOOP('',(#20918,#20919,#20920,#20921));
#7035=EDGE_LOOP('',(#20922,#20923,#20924,#20925));
#7036=EDGE_LOOP('',(#20926,#20927,#20928,#20929));
#7037=EDGE_LOOP('',(#20930,#20931,#20932,#20933));
#7038=EDGE_LOOP('',(#20934,#20935,#20936,#20937));
#7039=EDGE_LOOP('',(#20938,#20939,#20940,#20941));
#7040=EDGE_LOOP('',(#20942,#20943,#20944,#20945));
#7041=EDGE_LOOP('',(#20946,#20947,#20948,#20949));
#7042=EDGE_LOOP('',(#20950,#20951,#20952,#20953));
#7043=EDGE_LOOP('',(#20954,#20955,#20956,#20957));
#7044=EDGE_LOOP('',(#20958,#20959,#20960,#20961));
#7045=EDGE_LOOP('',(#20962,#20963,#20964,#20965));
#7046=EDGE_LOOP('',(#20966,#20967,#20968,#20969));
#7047=EDGE_LOOP('',(#20970,#20971,#20972,#20973));
#7048=EDGE_LOOP('',(#20974,#20975,#20976,#20977));
#7049=EDGE_LOOP('',(#20978,#20979,#20980,#20981));
#7050=EDGE_LOOP('',(#20982,#20983,#20984,#20985));
#7051=EDGE_LOOP('',(#20986,#20987,#20988,#20989));
#7052=EDGE_LOOP('',(#20990,#20991,#20992,#20993));
#7053=EDGE_LOOP('',(#20994,#20995,#20996,#20997));
#7054=EDGE_LOOP('',(#20998,#20999,#21000,#21001));
#7055=EDGE_LOOP('',(#21002,#21003,#21004,#21005));
#7056=EDGE_LOOP('',(#21006,#21007,#21008,#21009));
#7057=EDGE_LOOP('',(#21010,#21011,#21012,#21013));
#7058=EDGE_LOOP('',(#21014,#21015,#21016,#21017));
#7059=EDGE_LOOP('',(#21018,#21019,#21020,#21021));
#7060=EDGE_LOOP('',(#21022,#21023,#21024,#21025));
#7061=EDGE_LOOP('',(#21026,#21027,#21028,#21029));
#7062=EDGE_LOOP('',(#21030,#21031,#21032,#21033));
#7063=EDGE_LOOP('',(#21034,#21035,#21036,#21037));
#7064=EDGE_LOOP('',(#21038,#21039,#21040,#21041));
#7065=EDGE_LOOP('',(#21042,#21043,#21044,#21045));
#7066=EDGE_LOOP('',(#21046,#21047,#21048,#21049));
#7067=EDGE_LOOP('',(#21050,#21051,#21052,#21053));
#7068=EDGE_LOOP('',(#21054,#21055,#21056,#21057));
#7069=EDGE_LOOP('',(#21058,#21059,#21060,#21061));
#7070=EDGE_LOOP('',(#21062,#21063,#21064,#21065));
#7071=EDGE_LOOP('',(#21066,#21067,#21068,#21069));
#7072=EDGE_LOOP('',(#21070,#21071,#21072,#21073));
#7073=EDGE_LOOP('',(#21074,#21075,#21076,#21077));
#7074=EDGE_LOOP('',(#21078,#21079,#21080,#21081));
#7075=EDGE_LOOP('',(#21082,#21083,#21084,#21085));
#7076=EDGE_LOOP('',(#21086,#21087,#21088,#21089));
#7077=EDGE_LOOP('',(#21090,#21091,#21092,#21093));
#7078=EDGE_LOOP('',(#21094,#21095,#21096,#21097));
#7079=EDGE_LOOP('',(#21098,#21099,#21100,#21101));
#7080=EDGE_LOOP('',(#21102,#21103,#21104,#21105));
#7081=EDGE_LOOP('',(#21106,#21107,#21108,#21109));
#7082=EDGE_LOOP('',(#21110,#21111,#21112,#21113));
#7083=EDGE_LOOP('',(#21114,#21115,#21116,#21117));
#7084=EDGE_LOOP('',(#21118,#21119,#21120,#21121));
#7085=EDGE_LOOP('',(#21122,#21123,#21124,#21125));
#7086=EDGE_LOOP('',(#21126,#21127,#21128,#21129));
#7087=EDGE_LOOP('',(#21130,#21131,#21132,#21133));
#7088=EDGE_LOOP('',(#21134,#21135,#21136,#21137));
#7089=EDGE_LOOP('',(#21138,#21139,#21140,#21141));
#7090=EDGE_LOOP('',(#21142,#21143,#21144,#21145));
#7091=EDGE_LOOP('',(#21146,#21147,#21148,#21149));
#7092=EDGE_LOOP('',(#21150,#21151,#21152,#21153));
#7093=EDGE_LOOP('',(#21154,#21155,#21156,#21157));
#7094=EDGE_LOOP('',(#21158,#21159,#21160,#21161));
#7095=EDGE_LOOP('',(#21162,#21163,#21164,#21165));
#7096=EDGE_LOOP('',(#21166,#21167,#21168,#21169));
#7097=EDGE_LOOP('',(#21170,#21171,#21172,#21173));
#7098=EDGE_LOOP('',(#21174,#21175,#21176,#21177));
#7099=EDGE_LOOP('',(#21178,#21179,#21180,#21181));
#7100=EDGE_LOOP('',(#21182,#21183,#21184,#21185));
#7101=EDGE_LOOP('',(#21186,#21187,#21188,#21189));
#7102=EDGE_LOOP('',(#21190,#21191,#21192,#21193));
#7103=EDGE_LOOP('',(#21194,#21195,#21196,#21197));
#7104=EDGE_LOOP('',(#21198,#21199,#21200,#21201));
#7105=EDGE_LOOP('',(#21202,#21203,#21204,#21205));
#7106=EDGE_LOOP('',(#21206,#21207,#21208,#21209));
#7107=EDGE_LOOP('',(#21210,#21211,#21212,#21213));
#7108=EDGE_LOOP('',(#21214,#21215,#21216,#21217));
#7109=EDGE_LOOP('',(#21218,#21219,#21220,#21221));
#7110=EDGE_LOOP('',(#21222,#21223,#21224,#21225));
#7111=EDGE_LOOP('',(#21226,#21227,#21228,#21229));
#7112=EDGE_LOOP('',(#21230,#21231,#21232,#21233));
#7113=EDGE_LOOP('',(#21234,#21235,#21236,#21237));
#7114=EDGE_LOOP('',(#21238,#21239,#21240,#21241));
#7115=EDGE_LOOP('',(#21242,#21243,#21244,#21245));
#7116=EDGE_LOOP('',(#21246,#21247,#21248,#21249));
#7117=EDGE_LOOP('',(#21250,#21251,#21252,#21253));
#7118=EDGE_LOOP('',(#21254,#21255,#21256,#21257));
#7119=EDGE_LOOP('',(#21258,#21259,#21260,#21261));
#7120=EDGE_LOOP('',(#21262,#21263,#21264,#21265));
#7121=EDGE_LOOP('',(#21266,#21267,#21268,#21269));
#7122=EDGE_LOOP('',(#21270,#21271,#21272,#21273));
#7123=EDGE_LOOP('',(#21274,#21275,#21276,#21277));
#7124=EDGE_LOOP('',(#21278,#21279,#21280,#21281));
#7125=EDGE_LOOP('',(#21282,#21283,#21284,#21285));
#7126=EDGE_LOOP('',(#21286,#21287,#21288,#21289));
#7127=EDGE_LOOP('',(#21290,#21291,#21292,#21293));
#7128=EDGE_LOOP('',(#21294,#21295,#21296,#21297));
#7129=EDGE_LOOP('',(#21298,#21299,#21300,#21301));
#7130=EDGE_LOOP('',(#21302,#21303,#21304,#21305));
#7131=EDGE_LOOP('',(#21306,#21307,#21308,#21309));
#7132=EDGE_LOOP('',(#21310,#21311,#21312,#21313));
#7133=EDGE_LOOP('',(#21314,#21315,#21316,#21317));
#7134=EDGE_LOOP('',(#21318,#21319,#21320,#21321));
#7135=EDGE_LOOP('',(#21322,#21323,#21324,#21325));
#7136=EDGE_LOOP('',(#21326,#21327,#21328,#21329));
#7137=EDGE_LOOP('',(#21330,#21331,#21332,#21333));
#7138=EDGE_LOOP('',(#21334,#21335,#21336,#21337));
#7139=EDGE_LOOP('',(#21338,#21339,#21340,#21341));
#7140=EDGE_LOOP('',(#21342,#21343,#21344,#21345));
#7141=EDGE_LOOP('',(#21346,#21347,#21348,#21349));
#7142=EDGE_LOOP('',(#21350,#21351,#21352,#21353));
#7143=EDGE_LOOP('',(#21354,#21355,#21356,#21357));
#7144=EDGE_LOOP('',(#21358,#21359,#21360,#21361));
#7145=EDGE_LOOP('',(#21362,#21363,#21364,#21365));
#7146=EDGE_LOOP('',(#21366,#21367,#21368,#21369));
#7147=EDGE_LOOP('',(#21370,#21371,#21372,#21373));
#7148=EDGE_LOOP('',(#21374,#21375,#21376,#21377));
#7149=EDGE_LOOP('',(#21378,#21379,#21380,#21381));
#7150=EDGE_LOOP('',(#21382,#21383,#21384,#21385));
#7151=EDGE_LOOP('',(#21386,#21387,#21388,#21389));
#7152=EDGE_LOOP('',(#21390,#21391,#21392,#21393));
#7153=EDGE_LOOP('',(#21394,#21395,#21396,#21397));
#7154=EDGE_LOOP('',(#21398,#21399,#21400,#21401));
#7155=EDGE_LOOP('',(#21402,#21403,#21404,#21405));
#7156=EDGE_LOOP('',(#21406,#21407,#21408,#21409));
#7157=EDGE_LOOP('',(#21410,#21411,#21412,#21413));
#7158=EDGE_LOOP('',(#21414,#21415,#21416,#21417));
#7159=EDGE_LOOP('',(#21418,#21419,#21420,#21421));
#7160=EDGE_LOOP('',(#21422,#21423,#21424,#21425));
#7161=EDGE_LOOP('',(#21426,#21427,#21428,#21429));
#7162=EDGE_LOOP('',(#21430,#21431,#21432,#21433));
#7163=EDGE_LOOP('',(#21434,#21435,#21436,#21437));
#7164=EDGE_LOOP('',(#21438,#21439,#21440,#21441));
#7165=EDGE_LOOP('',(#21442,#21443,#21444,#21445));
#7166=EDGE_LOOP('',(#21446,#21447,#21448,#21449));
#7167=EDGE_LOOP('',(#21450,#21451,#21452,#21453));
#7168=EDGE_LOOP('',(#21454,#21455,#21456,#21457));
#7169=EDGE_LOOP('',(#21458,#21459,#21460,#21461));
#7170=EDGE_LOOP('',(#21462,#21463,#21464,#21465));
#7171=EDGE_LOOP('',(#21466,#21467,#21468,#21469));
#7172=EDGE_LOOP('',(#21470,#21471,#21472,#21473));
#7173=EDGE_LOOP('',(#21474,#21475,#21476,#21477));
#7174=EDGE_LOOP('',(#21478,#21479,#21480,#21481));
#7175=EDGE_LOOP('',(#21482,#21483,#21484,#21485));
#7176=EDGE_LOOP('',(#21486,#21487,#21488,#21489));
#7177=EDGE_LOOP('',(#21490,#21491,#21492,#21493));
#7178=EDGE_LOOP('',(#21494,#21495,#21496,#21497));
#7179=EDGE_LOOP('',(#21498,#21499,#21500,#21501));
#7180=EDGE_LOOP('',(#21502,#21503,#21504,#21505));
#7181=EDGE_LOOP('',(#21506,#21507,#21508,#21509));
#7182=EDGE_LOOP('',(#21510,#21511,#21512,#21513));
#7183=EDGE_LOOP('',(#21514,#21515,#21516,#21517));
#7184=EDGE_LOOP('',(#21518,#21519,#21520,#21521));
#7185=EDGE_LOOP('',(#21522,#21523,#21524,#21525));
#7186=EDGE_LOOP('',(#21526,#21527,#21528,#21529));
#7187=EDGE_LOOP('',(#21530,#21531,#21532,#21533));
#7188=EDGE_LOOP('',(#21534,#21535,#21536,#21537));
#7189=EDGE_LOOP('',(#21538,#21539,#21540,#21541));
#7190=EDGE_LOOP('',(#21542,#21543,#21544,#21545));
#7191=EDGE_LOOP('',(#21546,#21547,#21548,#21549));
#7192=EDGE_LOOP('',(#21550,#21551,#21552,#21553));
#7193=EDGE_LOOP('',(#21554,#21555,#21556,#21557));
#7194=EDGE_LOOP('',(#21558,#21559,#21560,#21561));
#7195=EDGE_LOOP('',(#21562,#21563,#21564,#21565));
#7196=EDGE_LOOP('',(#21566,#21567,#21568,#21569));
#7197=EDGE_LOOP('',(#21570,#21571,#21572,#21573));
#7198=EDGE_LOOP('',(#21574,#21575,#21576,#21577));
#7199=EDGE_LOOP('',(#21578,#21579,#21580,#21581));
#7200=EDGE_LOOP('',(#21582,#21583,#21584,#21585));
#7201=EDGE_LOOP('',(#21586,#21587,#21588,#21589));
#7202=EDGE_LOOP('',(#21590,#21591,#21592,#21593));
#7203=EDGE_LOOP('',(#21594,#21595,#21596,#21597));
#7204=EDGE_LOOP('',(#21598,#21599,#21600,#21601));
#7205=EDGE_LOOP('',(#21602,#21603,#21604,#21605));
#7206=EDGE_LOOP('',(#21606,#21607,#21608,#21609));
#7207=EDGE_LOOP('',(#21610,#21611,#21612,#21613));
#7208=EDGE_LOOP('',(#21614,#21615,#21616,#21617));
#7209=EDGE_LOOP('',(#21618,#21619,#21620,#21621));
#7210=EDGE_LOOP('',(#21622,#21623,#21624,#21625));
#7211=EDGE_LOOP('',(#21626,#21627,#21628,#21629));
#7212=EDGE_LOOP('',(#21630,#21631,#21632,#21633));
#7213=EDGE_LOOP('',(#21634,#21635,#21636,#21637));
#7214=EDGE_LOOP('',(#21638,#21639,#21640,#21641));
#7215=EDGE_LOOP('',(#21642,#21643,#21644,#21645));
#7216=EDGE_LOOP('',(#21646,#21647,#21648,#21649));
#7217=EDGE_LOOP('',(#21650,#21651,#21652,#21653));
#7218=EDGE_LOOP('',(#21654,#21655,#21656,#21657));
#7219=EDGE_LOOP('',(#21658,#21659,#21660,#21661));
#7220=EDGE_LOOP('',(#21662,#21663,#21664,#21665));
#7221=EDGE_LOOP('',(#21666,#21667,#21668,#21669));
#7222=EDGE_LOOP('',(#21670,#21671,#21672,#21673));
#7223=EDGE_LOOP('',(#21674,#21675,#21676,#21677));
#7224=EDGE_LOOP('',(#21678,#21679,#21680,#21681));
#7225=EDGE_LOOP('',(#21682,#21683,#21684,#21685));
#7226=EDGE_LOOP('',(#21686,#21687,#21688,#21689));
#7227=EDGE_LOOP('',(#21690,#21691,#21692,#21693));
#7228=EDGE_LOOP('',(#21694,#21695,#21696));
#7229=EDGE_LOOP('',(#21697));
#7230=EDGE_LOOP('',(#21698));
#7231=EDGE_LOOP('',(#21699,#21700,#21701,#21702));
#7232=EDGE_LOOP('',(#21703,#21704,#21705,#21706));
#7233=EDGE_LOOP('',(#21707,#21708,#21709,#21710));
#7234=EDGE_LOOP('',(#21711));
#7235=EDGE_LOOP('',(#21712));
#7236=EDGE_LOOP('',(#21713,#21714,#21715,#21716,#21717,#21718));
#7237=EDGE_LOOP('',(#21719,#21720,#21721,#21722));
#7238=EDGE_LOOP('',(#21723,#21724,#21725,#21726));
#7239=EDGE_LOOP('',(#21727,#21728,#21729,#21730));
#7240=EDGE_LOOP('',(#21731,#21732,#21733,#21734,#21735));
#7241=EDGE_LOOP('',(#21736,#21737,#21738,#21739));
#7242=EDGE_LOOP('',(#21740,#21741,#21742,#21743));
#7243=EDGE_LOOP('',(#21744,#21745,#21746,#21747,#21748,#21749,#21750,#21751,
#21752,#21753,#21754,#21755,#21756,#21757,#21758,#21759,#21760,#21761,#21762,
#21763,#21764,#21765,#21766,#21767,#21768,#21769,#21770,#21771,#21772,#21773,
#21774,#21775,#21776,#21777,#21778,#21779,#21780,#21781,#21782,#21783,#21784,
#21785,#21786,#21787,#21788,#21789,#21790,#21791,#21792,#21793,#21794,#21795,
#21796,#21797,#21798,#21799,#21800,#21801,#21802,#21803,#21804,#21805));
#7244=EDGE_LOOP('',(#21806,#21807,#21808,#21809,#21810,#21811,#21812,#21813,
#21814,#21815,#21816,#21817,#21818,#21819,#21820,#21821,#21822,#21823,#21824,
#21825,#21826,#21827,#21828,#21829,#21830,#21831,#21832,#21833,#21834,#21835,
#21836,#21837,#21838,#21839,#21840,#21841,#21842,#21843,#21844,#21845,#21846,
#21847,#21848,#21849,#21850,#21851,#21852,#21853,#21854,#21855,#21856,#21857,
#21858,#21859,#21860,#21861,#21862,#21863,#21864,#21865,#21866));
#7245=EDGE_LOOP('',(#21867,#21868,#21869,#21870));
#7246=EDGE_LOOP('',(#21871,#21872,#21873,#21874,#21875,#21876));
#7247=EDGE_LOOP('',(#21877,#21878,#21879,#21880,#21881));
#7248=EDGE_LOOP('',(#21882,#21883,#21884,#21885,#21886,#21887));
#7249=EDGE_LOOP('',(#21888,#21889,#21890,#21891,#21892,#21893));
#7250=EDGE_LOOP('',(#21894,#21895,#21896,#21897));
#7251=EDGE_LOOP('',(#21898,#21899,#21900,#21901,#21902,#21903));
#7252=EDGE_LOOP('',(#21904,#21905,#21906,#21907,#21908,#21909));
#7253=EDGE_LOOP('',(#21910,#21911,#21912,#21913));
#7254=EDGE_LOOP('',(#21914,#21915,#21916,#21917,#21918,#21919));
#7255=EDGE_LOOP('',(#21920,#21921,#21922,#21923,#21924,#21925));
#7256=EDGE_LOOP('',(#21926,#21927,#21928,#21929));
#7257=EDGE_LOOP('',(#21930,#21931,#21932,#21933,#21934,#21935));
#7258=EDGE_LOOP('',(#21936,#21937,#21938,#21939,#21940,#21941));
#7259=EDGE_LOOP('',(#21942,#21943,#21944,#21945));
#7260=EDGE_LOOP('',(#21946,#21947,#21948,#21949,#21950,#21951));
#7261=EDGE_LOOP('',(#21952,#21953,#21954,#21955,#21956,#21957));
#7262=EDGE_LOOP('',(#21958,#21959,#21960,#21961));
#7263=EDGE_LOOP('',(#21962,#21963,#21964,#21965,#21966,#21967));
#7264=EDGE_LOOP('',(#21968,#21969,#21970,#21971,#21972,#21973));
#7265=EDGE_LOOP('',(#21974,#21975,#21976,#21977));
#7266=EDGE_LOOP('',(#21978,#21979,#21980,#21981,#21982,#21983));
#7267=EDGE_LOOP('',(#21984,#21985,#21986,#21987,#21988,#21989));
#7268=EDGE_LOOP('',(#21990,#21991,#21992,#21993,#21994,#21995));
#7269=EDGE_LOOP('',(#21996,#21997,#21998,#21999,#22000,#22001));
#7270=EDGE_LOOP('',(#22002,#22003,#22004,#22005,#22006,#22007));
#7271=EDGE_LOOP('',(#22008,#22009,#22010,#22011,#22012,#22013));
#7272=EDGE_LOOP('',(#22014,#22015,#22016,#22017,#22018,#22019));
#7273=EDGE_LOOP('',(#22020,#22021,#22022,#22023,#22024,#22025));
#7274=EDGE_LOOP('',(#22026,#22027,#22028,#22029,#22030,#22031));
#7275=EDGE_LOOP('',(#22032,#22033,#22034,#22035,#22036,#22037));
#7276=EDGE_LOOP('',(#22038,#22039,#22040,#22041,#22042,#22043));
#7277=EDGE_LOOP('',(#22044,#22045,#22046,#22047,#22048,#22049));
#7278=EDGE_LOOP('',(#22050,#22051,#22052,#22053,#22054,#22055));
#7279=EDGE_LOOP('',(#22056,#22057,#22058,#22059,#22060,#22061));
#7280=EDGE_LOOP('',(#22062,#22063,#22064,#22065,#22066,#22067));
#7281=EDGE_LOOP('',(#22068,#22069,#22070,#22071,#22072,#22073));
#7282=EDGE_LOOP('',(#22074,#22075,#22076,#22077,#22078,#22079));
#7283=EDGE_LOOP('',(#22080,#22081,#22082,#22083,#22084,#22085));
#7284=EDGE_LOOP('',(#22086,#22087,#22088,#22089,#22090,#22091));
#7285=EDGE_LOOP('',(#22092,#22093,#22094,#22095,#22096,#22097));
#7286=EDGE_LOOP('',(#22098,#22099,#22100,#22101));
#7287=EDGE_LOOP('',(#22102,#22103,#22104,#22105,#22106,#22107));
#7288=EDGE_LOOP('',(#22108,#22109,#22110,#22111,#22112,#22113));
#7289=EDGE_LOOP('',(#22114,#22115,#22116,#22117));
#7290=EDGE_LOOP('',(#22118,#22119,#22120,#22121,#22122,#22123));
#7291=EDGE_LOOP('',(#22124,#22125,#22126,#22127,#22128,#22129));
#7292=EDGE_LOOP('',(#22130,#22131,#22132,#22133));
#7293=EDGE_LOOP('',(#22134,#22135,#22136,#22137,#22138,#22139));
#7294=EDGE_LOOP('',(#22140,#22141,#22142,#22143,#22144,#22145));
#7295=EDGE_LOOP('',(#22146,#22147,#22148,#22149));
#7296=EDGE_LOOP('',(#22150,#22151,#22152,#22153,#22154,#22155));
#7297=EDGE_LOOP('',(#22156,#22157,#22158,#22159,#22160,#22161));
#7298=EDGE_LOOP('',(#22162,#22163,#22164,#22165));
#7299=EDGE_LOOP('',(#22166,#22167,#22168,#22169,#22170,#22171));
#7300=EDGE_LOOP('',(#22172,#22173,#22174,#22175,#22176,#22177));
#7301=EDGE_LOOP('',(#22178,#22179,#22180,#22181));
#7302=EDGE_LOOP('',(#22182,#22183,#22184,#22185,#22186,#22187));
#7303=EDGE_LOOP('',(#22188,#22189,#22190,#22191,#22192,#22193));
#7304=EDGE_LOOP('',(#22194,#22195,#22196,#22197));
#7305=EDGE_LOOP('',(#22198,#22199,#22200,#22201,#22202,#22203));
#7306=EDGE_LOOP('',(#22204,#22205,#22206,#22207,#22208,#22209));
#7307=EDGE_LOOP('',(#22210,#22211,#22212,#22213));
#7308=EDGE_LOOP('',(#22214,#22215,#22216,#22217,#22218,#22219));
#7309=EDGE_LOOP('',(#22220,#22221,#22222,#22223,#22224,#22225));
#7310=EDGE_LOOP('',(#22226,#22227,#22228,#22229));
#7311=EDGE_LOOP('',(#22230,#22231,#22232,#22233,#22234,#22235));
#7312=EDGE_LOOP('',(#22236,#22237,#22238,#22239,#22240,#22241));
#7313=EDGE_LOOP('',(#22242,#22243,#22244,#22245));
#7314=EDGE_LOOP('',(#22246,#22247,#22248,#22249,#22250,#22251));
#7315=EDGE_LOOP('',(#22252,#22253,#22254,#22255,#22256,#22257));
#7316=EDGE_LOOP('',(#22258,#22259,#22260,#22261));
#7317=EDGE_LOOP('',(#22262,#22263,#22264,#22265,#22266,#22267));
#7318=EDGE_LOOP('',(#22268,#22269,#22270,#22271,#22272,#22273));
#7319=EDGE_LOOP('',(#22274,#22275,#22276,#22277));
#7320=EDGE_LOOP('',(#22278,#22279,#22280,#22281,#22282,#22283));
#7321=EDGE_LOOP('',(#22284,#22285,#22286,#22287,#22288,#22289));
#7322=EDGE_LOOP('',(#22290,#22291,#22292,#22293));
#7323=EDGE_LOOP('',(#22294,#22295,#22296,#22297,#22298,#22299));
#7324=EDGE_LOOP('',(#22300,#22301,#22302,#22303,#22304,#22305));
#7325=EDGE_LOOP('',(#22306,#22307,#22308,#22309));
#7326=EDGE_LOOP('',(#22310,#22311,#22312,#22313,#22314,#22315));
#7327=EDGE_LOOP('',(#22316,#22317,#22318,#22319,#22320,#22321));
#7328=EDGE_LOOP('',(#22322,#22323,#22324,#22325));
#7329=EDGE_LOOP('',(#22326,#22327,#22328,#22329,#22330,#22331));
#7330=EDGE_LOOP('',(#22332,#22333,#22334,#22335,#22336,#22337));
#7331=EDGE_LOOP('',(#22338,#22339,#22340,#22341));
#7332=EDGE_LOOP('',(#22342,#22343,#22344,#22345,#22346,#22347));
#7333=EDGE_LOOP('',(#22348,#22349,#22350,#22351,#22352,#22353));
#7334=EDGE_LOOP('',(#22354,#22355,#22356,#22357));
#7335=EDGE_LOOP('',(#22358,#22359,#22360,#22361,#22362,#22363));
#7336=EDGE_LOOP('',(#22364,#22365,#22366,#22367,#22368,#22369));
#7337=EDGE_LOOP('',(#22370,#22371,#22372,#22373));
#7338=EDGE_LOOP('',(#22374,#22375,#22376,#22377,#22378,#22379));
#7339=EDGE_LOOP('',(#22380,#22381,#22382,#22383,#22384,#22385));
#7340=EDGE_LOOP('',(#22386,#22387,#22388,#22389));
#7341=EDGE_LOOP('',(#22390,#22391,#22392,#22393,#22394,#22395));
#7342=EDGE_LOOP('',(#22396,#22397,#22398,#22399,#22400,#22401));
#7343=EDGE_LOOP('',(#22402,#22403,#22404,#22405));
#7344=EDGE_LOOP('',(#22406,#22407,#22408,#22409,#22410,#22411));
#7345=EDGE_LOOP('',(#22412,#22413,#22414,#22415,#22416,#22417));
#7346=EDGE_LOOP('',(#22418,#22419,#22420,#22421));
#7347=EDGE_LOOP('',(#22422,#22423,#22424,#22425,#22426,#22427));
#7348=EDGE_LOOP('',(#22428,#22429,#22430,#22431,#22432,#22433));
#7349=EDGE_LOOP('',(#22434,#22435,#22436,#22437));
#7350=EDGE_LOOP('',(#22438,#22439,#22440,#22441,#22442,#22443));
#7351=EDGE_LOOP('',(#22444,#22445,#22446,#22447,#22448,#22449));
#7352=EDGE_LOOP('',(#22450,#22451,#22452,#22453));
#7353=EDGE_LOOP('',(#22454,#22455,#22456,#22457,#22458,#22459));
#7354=EDGE_LOOP('',(#22460,#22461,#22462,#22463,#22464,#22465));
#7355=EDGE_LOOP('',(#22466,#22467,#22468,#22469));
#7356=EDGE_LOOP('',(#22470,#22471,#22472,#22473,#22474,#22475));
#7357=EDGE_LOOP('',(#22476,#22477,#22478,#22479,#22480,#22481));
#7358=EDGE_LOOP('',(#22482,#22483,#22484,#22485));
#7359=EDGE_LOOP('',(#22486,#22487,#22488,#22489,#22490,#22491));
#7360=EDGE_LOOP('',(#22492,#22493,#22494,#22495,#22496,#22497));
#7361=EDGE_LOOP('',(#22498,#22499,#22500,#22501));
#7362=EDGE_LOOP('',(#22502,#22503,#22504,#22505,#22506,#22507));
#7363=EDGE_LOOP('',(#22508,#22509,#22510,#22511,#22512,#22513));
#7364=EDGE_LOOP('',(#22514,#22515,#22516,#22517));
#7365=EDGE_LOOP('',(#22518,#22519,#22520,#22521,#22522,#22523));
#7366=EDGE_LOOP('',(#22524,#22525,#22526,#22527,#22528,#22529));
#7367=EDGE_LOOP('',(#22530,#22531,#22532,#22533));
#7368=EDGE_LOOP('',(#22534,#22535,#22536,#22537,#22538,#22539));
#7369=EDGE_LOOP('',(#22540,#22541,#22542,#22543,#22544,#22545));
#7370=EDGE_LOOP('',(#22546,#22547,#22548,#22549));
#7371=EDGE_LOOP('',(#22550,#22551,#22552,#22553,#22554,#22555));
#7372=EDGE_LOOP('',(#22556,#22557,#22558,#22559,#22560,#22561));
#7373=EDGE_LOOP('',(#22562,#22563,#22564,#22565));
#7374=EDGE_LOOP('',(#22566,#22567,#22568,#22569,#22570,#22571));
#7375=EDGE_LOOP('',(#22572,#22573,#22574,#22575,#22576,#22577));
#7376=EDGE_LOOP('',(#22578,#22579,#22580,#22581));
#7377=EDGE_LOOP('',(#22582,#22583,#22584,#22585,#22586,#22587));
#7378=EDGE_LOOP('',(#22588,#22589,#22590,#22591,#22592,#22593));
#7379=EDGE_LOOP('',(#22594,#22595,#22596,#22597));
#7380=EDGE_LOOP('',(#22598,#22599,#22600,#22601,#22602,#22603));
#7381=EDGE_LOOP('',(#22604,#22605,#22606,#22607,#22608,#22609));
#7382=EDGE_LOOP('',(#22610,#22611,#22612,#22613));
#7383=EDGE_LOOP('',(#22614,#22615,#22616,#22617,#22618,#22619));
#7384=EDGE_LOOP('',(#22620,#22621,#22622,#22623,#22624,#22625));
#7385=EDGE_LOOP('',(#22626,#22627,#22628,#22629));
#7386=EDGE_LOOP('',(#22630,#22631,#22632,#22633,#22634,#22635));
#7387=EDGE_LOOP('',(#22636,#22637,#22638,#22639,#22640,#22641));
#7388=EDGE_LOOP('',(#22642,#22643,#22644,#22645));
#7389=EDGE_LOOP('',(#22646,#22647,#22648,#22649,#22650,#22651));
#7390=EDGE_LOOP('',(#22652,#22653,#22654,#22655,#22656,#22657));
#7391=EDGE_LOOP('',(#22658,#22659,#22660,#22661));
#7392=EDGE_LOOP('',(#22662,#22663,#22664,#22665,#22666,#22667));
#7393=EDGE_LOOP('',(#22668,#22669,#22670,#22671,#22672,#22673));
#7394=EDGE_LOOP('',(#22674,#22675,#22676,#22677));
#7395=EDGE_LOOP('',(#22678,#22679,#22680,#22681,#22682,#22683));
#7396=EDGE_LOOP('',(#22684,#22685,#22686,#22687,#22688,#22689));
#7397=EDGE_LOOP('',(#22690,#22691,#22692,#22693));
#7398=EDGE_LOOP('',(#22694,#22695,#22696,#22697,#22698,#22699));
#7399=EDGE_LOOP('',(#22700,#22701,#22702,#22703,#22704,#22705));
#7400=EDGE_LOOP('',(#22706,#22707,#22708,#22709,#22710));
#7401=EDGE_LOOP('',(#22711,#22712,#22713,#22714,#22715,#22716));
#7402=EDGE_LOOP('',(#22717,#22718,#22719,#22720,#22721,#22722));
#7403=EDGE_LOOP('',(#22723,#22724,#22725,#22726));
#7404=EDGE_LOOP('',(#22727,#22728,#22729,#22730,#22731,#22732));
#7405=EDGE_LOOP('',(#22733,#22734,#22735,#22736,#22737,#22738));
#7406=EDGE_LOOP('',(#22739,#22740,#22741,#22742));
#7407=EDGE_LOOP('',(#22743,#22744,#22745,#22746,#22747,#22748));
#7408=EDGE_LOOP('',(#22749,#22750,#22751,#22752,#22753,#22754));
#7409=EDGE_LOOP('',(#22755,#22756,#22757,#22758));
#7410=EDGE_LOOP('',(#22759,#22760,#22761,#22762,#22763,#22764));
#7411=EDGE_LOOP('',(#22765,#22766,#22767,#22768,#22769,#22770));
#7412=EDGE_LOOP('',(#22771,#22772,#22773,#22774));
#7413=EDGE_LOOP('',(#22775,#22776,#22777,#22778,#22779,#22780));
#7414=EDGE_LOOP('',(#22781,#22782,#22783,#22784,#22785,#22786));
#7415=EDGE_LOOP('',(#22787,#22788,#22789,#22790));
#7416=EDGE_LOOP('',(#22791,#22792,#22793,#22794,#22795,#22796));
#7417=EDGE_LOOP('',(#22797,#22798,#22799,#22800,#22801,#22802));
#7418=EDGE_LOOP('',(#22803,#22804,#22805,#22806));
#7419=EDGE_LOOP('',(#22807,#22808,#22809,#22810,#22811,#22812));
#7420=EDGE_LOOP('',(#22813,#22814,#22815,#22816,#22817,#22818));
#7421=EDGE_LOOP('',(#22819,#22820,#22821,#22822));
#7422=EDGE_LOOP('',(#22823,#22824,#22825,#22826,#22827,#22828));
#7423=EDGE_LOOP('',(#22829,#22830,#22831,#22832,#22833,#22834));
#7424=EDGE_LOOP('',(#22835,#22836,#22837,#22838));
#7425=EDGE_LOOP('',(#22839,#22840,#22841,#22842,#22843,#22844));
#7426=EDGE_LOOP('',(#22845,#22846,#22847,#22848,#22849,#22850));
#7427=EDGE_LOOP('',(#22851,#22852,#22853,#22854));
#7428=EDGE_LOOP('',(#22855,#22856,#22857,#22858,#22859,#22860));
#7429=EDGE_LOOP('',(#22861,#22862,#22863,#22864,#22865,#22866));
#7430=EDGE_LOOP('',(#22867,#22868,#22869,#22870));
#7431=EDGE_LOOP('',(#22871,#22872,#22873,#22874,#22875,#22876));
#7432=EDGE_LOOP('',(#22877,#22878,#22879,#22880,#22881,#22882));
#7433=EDGE_LOOP('',(#22883,#22884,#22885,#22886));
#7434=EDGE_LOOP('',(#22887,#22888,#22889,#22890,#22891,#22892));
#7435=EDGE_LOOP('',(#22893,#22894,#22895,#22896,#22897,#22898));
#7436=EDGE_LOOP('',(#22899,#22900,#22901,#22902));
#7437=EDGE_LOOP('',(#22903,#22904,#22905,#22906,#22907,#22908));
#7438=EDGE_LOOP('',(#22909,#22910,#22911,#22912,#22913,#22914));
#7439=EDGE_LOOP('',(#22915,#22916,#22917,#22918));
#7440=EDGE_LOOP('',(#22919,#22920,#22921,#22922,#22923,#22924));
#7441=EDGE_LOOP('',(#22925,#22926,#22927,#22928,#22929,#22930));
#7442=EDGE_LOOP('',(#22931,#22932,#22933,#22934));
#7443=EDGE_LOOP('',(#22935,#22936,#22937,#22938,#22939,#22940));
#7444=EDGE_LOOP('',(#22941,#22942,#22943,#22944,#22945,#22946));
#7445=EDGE_LOOP('',(#22947,#22948,#22949,#22950));
#7446=EDGE_LOOP('',(#22951,#22952,#22953,#22954,#22955,#22956));
#7447=EDGE_LOOP('',(#22957,#22958,#22959,#22960,#22961,#22962));
#7448=EDGE_LOOP('',(#22963,#22964,#22965,#22966));
#7449=EDGE_LOOP('',(#22967,#22968,#22969,#22970,#22971,#22972));
#7450=EDGE_LOOP('',(#22973,#22974,#22975,#22976,#22977,#22978));
#7451=EDGE_LOOP('',(#22979,#22980,#22981,#22982));
#7452=EDGE_LOOP('',(#22983,#22984,#22985,#22986,#22987,#22988));
#7453=EDGE_LOOP('',(#22989,#22990,#22991,#22992,#22993,#22994));
#7454=EDGE_LOOP('',(#22995,#22996,#22997,#22998));
#7455=EDGE_LOOP('',(#22999,#23000,#23001,#23002,#23003,#23004));
#7456=EDGE_LOOP('',(#23005,#23006,#23007,#23008,#23009,#23010));
#7457=EDGE_LOOP('',(#23011,#23012,#23013,#23014));
#7458=EDGE_LOOP('',(#23015,#23016,#23017,#23018,#23019,#23020));
#7459=EDGE_LOOP('',(#23021,#23022,#23023,#23024,#23025,#23026));
#7460=EDGE_LOOP('',(#23027,#23028,#23029,#23030,#23031,#23032));
#7461=EDGE_LOOP('',(#23033,#23034,#23035,#23036,#23037,#23038));
#7462=EDGE_LOOP('',(#23039,#23040,#23041,#23042,#23043,#23044));
#7463=EDGE_LOOP('',(#23045,#23046,#23047,#23048,#23049,#23050));
#7464=EDGE_LOOP('',(#23051,#23052,#23053,#23054,#23055,#23056));
#7465=EDGE_LOOP('',(#23057,#23058,#23059,#23060,#23061,#23062));
#7466=EDGE_LOOP('',(#23063,#23064,#23065,#23066,#23067,#23068));
#7467=EDGE_LOOP('',(#23069,#23070,#23071,#23072,#23073,#23074));
#7468=EDGE_LOOP('',(#23075,#23076,#23077,#23078,#23079,#23080));
#7469=EDGE_LOOP('',(#23081,#23082,#23083,#23084,#23085,#23086));
#7470=EDGE_LOOP('',(#23087,#23088,#23089,#23090,#23091,#23092));
#7471=EDGE_LOOP('',(#23093,#23094,#23095,#23096,#23097,#23098,#23099));
#7472=EDGE_LOOP('',(#23100,#23101,#23102,#23103));
#7473=EDGE_LOOP('',(#23104,#23105,#23106,#23107));
#7474=EDGE_LOOP('',(#23108,#23109,#23110,#23111));
#7475=EDGE_LOOP('',(#23112,#23113,#23114,#23115));
#7476=EDGE_LOOP('',(#23116,#23117,#23118,#23119));
#7477=EDGE_LOOP('',(#23120,#23121,#23122,#23123));
#7478=EDGE_LOOP('',(#23124,#23125,#23126,#23127));
#7479=EDGE_LOOP('',(#23128,#23129,#23130,#23131));
#7480=EDGE_LOOP('',(#23132,#23133,#23134,#23135));
#7481=EDGE_LOOP('',(#23136,#23137,#23138,#23139));
#7482=EDGE_LOOP('',(#23140,#23141,#23142,#23143));
#7483=EDGE_LOOP('',(#23144,#23145,#23146,#23147));
#7484=EDGE_LOOP('',(#23148,#23149,#23150,#23151));
#7485=EDGE_LOOP('',(#23152,#23153,#23154,#23155));
#7486=EDGE_LOOP('',(#23156,#23157,#23158,#23159));
#7487=EDGE_LOOP('',(#23160,#23161,#23162,#23163));
#7488=EDGE_LOOP('',(#23164,#23165,#23166,#23167));
#7489=EDGE_LOOP('',(#23168,#23169,#23170,#23171));
#7490=EDGE_LOOP('',(#23172,#23173,#23174,#23175));
#7491=EDGE_LOOP('',(#23176,#23177,#23178,#23179));
#7492=EDGE_LOOP('',(#23180,#23181,#23182,#23183));
#7493=EDGE_LOOP('',(#23184,#23185,#23186,#23187));
#7494=EDGE_LOOP('',(#23188,#23189,#23190,#23191));
#7495=EDGE_LOOP('',(#23192,#23193,#23194,#23195));
#7496=EDGE_LOOP('',(#23196,#23197,#23198,#23199));
#7497=EDGE_LOOP('',(#23200,#23201,#23202,#23203));
#7498=EDGE_LOOP('',(#23204,#23205,#23206,#23207));
#7499=EDGE_LOOP('',(#23208,#23209,#23210));
#7500=EDGE_LOOP('',(#23211,#23212,#23213));
#7501=EDGE_LOOP('',(#23214,#23215,#23216,#23217));
#7502=EDGE_LOOP('',(#23218,#23219,#23220,#23221));
#7503=EDGE_LOOP('',(#23222,#23223,#23224,#23225));
#7504=EDGE_LOOP('',(#23226,#23227,#23228,#23229));
#7505=EDGE_LOOP('',(#23230,#23231,#23232,#23233));
#7506=EDGE_LOOP('',(#23234,#23235,#23236,#23237));
#7507=EDGE_LOOP('',(#23238,#23239,#23240,#23241));
#7508=EDGE_LOOP('',(#23242,#23243,#23244,#23245));
#7509=EDGE_LOOP('',(#23246,#23247,#23248,#23249));
#7510=EDGE_LOOP('',(#23250,#23251,#23252,#23253));
#7511=EDGE_LOOP('',(#23254,#23255,#23256,#23257));
#7512=EDGE_LOOP('',(#23258,#23259,#23260,#23261));
#7513=EDGE_LOOP('',(#23262,#23263,#23264,#23265));
#7514=EDGE_LOOP('',(#23266,#23267,#23268,#23269));
#7515=EDGE_LOOP('',(#23270,#23271,#23272,#23273));
#7516=EDGE_LOOP('',(#23274,#23275,#23276,#23277));
#7517=EDGE_LOOP('',(#23278,#23279,#23280,#23281));
#7518=EDGE_LOOP('',(#23282,#23283,#23284,#23285));
#7519=EDGE_LOOP('',(#23286,#23287,#23288,#23289));
#7520=EDGE_LOOP('',(#23290,#23291,#23292,#23293));
#7521=EDGE_LOOP('',(#23294,#23295,#23296,#23297));
#7522=EDGE_LOOP('',(#23298,#23299,#23300,#23301));
#7523=EDGE_LOOP('',(#23302,#23303,#23304,#23305));
#7524=EDGE_LOOP('',(#23306,#23307,#23308,#23309));
#7525=EDGE_LOOP('',(#23310,#23311,#23312,#23313));
#7526=EDGE_LOOP('',(#23314,#23315,#23316,#23317));
#7527=EDGE_LOOP('',(#23318,#23319,#23320,#23321));
#7528=EDGE_LOOP('',(#23322,#23323,#23324,#23325));
#7529=EDGE_LOOP('',(#23326,#23327,#23328,#23329));
#7530=EDGE_LOOP('',(#23330,#23331,#23332));
#7531=EDGE_LOOP('',(#23333,#23334,#23335,#23336,#23337));
#7532=EDGE_LOOP('',(#23338,#23339,#23340,#23341));
#7533=EDGE_LOOP('',(#23342,#23343,#23344,#23345));
#7534=EDGE_LOOP('',(#23346,#23347,#23348,#23349));
#7535=EDGE_LOOP('',(#23350,#23351,#23352,#23353));
#7536=EDGE_LOOP('',(#23354,#23355,#23356,#23357));
#7537=EDGE_LOOP('',(#23358,#23359,#23360,#23361));
#7538=EDGE_LOOP('',(#23362,#23363,#23364,#23365));
#7539=EDGE_LOOP('',(#23366,#23367,#23368,#23369));
#7540=EDGE_LOOP('',(#23370,#23371,#23372,#23373));
#7541=EDGE_LOOP('',(#23374,#23375,#23376,#23377));
#7542=EDGE_LOOP('',(#23378,#23379,#23380,#23381));
#7543=EDGE_LOOP('',(#23382,#23383,#23384,#23385));
#7544=EDGE_LOOP('',(#23386,#23387,#23388,#23389));
#7545=EDGE_LOOP('',(#23390,#23391,#23392,#23393));
#7546=EDGE_LOOP('',(#23394,#23395,#23396,#23397));
#7547=EDGE_LOOP('',(#23398,#23399,#23400,#23401));
#7548=EDGE_LOOP('',(#23402,#23403,#23404,#23405,#23406,#23407,#23408,#23409,
#23410,#23411));
#7549=EDGE_LOOP('',(#23412,#23413,#23414,#23415));
#7550=EDGE_LOOP('',(#23416,#23417,#23418,#23419,#23420,#23421,#23422,#23423,
#23424,#23425,#23426,#23427,#23428,#23429,#23430,#23431,#23432,#23433,#23434,
#23435,#23436,#23437,#23438,#23439,#23440,#23441,#23442,#23443,#23444,#23445,
#23446,#23447,#23448,#23449,#23450,#23451,#23452,#23453,#23454,#23455,#23456,
#23457,#23458,#23459,#23460,#23461,#23462,#23463,#23464,#23465,#23466,#23467,
#23468,#23469,#23470,#23471,#23472,#23473,#23474,#23475,#23476,#23477,#23478,
#23479,#23480,#23481,#23482,#23483,#23484,#23485,#23486,#23487,#23488,#23489,
#23490,#23491,#23492,#23493,#23494,#23495,#23496,#23497,#23498,#23499,#23500,
#23501,#23502,#23503,#23504,#23505,#23506,#23507,#23508,#23509,#23510,#23511,
#23512,#23513,#23514,#23515,#23516,#23517,#23518,#23519,#23520,#23521,#23522,
#23523,#23524,#23525,#23526,#23527,#23528,#23529,#23530,#23531,#23532,#23533,
#23534,#23535,#23536,#23537,#23538,#23539,#23540,#23541,#23542,#23543,#23544,
#23545,#23546,#23547,#23548,#23549,#23550,#23551,#23552,#23553,#23554,#23555,
#23556,#23557,#23558,#23559,#23560,#23561,#23562,#23563,#23564,#23565,#23566,
#23567,#23568,#23569,#23570,#23571,#23572,#23573,#23574,#23575,#23576,#23577,
#23578,#23579,#23580,#23581,#23582,#23583,#23584,#23585,#23586,#23587,#23588,
#23589,#23590,#23591,#23592,#23593,#23594,#23595,#23596,#23597,#23598,#23599,
#23600,#23601,#23602,#23603,#23604,#23605,#23606,#23607,#23608,#23609,#23610,
#23611,#23612,#23613,#23614,#23615,#23616,#23617,#23618,#23619,#23620,#23621,
#23622,#23623,#23624,#23625,#23626,#23627,#23628,#23629,#23630,#23631,#23632,
#23633,#23634,#23635,#23636,#23637,#23638,#23639,#23640,#23641,#23642,#23643,
#23644,#23645,#23646,#23647,#23648,#23649,#23650,#23651,#23652,#23653,#23654,
#23655,#23656,#23657,#23658,#23659,#23660,#23661,#23662,#23663,#23664,#23665,
#23666,#23667,#23668,#23669,#23670,#23671,#23672,#23673,#23674,#23675,#23676,
#23677,#23678,#23679,#23680,#23681,#23682,#23683,#23684,#23685,#23686,#23687,
#23688,#23689,#23690,#23691,#23692,#23693,#23694,#23695,#23696,#23697,#23698,
#23699,#23700,#23701,#23702,#23703,#23704,#23705,#23706,#23707,#23708,#23709,
#23710,#23711,#23712,#23713,#23714,#23715,#23716,#23717,#23718,#23719,#23720,
#23721,#23722,#23723,#23724,#23725,#23726,#23727,#23728,#23729,#23730,#23731,
#23732,#23733,#23734,#23735,#23736,#23737,#23738,#23739));
#7551=EDGE_LOOP('',(#23740,#23741,#23742,#23743,#23744,#23745,#23746,#23747,
#23748,#23749,#23750,#23751,#23752,#23753,#23754,#23755,#23756,#23757,#23758,
#23759,#23760,#23761,#23762,#23763,#23764,#23765,#23766,#23767,#23768,#23769,
#23770,#23771,#23772,#23773,#23774,#23775,#23776,#23777,#23778,#23779,#23780,
#23781,#23782,#23783,#23784,#23785,#23786,#23787,#23788,#23789,#23790,#23791,
#23792,#23793,#23794,#23795,#23796,#23797,#23798,#23799,#23800,#23801,#23802,
#23803,#23804,#23805,#23806,#23807,#23808,#23809,#23810,#23811,#23812,#23813,
#23814,#23815,#23816,#23817,#23818,#23819,#23820,#23821,#23822,#23823,#23824,
#23825,#23826,#23827,#23828,#23829,#23830,#23831,#23832,#23833,#23834,#23835,
#23836,#23837,#23838,#23839,#23840,#23841,#23842,#23843,#23844,#23845,#23846,
#23847,#23848,#23849,#23850,#23851,#23852,#23853,#23854,#23855,#23856,#23857,
#23858,#23859,#23860,#23861,#23862,#23863,#23864,#23865,#23866,#23867,#23868,
#23869,#23870,#23871,#23872,#23873,#23874,#23875,#23876,#23877,#23878,#23879,
#23880,#23881,#23882,#23883,#23884,#23885,#23886,#23887,#23888,#23889,#23890,
#23891,#23892,#23893,#23894,#23895,#23896,#23897,#23898,#23899,#23900,#23901,
#23902,#23903,#23904,#23905,#23906,#23907,#23908,#23909,#23910,#23911,#23912,
#23913,#23914,#23915,#23916,#23917,#23918,#23919,#23920,#23921,#23922,#23923,
#23924,#23925,#23926,#23927,#23928,#23929,#23930,#23931,#23932,#23933,#23934,
#23935,#23936,#23937,#23938,#23939,#23940,#23941,#23942,#23943,#23944,#23945,
#23946,#23947,#23948,#23949,#23950,#23951,#23952,#23953,#23954,#23955,#23956,
#23957,#23958,#23959,#23960,#23961,#23962,#23963,#23964,#23965,#23966,#23967,
#23968,#23969,#23970,#23971,#23972,#23973,#23974,#23975,#23976,#23977,#23978,
#23979,#23980,#23981,#23982,#23983,#23984,#23985,#23986,#23987,#23988,#23989,
#23990,#23991,#23992,#23993,#23994,#23995,#23996,#23997,#23998,#23999,#24000,
#24001,#24002,#24003,#24004,#24005,#24006,#24007,#24008,#24009,#24010,#24011,
#24012,#24013,#24014,#24015,#24016,#24017,#24018,#24019,#24020,#24021,#24022,
#24023,#24024,#24025,#24026,#24027,#24028,#24029,#24030,#24031,#24032,#24033,
#24034,#24035,#24036,#24037,#24038,#24039,#24040,#24041,#24042,#24043,#24044,
#24045,#24046,#24047,#24048,#24049,#24050,#24051,#24052,#24053,#24054,#24055,
#24056,#24057,#24058,#24059,#24060,#24061,#24062,#24063,#24064));
#7552=EDGE_LOOP('',(#24065,#24066,#24067,#24068,#24069));
#7553=EDGE_LOOP('',(#24070,#24071,#24072,#24073));
#7554=EDGE_LOOP('',(#24074,#24075,#24076,#24077));
#7555=EDGE_LOOP('',(#24078,#24079,#24080,#24081));
#7556=EDGE_LOOP('',(#24082,#24083,#24084,#24085));
#7557=EDGE_LOOP('',(#24086,#24087,#24088,#24089));
#7558=EDGE_LOOP('',(#24090,#24091,#24092,#24093));
#7559=EDGE_LOOP('',(#24094,#24095,#24096,#24097));
#7560=EDGE_LOOP('',(#24098,#24099,#24100,#24101));
#7561=EDGE_LOOP('',(#24102,#24103,#24104,#24105));
#7562=EDGE_LOOP('',(#24106,#24107,#24108,#24109));
#7563=EDGE_LOOP('',(#24110,#24111,#24112,#24113));
#7564=EDGE_LOOP('',(#24114,#24115,#24116,#24117));
#7565=EDGE_LOOP('',(#24118,#24119,#24120,#24121));
#7566=EDGE_LOOP('',(#24122,#24123,#24124,#24125));
#7567=EDGE_LOOP('',(#24126,#24127,#24128,#24129));
#7568=EDGE_LOOP('',(#24130,#24131,#24132,#24133));
#7569=EDGE_LOOP('',(#24134,#24135,#24136,#24137));
#7570=EDGE_LOOP('',(#24138,#24139,#24140,#24141));
#7571=EDGE_LOOP('',(#24142,#24143,#24144,#24145));
#7572=EDGE_LOOP('',(#24146,#24147,#24148,#24149));
#7573=EDGE_LOOP('',(#24150,#24151,#24152,#24153));
#7574=EDGE_LOOP('',(#24154,#24155,#24156,#24157));
#7575=EDGE_LOOP('',(#24158,#24159,#24160,#24161));
#7576=EDGE_LOOP('',(#24162,#24163,#24164,#24165));
#7577=EDGE_LOOP('',(#24166,#24167,#24168,#24169));
#7578=EDGE_LOOP('',(#24170,#24171,#24172,#24173));
#7579=EDGE_LOOP('',(#24174,#24175,#24176,#24177));
#7580=EDGE_LOOP('',(#24178,#24179,#24180,#24181));
#7581=EDGE_LOOP('',(#24182,#24183,#24184,#24185));
#7582=EDGE_LOOP('',(#24186,#24187,#24188,#24189));
#7583=EDGE_LOOP('',(#24190,#24191,#24192,#24193));
#7584=EDGE_LOOP('',(#24194,#24195,#24196,#24197));
#7585=EDGE_LOOP('',(#24198,#24199,#24200,#24201));
#7586=EDGE_LOOP('',(#24202,#24203,#24204,#24205));
#7587=EDGE_LOOP('',(#24206,#24207,#24208,#24209));
#7588=EDGE_LOOP('',(#24210,#24211,#24212,#24213));
#7589=EDGE_LOOP('',(#24214,#24215,#24216,#24217));
#7590=EDGE_LOOP('',(#24218,#24219,#24220,#24221));
#7591=EDGE_LOOP('',(#24222,#24223,#24224,#24225));
#7592=EDGE_LOOP('',(#24226,#24227,#24228,#24229));
#7593=EDGE_LOOP('',(#24230,#24231,#24232,#24233));
#7594=EDGE_LOOP('',(#24234,#24235,#24236,#24237));
#7595=EDGE_LOOP('',(#24238,#24239,#24240,#24241));
#7596=EDGE_LOOP('',(#24242,#24243,#24244,#24245));
#7597=EDGE_LOOP('',(#24246,#24247,#24248,#24249));
#7598=EDGE_LOOP('',(#24250,#24251,#24252,#24253));
#7599=EDGE_LOOP('',(#24254,#24255,#24256,#24257));
#7600=EDGE_LOOP('',(#24258,#24259,#24260,#24261));
#7601=EDGE_LOOP('',(#24262,#24263,#24264,#24265));
#7602=EDGE_LOOP('',(#24266,#24267,#24268,#24269));
#7603=EDGE_LOOP('',(#24270,#24271,#24272,#24273));
#7604=EDGE_LOOP('',(#24274,#24275,#24276,#24277));
#7605=EDGE_LOOP('',(#24278,#24279,#24280,#24281));
#7606=EDGE_LOOP('',(#24282,#24283,#24284,#24285));
#7607=EDGE_LOOP('',(#24286,#24287,#24288,#24289));
#7608=EDGE_LOOP('',(#24290,#24291,#24292,#24293));
#7609=EDGE_LOOP('',(#24294,#24295,#24296,#24297));
#7610=EDGE_LOOP('',(#24298,#24299,#24300,#24301));
#7611=EDGE_LOOP('',(#24302,#24303,#24304,#24305));
#7612=EDGE_LOOP('',(#24306,#24307,#24308,#24309));
#7613=EDGE_LOOP('',(#24310,#24311,#24312,#24313));
#7614=EDGE_LOOP('',(#24314,#24315,#24316,#24317));
#7615=EDGE_LOOP('',(#24318,#24319,#24320,#24321));
#7616=EDGE_LOOP('',(#24322,#24323,#24324,#24325));
#7617=EDGE_LOOP('',(#24326,#24327,#24328,#24329));
#7618=EDGE_LOOP('',(#24330,#24331,#24332,#24333));
#7619=EDGE_LOOP('',(#24334,#24335,#24336,#24337));
#7620=EDGE_LOOP('',(#24338,#24339,#24340,#24341));
#7621=EDGE_LOOP('',(#24342,#24343,#24344,#24345));
#7622=EDGE_LOOP('',(#24346,#24347,#24348,#24349));
#7623=EDGE_LOOP('',(#24350,#24351,#24352,#24353));
#7624=EDGE_LOOP('',(#24354,#24355,#24356,#24357));
#7625=EDGE_LOOP('',(#24358,#24359,#24360,#24361));
#7626=EDGE_LOOP('',(#24362,#24363,#24364,#24365));
#7627=EDGE_LOOP('',(#24366,#24367,#24368,#24369));
#7628=EDGE_LOOP('',(#24370,#24371,#24372,#24373));
#7629=EDGE_LOOP('',(#24374,#24375,#24376,#24377));
#7630=EDGE_LOOP('',(#24378,#24379,#24380,#24381));
#7631=EDGE_LOOP('',(#24382,#24383,#24384,#24385));
#7632=EDGE_LOOP('',(#24386,#24387,#24388,#24389));
#7633=EDGE_LOOP('',(#24390,#24391,#24392,#24393));
#7634=EDGE_LOOP('',(#24394,#24395,#24396,#24397));
#7635=EDGE_LOOP('',(#24398,#24399,#24400,#24401));
#7636=EDGE_LOOP('',(#24402,#24403,#24404,#24405));
#7637=EDGE_LOOP('',(#24406,#24407,#24408,#24409));
#7638=EDGE_LOOP('',(#24410,#24411,#24412,#24413));
#7639=EDGE_LOOP('',(#24414,#24415,#24416,#24417));
#7640=EDGE_LOOP('',(#24418,#24419,#24420,#24421));
#7641=EDGE_LOOP('',(#24422,#24423,#24424,#24425));
#7642=EDGE_LOOP('',(#24426,#24427,#24428,#24429));
#7643=EDGE_LOOP('',(#24430,#24431,#24432,#24433));
#7644=EDGE_LOOP('',(#24434,#24435,#24436,#24437));
#7645=EDGE_LOOP('',(#24438,#24439,#24440,#24441));
#7646=EDGE_LOOP('',(#24442,#24443,#24444,#24445));
#7647=EDGE_LOOP('',(#24446,#24447,#24448,#24449));
#7648=EDGE_LOOP('',(#24450,#24451,#24452,#24453));
#7649=EDGE_LOOP('',(#24454,#24455,#24456,#24457));
#7650=EDGE_LOOP('',(#24458,#24459,#24460,#24461));
#7651=EDGE_LOOP('',(#24462,#24463,#24464,#24465));
#7652=EDGE_LOOP('',(#24466,#24467,#24468,#24469));
#7653=EDGE_LOOP('',(#24470,#24471,#24472,#24473));
#7654=EDGE_LOOP('',(#24474,#24475,#24476,#24477));
#7655=EDGE_LOOP('',(#24478,#24479,#24480,#24481));
#7656=EDGE_LOOP('',(#24482,#24483,#24484,#24485));
#7657=EDGE_LOOP('',(#24486,#24487,#24488,#24489));
#7658=EDGE_LOOP('',(#24490,#24491,#24492,#24493));
#7659=EDGE_LOOP('',(#24494,#24495,#24496,#24497));
#7660=EDGE_LOOP('',(#24498,#24499,#24500,#24501));
#7661=EDGE_LOOP('',(#24502,#24503,#24504,#24505));
#7662=EDGE_LOOP('',(#24506,#24507,#24508,#24509));
#7663=EDGE_LOOP('',(#24510,#24511,#24512,#24513));
#7664=EDGE_LOOP('',(#24514,#24515,#24516,#24517));
#7665=EDGE_LOOP('',(#24518,#24519,#24520,#24521));
#7666=EDGE_LOOP('',(#24522,#24523,#24524,#24525));
#7667=EDGE_LOOP('',(#24526,#24527,#24528,#24529));
#7668=EDGE_LOOP('',(#24530,#24531,#24532,#24533));
#7669=EDGE_LOOP('',(#24534,#24535,#24536,#24537));
#7670=EDGE_LOOP('',(#24538,#24539,#24540,#24541));
#7671=EDGE_LOOP('',(#24542,#24543,#24544,#24545));
#7672=EDGE_LOOP('',(#24546,#24547,#24548,#24549));
#7673=EDGE_LOOP('',(#24550,#24551,#24552,#24553));
#7674=EDGE_LOOP('',(#24554,#24555,#24556,#24557));
#7675=EDGE_LOOP('',(#24558,#24559,#24560,#24561));
#7676=EDGE_LOOP('',(#24562,#24563,#24564,#24565));
#7677=EDGE_LOOP('',(#24566,#24567,#24568,#24569));
#7678=EDGE_LOOP('',(#24570,#24571,#24572,#24573));
#7679=EDGE_LOOP('',(#24574,#24575,#24576,#24577));
#7680=EDGE_LOOP('',(#24578,#24579,#24580,#24581));
#7681=EDGE_LOOP('',(#24582,#24583,#24584,#24585));
#7682=EDGE_LOOP('',(#24586,#24587,#24588,#24589));
#7683=EDGE_LOOP('',(#24590,#24591,#24592,#24593));
#7684=EDGE_LOOP('',(#24594,#24595,#24596,#24597));
#7685=EDGE_LOOP('',(#24598,#24599,#24600,#24601));
#7686=EDGE_LOOP('',(#24602,#24603,#24604,#24605));
#7687=EDGE_LOOP('',(#24606,#24607,#24608,#24609));
#7688=EDGE_LOOP('',(#24610,#24611,#24612,#24613));
#7689=EDGE_LOOP('',(#24614,#24615,#24616,#24617));
#7690=EDGE_LOOP('',(#24618,#24619,#24620,#24621));
#7691=EDGE_LOOP('',(#24622,#24623,#24624,#24625));
#7692=EDGE_LOOP('',(#24626,#24627,#24628,#24629));
#7693=EDGE_LOOP('',(#24630,#24631,#24632,#24633));
#7694=EDGE_LOOP('',(#24634,#24635,#24636,#24637));
#7695=EDGE_LOOP('',(#24638,#24639,#24640,#24641));
#7696=EDGE_LOOP('',(#24642,#24643,#24644,#24645));
#7697=EDGE_LOOP('',(#24646,#24647,#24648,#24649));
#7698=EDGE_LOOP('',(#24650,#24651,#24652,#24653));
#7699=EDGE_LOOP('',(#24654,#24655,#24656,#24657));
#7700=EDGE_LOOP('',(#24658,#24659,#24660,#24661));
#7701=EDGE_LOOP('',(#24662,#24663,#24664,#24665));
#7702=EDGE_LOOP('',(#24666,#24667,#24668,#24669));
#7703=EDGE_LOOP('',(#24670,#24671,#24672,#24673));
#7704=EDGE_LOOP('',(#24674,#24675,#24676,#24677));
#7705=EDGE_LOOP('',(#24678,#24679,#24680,#24681));
#7706=EDGE_LOOP('',(#24682,#24683,#24684,#24685));
#7707=EDGE_LOOP('',(#24686,#24687,#24688,#24689));
#7708=EDGE_LOOP('',(#24690,#24691,#24692,#24693));
#7709=EDGE_LOOP('',(#24694,#24695,#24696,#24697));
#7710=EDGE_LOOP('',(#24698,#24699,#24700,#24701));
#7711=EDGE_LOOP('',(#24702,#24703,#24704,#24705));
#7712=EDGE_LOOP('',(#24706,#24707,#24708,#24709));
#7713=EDGE_LOOP('',(#24710,#24711,#24712,#24713));
#7714=EDGE_LOOP('',(#24714,#24715,#24716,#24717));
#7715=EDGE_LOOP('',(#24718,#24719,#24720,#24721));
#7716=EDGE_LOOP('',(#24722,#24723,#24724,#24725));
#7717=EDGE_LOOP('',(#24726,#24727,#24728,#24729));
#7718=EDGE_LOOP('',(#24730,#24731,#24732,#24733));
#7719=EDGE_LOOP('',(#24734,#24735,#24736,#24737));
#7720=EDGE_LOOP('',(#24738,#24739,#24740,#24741));
#7721=EDGE_LOOP('',(#24742,#24743,#24744,#24745));
#7722=EDGE_LOOP('',(#24746,#24747,#24748,#24749));
#7723=EDGE_LOOP('',(#24750,#24751,#24752,#24753));
#7724=EDGE_LOOP('',(#24754,#24755,#24756,#24757));
#7725=EDGE_LOOP('',(#24758,#24759,#24760,#24761));
#7726=EDGE_LOOP('',(#24762,#24763,#24764,#24765));
#7727=EDGE_LOOP('',(#24766,#24767,#24768,#24769));
#7728=EDGE_LOOP('',(#24770,#24771,#24772,#24773));
#7729=EDGE_LOOP('',(#24774,#24775,#24776,#24777));
#7730=EDGE_LOOP('',(#24778,#24779,#24780,#24781));
#7731=EDGE_LOOP('',(#24782,#24783,#24784,#24785));
#7732=EDGE_LOOP('',(#24786,#24787,#24788,#24789));
#7733=EDGE_LOOP('',(#24790,#24791,#24792,#24793));
#7734=EDGE_LOOP('',(#24794,#24795,#24796,#24797));
#7735=EDGE_LOOP('',(#24798,#24799,#24800,#24801));
#7736=EDGE_LOOP('',(#24802,#24803,#24804,#24805));
#7737=EDGE_LOOP('',(#24806,#24807,#24808,#24809));
#7738=EDGE_LOOP('',(#24810,#24811,#24812,#24813));
#7739=EDGE_LOOP('',(#24814,#24815,#24816,#24817));
#7740=EDGE_LOOP('',(#24818,#24819,#24820,#24821));
#7741=EDGE_LOOP('',(#24822,#24823,#24824,#24825));
#7742=EDGE_LOOP('',(#24826,#24827,#24828,#24829));
#7743=EDGE_LOOP('',(#24830,#24831,#24832,#24833));
#7744=EDGE_LOOP('',(#24834,#24835,#24836,#24837));
#7745=EDGE_LOOP('',(#24838,#24839,#24840,#24841));
#7746=EDGE_LOOP('',(#24842,#24843,#24844,#24845));
#7747=EDGE_LOOP('',(#24846,#24847,#24848,#24849));
#7748=EDGE_LOOP('',(#24850,#24851,#24852,#24853));
#7749=EDGE_LOOP('',(#24854,#24855,#24856,#24857));
#7750=EDGE_LOOP('',(#24858,#24859,#24860,#24861));
#7751=EDGE_LOOP('',(#24862,#24863,#24864,#24865));
#7752=EDGE_LOOP('',(#24866,#24867,#24868,#24869));
#7753=EDGE_LOOP('',(#24870,#24871,#24872,#24873));
#7754=EDGE_LOOP('',(#24874,#24875,#24876,#24877));
#7755=EDGE_LOOP('',(#24878,#24879,#24880,#24881));
#7756=EDGE_LOOP('',(#24882,#24883,#24884,#24885));
#7757=EDGE_LOOP('',(#24886,#24887,#24888,#24889));
#7758=EDGE_LOOP('',(#24890,#24891,#24892,#24893));
#7759=EDGE_LOOP('',(#24894,#24895,#24896,#24897));
#7760=EDGE_LOOP('',(#24898,#24899,#24900,#24901));
#7761=EDGE_LOOP('',(#24902,#24903,#24904,#24905));
#7762=EDGE_LOOP('',(#24906,#24907,#24908,#24909));
#7763=EDGE_LOOP('',(#24910,#24911,#24912,#24913));
#7764=EDGE_LOOP('',(#24914,#24915,#24916,#24917));
#7765=EDGE_LOOP('',(#24918,#24919,#24920,#24921));
#7766=EDGE_LOOP('',(#24922,#24923,#24924,#24925));
#7767=EDGE_LOOP('',(#24926,#24927,#24928,#24929));
#7768=EDGE_LOOP('',(#24930,#24931,#24932,#24933));
#7769=EDGE_LOOP('',(#24934,#24935,#24936,#24937));
#7770=EDGE_LOOP('',(#24938,#24939,#24940,#24941));
#7771=EDGE_LOOP('',(#24942,#24943,#24944,#24945));
#7772=EDGE_LOOP('',(#24946,#24947,#24948,#24949));
#7773=EDGE_LOOP('',(#24950,#24951,#24952,#24953));
#7774=EDGE_LOOP('',(#24954,#24955,#24956,#24957));
#7775=EDGE_LOOP('',(#24958,#24959,#24960,#24961));
#7776=EDGE_LOOP('',(#24962,#24963,#24964,#24965));
#7777=EDGE_LOOP('',(#24966,#24967,#24968,#24969));
#7778=EDGE_LOOP('',(#24970,#24971,#24972,#24973));
#7779=EDGE_LOOP('',(#24974,#24975,#24976,#24977));
#7780=EDGE_LOOP('',(#24978,#24979,#24980,#24981));
#7781=EDGE_LOOP('',(#24982,#24983,#24984,#24985));
#7782=EDGE_LOOP('',(#24986,#24987,#24988,#24989));
#7783=EDGE_LOOP('',(#24990,#24991,#24992,#24993));
#7784=EDGE_LOOP('',(#24994,#24995,#24996,#24997));
#7785=EDGE_LOOP('',(#24998,#24999,#25000,#25001));
#7786=EDGE_LOOP('',(#25002,#25003,#25004,#25005));
#7787=EDGE_LOOP('',(#25006,#25007,#25008,#25009));
#7788=EDGE_LOOP('',(#25010,#25011,#25012,#25013));
#7789=EDGE_LOOP('',(#25014,#25015,#25016,#25017));
#7790=EDGE_LOOP('',(#25018,#25019,#25020,#25021));
#7791=EDGE_LOOP('',(#25022,#25023,#25024,#25025));
#7792=EDGE_LOOP('',(#25026,#25027,#25028,#25029));
#7793=EDGE_LOOP('',(#25030,#25031,#25032));
#7794=EDGE_LOOP('',(#25033));
#7795=EDGE_LOOP('',(#25034));
#7796=EDGE_LOOP('',(#25035,#25036,#25037,#25038));
#7797=EDGE_LOOP('',(#25039,#25040,#25041,#25042));
#7798=EDGE_LOOP('',(#25043,#25044,#25045,#25046));
#7799=EDGE_LOOP('',(#25047));
#7800=EDGE_LOOP('',(#25048));
#7801=EDGE_LOOP('',(#25049,#25050,#25051,#25052,#25053,#25054));
#7802=EDGE_LOOP('',(#25055,#25056,#25057,#25058));
#7803=EDGE_LOOP('',(#25059,#25060,#25061,#25062));
#7804=EDGE_LOOP('',(#25063,#25064,#25065,#25066));
#7805=EDGE_LOOP('',(#25067,#25068,#25069,#25070,#25071));
#7806=EDGE_LOOP('',(#25072,#25073,#25074,#25075));
#7807=EDGE_LOOP('',(#25076,#25077,#25078,#25079));
#7808=EDGE_LOOP('',(#25080,#25081,#25082,#25083,#25084,#25085,#25086,#25087,
#25088,#25089,#25090,#25091,#25092,#25093,#25094,#25095,#25096,#25097,#25098,
#25099,#25100,#25101,#25102,#25103,#25104,#25105,#25106,#25107,#25108,#25109,
#25110,#25111,#25112,#25113,#25114,#25115,#25116,#25117,#25118,#25119,#25120,
#25121,#25122,#25123,#25124,#25125,#25126,#25127,#25128,#25129,#25130,#25131,
#25132,#25133,#25134,#25135,#25136,#25137,#25138,#25139,#25140,#25141));
#7809=EDGE_LOOP('',(#25142,#25143,#25144,#25145,#25146,#25147,#25148,#25149,
#25150,#25151,#25152,#25153,#25154,#25155,#25156,#25157,#25158,#25159,#25160,
#25161,#25162,#25163,#25164,#25165,#25166,#25167,#25168,#25169,#25170,#25171,
#25172,#25173,#25174,#25175,#25176,#25177,#25178,#25179,#25180,#25181,#25182,
#25183,#25184,#25185,#25186,#25187,#25188,#25189,#25190,#25191,#25192,#25193,
#25194,#25195,#25196,#25197,#25198,#25199,#25200,#25201,#25202));
#7810=EDGE_LOOP('',(#25203,#25204,#25205,#25206));
#7811=EDGE_LOOP('',(#25207,#25208,#25209,#25210,#25211,#25212));
#7812=EDGE_LOOP('',(#25213,#25214,#25215,#25216,#25217));
#7813=EDGE_LOOP('',(#25218,#25219,#25220,#25221,#25222,#25223));
#7814=EDGE_LOOP('',(#25224,#25225,#25226,#25227,#25228,#25229));
#7815=EDGE_LOOP('',(#25230,#25231,#25232,#25233));
#7816=EDGE_LOOP('',(#25234,#25235,#25236,#25237,#25238,#25239));
#7817=EDGE_LOOP('',(#25240,#25241,#25242,#25243,#25244,#25245));
#7818=EDGE_LOOP('',(#25246,#25247,#25248,#25249));
#7819=EDGE_LOOP('',(#25250,#25251,#25252,#25253,#25254,#25255));
#7820=EDGE_LOOP('',(#25256,#25257,#25258,#25259,#25260,#25261));
#7821=EDGE_LOOP('',(#25262,#25263,#25264,#25265));
#7822=EDGE_LOOP('',(#25266,#25267,#25268,#25269,#25270,#25271));
#7823=EDGE_LOOP('',(#25272,#25273,#25274,#25275,#25276,#25277));
#7824=EDGE_LOOP('',(#25278,#25279,#25280,#25281));
#7825=EDGE_LOOP('',(#25282,#25283,#25284,#25285,#25286,#25287));
#7826=EDGE_LOOP('',(#25288,#25289,#25290,#25291,#25292,#25293));
#7827=EDGE_LOOP('',(#25294,#25295,#25296,#25297));
#7828=EDGE_LOOP('',(#25298,#25299,#25300,#25301,#25302,#25303));
#7829=EDGE_LOOP('',(#25304,#25305,#25306,#25307,#25308,#25309));
#7830=EDGE_LOOP('',(#25310,#25311,#25312,#25313));
#7831=EDGE_LOOP('',(#25314,#25315,#25316,#25317,#25318,#25319));
#7832=EDGE_LOOP('',(#25320,#25321,#25322,#25323,#25324,#25325));
#7833=EDGE_LOOP('',(#25326,#25327,#25328,#25329,#25330,#25331));
#7834=EDGE_LOOP('',(#25332,#25333,#25334,#25335,#25336,#25337));
#7835=EDGE_LOOP('',(#25338,#25339,#25340,#25341,#25342,#25343));
#7836=EDGE_LOOP('',(#25344,#25345,#25346,#25347,#25348,#25349));
#7837=EDGE_LOOP('',(#25350,#25351,#25352,#25353,#25354,#25355));
#7838=EDGE_LOOP('',(#25356,#25357,#25358,#25359,#25360,#25361));
#7839=EDGE_LOOP('',(#25362,#25363,#25364,#25365,#25366,#25367));
#7840=EDGE_LOOP('',(#25368,#25369,#25370,#25371,#25372,#25373));
#7841=EDGE_LOOP('',(#25374,#25375,#25376,#25377,#25378,#25379));
#7842=EDGE_LOOP('',(#25380,#25381,#25382,#25383,#25384,#25385));
#7843=EDGE_LOOP('',(#25386,#25387,#25388,#25389,#25390,#25391));
#7844=EDGE_LOOP('',(#25392,#25393,#25394,#25395,#25396,#25397));
#7845=EDGE_LOOP('',(#25398,#25399,#25400,#25401,#25402,#25403));
#7846=EDGE_LOOP('',(#25404,#25405,#25406,#25407,#25408,#25409));
#7847=EDGE_LOOP('',(#25410,#25411,#25412,#25413,#25414,#25415));
#7848=EDGE_LOOP('',(#25416,#25417,#25418,#25419,#25420,#25421));
#7849=EDGE_LOOP('',(#25422,#25423,#25424,#25425,#25426,#25427));
#7850=EDGE_LOOP('',(#25428,#25429,#25430,#25431,#25432,#25433));
#7851=EDGE_LOOP('',(#25434,#25435,#25436,#25437));
#7852=EDGE_LOOP('',(#25438,#25439,#25440,#25441,#25442,#25443));
#7853=EDGE_LOOP('',(#25444,#25445,#25446,#25447,#25448,#25449));
#7854=EDGE_LOOP('',(#25450,#25451,#25452,#25453));
#7855=EDGE_LOOP('',(#25454,#25455,#25456,#25457,#25458,#25459));
#7856=EDGE_LOOP('',(#25460,#25461,#25462,#25463,#25464,#25465));
#7857=EDGE_LOOP('',(#25466,#25467,#25468,#25469));
#7858=EDGE_LOOP('',(#25470,#25471,#25472,#25473,#25474,#25475));
#7859=EDGE_LOOP('',(#25476,#25477,#25478,#25479,#25480,#25481));
#7860=EDGE_LOOP('',(#25482,#25483,#25484,#25485));
#7861=EDGE_LOOP('',(#25486,#25487,#25488,#25489,#25490,#25491));
#7862=EDGE_LOOP('',(#25492,#25493,#25494,#25495,#25496,#25497));
#7863=EDGE_LOOP('',(#25498,#25499,#25500,#25501));
#7864=EDGE_LOOP('',(#25502,#25503,#25504,#25505,#25506,#25507));
#7865=EDGE_LOOP('',(#25508,#25509,#25510,#25511,#25512,#25513));
#7866=EDGE_LOOP('',(#25514,#25515,#25516,#25517));
#7867=EDGE_LOOP('',(#25518,#25519,#25520,#25521,#25522,#25523));
#7868=EDGE_LOOP('',(#25524,#25525,#25526,#25527,#25528,#25529));
#7869=EDGE_LOOP('',(#25530,#25531,#25532,#25533));
#7870=EDGE_LOOP('',(#25534,#25535,#25536,#25537,#25538,#25539));
#7871=EDGE_LOOP('',(#25540,#25541,#25542,#25543,#25544,#25545));
#7872=EDGE_LOOP('',(#25546,#25547,#25548,#25549));
#7873=EDGE_LOOP('',(#25550,#25551,#25552,#25553,#25554,#25555));
#7874=EDGE_LOOP('',(#25556,#25557,#25558,#25559,#25560,#25561));
#7875=EDGE_LOOP('',(#25562,#25563,#25564,#25565));
#7876=EDGE_LOOP('',(#25566,#25567,#25568,#25569,#25570,#25571));
#7877=EDGE_LOOP('',(#25572,#25573,#25574,#25575,#25576,#25577));
#7878=EDGE_LOOP('',(#25578,#25579,#25580,#25581));
#7879=EDGE_LOOP('',(#25582,#25583,#25584,#25585,#25586,#25587));
#7880=EDGE_LOOP('',(#25588,#25589,#25590,#25591,#25592,#25593));
#7881=EDGE_LOOP('',(#25594,#25595,#25596,#25597));
#7882=EDGE_LOOP('',(#25598,#25599,#25600,#25601,#25602,#25603));
#7883=EDGE_LOOP('',(#25604,#25605,#25606,#25607,#25608,#25609));
#7884=EDGE_LOOP('',(#25610,#25611,#25612,#25613));
#7885=EDGE_LOOP('',(#25614,#25615,#25616,#25617,#25618,#25619));
#7886=EDGE_LOOP('',(#25620,#25621,#25622,#25623,#25624,#25625));
#7887=EDGE_LOOP('',(#25626,#25627,#25628,#25629));
#7888=EDGE_LOOP('',(#25630,#25631,#25632,#25633,#25634,#25635));
#7889=EDGE_LOOP('',(#25636,#25637,#25638,#25639,#25640,#25641));
#7890=EDGE_LOOP('',(#25642,#25643,#25644,#25645));
#7891=EDGE_LOOP('',(#25646,#25647,#25648,#25649,#25650,#25651));
#7892=EDGE_LOOP('',(#25652,#25653,#25654,#25655,#25656,#25657));
#7893=EDGE_LOOP('',(#25658,#25659,#25660,#25661));
#7894=EDGE_LOOP('',(#25662,#25663,#25664,#25665,#25666,#25667));
#7895=EDGE_LOOP('',(#25668,#25669,#25670,#25671,#25672,#25673));
#7896=EDGE_LOOP('',(#25674,#25675,#25676,#25677));
#7897=EDGE_LOOP('',(#25678,#25679,#25680,#25681,#25682,#25683));
#7898=EDGE_LOOP('',(#25684,#25685,#25686,#25687,#25688,#25689));
#7899=EDGE_LOOP('',(#25690,#25691,#25692,#25693));
#7900=EDGE_LOOP('',(#25694,#25695,#25696,#25697,#25698,#25699));
#7901=EDGE_LOOP('',(#25700,#25701,#25702,#25703,#25704,#25705));
#7902=EDGE_LOOP('',(#25706,#25707,#25708,#25709));
#7903=EDGE_LOOP('',(#25710,#25711,#25712,#25713,#25714,#25715));
#7904=EDGE_LOOP('',(#25716,#25717,#25718,#25719,#25720,#25721));
#7905=EDGE_LOOP('',(#25722,#25723,#25724,#25725));
#7906=EDGE_LOOP('',(#25726,#25727,#25728,#25729,#25730,#25731));
#7907=EDGE_LOOP('',(#25732,#25733,#25734,#25735,#25736,#25737));
#7908=EDGE_LOOP('',(#25738,#25739,#25740,#25741));
#7909=EDGE_LOOP('',(#25742,#25743,#25744,#25745,#25746,#25747));
#7910=EDGE_LOOP('',(#25748,#25749,#25750,#25751,#25752,#25753));
#7911=EDGE_LOOP('',(#25754,#25755,#25756,#25757));
#7912=EDGE_LOOP('',(#25758,#25759,#25760,#25761,#25762,#25763));
#7913=EDGE_LOOP('',(#25764,#25765,#25766,#25767,#25768,#25769));
#7914=EDGE_LOOP('',(#25770,#25771,#25772,#25773));
#7915=EDGE_LOOP('',(#25774,#25775,#25776,#25777,#25778,#25779));
#7916=EDGE_LOOP('',(#25780,#25781,#25782,#25783,#25784,#25785));
#7917=EDGE_LOOP('',(#25786,#25787,#25788,#25789));
#7918=EDGE_LOOP('',(#25790,#25791,#25792,#25793,#25794,#25795));
#7919=EDGE_LOOP('',(#25796,#25797,#25798,#25799,#25800,#25801));
#7920=EDGE_LOOP('',(#25802,#25803,#25804,#25805));
#7921=EDGE_LOOP('',(#25806,#25807,#25808,#25809,#25810,#25811));
#7922=EDGE_LOOP('',(#25812,#25813,#25814,#25815,#25816,#25817));
#7923=EDGE_LOOP('',(#25818,#25819,#25820,#25821));
#7924=EDGE_LOOP('',(#25822,#25823,#25824,#25825,#25826,#25827));
#7925=EDGE_LOOP('',(#25828,#25829,#25830,#25831,#25832,#25833));
#7926=EDGE_LOOP('',(#25834,#25835,#25836,#25837));
#7927=EDGE_LOOP('',(#25838,#25839,#25840,#25841,#25842,#25843));
#7928=EDGE_LOOP('',(#25844,#25845,#25846,#25847,#25848,#25849));
#7929=EDGE_LOOP('',(#25850,#25851,#25852,#25853));
#7930=EDGE_LOOP('',(#25854,#25855,#25856,#25857,#25858,#25859));
#7931=EDGE_LOOP('',(#25860,#25861,#25862,#25863,#25864,#25865));
#7932=EDGE_LOOP('',(#25866,#25867,#25868,#25869));
#7933=EDGE_LOOP('',(#25870,#25871,#25872,#25873,#25874,#25875));
#7934=EDGE_LOOP('',(#25876,#25877,#25878,#25879,#25880,#25881));
#7935=EDGE_LOOP('',(#25882,#25883,#25884,#25885));
#7936=EDGE_LOOP('',(#25886,#25887,#25888,#25889,#25890,#25891));
#7937=EDGE_LOOP('',(#25892,#25893,#25894,#25895,#25896,#25897));
#7938=EDGE_LOOP('',(#25898,#25899,#25900,#25901));
#7939=EDGE_LOOP('',(#25902,#25903,#25904,#25905,#25906,#25907));
#7940=EDGE_LOOP('',(#25908,#25909,#25910,#25911,#25912,#25913));
#7941=EDGE_LOOP('',(#25914,#25915,#25916,#25917));
#7942=EDGE_LOOP('',(#25918,#25919,#25920,#25921,#25922,#25923));
#7943=EDGE_LOOP('',(#25924,#25925,#25926,#25927,#25928,#25929));
#7944=EDGE_LOOP('',(#25930,#25931,#25932,#25933));
#7945=EDGE_LOOP('',(#25934,#25935,#25936,#25937,#25938,#25939));
#7946=EDGE_LOOP('',(#25940,#25941,#25942,#25943,#25944,#25945));
#7947=EDGE_LOOP('',(#25946,#25947,#25948,#25949));
#7948=EDGE_LOOP('',(#25950,#25951,#25952,#25953,#25954,#25955));
#7949=EDGE_LOOP('',(#25956,#25957,#25958,#25959,#25960,#25961));
#7950=EDGE_LOOP('',(#25962,#25963,#25964,#25965));
#7951=EDGE_LOOP('',(#25966,#25967,#25968,#25969,#25970,#25971));
#7952=EDGE_LOOP('',(#25972,#25973,#25974,#25975,#25976,#25977));
#7953=EDGE_LOOP('',(#25978,#25979,#25980,#25981));
#7954=EDGE_LOOP('',(#25982,#25983,#25984,#25985,#25986,#25987));
#7955=EDGE_LOOP('',(#25988,#25989,#25990,#25991,#25992,#25993));
#7956=EDGE_LOOP('',(#25994,#25995,#25996,#25997));
#7957=EDGE_LOOP('',(#25998,#25999,#26000,#26001,#26002,#26003));
#7958=EDGE_LOOP('',(#26004,#26005,#26006,#26007,#26008,#26009));
#7959=EDGE_LOOP('',(#26010,#26011,#26012,#26013));
#7960=EDGE_LOOP('',(#26014,#26015,#26016,#26017,#26018,#26019));
#7961=EDGE_LOOP('',(#26020,#26021,#26022,#26023,#26024,#26025));
#7962=EDGE_LOOP('',(#26026,#26027,#26028,#26029));
#7963=EDGE_LOOP('',(#26030,#26031,#26032,#26033,#26034,#26035));
#7964=EDGE_LOOP('',(#26036,#26037,#26038,#26039,#26040,#26041));
#7965=EDGE_LOOP('',(#26042,#26043,#26044,#26045,#26046));
#7966=EDGE_LOOP('',(#26047,#26048,#26049,#26050,#26051,#26052));
#7967=EDGE_LOOP('',(#26053,#26054,#26055,#26056,#26057,#26058));
#7968=EDGE_LOOP('',(#26059,#26060,#26061,#26062));
#7969=EDGE_LOOP('',(#26063,#26064,#26065,#26066,#26067,#26068));
#7970=EDGE_LOOP('',(#26069,#26070,#26071,#26072,#26073,#26074));
#7971=EDGE_LOOP('',(#26075,#26076,#26077,#26078));
#7972=EDGE_LOOP('',(#26079,#26080,#26081,#26082,#26083,#26084));
#7973=EDGE_LOOP('',(#26085,#26086,#26087,#26088,#26089,#26090));
#7974=EDGE_LOOP('',(#26091,#26092,#26093,#26094));
#7975=EDGE_LOOP('',(#26095,#26096,#26097,#26098,#26099,#26100));
#7976=EDGE_LOOP('',(#26101,#26102,#26103,#26104,#26105,#26106));
#7977=EDGE_LOOP('',(#26107,#26108,#26109,#26110));
#7978=EDGE_LOOP('',(#26111,#26112,#26113,#26114,#26115,#26116));
#7979=EDGE_LOOP('',(#26117,#26118,#26119,#26120,#26121,#26122));
#7980=EDGE_LOOP('',(#26123,#26124,#26125,#26126));
#7981=EDGE_LOOP('',(#26127,#26128,#26129,#26130,#26131,#26132));
#7982=EDGE_LOOP('',(#26133,#26134,#26135,#26136,#26137,#26138));
#7983=EDGE_LOOP('',(#26139,#26140,#26141,#26142));
#7984=EDGE_LOOP('',(#26143,#26144,#26145,#26146,#26147,#26148));
#7985=EDGE_LOOP('',(#26149,#26150,#26151,#26152,#26153,#26154));
#7986=EDGE_LOOP('',(#26155,#26156,#26157,#26158));
#7987=EDGE_LOOP('',(#26159,#26160,#26161,#26162,#26163,#26164));
#7988=EDGE_LOOP('',(#26165,#26166,#26167,#26168,#26169,#26170));
#7989=EDGE_LOOP('',(#26171,#26172,#26173,#26174));
#7990=EDGE_LOOP('',(#26175,#26176,#26177,#26178,#26179,#26180));
#7991=EDGE_LOOP('',(#26181,#26182,#26183,#26184,#26185,#26186));
#7992=EDGE_LOOP('',(#26187,#26188,#26189,#26190));
#7993=EDGE_LOOP('',(#26191,#26192,#26193,#26194,#26195,#26196));
#7994=EDGE_LOOP('',(#26197,#26198,#26199,#26200,#26201,#26202));
#7995=EDGE_LOOP('',(#26203,#26204,#26205,#26206));
#7996=EDGE_LOOP('',(#26207,#26208,#26209,#26210,#26211,#26212));
#7997=EDGE_LOOP('',(#26213,#26214,#26215,#26216,#26217,#26218));
#7998=EDGE_LOOP('',(#26219,#26220,#26221,#26222));
#7999=EDGE_LOOP('',(#26223,#26224,#26225,#26226,#26227,#26228));
#8000=EDGE_LOOP('',(#26229,#26230,#26231,#26232,#26233,#26234));
#8001=EDGE_LOOP('',(#26235,#26236,#26237,#26238));
#8002=EDGE_LOOP('',(#26239,#26240,#26241,#26242,#26243,#26244));
#8003=EDGE_LOOP('',(#26245,#26246,#26247,#26248,#26249,#26250));
#8004=EDGE_LOOP('',(#26251,#26252,#26253,#26254));
#8005=EDGE_LOOP('',(#26255,#26256,#26257,#26258,#26259,#26260));
#8006=EDGE_LOOP('',(#26261,#26262,#26263,#26264,#26265,#26266));
#8007=EDGE_LOOP('',(#26267,#26268,#26269,#26270));
#8008=EDGE_LOOP('',(#26271,#26272,#26273,#26274,#26275,#26276));
#8009=EDGE_LOOP('',(#26277,#26278,#26279,#26280,#26281,#26282));
#8010=EDGE_LOOP('',(#26283,#26284,#26285,#26286));
#8011=EDGE_LOOP('',(#26287,#26288,#26289,#26290,#26291,#26292));
#8012=EDGE_LOOP('',(#26293,#26294,#26295,#26296,#26297,#26298));
#8013=EDGE_LOOP('',(#26299,#26300,#26301,#26302));
#8014=EDGE_LOOP('',(#26303,#26304,#26305,#26306,#26307,#26308));
#8015=EDGE_LOOP('',(#26309,#26310,#26311,#26312,#26313,#26314));
#8016=EDGE_LOOP('',(#26315,#26316,#26317,#26318));
#8017=EDGE_LOOP('',(#26319,#26320,#26321,#26322,#26323,#26324));
#8018=EDGE_LOOP('',(#26325,#26326,#26327,#26328,#26329,#26330));
#8019=EDGE_LOOP('',(#26331,#26332,#26333,#26334));
#8020=EDGE_LOOP('',(#26335,#26336,#26337,#26338,#26339,#26340));
#8021=EDGE_LOOP('',(#26341,#26342,#26343,#26344,#26345,#26346));
#8022=EDGE_LOOP('',(#26347,#26348,#26349,#26350));
#8023=EDGE_LOOP('',(#26351,#26352,#26353,#26354,#26355,#26356));
#8024=EDGE_LOOP('',(#26357,#26358,#26359,#26360,#26361,#26362));
#8025=EDGE_LOOP('',(#26363,#26364,#26365,#26366,#26367,#26368));
#8026=EDGE_LOOP('',(#26369,#26370,#26371,#26372,#26373,#26374));
#8027=EDGE_LOOP('',(#26375,#26376,#26377,#26378,#26379,#26380));
#8028=EDGE_LOOP('',(#26381,#26382,#26383,#26384,#26385,#26386));
#8029=EDGE_LOOP('',(#26387,#26388,#26389,#26390,#26391,#26392));
#8030=EDGE_LOOP('',(#26393,#26394,#26395,#26396,#26397,#26398));
#8031=EDGE_LOOP('',(#26399,#26400,#26401,#26402,#26403,#26404));
#8032=EDGE_LOOP('',(#26405,#26406,#26407,#26408,#26409,#26410));
#8033=EDGE_LOOP('',(#26411,#26412,#26413,#26414,#26415,#26416));
#8034=EDGE_LOOP('',(#26417,#26418,#26419,#26420,#26421,#26422));
#8035=EDGE_LOOP('',(#26423,#26424,#26425,#26426,#26427,#26428));
#8036=EDGE_LOOP('',(#26429,#26430,#26431,#26432,#26433,#26434,#26435));
#8037=EDGE_LOOP('',(#26436,#26437,#26438,#26439));
#8038=EDGE_LOOP('',(#26440,#26441,#26442,#26443));
#8039=EDGE_LOOP('',(#26444,#26445,#26446,#26447));
#8040=EDGE_LOOP('',(#26448,#26449,#26450,#26451));
#8041=EDGE_LOOP('',(#26452,#26453,#26454,#26455));
#8042=EDGE_LOOP('',(#26456,#26457,#26458,#26459));
#8043=EDGE_LOOP('',(#26460,#26461,#26462,#26463));
#8044=EDGE_LOOP('',(#26464,#26465,#26466,#26467));
#8045=EDGE_LOOP('',(#26468,#26469,#26470,#26471));
#8046=EDGE_LOOP('',(#26472,#26473,#26474,#26475));
#8047=EDGE_LOOP('',(#26476,#26477,#26478,#26479));
#8048=EDGE_LOOP('',(#26480,#26481,#26482,#26483));
#8049=EDGE_LOOP('',(#26484,#26485,#26486,#26487));
#8050=EDGE_LOOP('',(#26488,#26489,#26490,#26491));
#8051=EDGE_LOOP('',(#26492,#26493,#26494,#26495));
#8052=EDGE_LOOP('',(#26496,#26497,#26498,#26499));
#8053=EDGE_LOOP('',(#26500,#26501,#26502,#26503));
#8054=EDGE_LOOP('',(#26504,#26505,#26506,#26507));
#8055=EDGE_LOOP('',(#26508,#26509,#26510,#26511));
#8056=EDGE_LOOP('',(#26512,#26513,#26514,#26515));
#8057=EDGE_LOOP('',(#26516,#26517,#26518,#26519));
#8058=EDGE_LOOP('',(#26520,#26521,#26522,#26523));
#8059=EDGE_LOOP('',(#26524,#26525,#26526,#26527));
#8060=EDGE_LOOP('',(#26528,#26529,#26530,#26531));
#8061=EDGE_LOOP('',(#26532,#26533,#26534,#26535));
#8062=EDGE_LOOP('',(#26536,#26537,#26538,#26539));
#8063=EDGE_LOOP('',(#26540,#26541,#26542,#26543));
#8064=EDGE_LOOP('',(#26544,#26545,#26546));
#8065=EDGE_LOOP('',(#26547,#26548,#26549));
#8066=EDGE_LOOP('',(#26550,#26551,#26552,#26553));
#8067=EDGE_LOOP('',(#26554,#26555,#26556,#26557));
#8068=EDGE_LOOP('',(#26558,#26559,#26560,#26561));
#8069=EDGE_LOOP('',(#26562,#26563,#26564,#26565));
#8070=EDGE_LOOP('',(#26566,#26567,#26568,#26569));
#8071=EDGE_LOOP('',(#26570,#26571,#26572,#26573));
#8072=EDGE_LOOP('',(#26574,#26575,#26576,#26577));
#8073=EDGE_LOOP('',(#26578,#26579,#26580,#26581));
#8074=EDGE_LOOP('',(#26582,#26583,#26584,#26585));
#8075=EDGE_LOOP('',(#26586,#26587,#26588,#26589));
#8076=EDGE_LOOP('',(#26590,#26591,#26592,#26593));
#8077=EDGE_LOOP('',(#26594,#26595,#26596,#26597));
#8078=EDGE_LOOP('',(#26598,#26599,#26600,#26601));
#8079=EDGE_LOOP('',(#26602,#26603,#26604,#26605));
#8080=EDGE_LOOP('',(#26606,#26607,#26608,#26609));
#8081=EDGE_LOOP('',(#26610,#26611,#26612,#26613));
#8082=EDGE_LOOP('',(#26614,#26615,#26616,#26617));
#8083=EDGE_LOOP('',(#26618,#26619,#26620,#26621));
#8084=EDGE_LOOP('',(#26622,#26623,#26624,#26625));
#8085=EDGE_LOOP('',(#26626,#26627,#26628,#26629));
#8086=EDGE_LOOP('',(#26630,#26631,#26632,#26633));
#8087=EDGE_LOOP('',(#26634,#26635,#26636,#26637));
#8088=EDGE_LOOP('',(#26638,#26639,#26640,#26641));
#8089=EDGE_LOOP('',(#26642,#26643,#26644,#26645));
#8090=EDGE_LOOP('',(#26646,#26647,#26648,#26649));
#8091=EDGE_LOOP('',(#26650,#26651,#26652,#26653));
#8092=EDGE_LOOP('',(#26654,#26655,#26656,#26657));
#8093=EDGE_LOOP('',(#26658,#26659,#26660,#26661));
#8094=EDGE_LOOP('',(#26662,#26663,#26664,#26665));
#8095=EDGE_LOOP('',(#26666,#26667,#26668));
#8096=EDGE_LOOP('',(#26669,#26670,#26671,#26672,#26673));
#8097=EDGE_LOOP('',(#26674,#26675,#26676,#26677));
#8098=EDGE_LOOP('',(#26678,#26679,#26680,#26681));
#8099=EDGE_LOOP('',(#26682,#26683,#26684,#26685));
#8100=EDGE_LOOP('',(#26686,#26687,#26688,#26689));
#8101=EDGE_LOOP('',(#26690,#26691,#26692,#26693));
#8102=EDGE_LOOP('',(#26694,#26695,#26696,#26697));
#8103=EDGE_LOOP('',(#26698,#26699,#26700,#26701));
#8104=EDGE_LOOP('',(#26702,#26703,#26704,#26705));
#8105=EDGE_LOOP('',(#26706,#26707,#26708,#26709));
#8106=EDGE_LOOP('',(#26710,#26711,#26712,#26713));
#8107=EDGE_LOOP('',(#26714,#26715,#26716,#26717));
#8108=EDGE_LOOP('',(#26718,#26719,#26720,#26721));
#8109=EDGE_LOOP('',(#26722,#26723,#26724,#26725));
#8110=EDGE_LOOP('',(#26726,#26727,#26728,#26729));
#8111=EDGE_LOOP('',(#26730,#26731,#26732,#26733));
#8112=EDGE_LOOP('',(#26734,#26735,#26736,#26737));
#8113=EDGE_LOOP('',(#26738,#26739,#26740,#26741,#26742,#26743,#26744,#26745,
#26746,#26747));
#8114=EDGE_LOOP('',(#26748,#26749,#26750,#26751));
#8115=EDGE_LOOP('',(#26752,#26753,#26754,#26755,#26756,#26757,#26758,#26759,
#26760,#26761,#26762,#26763,#26764,#26765,#26766,#26767,#26768,#26769,#26770,
#26771,#26772,#26773,#26774,#26775,#26776,#26777,#26778,#26779,#26780,#26781,
#26782,#26783,#26784,#26785,#26786,#26787,#26788,#26789,#26790,#26791,#26792,
#26793,#26794,#26795,#26796,#26797,#26798,#26799,#26800,#26801,#26802,#26803,
#26804,#26805,#26806,#26807,#26808,#26809,#26810,#26811,#26812,#26813,#26814,
#26815,#26816,#26817,#26818,#26819,#26820,#26821,#26822,#26823,#26824,#26825,
#26826,#26827,#26828,#26829,#26830,#26831,#26832,#26833,#26834,#26835,#26836,
#26837,#26838,#26839,#26840,#26841,#26842,#26843,#26844,#26845,#26846,#26847,
#26848,#26849,#26850,#26851,#26852,#26853,#26854,#26855,#26856,#26857,#26858,
#26859,#26860,#26861,#26862,#26863,#26864,#26865,#26866,#26867,#26868,#26869,
#26870,#26871,#26872,#26873,#26874,#26875,#26876,#26877,#26878,#26879,#26880,
#26881,#26882,#26883,#26884,#26885,#26886,#26887,#26888,#26889,#26890,#26891,
#26892,#26893,#26894,#26895,#26896,#26897,#26898,#26899,#26900,#26901,#26902,
#26903,#26904,#26905,#26906,#26907,#26908,#26909,#26910,#26911,#26912,#26913,
#26914,#26915,#26916,#26917,#26918,#26919,#26920,#26921,#26922,#26923,#26924,
#26925,#26926,#26927,#26928,#26929,#26930,#26931,#26932,#26933,#26934,#26935,
#26936,#26937,#26938,#26939,#26940,#26941,#26942,#26943,#26944,#26945,#26946,
#26947,#26948,#26949,#26950,#26951,#26952,#26953,#26954,#26955,#26956,#26957,
#26958,#26959,#26960,#26961,#26962,#26963,#26964,#26965,#26966,#26967,#26968,
#26969,#26970,#26971,#26972,#26973,#26974,#26975,#26976,#26977,#26978,#26979,
#26980,#26981,#26982,#26983,#26984,#26985,#26986,#26987,#26988,#26989,#26990,
#26991,#26992,#26993,#26994,#26995,#26996,#26997,#26998,#26999,#27000,#27001,
#27002,#27003,#27004,#27005,#27006,#27007,#27008,#27009,#27010,#27011,#27012,
#27013,#27014,#27015,#27016,#27017,#27018,#27019,#27020,#27021,#27022,#27023,
#27024,#27025,#27026,#27027,#27028,#27029,#27030,#27031,#27032,#27033,#27034,
#27035,#27036,#27037,#27038,#27039,#27040,#27041,#27042,#27043,#27044,#27045,
#27046,#27047,#27048,#27049,#27050,#27051,#27052,#27053,#27054,#27055,#27056,
#27057,#27058,#27059,#27060,#27061,#27062,#27063,#27064,#27065,#27066,#27067,
#27068,#27069,#27070,#27071,#27072,#27073,#27074,#27075));
#8116=EDGE_LOOP('',(#27076,#27077,#27078,#27079,#27080,#27081,#27082,#27083,
#27084,#27085,#27086,#27087,#27088,#27089,#27090,#27091,#27092,#27093,#27094,
#27095,#27096,#27097,#27098,#27099,#27100,#27101,#27102,#27103,#27104,#27105,
#27106,#27107,#27108,#27109,#27110,#27111,#27112,#27113,#27114,#27115,#27116,
#27117,#27118,#27119,#27120,#27121,#27122,#27123,#27124,#27125,#27126,#27127,
#27128,#27129,#27130,#27131,#27132,#27133,#27134,#27135,#27136,#27137,#27138,
#27139,#27140,#27141,#27142,#27143,#27144,#27145,#27146,#27147,#27148,#27149,
#27150,#27151,#27152,#27153,#27154,#27155,#27156,#27157,#27158,#27159,#27160,
#27161,#27162,#27163,#27164,#27165,#27166,#27167,#27168,#27169,#27170,#27171,
#27172,#27173,#27174,#27175,#27176,#27177,#27178,#27179,#27180,#27181,#27182,
#27183,#27184,#27185,#27186,#27187,#27188,#27189,#27190,#27191,#27192,#27193,
#27194,#27195,#27196,#27197,#27198,#27199,#27200,#27201,#27202,#27203,#27204,
#27205,#27206,#27207,#27208,#27209,#27210,#27211,#27212,#27213,#27214,#27215,
#27216,#27217,#27218,#27219,#27220,#27221,#27222,#27223,#27224,#27225,#27226,
#27227,#27228,#27229,#27230,#27231,#27232,#27233,#27234,#27235,#27236,#27237,
#27238,#27239,#27240,#27241,#27242,#27243,#27244,#27245,#27246,#27247,#27248,
#27249,#27250,#27251,#27252,#27253,#27254,#27255,#27256,#27257,#27258,#27259,
#27260,#27261,#27262,#27263,#27264,#27265,#27266,#27267,#27268,#27269,#27270,
#27271,#27272,#27273,#27274,#27275,#27276,#27277,#27278,#27279,#27280,#27281,
#27282,#27283,#27284,#27285,#27286,#27287,#27288,#27289,#27290,#27291,#27292,
#27293,#27294,#27295,#27296,#27297,#27298,#27299,#27300,#27301,#27302,#27303,
#27304,#27305,#27306,#27307,#27308,#27309,#27310,#27311,#27312,#27313,#27314,
#27315,#27316,#27317,#27318,#27319,#27320,#27321,#27322,#27323,#27324,#27325,
#27326,#27327,#27328,#27329,#27330,#27331,#27332,#27333,#27334,#27335,#27336,
#27337,#27338,#27339,#27340,#27341,#27342,#27343,#27344,#27345,#27346,#27347,
#27348,#27349,#27350,#27351,#27352,#27353,#27354,#27355,#27356,#27357,#27358,
#27359,#27360,#27361,#27362,#27363,#27364,#27365,#27366,#27367,#27368,#27369,
#27370,#27371,#27372,#27373,#27374,#27375,#27376,#27377,#27378,#27379,#27380,
#27381,#27382,#27383,#27384,#27385,#27386,#27387,#27388,#27389,#27390,#27391,
#27392,#27393,#27394,#27395,#27396,#27397,#27398,#27399,#27400));
#8117=EDGE_LOOP('',(#27401,#27402,#27403,#27404,#27405));
#8118=EDGE_LOOP('',(#27406,#27407,#27408,#27409));
#8119=EDGE_LOOP('',(#27410,#27411,#27412,#27413));
#8120=EDGE_LOOP('',(#27414,#27415,#27416,#27417));
#8121=EDGE_LOOP('',(#27418,#27419,#27420,#27421));
#8122=EDGE_LOOP('',(#27422,#27423,#27424,#27425));
#8123=EDGE_LOOP('',(#27426,#27427,#27428,#27429));
#8124=EDGE_LOOP('',(#27430,#27431,#27432,#27433));
#8125=EDGE_LOOP('',(#27434,#27435,#27436,#27437));
#8126=EDGE_LOOP('',(#27438,#27439,#27440,#27441));
#8127=EDGE_LOOP('',(#27442,#27443,#27444,#27445));
#8128=EDGE_LOOP('',(#27446,#27447,#27448,#27449));
#8129=EDGE_LOOP('',(#27450,#27451,#27452,#27453));
#8130=EDGE_LOOP('',(#27454,#27455,#27456,#27457));
#8131=EDGE_LOOP('',(#27458,#27459,#27460,#27461));
#8132=EDGE_LOOP('',(#27462,#27463,#27464,#27465));
#8133=EDGE_LOOP('',(#27466,#27467,#27468,#27469));
#8134=EDGE_LOOP('',(#27470,#27471,#27472,#27473));
#8135=EDGE_LOOP('',(#27474,#27475,#27476,#27477));
#8136=EDGE_LOOP('',(#27478,#27479,#27480,#27481));
#8137=EDGE_LOOP('',(#27482,#27483,#27484,#27485));
#8138=EDGE_LOOP('',(#27486,#27487,#27488,#27489));
#8139=EDGE_LOOP('',(#27490,#27491,#27492,#27493));
#8140=EDGE_LOOP('',(#27494,#27495,#27496,#27497));
#8141=EDGE_LOOP('',(#27498,#27499,#27500,#27501));
#8142=EDGE_LOOP('',(#27502,#27503,#27504,#27505));
#8143=EDGE_LOOP('',(#27506,#27507,#27508,#27509));
#8144=EDGE_LOOP('',(#27510,#27511,#27512,#27513));
#8145=EDGE_LOOP('',(#27514,#27515,#27516,#27517));
#8146=EDGE_LOOP('',(#27518,#27519,#27520,#27521));
#8147=EDGE_LOOP('',(#27522,#27523,#27524,#27525));
#8148=EDGE_LOOP('',(#27526,#27527,#27528,#27529));
#8149=EDGE_LOOP('',(#27530,#27531,#27532,#27533));
#8150=EDGE_LOOP('',(#27534,#27535,#27536,#27537));
#8151=EDGE_LOOP('',(#27538,#27539,#27540,#27541));
#8152=EDGE_LOOP('',(#27542,#27543,#27544,#27545));
#8153=EDGE_LOOP('',(#27546,#27547,#27548,#27549));
#8154=EDGE_LOOP('',(#27550,#27551,#27552,#27553));
#8155=EDGE_LOOP('',(#27554,#27555,#27556,#27557));
#8156=EDGE_LOOP('',(#27558,#27559,#27560,#27561));
#8157=EDGE_LOOP('',(#27562,#27563,#27564,#27565));
#8158=EDGE_LOOP('',(#27566,#27567,#27568,#27569));
#8159=EDGE_LOOP('',(#27570,#27571,#27572,#27573));
#8160=EDGE_LOOP('',(#27574,#27575,#27576,#27577));
#8161=EDGE_LOOP('',(#27578,#27579,#27580,#27581));
#8162=EDGE_LOOP('',(#27582,#27583,#27584,#27585));
#8163=EDGE_LOOP('',(#27586,#27587,#27588,#27589));
#8164=EDGE_LOOP('',(#27590,#27591,#27592,#27593));
#8165=EDGE_LOOP('',(#27594,#27595,#27596,#27597));
#8166=EDGE_LOOP('',(#27598,#27599,#27600,#27601));
#8167=EDGE_LOOP('',(#27602,#27603,#27604,#27605));
#8168=EDGE_LOOP('',(#27606,#27607,#27608,#27609));
#8169=EDGE_LOOP('',(#27610,#27611,#27612,#27613));
#8170=EDGE_LOOP('',(#27614,#27615,#27616,#27617));
#8171=EDGE_LOOP('',(#27618,#27619,#27620,#27621));
#8172=EDGE_LOOP('',(#27622,#27623,#27624,#27625));
#8173=EDGE_LOOP('',(#27626,#27627,#27628,#27629));
#8174=EDGE_LOOP('',(#27630,#27631,#27632,#27633));
#8175=EDGE_LOOP('',(#27634,#27635,#27636,#27637));
#8176=EDGE_LOOP('',(#27638,#27639,#27640,#27641));
#8177=EDGE_LOOP('',(#27642,#27643,#27644,#27645));
#8178=EDGE_LOOP('',(#27646,#27647,#27648,#27649));
#8179=EDGE_LOOP('',(#27650,#27651,#27652,#27653));
#8180=EDGE_LOOP('',(#27654,#27655,#27656,#27657));
#8181=EDGE_LOOP('',(#27658,#27659,#27660,#27661));
#8182=EDGE_LOOP('',(#27662,#27663,#27664,#27665));
#8183=EDGE_LOOP('',(#27666,#27667,#27668,#27669));
#8184=EDGE_LOOP('',(#27670,#27671,#27672,#27673));
#8185=EDGE_LOOP('',(#27674,#27675,#27676,#27677));
#8186=EDGE_LOOP('',(#27678,#27679,#27680,#27681));
#8187=EDGE_LOOP('',(#27682,#27683,#27684,#27685));
#8188=EDGE_LOOP('',(#27686,#27687,#27688,#27689));
#8189=EDGE_LOOP('',(#27690,#27691,#27692,#27693));
#8190=EDGE_LOOP('',(#27694,#27695,#27696,#27697));
#8191=EDGE_LOOP('',(#27698,#27699,#27700,#27701));
#8192=EDGE_LOOP('',(#27702,#27703,#27704,#27705));
#8193=EDGE_LOOP('',(#27706,#27707,#27708,#27709));
#8194=EDGE_LOOP('',(#27710,#27711,#27712,#27713));
#8195=EDGE_LOOP('',(#27714,#27715,#27716,#27717));
#8196=EDGE_LOOP('',(#27718,#27719,#27720,#27721));
#8197=EDGE_LOOP('',(#27722,#27723,#27724,#27725));
#8198=EDGE_LOOP('',(#27726,#27727,#27728,#27729));
#8199=EDGE_LOOP('',(#27730,#27731,#27732,#27733));
#8200=EDGE_LOOP('',(#27734,#27735,#27736,#27737));
#8201=EDGE_LOOP('',(#27738,#27739,#27740,#27741));
#8202=EDGE_LOOP('',(#27742,#27743,#27744,#27745));
#8203=EDGE_LOOP('',(#27746,#27747,#27748,#27749));
#8204=EDGE_LOOP('',(#27750,#27751,#27752,#27753));
#8205=EDGE_LOOP('',(#27754,#27755,#27756,#27757));
#8206=EDGE_LOOP('',(#27758,#27759,#27760,#27761));
#8207=EDGE_LOOP('',(#27762,#27763,#27764,#27765));
#8208=EDGE_LOOP('',(#27766,#27767,#27768,#27769));
#8209=EDGE_LOOP('',(#27770,#27771,#27772,#27773));
#8210=EDGE_LOOP('',(#27774,#27775,#27776,#27777));
#8211=EDGE_LOOP('',(#27778,#27779,#27780,#27781));
#8212=EDGE_LOOP('',(#27782,#27783,#27784,#27785));
#8213=EDGE_LOOP('',(#27786,#27787,#27788,#27789));
#8214=EDGE_LOOP('',(#27790,#27791,#27792,#27793));
#8215=EDGE_LOOP('',(#27794,#27795,#27796,#27797));
#8216=EDGE_LOOP('',(#27798,#27799,#27800,#27801));
#8217=EDGE_LOOP('',(#27802,#27803,#27804,#27805));
#8218=EDGE_LOOP('',(#27806,#27807,#27808,#27809));
#8219=EDGE_LOOP('',(#27810,#27811,#27812,#27813));
#8220=EDGE_LOOP('',(#27814,#27815,#27816,#27817));
#8221=EDGE_LOOP('',(#27818,#27819,#27820,#27821));
#8222=EDGE_LOOP('',(#27822,#27823,#27824,#27825));
#8223=EDGE_LOOP('',(#27826,#27827,#27828,#27829));
#8224=EDGE_LOOP('',(#27830,#27831,#27832,#27833));
#8225=EDGE_LOOP('',(#27834,#27835,#27836,#27837));
#8226=EDGE_LOOP('',(#27838,#27839,#27840,#27841));
#8227=EDGE_LOOP('',(#27842,#27843,#27844,#27845));
#8228=EDGE_LOOP('',(#27846,#27847,#27848,#27849));
#8229=EDGE_LOOP('',(#27850,#27851,#27852,#27853));
#8230=EDGE_LOOP('',(#27854,#27855,#27856,#27857));
#8231=EDGE_LOOP('',(#27858,#27859,#27860,#27861));
#8232=EDGE_LOOP('',(#27862,#27863,#27864,#27865));
#8233=EDGE_LOOP('',(#27866,#27867,#27868,#27869));
#8234=EDGE_LOOP('',(#27870,#27871,#27872,#27873));
#8235=EDGE_LOOP('',(#27874,#27875,#27876,#27877));
#8236=EDGE_LOOP('',(#27878,#27879,#27880,#27881));
#8237=EDGE_LOOP('',(#27882,#27883,#27884,#27885));
#8238=EDGE_LOOP('',(#27886,#27887,#27888,#27889));
#8239=EDGE_LOOP('',(#27890,#27891,#27892,#27893));
#8240=EDGE_LOOP('',(#27894,#27895,#27896,#27897));
#8241=EDGE_LOOP('',(#27898,#27899,#27900,#27901));
#8242=EDGE_LOOP('',(#27902,#27903,#27904,#27905));
#8243=EDGE_LOOP('',(#27906,#27907,#27908,#27909));
#8244=EDGE_LOOP('',(#27910,#27911,#27912,#27913));
#8245=EDGE_LOOP('',(#27914,#27915,#27916,#27917));
#8246=EDGE_LOOP('',(#27918,#27919,#27920,#27921));
#8247=EDGE_LOOP('',(#27922,#27923,#27924,#27925));
#8248=EDGE_LOOP('',(#27926,#27927,#27928,#27929));
#8249=EDGE_LOOP('',(#27930,#27931,#27932,#27933));
#8250=EDGE_LOOP('',(#27934,#27935,#27936,#27937));
#8251=EDGE_LOOP('',(#27938,#27939,#27940,#27941));
#8252=EDGE_LOOP('',(#27942,#27943,#27944,#27945));
#8253=EDGE_LOOP('',(#27946,#27947,#27948,#27949));
#8254=EDGE_LOOP('',(#27950,#27951,#27952,#27953));
#8255=EDGE_LOOP('',(#27954,#27955,#27956,#27957));
#8256=EDGE_LOOP('',(#27958,#27959,#27960,#27961));
#8257=EDGE_LOOP('',(#27962,#27963,#27964,#27965));
#8258=EDGE_LOOP('',(#27966,#27967,#27968,#27969));
#8259=EDGE_LOOP('',(#27970,#27971,#27972,#27973));
#8260=EDGE_LOOP('',(#27974,#27975,#27976,#27977));
#8261=EDGE_LOOP('',(#27978,#27979,#27980,#27981));
#8262=EDGE_LOOP('',(#27982,#27983,#27984,#27985));
#8263=EDGE_LOOP('',(#27986,#27987,#27988,#27989));
#8264=EDGE_LOOP('',(#27990,#27991,#27992,#27993));
#8265=EDGE_LOOP('',(#27994,#27995,#27996,#27997));
#8266=EDGE_LOOP('',(#27998,#27999,#28000,#28001));
#8267=EDGE_LOOP('',(#28002,#28003,#28004,#28005));
#8268=EDGE_LOOP('',(#28006,#28007,#28008,#28009));
#8269=EDGE_LOOP('',(#28010,#28011,#28012,#28013));
#8270=EDGE_LOOP('',(#28014,#28015,#28016,#28017));
#8271=EDGE_LOOP('',(#28018,#28019,#28020,#28021));
#8272=EDGE_LOOP('',(#28022,#28023,#28024,#28025));
#8273=EDGE_LOOP('',(#28026,#28027,#28028,#28029));
#8274=EDGE_LOOP('',(#28030,#28031,#28032,#28033));
#8275=EDGE_LOOP('',(#28034,#28035,#28036,#28037));
#8276=EDGE_LOOP('',(#28038,#28039,#28040,#28041));
#8277=EDGE_LOOP('',(#28042,#28043,#28044,#28045));
#8278=EDGE_LOOP('',(#28046,#28047,#28048,#28049));
#8279=EDGE_LOOP('',(#28050,#28051,#28052,#28053));
#8280=EDGE_LOOP('',(#28054,#28055,#28056,#28057));
#8281=EDGE_LOOP('',(#28058,#28059,#28060,#28061));
#8282=EDGE_LOOP('',(#28062,#28063,#28064,#28065));
#8283=EDGE_LOOP('',(#28066,#28067,#28068,#28069));
#8284=EDGE_LOOP('',(#28070,#28071,#28072,#28073));
#8285=EDGE_LOOP('',(#28074,#28075,#28076,#28077));
#8286=EDGE_LOOP('',(#28078,#28079,#28080,#28081));
#8287=EDGE_LOOP('',(#28082,#28083,#28084,#28085));
#8288=EDGE_LOOP('',(#28086,#28087,#28088,#28089));
#8289=EDGE_LOOP('',(#28090,#28091,#28092,#28093));
#8290=EDGE_LOOP('',(#28094,#28095,#28096,#28097));
#8291=EDGE_LOOP('',(#28098,#28099,#28100,#28101));
#8292=EDGE_LOOP('',(#28102,#28103,#28104,#28105));
#8293=EDGE_LOOP('',(#28106,#28107,#28108,#28109));
#8294=EDGE_LOOP('',(#28110,#28111,#28112,#28113));
#8295=EDGE_LOOP('',(#28114,#28115,#28116,#28117));
#8296=EDGE_LOOP('',(#28118,#28119,#28120,#28121));
#8297=EDGE_LOOP('',(#28122,#28123,#28124,#28125));
#8298=EDGE_LOOP('',(#28126,#28127,#28128,#28129));
#8299=EDGE_LOOP('',(#28130,#28131,#28132,#28133));
#8300=EDGE_LOOP('',(#28134,#28135,#28136,#28137));
#8301=EDGE_LOOP('',(#28138,#28139,#28140,#28141));
#8302=EDGE_LOOP('',(#28142,#28143,#28144,#28145));
#8303=EDGE_LOOP('',(#28146,#28147,#28148,#28149));
#8304=EDGE_LOOP('',(#28150,#28151,#28152,#28153));
#8305=EDGE_LOOP('',(#28154,#28155,#28156,#28157));
#8306=EDGE_LOOP('',(#28158,#28159,#28160,#28161));
#8307=EDGE_LOOP('',(#28162,#28163,#28164,#28165));
#8308=EDGE_LOOP('',(#28166,#28167,#28168,#28169));
#8309=EDGE_LOOP('',(#28170,#28171,#28172,#28173));
#8310=EDGE_LOOP('',(#28174,#28175,#28176,#28177));
#8311=EDGE_LOOP('',(#28178,#28179,#28180,#28181));
#8312=EDGE_LOOP('',(#28182,#28183,#28184,#28185));
#8313=EDGE_LOOP('',(#28186,#28187,#28188,#28189));
#8314=EDGE_LOOP('',(#28190,#28191,#28192,#28193));
#8315=EDGE_LOOP('',(#28194,#28195,#28196,#28197));
#8316=EDGE_LOOP('',(#28198,#28199,#28200,#28201));
#8317=EDGE_LOOP('',(#28202,#28203,#28204,#28205));
#8318=EDGE_LOOP('',(#28206,#28207,#28208,#28209));
#8319=EDGE_LOOP('',(#28210,#28211,#28212,#28213));
#8320=EDGE_LOOP('',(#28214,#28215,#28216,#28217));
#8321=EDGE_LOOP('',(#28218,#28219,#28220,#28221));
#8322=EDGE_LOOP('',(#28222,#28223,#28224,#28225));
#8323=EDGE_LOOP('',(#28226,#28227,#28228,#28229));
#8324=EDGE_LOOP('',(#28230,#28231,#28232,#28233));
#8325=EDGE_LOOP('',(#28234,#28235,#28236,#28237));
#8326=EDGE_LOOP('',(#28238,#28239,#28240,#28241));
#8327=EDGE_LOOP('',(#28242,#28243,#28244,#28245));
#8328=EDGE_LOOP('',(#28246,#28247,#28248,#28249));
#8329=EDGE_LOOP('',(#28250,#28251,#28252,#28253));
#8330=EDGE_LOOP('',(#28254,#28255,#28256,#28257));
#8331=EDGE_LOOP('',(#28258,#28259,#28260,#28261));
#8332=EDGE_LOOP('',(#28262,#28263,#28264,#28265));
#8333=EDGE_LOOP('',(#28266,#28267,#28268,#28269));
#8334=EDGE_LOOP('',(#28270,#28271,#28272,#28273));
#8335=EDGE_LOOP('',(#28274,#28275,#28276,#28277));
#8336=EDGE_LOOP('',(#28278,#28279,#28280,#28281));
#8337=EDGE_LOOP('',(#28282,#28283,#28284,#28285));
#8338=EDGE_LOOP('',(#28286,#28287,#28288,#28289));
#8339=EDGE_LOOP('',(#28290,#28291,#28292,#28293));
#8340=EDGE_LOOP('',(#28294,#28295,#28296,#28297));
#8341=EDGE_LOOP('',(#28298,#28299,#28300,#28301));
#8342=EDGE_LOOP('',(#28302,#28303,#28304,#28305));
#8343=EDGE_LOOP('',(#28306,#28307,#28308,#28309));
#8344=EDGE_LOOP('',(#28310,#28311,#28312,#28313));
#8345=EDGE_LOOP('',(#28314,#28315,#28316,#28317));
#8346=EDGE_LOOP('',(#28318,#28319,#28320,#28321));
#8347=EDGE_LOOP('',(#28322,#28323,#28324,#28325));
#8348=EDGE_LOOP('',(#28326,#28327,#28328,#28329));
#8349=EDGE_LOOP('',(#28330,#28331,#28332,#28333));
#8350=EDGE_LOOP('',(#28334,#28335,#28336,#28337));
#8351=EDGE_LOOP('',(#28338,#28339,#28340,#28341));
#8352=EDGE_LOOP('',(#28342,#28343,#28344,#28345));
#8353=EDGE_LOOP('',(#28346,#28347,#28348,#28349));
#8354=EDGE_LOOP('',(#28350,#28351,#28352,#28353));
#8355=EDGE_LOOP('',(#28354,#28355,#28356,#28357));
#8356=EDGE_LOOP('',(#28358,#28359,#28360,#28361));
#8357=EDGE_LOOP('',(#28362,#28363,#28364,#28365));
#8358=EDGE_LOOP('',(#28366,#28367,#28368));
#8359=EDGE_LOOP('',(#28369));
#8360=EDGE_LOOP('',(#28370));
#8361=EDGE_LOOP('',(#28371,#28372,#28373,#28374));
#8362=EDGE_LOOP('',(#28375,#28376,#28377,#28378));
#8363=EDGE_LOOP('',(#28379,#28380,#28381,#28382));
#8364=EDGE_LOOP('',(#28383));
#8365=EDGE_LOOP('',(#28384));
#8366=EDGE_LOOP('',(#28385,#28386,#28387,#28388,#28389,#28390));
#8367=EDGE_LOOP('',(#28391,#28392,#28393,#28394));
#8368=EDGE_LOOP('',(#28395,#28396,#28397,#28398));
#8369=EDGE_LOOP('',(#28399,#28400,#28401,#28402));
#8370=EDGE_LOOP('',(#28403,#28404,#28405,#28406,#28407));
#8371=EDGE_LOOP('',(#28408,#28409,#28410,#28411));
#8372=EDGE_LOOP('',(#28412,#28413,#28414,#28415));
#8373=EDGE_LOOP('',(#28416,#28417,#28418,#28419,#28420,#28421,#28422,#28423,
#28424,#28425,#28426,#28427,#28428,#28429,#28430,#28431,#28432,#28433,#28434,
#28435,#28436,#28437,#28438,#28439,#28440,#28441,#28442,#28443,#28444,#28445,
#28446,#28447,#28448,#28449,#28450,#28451,#28452,#28453,#28454,#28455,#28456,
#28457,#28458,#28459,#28460,#28461,#28462,#28463,#28464,#28465,#28466,#28467,
#28468,#28469,#28470,#28471,#28472,#28473,#28474,#28475,#28476,#28477));
#8374=EDGE_LOOP('',(#28478,#28479,#28480,#28481,#28482,#28483,#28484,#28485,
#28486,#28487,#28488,#28489,#28490,#28491,#28492,#28493,#28494,#28495,#28496,
#28497,#28498,#28499,#28500,#28501,#28502,#28503,#28504,#28505,#28506,#28507,
#28508,#28509,#28510,#28511,#28512,#28513,#28514,#28515,#28516,#28517,#28518,
#28519,#28520,#28521,#28522,#28523,#28524,#28525,#28526,#28527,#28528,#28529,
#28530,#28531,#28532,#28533,#28534,#28535,#28536,#28537,#28538));
#8375=EDGE_LOOP('',(#28539,#28540,#28541,#28542));
#8376=EDGE_LOOP('',(#28543,#28544,#28545,#28546,#28547,#28548));
#8377=EDGE_LOOP('',(#28549,#28550,#28551,#28552,#28553));
#8378=EDGE_LOOP('',(#28554,#28555,#28556,#28557,#28558,#28559));
#8379=EDGE_LOOP('',(#28560,#28561,#28562,#28563,#28564,#28565));
#8380=EDGE_LOOP('',(#28566,#28567,#28568,#28569));
#8381=EDGE_LOOP('',(#28570,#28571,#28572,#28573,#28574,#28575));
#8382=EDGE_LOOP('',(#28576,#28577,#28578,#28579,#28580,#28581));
#8383=EDGE_LOOP('',(#28582,#28583,#28584,#28585));
#8384=EDGE_LOOP('',(#28586,#28587,#28588,#28589,#28590,#28591));
#8385=EDGE_LOOP('',(#28592,#28593,#28594,#28595,#28596,#28597));
#8386=EDGE_LOOP('',(#28598,#28599,#28600,#28601));
#8387=EDGE_LOOP('',(#28602,#28603,#28604,#28605,#28606,#28607));
#8388=EDGE_LOOP('',(#28608,#28609,#28610,#28611,#28612,#28613));
#8389=EDGE_LOOP('',(#28614,#28615,#28616,#28617));
#8390=EDGE_LOOP('',(#28618,#28619,#28620,#28621,#28622,#28623));
#8391=EDGE_LOOP('',(#28624,#28625,#28626,#28627,#28628,#28629));
#8392=EDGE_LOOP('',(#28630,#28631,#28632,#28633));
#8393=EDGE_LOOP('',(#28634,#28635,#28636,#28637,#28638,#28639));
#8394=EDGE_LOOP('',(#28640,#28641,#28642,#28643,#28644,#28645));
#8395=EDGE_LOOP('',(#28646,#28647,#28648,#28649));
#8396=EDGE_LOOP('',(#28650,#28651,#28652,#28653,#28654,#28655));
#8397=EDGE_LOOP('',(#28656,#28657,#28658,#28659,#28660,#28661));
#8398=EDGE_LOOP('',(#28662,#28663,#28664,#28665,#28666,#28667));
#8399=EDGE_LOOP('',(#28668,#28669,#28670,#28671,#28672,#28673));
#8400=EDGE_LOOP('',(#28674,#28675,#28676,#28677,#28678,#28679));
#8401=EDGE_LOOP('',(#28680,#28681,#28682,#28683,#28684,#28685));
#8402=EDGE_LOOP('',(#28686,#28687,#28688,#28689,#28690,#28691));
#8403=EDGE_LOOP('',(#28692,#28693,#28694,#28695,#28696,#28697));
#8404=EDGE_LOOP('',(#28698,#28699,#28700,#28701,#28702,#28703));
#8405=EDGE_LOOP('',(#28704,#28705,#28706,#28707,#28708,#28709));
#8406=EDGE_LOOP('',(#28710,#28711,#28712,#28713,#28714,#28715));
#8407=EDGE_LOOP('',(#28716,#28717,#28718,#28719,#28720,#28721));
#8408=EDGE_LOOP('',(#28722,#28723,#28724,#28725,#28726,#28727));
#8409=EDGE_LOOP('',(#28728,#28729,#28730,#28731,#28732,#28733));
#8410=EDGE_LOOP('',(#28734,#28735,#28736,#28737,#28738,#28739));
#8411=EDGE_LOOP('',(#28740,#28741,#28742,#28743,#28744,#28745));
#8412=EDGE_LOOP('',(#28746,#28747,#28748,#28749,#28750,#28751));
#8413=EDGE_LOOP('',(#28752,#28753,#28754,#28755,#28756,#28757));
#8414=EDGE_LOOP('',(#28758,#28759,#28760,#28761,#28762,#28763));
#8415=EDGE_LOOP('',(#28764,#28765,#28766,#28767,#28768,#28769));
#8416=EDGE_LOOP('',(#28770,#28771,#28772,#28773));
#8417=EDGE_LOOP('',(#28774,#28775,#28776,#28777,#28778,#28779));
#8418=EDGE_LOOP('',(#28780,#28781,#28782,#28783,#28784,#28785));
#8419=EDGE_LOOP('',(#28786,#28787,#28788,#28789));
#8420=EDGE_LOOP('',(#28790,#28791,#28792,#28793,#28794,#28795));
#8421=EDGE_LOOP('',(#28796,#28797,#28798,#28799,#28800,#28801));
#8422=EDGE_LOOP('',(#28802,#28803,#28804,#28805));
#8423=EDGE_LOOP('',(#28806,#28807,#28808,#28809,#28810,#28811));
#8424=EDGE_LOOP('',(#28812,#28813,#28814,#28815,#28816,#28817));
#8425=EDGE_LOOP('',(#28818,#28819,#28820,#28821));
#8426=EDGE_LOOP('',(#28822,#28823,#28824,#28825,#28826,#28827));
#8427=EDGE_LOOP('',(#28828,#28829,#28830,#28831,#28832,#28833));
#8428=EDGE_LOOP('',(#28834,#28835,#28836,#28837));
#8429=EDGE_LOOP('',(#28838,#28839,#28840,#28841,#28842,#28843));
#8430=EDGE_LOOP('',(#28844,#28845,#28846,#28847,#28848,#28849));
#8431=EDGE_LOOP('',(#28850,#28851,#28852,#28853));
#8432=EDGE_LOOP('',(#28854,#28855,#28856,#28857,#28858,#28859));
#8433=EDGE_LOOP('',(#28860,#28861,#28862,#28863,#28864,#28865));
#8434=EDGE_LOOP('',(#28866,#28867,#28868,#28869));
#8435=EDGE_LOOP('',(#28870,#28871,#28872,#28873,#28874,#28875));
#8436=EDGE_LOOP('',(#28876,#28877,#28878,#28879,#28880,#28881));
#8437=EDGE_LOOP('',(#28882,#28883,#28884,#28885));
#8438=EDGE_LOOP('',(#28886,#28887,#28888,#28889,#28890,#28891));
#8439=EDGE_LOOP('',(#28892,#28893,#28894,#28895,#28896,#28897));
#8440=EDGE_LOOP('',(#28898,#28899,#28900,#28901));
#8441=EDGE_LOOP('',(#28902,#28903,#28904,#28905,#28906,#28907));
#8442=EDGE_LOOP('',(#28908,#28909,#28910,#28911,#28912,#28913));
#8443=EDGE_LOOP('',(#28914,#28915,#28916,#28917));
#8444=EDGE_LOOP('',(#28918,#28919,#28920,#28921,#28922,#28923));
#8445=EDGE_LOOP('',(#28924,#28925,#28926,#28927,#28928,#28929));
#8446=EDGE_LOOP('',(#28930,#28931,#28932,#28933));
#8447=EDGE_LOOP('',(#28934,#28935,#28936,#28937,#28938,#28939));
#8448=EDGE_LOOP('',(#28940,#28941,#28942,#28943,#28944,#28945));
#8449=EDGE_LOOP('',(#28946,#28947,#28948,#28949));
#8450=EDGE_LOOP('',(#28950,#28951,#28952,#28953,#28954,#28955));
#8451=EDGE_LOOP('',(#28956,#28957,#28958,#28959,#28960,#28961));
#8452=EDGE_LOOP('',(#28962,#28963,#28964,#28965));
#8453=EDGE_LOOP('',(#28966,#28967,#28968,#28969,#28970,#28971));
#8454=EDGE_LOOP('',(#28972,#28973,#28974,#28975,#28976,#28977));
#8455=EDGE_LOOP('',(#28978,#28979,#28980,#28981));
#8456=EDGE_LOOP('',(#28982,#28983,#28984,#28985,#28986,#28987));
#8457=EDGE_LOOP('',(#28988,#28989,#28990,#28991,#28992,#28993));
#8458=EDGE_LOOP('',(#28994,#28995,#28996,#28997));
#8459=EDGE_LOOP('',(#28998,#28999,#29000,#29001,#29002,#29003));
#8460=EDGE_LOOP('',(#29004,#29005,#29006,#29007,#29008,#29009));
#8461=EDGE_LOOP('',(#29010,#29011,#29012,#29013));
#8462=EDGE_LOOP('',(#29014,#29015,#29016,#29017,#29018,#29019));
#8463=EDGE_LOOP('',(#29020,#29021,#29022,#29023,#29024,#29025));
#8464=EDGE_LOOP('',(#29026,#29027,#29028,#29029));
#8465=EDGE_LOOP('',(#29030,#29031,#29032,#29033,#29034,#29035));
#8466=EDGE_LOOP('',(#29036,#29037,#29038,#29039,#29040,#29041));
#8467=EDGE_LOOP('',(#29042,#29043,#29044,#29045));
#8468=EDGE_LOOP('',(#29046,#29047,#29048,#29049,#29050,#29051));
#8469=EDGE_LOOP('',(#29052,#29053,#29054,#29055,#29056,#29057));
#8470=EDGE_LOOP('',(#29058,#29059,#29060,#29061));
#8471=EDGE_LOOP('',(#29062,#29063,#29064,#29065,#29066,#29067));
#8472=EDGE_LOOP('',(#29068,#29069,#29070,#29071,#29072,#29073));
#8473=EDGE_LOOP('',(#29074,#29075,#29076,#29077));
#8474=EDGE_LOOP('',(#29078,#29079,#29080,#29081,#29082,#29083));
#8475=EDGE_LOOP('',(#29084,#29085,#29086,#29087,#29088,#29089));
#8476=EDGE_LOOP('',(#29090,#29091,#29092,#29093));
#8477=EDGE_LOOP('',(#29094,#29095,#29096,#29097,#29098,#29099));
#8478=EDGE_LOOP('',(#29100,#29101,#29102,#29103,#29104,#29105));
#8479=EDGE_LOOP('',(#29106,#29107,#29108,#29109));
#8480=EDGE_LOOP('',(#29110,#29111,#29112,#29113,#29114,#29115));
#8481=EDGE_LOOP('',(#29116,#29117,#29118,#29119,#29120,#29121));
#8482=EDGE_LOOP('',(#29122,#29123,#29124,#29125));
#8483=EDGE_LOOP('',(#29126,#29127,#29128,#29129,#29130,#29131));
#8484=EDGE_LOOP('',(#29132,#29133,#29134,#29135,#29136,#29137));
#8485=EDGE_LOOP('',(#29138,#29139,#29140,#29141));
#8486=EDGE_LOOP('',(#29142,#29143,#29144,#29145,#29146,#29147));
#8487=EDGE_LOOP('',(#29148,#29149,#29150,#29151,#29152,#29153));
#8488=EDGE_LOOP('',(#29154,#29155,#29156,#29157));
#8489=EDGE_LOOP('',(#29158,#29159,#29160,#29161,#29162,#29163));
#8490=EDGE_LOOP('',(#29164,#29165,#29166,#29167,#29168,#29169));
#8491=EDGE_LOOP('',(#29170,#29171,#29172,#29173));
#8492=EDGE_LOOP('',(#29174,#29175,#29176,#29177,#29178,#29179));
#8493=EDGE_LOOP('',(#29180,#29181,#29182,#29183,#29184,#29185));
#8494=EDGE_LOOP('',(#29186,#29187,#29188,#29189));
#8495=EDGE_LOOP('',(#29190,#29191,#29192,#29193,#29194,#29195));
#8496=EDGE_LOOP('',(#29196,#29197,#29198,#29199,#29200,#29201));
#8497=EDGE_LOOP('',(#29202,#29203,#29204,#29205));
#8498=EDGE_LOOP('',(#29206,#29207,#29208,#29209,#29210,#29211));
#8499=EDGE_LOOP('',(#29212,#29213,#29214,#29215,#29216,#29217));
#8500=EDGE_LOOP('',(#29218,#29219,#29220,#29221));
#8501=EDGE_LOOP('',(#29222,#29223,#29224,#29225,#29226,#29227));
#8502=EDGE_LOOP('',(#29228,#29229,#29230,#29231,#29232,#29233));
#8503=EDGE_LOOP('',(#29234,#29235,#29236,#29237));
#8504=EDGE_LOOP('',(#29238,#29239,#29240,#29241,#29242,#29243));
#8505=EDGE_LOOP('',(#29244,#29245,#29246,#29247,#29248,#29249));
#8506=EDGE_LOOP('',(#29250,#29251,#29252,#29253));
#8507=EDGE_LOOP('',(#29254,#29255,#29256,#29257,#29258,#29259));
#8508=EDGE_LOOP('',(#29260,#29261,#29262,#29263,#29264,#29265));
#8509=EDGE_LOOP('',(#29266,#29267,#29268,#29269));
#8510=EDGE_LOOP('',(#29270,#29271,#29272,#29273,#29274,#29275));
#8511=EDGE_LOOP('',(#29276,#29277,#29278,#29279,#29280,#29281));
#8512=EDGE_LOOP('',(#29282,#29283,#29284,#29285));
#8513=EDGE_LOOP('',(#29286,#29287,#29288,#29289,#29290,#29291));
#8514=EDGE_LOOP('',(#29292,#29293,#29294,#29295,#29296,#29297));
#8515=EDGE_LOOP('',(#29298,#29299,#29300,#29301));
#8516=EDGE_LOOP('',(#29302,#29303,#29304,#29305,#29306,#29307));
#8517=EDGE_LOOP('',(#29308,#29309,#29310,#29311,#29312,#29313));
#8518=EDGE_LOOP('',(#29314,#29315,#29316,#29317));
#8519=EDGE_LOOP('',(#29318,#29319,#29320,#29321,#29322,#29323));
#8520=EDGE_LOOP('',(#29324,#29325,#29326,#29327,#29328,#29329));
#8521=EDGE_LOOP('',(#29330,#29331,#29332,#29333));
#8522=EDGE_LOOP('',(#29334,#29335,#29336,#29337,#29338,#29339));
#8523=EDGE_LOOP('',(#29340,#29341,#29342,#29343,#29344,#29345));
#8524=EDGE_LOOP('',(#29346,#29347,#29348,#29349));
#8525=EDGE_LOOP('',(#29350,#29351,#29352,#29353,#29354,#29355));
#8526=EDGE_LOOP('',(#29356,#29357,#29358,#29359,#29360,#29361));
#8527=EDGE_LOOP('',(#29362,#29363,#29364,#29365));
#8528=EDGE_LOOP('',(#29366,#29367,#29368,#29369,#29370,#29371));
#8529=EDGE_LOOP('',(#29372,#29373,#29374,#29375,#29376,#29377));
#8530=EDGE_LOOP('',(#29378,#29379,#29380,#29381,#29382));
#8531=EDGE_LOOP('',(#29383,#29384,#29385,#29386,#29387,#29388));
#8532=EDGE_LOOP('',(#29389,#29390,#29391,#29392,#29393,#29394));
#8533=EDGE_LOOP('',(#29395,#29396,#29397,#29398));
#8534=EDGE_LOOP('',(#29399,#29400,#29401,#29402,#29403,#29404));
#8535=EDGE_LOOP('',(#29405,#29406,#29407,#29408,#29409,#29410));
#8536=EDGE_LOOP('',(#29411,#29412,#29413,#29414));
#8537=EDGE_LOOP('',(#29415,#29416,#29417,#29418,#29419,#29420));
#8538=EDGE_LOOP('',(#29421,#29422,#29423,#29424,#29425,#29426));
#8539=EDGE_LOOP('',(#29427,#29428,#29429,#29430));
#8540=EDGE_LOOP('',(#29431,#29432,#29433,#29434,#29435,#29436));
#8541=EDGE_LOOP('',(#29437,#29438,#29439,#29440,#29441,#29442));
#8542=EDGE_LOOP('',(#29443,#29444,#29445,#29446));
#8543=EDGE_LOOP('',(#29447,#29448,#29449,#29450,#29451,#29452));
#8544=EDGE_LOOP('',(#29453,#29454,#29455,#29456,#29457,#29458));
#8545=EDGE_LOOP('',(#29459,#29460,#29461,#29462));
#8546=EDGE_LOOP('',(#29463,#29464,#29465,#29466,#29467,#29468));
#8547=EDGE_LOOP('',(#29469,#29470,#29471,#29472,#29473,#29474));
#8548=EDGE_LOOP('',(#29475,#29476,#29477,#29478));
#8549=EDGE_LOOP('',(#29479,#29480,#29481,#29482,#29483,#29484));
#8550=EDGE_LOOP('',(#29485,#29486,#29487,#29488,#29489,#29490));
#8551=EDGE_LOOP('',(#29491,#29492,#29493,#29494));
#8552=EDGE_LOOP('',(#29495,#29496,#29497,#29498,#29499,#29500));
#8553=EDGE_LOOP('',(#29501,#29502,#29503,#29504,#29505,#29506));
#8554=EDGE_LOOP('',(#29507,#29508,#29509,#29510));
#8555=EDGE_LOOP('',(#29511,#29512,#29513,#29514,#29515,#29516));
#8556=EDGE_LOOP('',(#29517,#29518,#29519,#29520,#29521,#29522));
#8557=EDGE_LOOP('',(#29523,#29524,#29525,#29526));
#8558=EDGE_LOOP('',(#29527,#29528,#29529,#29530,#29531,#29532));
#8559=EDGE_LOOP('',(#29533,#29534,#29535,#29536,#29537,#29538));
#8560=EDGE_LOOP('',(#29539,#29540,#29541,#29542));
#8561=EDGE_LOOP('',(#29543,#29544,#29545,#29546,#29547,#29548));
#8562=EDGE_LOOP('',(#29549,#29550,#29551,#29552,#29553,#29554));
#8563=EDGE_LOOP('',(#29555,#29556,#29557,#29558));
#8564=EDGE_LOOP('',(#29559,#29560,#29561,#29562,#29563,#29564));
#8565=EDGE_LOOP('',(#29565,#29566,#29567,#29568,#29569,#29570));
#8566=EDGE_LOOP('',(#29571,#29572,#29573,#29574));
#8567=EDGE_LOOP('',(#29575,#29576,#29577,#29578,#29579,#29580));
#8568=EDGE_LOOP('',(#29581,#29582,#29583,#29584,#29585,#29586));
#8569=EDGE_LOOP('',(#29587,#29588,#29589,#29590));
#8570=EDGE_LOOP('',(#29591,#29592,#29593,#29594,#29595,#29596));
#8571=EDGE_LOOP('',(#29597,#29598,#29599,#29600,#29601,#29602));
#8572=EDGE_LOOP('',(#29603,#29604,#29605,#29606));
#8573=EDGE_LOOP('',(#29607,#29608,#29609,#29610,#29611,#29612));
#8574=EDGE_LOOP('',(#29613,#29614,#29615,#29616,#29617,#29618));
#8575=EDGE_LOOP('',(#29619,#29620,#29621,#29622));
#8576=EDGE_LOOP('',(#29623,#29624,#29625,#29626,#29627,#29628));
#8577=EDGE_LOOP('',(#29629,#29630,#29631,#29632,#29633,#29634));
#8578=EDGE_LOOP('',(#29635,#29636,#29637,#29638));
#8579=EDGE_LOOP('',(#29639,#29640,#29641,#29642,#29643,#29644));
#8580=EDGE_LOOP('',(#29645,#29646,#29647,#29648,#29649,#29650));
#8581=EDGE_LOOP('',(#29651,#29652,#29653,#29654));
#8582=EDGE_LOOP('',(#29655,#29656,#29657,#29658,#29659,#29660));
#8583=EDGE_LOOP('',(#29661,#29662,#29663,#29664,#29665,#29666));
#8584=EDGE_LOOP('',(#29667,#29668,#29669,#29670));
#8585=EDGE_LOOP('',(#29671,#29672,#29673,#29674,#29675,#29676));
#8586=EDGE_LOOP('',(#29677,#29678,#29679,#29680,#29681,#29682));
#8587=EDGE_LOOP('',(#29683,#29684,#29685,#29686));
#8588=EDGE_LOOP('',(#29687,#29688,#29689,#29690,#29691,#29692));
#8589=EDGE_LOOP('',(#29693,#29694,#29695,#29696,#29697,#29698));
#8590=EDGE_LOOP('',(#29699,#29700,#29701,#29702,#29703,#29704));
#8591=EDGE_LOOP('',(#29705,#29706,#29707,#29708,#29709,#29710));
#8592=EDGE_LOOP('',(#29711,#29712,#29713,#29714,#29715,#29716));
#8593=EDGE_LOOP('',(#29717,#29718,#29719,#29720,#29721,#29722));
#8594=EDGE_LOOP('',(#29723,#29724,#29725,#29726,#29727,#29728));
#8595=EDGE_LOOP('',(#29729,#29730,#29731,#29732,#29733,#29734));
#8596=EDGE_LOOP('',(#29735,#29736,#29737,#29738,#29739,#29740));
#8597=EDGE_LOOP('',(#29741,#29742,#29743,#29744,#29745,#29746));
#8598=EDGE_LOOP('',(#29747,#29748,#29749,#29750,#29751,#29752));
#8599=EDGE_LOOP('',(#29753,#29754,#29755,#29756,#29757,#29758));
#8600=EDGE_LOOP('',(#29759,#29760,#29761,#29762,#29763,#29764));
#8601=LINE('',#46050,#9847);
#8602=LINE('',#46052,#9848);
#8603=LINE('',#46054,#9849);
#8604=LINE('',#46055,#9850);
#8605=LINE('',#46058,#9851);
#8606=LINE('',#46060,#9852);
#8607=LINE('',#46062,#9853);
#8608=LINE('',#46063,#9854);
#8609=LINE('',#46066,#9855);
#8610=LINE('',#46068,#9856);
#8611=LINE('',#46069,#9857);
#8612=LINE('',#46071,#9858);
#8613=LINE('',#46074,#9859);
#8614=LINE('',#46075,#9860);
#8615=LINE('',#46077,#9861);
#8616=LINE('',#46080,#9862);
#8617=LINE('',#46082,#9863);
#8618=LINE('',#46083,#9864);
#8619=LINE('',#46086,#9865);
#8620=LINE('',#46087,#9866);
#8621=LINE('',#46089,#9867);
#8622=LINE('',#46094,#9868);
#8623=LINE('',#46118,#9869);
#8624=LINE('',#46124,#9870);
#8625=LINE('',#46130,#9871);
#8626=LINE('',#46137,#9872);
#8627=LINE('',#46140,#9873);
#8628=LINE('',#46143,#9874);
#8629=LINE('',#46145,#9875);
#8630=LINE('',#46146,#9876);
#8631=LINE('',#46152,#9877);
#8632=LINE('',#46155,#9878);
#8633=LINE('',#46158,#9879);
#8634=LINE('',#46160,#9880);
#8635=LINE('',#46161,#9881);
#8636=LINE('',#46167,#9882);
#8637=LINE('',#46170,#9883);
#8638=LINE('',#46173,#9884);
#8639=LINE('',#46175,#9885);
#8640=LINE('',#46176,#9886);
#8641=LINE('',#46182,#9887);
#8642=LINE('',#46185,#9888);
#8643=LINE('',#46190,#9889);
#8644=LINE('',#46193,#9890);
#8645=LINE('',#46200,#9891);
#8646=LINE('',#46207,#9892);
#8647=LINE('',#46212,#9893);
#8648=LINE('',#46216,#9894);
#8649=LINE('',#46220,#9895);
#8650=LINE('',#46224,#9896);
#8651=LINE('',#46229,#9897);
#8652=LINE('',#46232,#9898);
#8653=LINE('',#46234,#9899);
#8654=LINE('',#46238,#9900);
#8655=LINE('',#46240,#9901);
#8656=LINE('',#46246,#9902);
#8657=LINE('',#46285,#9903);
#8658=LINE('',#46326,#9904);
#8659=LINE('',#46402,#9905);
#8660=LINE('',#46480,#9906);
#8661=LINE('',#46556,#9907);
#8662=LINE('',#46632,#9908);
#8663=LINE('',#46708,#9909);
#8664=LINE('',#46784,#9910);
#8665=LINE('',#46862,#9911);
#8666=LINE('',#46940,#9912);
#8667=LINE('',#47016,#9913);
#8668=LINE('',#47092,#9914);
#8669=LINE('',#47168,#9915);
#8670=LINE('',#47244,#9916);
#8671=LINE('',#47322,#9917);
#8672=LINE('',#47398,#9918);
#8673=LINE('',#47476,#9919);
#8674=LINE('',#47552,#9920);
#8675=LINE('',#47628,#9921);
#8676=LINE('',#47704,#9922);
#8677=LINE('',#47780,#9923);
#8678=LINE('',#47858,#9924);
#8679=LINE('',#47936,#9925);
#8680=LINE('',#48012,#9926);
#8681=LINE('',#48088,#9927);
#8682=LINE('',#48164,#9928);
#8683=LINE('',#48240,#9929);
#8684=LINE('',#48318,#9930);
#8685=LINE('',#48394,#9931);
#8686=LINE('',#48419,#9932);
#8687=LINE('',#48433,#9933);
#8688=LINE('',#48509,#9934);
#8689=LINE('',#48585,#9935);
#8690=LINE('',#48663,#9936);
#8691=LINE('',#48739,#9937);
#8692=LINE('',#48817,#9938);
#8693=LINE('',#48893,#9939);
#8694=LINE('',#48969,#9940);
#8695=LINE('',#49045,#9941);
#8696=LINE('',#49121,#9942);
#8697=LINE('',#49199,#9943);
#8698=LINE('',#49275,#9944);
#8699=LINE('',#49353,#9945);
#8700=LINE('',#49429,#9946);
#8701=LINE('',#49505,#9947);
#8702=LINE('',#49581,#9948);
#8703=LINE('',#49657,#9949);
#8704=LINE('',#49733,#9950);
#8705=LINE('',#49811,#9951);
#8706=LINE('',#49887,#9952);
#8707=LINE('',#49965,#9953);
#8708=LINE('',#50041,#9954);
#8709=LINE('',#50117,#9955);
#8710=LINE('',#50193,#9956);
#8711=LINE('',#50269,#9957);
#8712=LINE('',#50347,#9958);
#8713=LINE('',#50423,#9959);
#8714=LINE('',#50501,#9960);
#8715=LINE('',#50577,#9961);
#8716=LINE('',#50772,#9962);
#8717=LINE('',#50775,#9963);
#8718=LINE('',#50781,#9964);
#8719=LINE('',#50784,#9965);
#8720=LINE('',#50790,#9966);
#8721=LINE('',#50793,#9967);
#8722=LINE('',#50799,#9968);
#8723=LINE('',#50802,#9969);
#8724=LINE('',#50808,#9970);
#8725=LINE('',#50811,#9971);
#8726=LINE('',#50817,#9972);
#8727=LINE('',#50820,#9973);
#8728=LINE('',#50826,#9974);
#8729=LINE('',#50829,#9975);
#8730=LINE('',#50835,#9976);
#8731=LINE('',#50838,#9977);
#8732=LINE('',#50844,#9978);
#8733=LINE('',#50847,#9979);
#8734=LINE('',#50853,#9980);
#8735=LINE('',#50856,#9981);
#8736=LINE('',#50862,#9982);
#8737=LINE('',#50865,#9983);
#8738=LINE('',#50871,#9984);
#8739=LINE('',#50874,#9985);
#8740=LINE('',#50880,#9986);
#8741=LINE('',#50883,#9987);
#8742=LINE('',#50889,#9988);
#8743=LINE('',#50892,#9989);
#8744=LINE('',#50898,#9990);
#8745=LINE('',#50901,#9991);
#8746=LINE('',#50932,#9992);
#8747=LINE('',#51872,#9993);
#8748=LINE('',#52806,#9994);
#8749=LINE('',#52817,#9995);
#8750=LINE('',#53302,#9996);
#8751=LINE('',#53305,#9997);
#8752=LINE('',#53308,#9998);
#8753=LINE('',#53310,#9999);
#8754=LINE('',#53314,#10000);
#8755=LINE('',#53316,#10001);
#8756=LINE('',#53320,#10002);
#8757=LINE('',#53322,#10003);
#8758=LINE('',#53326,#10004);
#8759=LINE('',#53328,#10005);
#8760=LINE('',#53332,#10006);
#8761=LINE('',#53334,#10007);
#8762=LINE('',#53338,#10008);
#8763=LINE('',#53340,#10009);
#8764=LINE('',#53344,#10010);
#8765=LINE('',#53346,#10011);
#8766=LINE('',#53350,#10012);
#8767=LINE('',#53352,#10013);
#8768=LINE('',#53356,#10014);
#8769=LINE('',#53358,#10015);
#8770=LINE('',#53362,#10016);
#8771=LINE('',#53364,#10017);
#8772=LINE('',#53368,#10018);
#8773=LINE('',#53370,#10019);
#8774=LINE('',#53374,#10020);
#8775=LINE('',#53376,#10021);
#8776=LINE('',#53380,#10022);
#8777=LINE('',#53382,#10023);
#8778=LINE('',#53386,#10024);
#8779=LINE('',#53388,#10025);
#8780=LINE('',#53392,#10026);
#8781=LINE('',#53394,#10027);
#8782=LINE('',#53398,#10028);
#8783=LINE('',#53400,#10029);
#8784=LINE('',#53404,#10030);
#8785=LINE('',#53406,#10031);
#8786=LINE('',#53410,#10032);
#8787=LINE('',#53412,#10033);
#8788=LINE('',#53416,#10034);
#8789=LINE('',#53418,#10035);
#8790=LINE('',#53422,#10036);
#8791=LINE('',#53424,#10037);
#8792=LINE('',#53428,#10038);
#8793=LINE('',#53430,#10039);
#8794=LINE('',#53434,#10040);
#8795=LINE('',#53436,#10041);
#8796=LINE('',#53440,#10042);
#8797=LINE('',#53442,#10043);
#8798=LINE('',#53446,#10044);
#8799=LINE('',#53448,#10045);
#8800=LINE('',#53452,#10046);
#8801=LINE('',#53454,#10047);
#8802=LINE('',#53458,#10048);
#8803=LINE('',#53460,#10049);
#8804=LINE('',#53464,#10050);
#8805=LINE('',#53466,#10051);
#8806=LINE('',#53470,#10052);
#8807=LINE('',#53472,#10053);
#8808=LINE('',#53476,#10054);
#8809=LINE('',#53478,#10055);
#8810=LINE('',#53482,#10056);
#8811=LINE('',#53484,#10057);
#8812=LINE('',#53488,#10058);
#8813=LINE('',#53490,#10059);
#8814=LINE('',#53494,#10060);
#8815=LINE('',#53496,#10061);
#8816=LINE('',#53500,#10062);
#8817=LINE('',#53502,#10063);
#8818=LINE('',#53506,#10064);
#8819=LINE('',#53508,#10065);
#8820=LINE('',#53512,#10066);
#8821=LINE('',#53514,#10067);
#8822=LINE('',#53518,#10068);
#8823=LINE('',#53520,#10069);
#8824=LINE('',#53524,#10070);
#8825=LINE('',#53526,#10071);
#8826=LINE('',#53530,#10072);
#8827=LINE('',#53532,#10073);
#8828=LINE('',#53536,#10074);
#8829=LINE('',#53538,#10075);
#8830=LINE('',#53542,#10076);
#8831=LINE('',#53544,#10077);
#8832=LINE('',#53548,#10078);
#8833=LINE('',#53550,#10079);
#8834=LINE('',#53554,#10080);
#8835=LINE('',#53556,#10081);
#8836=LINE('',#53560,#10082);
#8837=LINE('',#53562,#10083);
#8838=LINE('',#53566,#10084);
#8839=LINE('',#53568,#10085);
#8840=LINE('',#53572,#10086);
#8841=LINE('',#53574,#10087);
#8842=LINE('',#53578,#10088);
#8843=LINE('',#53580,#10089);
#8844=LINE('',#53584,#10090);
#8845=LINE('',#53586,#10091);
#8846=LINE('',#53590,#10092);
#8847=LINE('',#53592,#10093);
#8848=LINE('',#53596,#10094);
#8849=LINE('',#53598,#10095);
#8850=LINE('',#53602,#10096);
#8851=LINE('',#53604,#10097);
#8852=LINE('',#53608,#10098);
#8853=LINE('',#53610,#10099);
#8854=LINE('',#53614,#10100);
#8855=LINE('',#53616,#10101);
#8856=LINE('',#53620,#10102);
#8857=LINE('',#53622,#10103);
#8858=LINE('',#53626,#10104);
#8859=LINE('',#53628,#10105);
#8860=LINE('',#53632,#10106);
#8861=LINE('',#53634,#10107);
#8862=LINE('',#53638,#10108);
#8863=LINE('',#53640,#10109);
#8864=LINE('',#53644,#10110);
#8865=LINE('',#53646,#10111);
#8866=LINE('',#53650,#10112);
#8867=LINE('',#53652,#10113);
#8868=LINE('',#53656,#10114);
#8869=LINE('',#53658,#10115);
#8870=LINE('',#53662,#10116);
#8871=LINE('',#53664,#10117);
#8872=LINE('',#53668,#10118);
#8873=LINE('',#53670,#10119);
#8874=LINE('',#53674,#10120);
#8875=LINE('',#53676,#10121);
#8876=LINE('',#53680,#10122);
#8877=LINE('',#53682,#10123);
#8878=LINE('',#53686,#10124);
#8879=LINE('',#53689,#10125);
#8880=LINE('',#53692,#10126);
#8881=LINE('',#53695,#10127);
#8882=LINE('',#53698,#10128);
#8883=LINE('',#53701,#10129);
#8884=LINE('',#53704,#10130);
#8885=LINE('',#53707,#10131);
#8886=LINE('',#53710,#10132);
#8887=LINE('',#53713,#10133);
#8888=LINE('',#53716,#10134);
#8889=LINE('',#53719,#10135);
#8890=LINE('',#53722,#10136);
#8891=LINE('',#53725,#10137);
#8892=LINE('',#53728,#10138);
#8893=LINE('',#53731,#10139);
#8894=LINE('',#53734,#10140);
#8895=LINE('',#53737,#10141);
#8896=LINE('',#53740,#10142);
#8897=LINE('',#53743,#10143);
#8898=LINE('',#53746,#10144);
#8899=LINE('',#53749,#10145);
#8900=LINE('',#53752,#10146);
#8901=LINE('',#53755,#10147);
#8902=LINE('',#53758,#10148);
#8903=LINE('',#53761,#10149);
#8904=LINE('',#53764,#10150);
#8905=LINE('',#53767,#10151);
#8906=LINE('',#53770,#10152);
#8907=LINE('',#53772,#10153);
#8908=LINE('',#54021,#10154);
#8909=LINE('',#54023,#10155);
#8910=LINE('',#54032,#10156);
#8911=LINE('',#54034,#10157);
#8912=LINE('',#54036,#10158);
#8913=LINE('',#54038,#10159);
#8914=LINE('',#54040,#10160);
#8915=LINE('',#54041,#10161);
#8916=LINE('',#54043,#10162);
#8917=LINE('',#54044,#10163);
#8918=LINE('',#54046,#10164);
#8919=LINE('',#54048,#10165);
#8920=LINE('',#54050,#10166);
#8921=LINE('',#54052,#10167);
#8922=LINE('',#55574,#10168);
#8923=LINE('',#55577,#10169);
#8924=LINE('',#55579,#10170);
#8925=LINE('',#55582,#10171);
#8926=LINE('',#55584,#10172);
#8927=LINE('',#55587,#10173);
#8928=LINE('',#55589,#10174);
#8929=LINE('',#55592,#10175);
#8930=LINE('',#55594,#10176);
#8931=LINE('',#55597,#10177);
#8932=LINE('',#55599,#10178);
#8933=LINE('',#55602,#10179);
#8934=LINE('',#55604,#10180);
#8935=LINE('',#55607,#10181);
#8936=LINE('',#55609,#10182);
#8937=LINE('',#55630,#10183);
#8938=LINE('',#55632,#10184);
#8939=LINE('',#55635,#10185);
#8940=LINE('',#55637,#10186);
#8941=LINE('',#55640,#10187);
#8942=LINE('',#55642,#10188);
#8943=LINE('',#55645,#10189);
#8944=LINE('',#55647,#10190);
#8945=LINE('',#55650,#10191);
#8946=LINE('',#55652,#10192);
#8947=LINE('',#55655,#10193);
#8948=LINE('',#55657,#10194);
#8949=LINE('',#55660,#10195);
#8950=LINE('',#55662,#10196);
#8951=LINE('',#55665,#10197);
#8952=LINE('',#55667,#10198);
#8953=LINE('',#55670,#10199);
#8954=LINE('',#55672,#10200);
#8955=LINE('',#55675,#10201);
#8956=LINE('',#55677,#10202);
#8957=LINE('',#55680,#10203);
#8958=LINE('',#55682,#10204);
#8959=LINE('',#55685,#10205);
#8960=LINE('',#55687,#10206);
#8961=LINE('',#55690,#10207);
#8962=LINE('',#55692,#10208);
#8963=LINE('',#55695,#10209);
#8964=LINE('',#55697,#10210);
#8965=LINE('',#55700,#10211);
#8966=LINE('',#55702,#10212);
#8967=LINE('',#55705,#10213);
#8968=LINE('',#55707,#10214);
#8969=LINE('',#55710,#10215);
#8970=LINE('',#55712,#10216);
#8971=LINE('',#55715,#10217);
#8972=LINE('',#55717,#10218);
#8973=LINE('',#55720,#10219);
#8974=LINE('',#55722,#10220);
#8975=LINE('',#55725,#10221);
#8976=LINE('',#55727,#10222);
#8977=LINE('',#55730,#10223);
#8978=LINE('',#55732,#10224);
#8979=LINE('',#55735,#10225);
#8980=LINE('',#55737,#10226);
#8981=LINE('',#55740,#10227);
#8982=LINE('',#55742,#10228);
#8983=LINE('',#55745,#10229);
#8984=LINE('',#55747,#10230);
#8985=LINE('',#55750,#10231);
#8986=LINE('',#55752,#10232);
#8987=LINE('',#55755,#10233);
#8988=LINE('',#55757,#10234);
#8989=LINE('',#55760,#10235);
#8990=LINE('',#55762,#10236);
#8991=LINE('',#55765,#10237);
#8992=LINE('',#55767,#10238);
#8993=LINE('',#55770,#10239);
#8994=LINE('',#55772,#10240);
#8995=LINE('',#55775,#10241);
#8996=LINE('',#55777,#10242);
#8997=LINE('',#55780,#10243);
#8998=LINE('',#55782,#10244);
#8999=LINE('',#55785,#10245);
#9000=LINE('',#55787,#10246);
#9001=LINE('',#55790,#10247);
#9002=LINE('',#55792,#10248);
#9003=LINE('',#55795,#10249);
#9004=LINE('',#55797,#10250);
#9005=LINE('',#55800,#10251);
#9006=LINE('',#55802,#10252);
#9007=LINE('',#55805,#10253);
#9008=LINE('',#55807,#10254);
#9009=LINE('',#55810,#10255);
#9010=LINE('',#55812,#10256);
#9011=LINE('',#55815,#10257);
#9012=LINE('',#55817,#10258);
#9013=LINE('',#55820,#10259);
#9014=LINE('',#55822,#10260);
#9015=LINE('',#55825,#10261);
#9016=LINE('',#55827,#10262);
#9017=LINE('',#55830,#10263);
#9018=LINE('',#55832,#10264);
#9019=LINE('',#55835,#10265);
#9020=LINE('',#55837,#10266);
#9021=LINE('',#55840,#10267);
#9022=LINE('',#55842,#10268);
#9023=LINE('',#55845,#10269);
#9024=LINE('',#55847,#10270);
#9025=LINE('',#55850,#10271);
#9026=LINE('',#55852,#10272);
#9027=LINE('',#55855,#10273);
#9028=LINE('',#55857,#10274);
#9029=LINE('',#55860,#10275);
#9030=LINE('',#55862,#10276);
#9031=LINE('',#55865,#10277);
#9032=LINE('',#55867,#10278);
#9033=LINE('',#55870,#10279);
#9034=LINE('',#55872,#10280);
#9035=LINE('',#55875,#10281);
#9036=LINE('',#55877,#10282);
#9037=LINE('',#55880,#10283);
#9038=LINE('',#55882,#10284);
#9039=LINE('',#55885,#10285);
#9040=LINE('',#55887,#10286);
#9041=LINE('',#55890,#10287);
#9042=LINE('',#55892,#10288);
#9043=LINE('',#55895,#10289);
#9044=LINE('',#55897,#10290);
#9045=LINE('',#55900,#10291);
#9046=LINE('',#55902,#10292);
#9047=LINE('',#55905,#10293);
#9048=LINE('',#55907,#10294);
#9049=LINE('',#55910,#10295);
#9050=LINE('',#55912,#10296);
#9051=LINE('',#55915,#10297);
#9052=LINE('',#55917,#10298);
#9053=LINE('',#55935,#10299);
#9054=LINE('',#55974,#10300);
#9055=LINE('',#56015,#10301);
#9056=LINE('',#56091,#10302);
#9057=LINE('',#56169,#10303);
#9058=LINE('',#56245,#10304);
#9059=LINE('',#56321,#10305);
#9060=LINE('',#56397,#10306);
#9061=LINE('',#56473,#10307);
#9062=LINE('',#56551,#10308);
#9063=LINE('',#56629,#10309);
#9064=LINE('',#56705,#10310);
#9065=LINE('',#56781,#10311);
#9066=LINE('',#56857,#10312);
#9067=LINE('',#56933,#10313);
#9068=LINE('',#57011,#10314);
#9069=LINE('',#57087,#10315);
#9070=LINE('',#57165,#10316);
#9071=LINE('',#57241,#10317);
#9072=LINE('',#57317,#10318);
#9073=LINE('',#57393,#10319);
#9074=LINE('',#57469,#10320);
#9075=LINE('',#57547,#10321);
#9076=LINE('',#57625,#10322);
#9077=LINE('',#57701,#10323);
#9078=LINE('',#57777,#10324);
#9079=LINE('',#57853,#10325);
#9080=LINE('',#57929,#10326);
#9081=LINE('',#58007,#10327);
#9082=LINE('',#58083,#10328);
#9083=LINE('',#58108,#10329);
#9084=LINE('',#58122,#10330);
#9085=LINE('',#58198,#10331);
#9086=LINE('',#58274,#10332);
#9087=LINE('',#58352,#10333);
#9088=LINE('',#58428,#10334);
#9089=LINE('',#58506,#10335);
#9090=LINE('',#58582,#10336);
#9091=LINE('',#58658,#10337);
#9092=LINE('',#58734,#10338);
#9093=LINE('',#58810,#10339);
#9094=LINE('',#58888,#10340);
#9095=LINE('',#58964,#10341);
#9096=LINE('',#59042,#10342);
#9097=LINE('',#59118,#10343);
#9098=LINE('',#59194,#10344);
#9099=LINE('',#59270,#10345);
#9100=LINE('',#59346,#10346);
#9101=LINE('',#59422,#10347);
#9102=LINE('',#59500,#10348);
#9103=LINE('',#59576,#10349);
#9104=LINE('',#59654,#10350);
#9105=LINE('',#59730,#10351);
#9106=LINE('',#59806,#10352);
#9107=LINE('',#59882,#10353);
#9108=LINE('',#59958,#10354);
#9109=LINE('',#60036,#10355);
#9110=LINE('',#60112,#10356);
#9111=LINE('',#60190,#10357);
#9112=LINE('',#60266,#10358);
#9113=LINE('',#60461,#10359);
#9114=LINE('',#60464,#10360);
#9115=LINE('',#60470,#10361);
#9116=LINE('',#60473,#10362);
#9117=LINE('',#60479,#10363);
#9118=LINE('',#60482,#10364);
#9119=LINE('',#60488,#10365);
#9120=LINE('',#60491,#10366);
#9121=LINE('',#60497,#10367);
#9122=LINE('',#60500,#10368);
#9123=LINE('',#60506,#10369);
#9124=LINE('',#60509,#10370);
#9125=LINE('',#60515,#10371);
#9126=LINE('',#60518,#10372);
#9127=LINE('',#60524,#10373);
#9128=LINE('',#60527,#10374);
#9129=LINE('',#60533,#10375);
#9130=LINE('',#60536,#10376);
#9131=LINE('',#60542,#10377);
#9132=LINE('',#60545,#10378);
#9133=LINE('',#60551,#10379);
#9134=LINE('',#60554,#10380);
#9135=LINE('',#60560,#10381);
#9136=LINE('',#60563,#10382);
#9137=LINE('',#60569,#10383);
#9138=LINE('',#60572,#10384);
#9139=LINE('',#60578,#10385);
#9140=LINE('',#60581,#10386);
#9141=LINE('',#60587,#10387);
#9142=LINE('',#60590,#10388);
#9143=LINE('',#60621,#10389);
#9144=LINE('',#61561,#10390);
#9145=LINE('',#62495,#10391);
#9146=LINE('',#62506,#10392);
#9147=LINE('',#62991,#10393);
#9148=LINE('',#62994,#10394);
#9149=LINE('',#62997,#10395);
#9150=LINE('',#62999,#10396);
#9151=LINE('',#63003,#10397);
#9152=LINE('',#63005,#10398);
#9153=LINE('',#63009,#10399);
#9154=LINE('',#63011,#10400);
#9155=LINE('',#63015,#10401);
#9156=LINE('',#63017,#10402);
#9157=LINE('',#63021,#10403);
#9158=LINE('',#63023,#10404);
#9159=LINE('',#63027,#10405);
#9160=LINE('',#63029,#10406);
#9161=LINE('',#63033,#10407);
#9162=LINE('',#63035,#10408);
#9163=LINE('',#63039,#10409);
#9164=LINE('',#63041,#10410);
#9165=LINE('',#63045,#10411);
#9166=LINE('',#63047,#10412);
#9167=LINE('',#63051,#10413);
#9168=LINE('',#63053,#10414);
#9169=LINE('',#63057,#10415);
#9170=LINE('',#63059,#10416);
#9171=LINE('',#63063,#10417);
#9172=LINE('',#63065,#10418);
#9173=LINE('',#63069,#10419);
#9174=LINE('',#63071,#10420);
#9175=LINE('',#63075,#10421);
#9176=LINE('',#63077,#10422);
#9177=LINE('',#63081,#10423);
#9178=LINE('',#63083,#10424);
#9179=LINE('',#63087,#10425);
#9180=LINE('',#63089,#10426);
#9181=LINE('',#63093,#10427);
#9182=LINE('',#63095,#10428);
#9183=LINE('',#63099,#10429);
#9184=LINE('',#63101,#10430);
#9185=LINE('',#63105,#10431);
#9186=LINE('',#63107,#10432);
#9187=LINE('',#63111,#10433);
#9188=LINE('',#63113,#10434);
#9189=LINE('',#63117,#10435);
#9190=LINE('',#63119,#10436);
#9191=LINE('',#63123,#10437);
#9192=LINE('',#63125,#10438);
#9193=LINE('',#63129,#10439);
#9194=LINE('',#63131,#10440);
#9195=LINE('',#63135,#10441);
#9196=LINE('',#63137,#10442);
#9197=LINE('',#63141,#10443);
#9198=LINE('',#63143,#10444);
#9199=LINE('',#63147,#10445);
#9200=LINE('',#63149,#10446);
#9201=LINE('',#63153,#10447);
#9202=LINE('',#63155,#10448);
#9203=LINE('',#63159,#10449);
#9204=LINE('',#63161,#10450);
#9205=LINE('',#63165,#10451);
#9206=LINE('',#63167,#10452);
#9207=LINE('',#63171,#10453);
#9208=LINE('',#63173,#10454);
#9209=LINE('',#63177,#10455);
#9210=LINE('',#63179,#10456);
#9211=LINE('',#63183,#10457);
#9212=LINE('',#63185,#10458);
#9213=LINE('',#63189,#10459);
#9214=LINE('',#63191,#10460);
#9215=LINE('',#63195,#10461);
#9216=LINE('',#63197,#10462);
#9217=LINE('',#63201,#10463);
#9218=LINE('',#63203,#10464);
#9219=LINE('',#63207,#10465);
#9220=LINE('',#63209,#10466);
#9221=LINE('',#63213,#10467);
#9222=LINE('',#63215,#10468);
#9223=LINE('',#63219,#10469);
#9224=LINE('',#63221,#10470);
#9225=LINE('',#63225,#10471);
#9226=LINE('',#63227,#10472);
#9227=LINE('',#63231,#10473);
#9228=LINE('',#63233,#10474);
#9229=LINE('',#63237,#10475);
#9230=LINE('',#63239,#10476);
#9231=LINE('',#63243,#10477);
#9232=LINE('',#63245,#10478);
#9233=LINE('',#63249,#10479);
#9234=LINE('',#63251,#10480);
#9235=LINE('',#63255,#10481);
#9236=LINE('',#63257,#10482);
#9237=LINE('',#63261,#10483);
#9238=LINE('',#63263,#10484);
#9239=LINE('',#63267,#10485);
#9240=LINE('',#63269,#10486);
#9241=LINE('',#63273,#10487);
#9242=LINE('',#63275,#10488);
#9243=LINE('',#63279,#10489);
#9244=LINE('',#63281,#10490);
#9245=LINE('',#63285,#10491);
#9246=LINE('',#63287,#10492);
#9247=LINE('',#63291,#10493);
#9248=LINE('',#63293,#10494);
#9249=LINE('',#63297,#10495);
#9250=LINE('',#63299,#10496);
#9251=LINE('',#63303,#10497);
#9252=LINE('',#63305,#10498);
#9253=LINE('',#63309,#10499);
#9254=LINE('',#63311,#10500);
#9255=LINE('',#63315,#10501);
#9256=LINE('',#63317,#10502);
#9257=LINE('',#63321,#10503);
#9258=LINE('',#63323,#10504);
#9259=LINE('',#63327,#10505);
#9260=LINE('',#63329,#10506);
#9261=LINE('',#63333,#10507);
#9262=LINE('',#63335,#10508);
#9263=LINE('',#63339,#10509);
#9264=LINE('',#63341,#10510);
#9265=LINE('',#63345,#10511);
#9266=LINE('',#63347,#10512);
#9267=LINE('',#63351,#10513);
#9268=LINE('',#63353,#10514);
#9269=LINE('',#63357,#10515);
#9270=LINE('',#63359,#10516);
#9271=LINE('',#63363,#10517);
#9272=LINE('',#63365,#10518);
#9273=LINE('',#63369,#10519);
#9274=LINE('',#63371,#10520);
#9275=LINE('',#63375,#10521);
#9276=LINE('',#63378,#10522);
#9277=LINE('',#63381,#10523);
#9278=LINE('',#63384,#10524);
#9279=LINE('',#63387,#10525);
#9280=LINE('',#63390,#10526);
#9281=LINE('',#63393,#10527);
#9282=LINE('',#63396,#10528);
#9283=LINE('',#63399,#10529);
#9284=LINE('',#63402,#10530);
#9285=LINE('',#63405,#10531);
#9286=LINE('',#63408,#10532);
#9287=LINE('',#63411,#10533);
#9288=LINE('',#63414,#10534);
#9289=LINE('',#63417,#10535);
#9290=LINE('',#63420,#10536);
#9291=LINE('',#63423,#10537);
#9292=LINE('',#63426,#10538);
#9293=LINE('',#63429,#10539);
#9294=LINE('',#63432,#10540);
#9295=LINE('',#63435,#10541);
#9296=LINE('',#63438,#10542);
#9297=LINE('',#63441,#10543);
#9298=LINE('',#63444,#10544);
#9299=LINE('',#63447,#10545);
#9300=LINE('',#63450,#10546);
#9301=LINE('',#63453,#10547);
#9302=LINE('',#63456,#10548);
#9303=LINE('',#63459,#10549);
#9304=LINE('',#63461,#10550);
#9305=LINE('',#63710,#10551);
#9306=LINE('',#63712,#10552);
#9307=LINE('',#63721,#10553);
#9308=LINE('',#63723,#10554);
#9309=LINE('',#63725,#10555);
#9310=LINE('',#63727,#10556);
#9311=LINE('',#63729,#10557);
#9312=LINE('',#63730,#10558);
#9313=LINE('',#63732,#10559);
#9314=LINE('',#63733,#10560);
#9315=LINE('',#63735,#10561);
#9316=LINE('',#63737,#10562);
#9317=LINE('',#63739,#10563);
#9318=LINE('',#63741,#10564);
#9319=LINE('',#65263,#10565);
#9320=LINE('',#65266,#10566);
#9321=LINE('',#65268,#10567);
#9322=LINE('',#65271,#10568);
#9323=LINE('',#65273,#10569);
#9324=LINE('',#65276,#10570);
#9325=LINE('',#65278,#10571);
#9326=LINE('',#65281,#10572);
#9327=LINE('',#65283,#10573);
#9328=LINE('',#65286,#10574);
#9329=LINE('',#65288,#10575);
#9330=LINE('',#65291,#10576);
#9331=LINE('',#65293,#10577);
#9332=LINE('',#65296,#10578);
#9333=LINE('',#65298,#10579);
#9334=LINE('',#65319,#10580);
#9335=LINE('',#65321,#10581);
#9336=LINE('',#65324,#10582);
#9337=LINE('',#65326,#10583);
#9338=LINE('',#65329,#10584);
#9339=LINE('',#65331,#10585);
#9340=LINE('',#65334,#10586);
#9341=LINE('',#65336,#10587);
#9342=LINE('',#65339,#10588);
#9343=LINE('',#65341,#10589);
#9344=LINE('',#65344,#10590);
#9345=LINE('',#65346,#10591);
#9346=LINE('',#65349,#10592);
#9347=LINE('',#65351,#10593);
#9348=LINE('',#65354,#10594);
#9349=LINE('',#65356,#10595);
#9350=LINE('',#65359,#10596);
#9351=LINE('',#65361,#10597);
#9352=LINE('',#65364,#10598);
#9353=LINE('',#65366,#10599);
#9354=LINE('',#65369,#10600);
#9355=LINE('',#65371,#10601);
#9356=LINE('',#65374,#10602);
#9357=LINE('',#65376,#10603);
#9358=LINE('',#65379,#10604);
#9359=LINE('',#65381,#10605);
#9360=LINE('',#65384,#10606);
#9361=LINE('',#65386,#10607);
#9362=LINE('',#65389,#10608);
#9363=LINE('',#65391,#10609);
#9364=LINE('',#65394,#10610);
#9365=LINE('',#65396,#10611);
#9366=LINE('',#65399,#10612);
#9367=LINE('',#65401,#10613);
#9368=LINE('',#65404,#10614);
#9369=LINE('',#65406,#10615);
#9370=LINE('',#65409,#10616);
#9371=LINE('',#65411,#10617);
#9372=LINE('',#65414,#10618);
#9373=LINE('',#65416,#10619);
#9374=LINE('',#65419,#10620);
#9375=LINE('',#65421,#10621);
#9376=LINE('',#65424,#10622);
#9377=LINE('',#65426,#10623);
#9378=LINE('',#65429,#10624);
#9379=LINE('',#65431,#10625);
#9380=LINE('',#65434,#10626);
#9381=LINE('',#65436,#10627);
#9382=LINE('',#65439,#10628);
#9383=LINE('',#65441,#10629);
#9384=LINE('',#65444,#10630);
#9385=LINE('',#65446,#10631);
#9386=LINE('',#65449,#10632);
#9387=LINE('',#65451,#10633);
#9388=LINE('',#65454,#10634);
#9389=LINE('',#65456,#10635);
#9390=LINE('',#65459,#10636);
#9391=LINE('',#65461,#10637);
#9392=LINE('',#65464,#10638);
#9393=LINE('',#65466,#10639);
#9394=LINE('',#65469,#10640);
#9395=LINE('',#65471,#10641);
#9396=LINE('',#65474,#10642);
#9397=LINE('',#65476,#10643);
#9398=LINE('',#65479,#10644);
#9399=LINE('',#65481,#10645);
#9400=LINE('',#65484,#10646);
#9401=LINE('',#65486,#10647);
#9402=LINE('',#65489,#10648);
#9403=LINE('',#65491,#10649);
#9404=LINE('',#65494,#10650);
#9405=LINE('',#65496,#10651);
#9406=LINE('',#65499,#10652);
#9407=LINE('',#65501,#10653);
#9408=LINE('',#65504,#10654);
#9409=LINE('',#65506,#10655);
#9410=LINE('',#65509,#10656);
#9411=LINE('',#65511,#10657);
#9412=LINE('',#65514,#10658);
#9413=LINE('',#65516,#10659);
#9414=LINE('',#65519,#10660);
#9415=LINE('',#65521,#10661);
#9416=LINE('',#65524,#10662);
#9417=LINE('',#65526,#10663);
#9418=LINE('',#65529,#10664);
#9419=LINE('',#65531,#10665);
#9420=LINE('',#65534,#10666);
#9421=LINE('',#65536,#10667);
#9422=LINE('',#65539,#10668);
#9423=LINE('',#65541,#10669);
#9424=LINE('',#65544,#10670);
#9425=LINE('',#65546,#10671);
#9426=LINE('',#65549,#10672);
#9427=LINE('',#65551,#10673);
#9428=LINE('',#65554,#10674);
#9429=LINE('',#65556,#10675);
#9430=LINE('',#65559,#10676);
#9431=LINE('',#65561,#10677);
#9432=LINE('',#65564,#10678);
#9433=LINE('',#65566,#10679);
#9434=LINE('',#65569,#10680);
#9435=LINE('',#65571,#10681);
#9436=LINE('',#65574,#10682);
#9437=LINE('',#65576,#10683);
#9438=LINE('',#65579,#10684);
#9439=LINE('',#65581,#10685);
#9440=LINE('',#65584,#10686);
#9441=LINE('',#65586,#10687);
#9442=LINE('',#65589,#10688);
#9443=LINE('',#65591,#10689);
#9444=LINE('',#65594,#10690);
#9445=LINE('',#65596,#10691);
#9446=LINE('',#65599,#10692);
#9447=LINE('',#65601,#10693);
#9448=LINE('',#65604,#10694);
#9449=LINE('',#65606,#10695);
#9450=LINE('',#65624,#10696);
#9451=LINE('',#65663,#10697);
#9452=LINE('',#65704,#10698);
#9453=LINE('',#65780,#10699);
#9454=LINE('',#65858,#10700);
#9455=LINE('',#65934,#10701);
#9456=LINE('',#66010,#10702);
#9457=LINE('',#66086,#10703);
#9458=LINE('',#66162,#10704);
#9459=LINE('',#66240,#10705);
#9460=LINE('',#66318,#10706);
#9461=LINE('',#66394,#10707);
#9462=LINE('',#66470,#10708);
#9463=LINE('',#66546,#10709);
#9464=LINE('',#66622,#10710);
#9465=LINE('',#66700,#10711);
#9466=LINE('',#66776,#10712);
#9467=LINE('',#66854,#10713);
#9468=LINE('',#66930,#10714);
#9469=LINE('',#67006,#10715);
#9470=LINE('',#67082,#10716);
#9471=LINE('',#67158,#10717);
#9472=LINE('',#67236,#10718);
#9473=LINE('',#67314,#10719);
#9474=LINE('',#67390,#10720);
#9475=LINE('',#67466,#10721);
#9476=LINE('',#67542,#10722);
#9477=LINE('',#67618,#10723);
#9478=LINE('',#67696,#10724);
#9479=LINE('',#67772,#10725);
#9480=LINE('',#67797,#10726);
#9481=LINE('',#67811,#10727);
#9482=LINE('',#67887,#10728);
#9483=LINE('',#67963,#10729);
#9484=LINE('',#68041,#10730);
#9485=LINE('',#68117,#10731);
#9486=LINE('',#68195,#10732);
#9487=LINE('',#68271,#10733);
#9488=LINE('',#68347,#10734);
#9489=LINE('',#68423,#10735);
#9490=LINE('',#68499,#10736);
#9491=LINE('',#68577,#10737);
#9492=LINE('',#68653,#10738);
#9493=LINE('',#68731,#10739);
#9494=LINE('',#68807,#10740);
#9495=LINE('',#68883,#10741);
#9496=LINE('',#68959,#10742);
#9497=LINE('',#69035,#10743);
#9498=LINE('',#69111,#10744);
#9499=LINE('',#69189,#10745);
#9500=LINE('',#69265,#10746);
#9501=LINE('',#69343,#10747);
#9502=LINE('',#69419,#10748);
#9503=LINE('',#69495,#10749);
#9504=LINE('',#69571,#10750);
#9505=LINE('',#69647,#10751);
#9506=LINE('',#69725,#10752);
#9507=LINE('',#69801,#10753);
#9508=LINE('',#69879,#10754);
#9509=LINE('',#69955,#10755);
#9510=LINE('',#70150,#10756);
#9511=LINE('',#70153,#10757);
#9512=LINE('',#70159,#10758);
#9513=LINE('',#70162,#10759);
#9514=LINE('',#70168,#10760);
#9515=LINE('',#70171,#10761);
#9516=LINE('',#70177,#10762);
#9517=LINE('',#70180,#10763);
#9518=LINE('',#70186,#10764);
#9519=LINE('',#70189,#10765);
#9520=LINE('',#70195,#10766);
#9521=LINE('',#70198,#10767);
#9522=LINE('',#70204,#10768);
#9523=LINE('',#70207,#10769);
#9524=LINE('',#70213,#10770);
#9525=LINE('',#70216,#10771);
#9526=LINE('',#70222,#10772);
#9527=LINE('',#70225,#10773);
#9528=LINE('',#70231,#10774);
#9529=LINE('',#70234,#10775);
#9530=LINE('',#70240,#10776);
#9531=LINE('',#70243,#10777);
#9532=LINE('',#70249,#10778);
#9533=LINE('',#70252,#10779);
#9534=LINE('',#70258,#10780);
#9535=LINE('',#70261,#10781);
#9536=LINE('',#70267,#10782);
#9537=LINE('',#70270,#10783);
#9538=LINE('',#70276,#10784);
#9539=LINE('',#70279,#10785);
#9540=LINE('',#70310,#10786);
#9541=LINE('',#71250,#10787);
#9542=LINE('',#72184,#10788);
#9543=LINE('',#72195,#10789);
#9544=LINE('',#72680,#10790);
#9545=LINE('',#72683,#10791);
#9546=LINE('',#72686,#10792);
#9547=LINE('',#72688,#10793);
#9548=LINE('',#72692,#10794);
#9549=LINE('',#72694,#10795);
#9550=LINE('',#72698,#10796);
#9551=LINE('',#72700,#10797);
#9552=LINE('',#72704,#10798);
#9553=LINE('',#72706,#10799);
#9554=LINE('',#72710,#10800);
#9555=LINE('',#72712,#10801);
#9556=LINE('',#72716,#10802);
#9557=LINE('',#72718,#10803);
#9558=LINE('',#72722,#10804);
#9559=LINE('',#72724,#10805);
#9560=LINE('',#72728,#10806);
#9561=LINE('',#72730,#10807);
#9562=LINE('',#72734,#10808);
#9563=LINE('',#72736,#10809);
#9564=LINE('',#72740,#10810);
#9565=LINE('',#72742,#10811);
#9566=LINE('',#72746,#10812);
#9567=LINE('',#72748,#10813);
#9568=LINE('',#72752,#10814);
#9569=LINE('',#72754,#10815);
#9570=LINE('',#72758,#10816);
#9571=LINE('',#72760,#10817);
#9572=LINE('',#72764,#10818);
#9573=LINE('',#72766,#10819);
#9574=LINE('',#72770,#10820);
#9575=LINE('',#72772,#10821);
#9576=LINE('',#72776,#10822);
#9577=LINE('',#72778,#10823);
#9578=LINE('',#72782,#10824);
#9579=LINE('',#72784,#10825);
#9580=LINE('',#72788,#10826);
#9581=LINE('',#72790,#10827);
#9582=LINE('',#72794,#10828);
#9583=LINE('',#72796,#10829);
#9584=LINE('',#72800,#10830);
#9585=LINE('',#72802,#10831);
#9586=LINE('',#72806,#10832);
#9587=LINE('',#72808,#10833);
#9588=LINE('',#72812,#10834);
#9589=LINE('',#72814,#10835);
#9590=LINE('',#72818,#10836);
#9591=LINE('',#72820,#10837);
#9592=LINE('',#72824,#10838);
#9593=LINE('',#72826,#10839);
#9594=LINE('',#72830,#10840);
#9595=LINE('',#72832,#10841);
#9596=LINE('',#72836,#10842);
#9597=LINE('',#72838,#10843);
#9598=LINE('',#72842,#10844);
#9599=LINE('',#72844,#10845);
#9600=LINE('',#72848,#10846);
#9601=LINE('',#72850,#10847);
#9602=LINE('',#72854,#10848);
#9603=LINE('',#72856,#10849);
#9604=LINE('',#72860,#10850);
#9605=LINE('',#72862,#10851);
#9606=LINE('',#72866,#10852);
#9607=LINE('',#72868,#10853);
#9608=LINE('',#72872,#10854);
#9609=LINE('',#72874,#10855);
#9610=LINE('',#72878,#10856);
#9611=LINE('',#72880,#10857);
#9612=LINE('',#72884,#10858);
#9613=LINE('',#72886,#10859);
#9614=LINE('',#72890,#10860);
#9615=LINE('',#72892,#10861);
#9616=LINE('',#72896,#10862);
#9617=LINE('',#72898,#10863);
#9618=LINE('',#72902,#10864);
#9619=LINE('',#72904,#10865);
#9620=LINE('',#72908,#10866);
#9621=LINE('',#72910,#10867);
#9622=LINE('',#72914,#10868);
#9623=LINE('',#72916,#10869);
#9624=LINE('',#72920,#10870);
#9625=LINE('',#72922,#10871);
#9626=LINE('',#72926,#10872);
#9627=LINE('',#72928,#10873);
#9628=LINE('',#72932,#10874);
#9629=LINE('',#72934,#10875);
#9630=LINE('',#72938,#10876);
#9631=LINE('',#72940,#10877);
#9632=LINE('',#72944,#10878);
#9633=LINE('',#72946,#10879);
#9634=LINE('',#72950,#10880);
#9635=LINE('',#72952,#10881);
#9636=LINE('',#72956,#10882);
#9637=LINE('',#72958,#10883);
#9638=LINE('',#72962,#10884);
#9639=LINE('',#72964,#10885);
#9640=LINE('',#72968,#10886);
#9641=LINE('',#72970,#10887);
#9642=LINE('',#72974,#10888);
#9643=LINE('',#72976,#10889);
#9644=LINE('',#72980,#10890);
#9645=LINE('',#72982,#10891);
#9646=LINE('',#72986,#10892);
#9647=LINE('',#72988,#10893);
#9648=LINE('',#72992,#10894);
#9649=LINE('',#72994,#10895);
#9650=LINE('',#72998,#10896);
#9651=LINE('',#73000,#10897);
#9652=LINE('',#73004,#10898);
#9653=LINE('',#73006,#10899);
#9654=LINE('',#73010,#10900);
#9655=LINE('',#73012,#10901);
#9656=LINE('',#73016,#10902);
#9657=LINE('',#73018,#10903);
#9658=LINE('',#73022,#10904);
#9659=LINE('',#73024,#10905);
#9660=LINE('',#73028,#10906);
#9661=LINE('',#73030,#10907);
#9662=LINE('',#73034,#10908);
#9663=LINE('',#73036,#10909);
#9664=LINE('',#73040,#10910);
#9665=LINE('',#73042,#10911);
#9666=LINE('',#73046,#10912);
#9667=LINE('',#73048,#10913);
#9668=LINE('',#73052,#10914);
#9669=LINE('',#73054,#10915);
#9670=LINE('',#73058,#10916);
#9671=LINE('',#73060,#10917);
#9672=LINE('',#73064,#10918);
#9673=LINE('',#73067,#10919);
#9674=LINE('',#73070,#10920);
#9675=LINE('',#73073,#10921);
#9676=LINE('',#73076,#10922);
#9677=LINE('',#73079,#10923);
#9678=LINE('',#73082,#10924);
#9679=LINE('',#73085,#10925);
#9680=LINE('',#73088,#10926);
#9681=LINE('',#73091,#10927);
#9682=LINE('',#73094,#10928);
#9683=LINE('',#73097,#10929);
#9684=LINE('',#73100,#10930);
#9685=LINE('',#73103,#10931);
#9686=LINE('',#73106,#10932);
#9687=LINE('',#73109,#10933);
#9688=LINE('',#73112,#10934);
#9689=LINE('',#73115,#10935);
#9690=LINE('',#73118,#10936);
#9691=LINE('',#73121,#10937);
#9692=LINE('',#73124,#10938);
#9693=LINE('',#73127,#10939);
#9694=LINE('',#73130,#10940);
#9695=LINE('',#73133,#10941);
#9696=LINE('',#73136,#10942);
#9697=LINE('',#73139,#10943);
#9698=LINE('',#73142,#10944);
#9699=LINE('',#73145,#10945);
#9700=LINE('',#73148,#10946);
#9701=LINE('',#73150,#10947);
#9702=LINE('',#73399,#10948);
#9703=LINE('',#73401,#10949);
#9704=LINE('',#73410,#10950);
#9705=LINE('',#73412,#10951);
#9706=LINE('',#73414,#10952);
#9707=LINE('',#73416,#10953);
#9708=LINE('',#73418,#10954);
#9709=LINE('',#73419,#10955);
#9710=LINE('',#73421,#10956);
#9711=LINE('',#73422,#10957);
#9712=LINE('',#73424,#10958);
#9713=LINE('',#73426,#10959);
#9714=LINE('',#73428,#10960);
#9715=LINE('',#73430,#10961);
#9716=LINE('',#74952,#10962);
#9717=LINE('',#74955,#10963);
#9718=LINE('',#74957,#10964);
#9719=LINE('',#74960,#10965);
#9720=LINE('',#74962,#10966);
#9721=LINE('',#74965,#10967);
#9722=LINE('',#74967,#10968);
#9723=LINE('',#74970,#10969);
#9724=LINE('',#74972,#10970);
#9725=LINE('',#74975,#10971);
#9726=LINE('',#74977,#10972);
#9727=LINE('',#74980,#10973);
#9728=LINE('',#74982,#10974);
#9729=LINE('',#74985,#10975);
#9730=LINE('',#74987,#10976);
#9731=LINE('',#75008,#10977);
#9732=LINE('',#75010,#10978);
#9733=LINE('',#75013,#10979);
#9734=LINE('',#75015,#10980);
#9735=LINE('',#75018,#10981);
#9736=LINE('',#75020,#10982);
#9737=LINE('',#75023,#10983);
#9738=LINE('',#75025,#10984);
#9739=LINE('',#75028,#10985);
#9740=LINE('',#75030,#10986);
#9741=LINE('',#75033,#10987);
#9742=LINE('',#75035,#10988);
#9743=LINE('',#75038,#10989);
#9744=LINE('',#75040,#10990);
#9745=LINE('',#75043,#10991);
#9746=LINE('',#75045,#10992);
#9747=LINE('',#75048,#10993);
#9748=LINE('',#75050,#10994);
#9749=LINE('',#75053,#10995);
#9750=LINE('',#75055,#10996);
#9751=LINE('',#75058,#10997);
#9752=LINE('',#75060,#10998);
#9753=LINE('',#75063,#10999);
#9754=LINE('',#75065,#11000);
#9755=LINE('',#75068,#11001);
#9756=LINE('',#75070,#11002);
#9757=LINE('',#75073,#11003);
#9758=LINE('',#75075,#11004);
#9759=LINE('',#75078,#11005);
#9760=LINE('',#75080,#11006);
#9761=LINE('',#75083,#11007);
#9762=LINE('',#75085,#11008);
#9763=LINE('',#75088,#11009);
#9764=LINE('',#75090,#11010);
#9765=LINE('',#75093,#11011);
#9766=LINE('',#75095,#11012);
#9767=LINE('',#75098,#11013);
#9768=LINE('',#75100,#11014);
#9769=LINE('',#75103,#11015);
#9770=LINE('',#75105,#11016);
#9771=LINE('',#75108,#11017);
#9772=LINE('',#75110,#11018);
#9773=LINE('',#75113,#11019);
#9774=LINE('',#75115,#11020);
#9775=LINE('',#75118,#11021);
#9776=LINE('',#75120,#11022);
#9777=LINE('',#75123,#11023);
#9778=LINE('',#75125,#11024);
#9779=LINE('',#75128,#11025);
#9780=LINE('',#75130,#11026);
#9781=LINE('',#75133,#11027);
#9782=LINE('',#75135,#11028);
#9783=LINE('',#75138,#11029);
#9784=LINE('',#75140,#11030);
#9785=LINE('',#75143,#11031);
#9786=LINE('',#75145,#11032);
#9787=LINE('',#75148,#11033);
#9788=LINE('',#75150,#11034);
#9789=LINE('',#75153,#11035);
#9790=LINE('',#75155,#11036);
#9791=LINE('',#75158,#11037);
#9792=LINE('',#75160,#11038);
#9793=LINE('',#75163,#11039);
#9794=LINE('',#75165,#11040);
#9795=LINE('',#75168,#11041);
#9796=LINE('',#75170,#11042);
#9797=LINE('',#75173,#11043);
#9798=LINE('',#75175,#11044);
#9799=LINE('',#75178,#11045);
#9800=LINE('',#75180,#11046);
#9801=LINE('',#75183,#11047);
#9802=LINE('',#75185,#11048);
#9803=LINE('',#75188,#11049);
#9804=LINE('',#75190,#11050);
#9805=LINE('',#75193,#11051);
#9806=LINE('',#75195,#11052);
#9807=LINE('',#75198,#11053);
#9808=LINE('',#75200,#11054);
#9809=LINE('',#75203,#11055);
#9810=LINE('',#75205,#11056);
#9811=LINE('',#75208,#11057);
#9812=LINE('',#75210,#11058);
#9813=LINE('',#75213,#11059);
#9814=LINE('',#75215,#11060);
#9815=LINE('',#75218,#11061);
#9816=LINE('',#75220,#11062);
#9817=LINE('',#75223,#11063);
#9818=LINE('',#75225,#11064);
#9819=LINE('',#75228,#11065);
#9820=LINE('',#75230,#11066);
#9821=LINE('',#75233,#11067);
#9822=LINE('',#75235,#11068);
#9823=LINE('',#75238,#11069);
#9824=LINE('',#75240,#11070);
#9825=LINE('',#75243,#11071);
#9826=LINE('',#75245,#11072);
#9827=LINE('',#75248,#11073);
#9828=LINE('',#75250,#11074);
#9829=LINE('',#75253,#11075);
#9830=LINE('',#75255,#11076);
#9831=LINE('',#75258,#11077);
#9832=LINE('',#75260,#11078);
#9833=LINE('',#75263,#11079);
#9834=LINE('',#75265,#11080);
#9835=LINE('',#75268,#11081);
#9836=LINE('',#75270,#11082);
#9837=LINE('',#75273,#11083);
#9838=LINE('',#75275,#11084);
#9839=LINE('',#75278,#11085);
#9840=LINE('',#75280,#11086);
#9841=LINE('',#75283,#11087);
#9842=LINE('',#75285,#11088);
#9843=LINE('',#75288,#11089);
#9844=LINE('',#75290,#11090);
#9845=LINE('',#75293,#11091);
#9846=LINE('',#75295,#11092);
#9847=VECTOR('',#36351,10.);
#9848=VECTOR('',#36352,10.);
#9849=VECTOR('',#36353,10.);
#9850=VECTOR('',#36354,10.);
#9851=VECTOR('',#36357,10.);
#9852=VECTOR('',#36358,9.99999999999999);
#9853=VECTOR('',#36359,10.);
#9854=VECTOR('',#36360,9.99999999999999);
#9855=VECTOR('',#36363,10.);
#9856=VECTOR('',#36364,10.);
#9857=VECTOR('',#36365,9.99999999999999);
#9858=VECTOR('',#36368,10.);
#9859=VECTOR('',#36371,10.);
#9860=VECTOR('',#36372,10.);
#9861=VECTOR('',#36375,10.);
#9862=VECTOR('',#36378,10.);
#9863=VECTOR('',#36379,10.);
#9864=VECTOR('',#36380,10.);
#9865=VECTOR('',#36383,10.);
#9866=VECTOR('',#36384,10.);
#9867=VECTOR('',#36387,10.);
#9868=VECTOR('',#36392,40.);
#9869=VECTOR('',#36423,1.5);
#9870=VECTOR('',#36430,1.5);
#9871=VECTOR('',#36437,1.5);
#9872=VECTOR('',#36444,10.);
#9873=VECTOR('',#36447,10.);
#9874=VECTOR('',#36450,10.);
#9875=VECTOR('',#36451,10.);
#9876=VECTOR('',#36452,10.);
#9877=VECTOR('',#36457,10.);
#9878=VECTOR('',#36460,10.);
#9879=VECTOR('',#36463,10.);
#9880=VECTOR('',#36464,10.);
#9881=VECTOR('',#36465,10.);
#9882=VECTOR('',#36470,10.);
#9883=VECTOR('',#36473,10.);
#9884=VECTOR('',#36476,9.99999999999999);
#9885=VECTOR('',#36477,10.);
#9886=VECTOR('',#36478,9.99999999999999);
#9887=VECTOR('',#36483,10.);
#9888=VECTOR('',#36486,10.);
#9889=VECTOR('',#36491,10.);
#9890=VECTOR('',#36496,9.99999999999999);
#9891=VECTOR('',#36503,10.);
#9892=VECTOR('',#36510,10.);
#9893=VECTOR('',#36517,10.);
#9894=VECTOR('',#36522,10.);
#9895=VECTOR('',#36527,10.);
#9896=VECTOR('',#36532,10.);
#9897=VECTOR('',#36539,10.);
#9898=VECTOR('',#36542,10.);
#9899=VECTOR('',#36545,10.);
#9900=VECTOR('',#36552,10.);
#9901=VECTOR('',#36555,9.99999999999999);
#9902=VECTOR('',#36562,1.5);
#9903=VECTOR('',#36563,1.5);
#9904=VECTOR('',#36570,1.5);
#9905=VECTOR('',#36573,1.5);
#9906=VECTOR('',#36576,1.5);
#9907=VECTOR('',#36579,1.5);
#9908=VECTOR('',#36582,1.5);
#9909=VECTOR('',#36585,1.5);
#9910=VECTOR('',#36588,1.5);
#9911=VECTOR('',#36591,1.5);
#9912=VECTOR('',#36594,1.5);
#9913=VECTOR('',#36597,1.5);
#9914=VECTOR('',#36600,1.5);
#9915=VECTOR('',#36603,1.5);
#9916=VECTOR('',#36606,1.5);
#9917=VECTOR('',#36609,1.5);
#9918=VECTOR('',#36612,1.5);
#9919=VECTOR('',#36615,1.5);
#9920=VECTOR('',#36618,1.5);
#9921=VECTOR('',#36621,1.5);
#9922=VECTOR('',#36624,1.5);
#9923=VECTOR('',#36627,1.5);
#9924=VECTOR('',#36630,1.5);
#9925=VECTOR('',#36633,1.5);
#9926=VECTOR('',#36636,1.5);
#9927=VECTOR('',#36639,1.5);
#9928=VECTOR('',#36642,1.5);
#9929=VECTOR('',#36645,1.5);
#9930=VECTOR('',#36648,1.5);
#9931=VECTOR('',#36651,1.17524047358084);
#9932=VECTOR('',#36656,1.17524047358084);
#9933=VECTOR('',#36661,1.17524047358084);
#9934=VECTOR('',#36664,1.17524047358084);
#9935=VECTOR('',#36667,1.17524047358084);
#9936=VECTOR('',#36670,1.17524047358084);
#9937=VECTOR('',#36673,1.17524047358084);
#9938=VECTOR('',#36676,1.17524047358084);
#9939=VECTOR('',#36679,1.17524047358084);
#9940=VECTOR('',#36682,1.17524047358084);
#9941=VECTOR('',#36685,1.17524047358084);
#9942=VECTOR('',#36688,1.17524047358084);
#9943=VECTOR('',#36691,1.17524047358084);
#9944=VECTOR('',#36694,1.17524047358084);
#9945=VECTOR('',#36697,1.17524047358084);
#9946=VECTOR('',#36700,1.17524047358084);
#9947=VECTOR('',#36703,1.17524047358084);
#9948=VECTOR('',#36706,1.17524047358084);
#9949=VECTOR('',#36709,1.17524047358084);
#9950=VECTOR('',#36712,1.17524047358084);
#9951=VECTOR('',#36715,1.17524047358084);
#9952=VECTOR('',#36718,1.17524047358084);
#9953=VECTOR('',#36721,1.17524047358084);
#9954=VECTOR('',#36724,1.17524047358084);
#9955=VECTOR('',#36727,1.17524047358084);
#9956=VECTOR('',#36730,1.17524047358084);
#9957=VECTOR('',#36733,1.17524047358084);
#9958=VECTOR('',#36736,1.17524047358084);
#9959=VECTOR('',#36739,1.17524047358084);
#9960=VECTOR('',#36742,1.17524047358084);
#9961=VECTOR('',#36745,1.17524047358084);
#9962=VECTOR('',#36762,1000.);
#9963=VECTOR('',#36765,1000.);
#9964=VECTOR('',#36770,1000.);
#9965=VECTOR('',#36773,1000.);
#9966=VECTOR('',#36778,1000.);
#9967=VECTOR('',#36781,1000.);
#9968=VECTOR('',#36786,1000.);
#9969=VECTOR('',#36789,1000.);
#9970=VECTOR('',#36794,1000.);
#9971=VECTOR('',#36797,1000.);
#9972=VECTOR('',#36802,1000.);
#9973=VECTOR('',#36805,1000.);
#9974=VECTOR('',#36810,1000.);
#9975=VECTOR('',#36813,1000.);
#9976=VECTOR('',#36818,1000.);
#9977=VECTOR('',#36821,1000.);
#9978=VECTOR('',#36826,1000.);
#9979=VECTOR('',#36829,1000.);
#9980=VECTOR('',#36834,1000.);
#9981=VECTOR('',#36837,1000.);
#9982=VECTOR('',#36842,1000.);
#9983=VECTOR('',#36845,1000.);
#9984=VECTOR('',#36850,1000.);
#9985=VECTOR('',#36853,1000.);
#9986=VECTOR('',#36858,1000.);
#9987=VECTOR('',#36861,1000.);
#9988=VECTOR('',#36866,1000.);
#9989=VECTOR('',#36869,1000.);
#9990=VECTOR('',#36874,1000.);
#9991=VECTOR('',#36877,1000.);
#9992=VECTOR('',#36880,1.55162884844711);
#9993=VECTOR('',#37181,2.73627063036812);
#9994=VECTOR('',#37472,2.68872936963188);
#9995=VECTOR('',#37487,2.675);
#9996=VECTOR('',#38134,1000.);
#9997=VECTOR('',#38137,1000.);
#9998=VECTOR('',#38140,1000.);
#9999=VECTOR('',#38141,1000.);
#10000=VECTOR('',#38146,1000.);
#10001=VECTOR('',#38147,1000.);
#10002=VECTOR('',#38152,1000.);
#10003=VECTOR('',#38153,1000.);
#10004=VECTOR('',#38158,1000.);
#10005=VECTOR('',#38159,1000.);
#10006=VECTOR('',#38164,1000.);
#10007=VECTOR('',#38165,1000.);
#10008=VECTOR('',#38170,1000.);
#10009=VECTOR('',#38171,1000.);
#10010=VECTOR('',#38176,1000.);
#10011=VECTOR('',#38177,1000.);
#10012=VECTOR('',#38182,1000.);
#10013=VECTOR('',#38183,1000.);
#10014=VECTOR('',#38188,1000.);
#10015=VECTOR('',#38189,1000.);
#10016=VECTOR('',#38194,1000.);
#10017=VECTOR('',#38195,1000.);
#10018=VECTOR('',#38200,1000.);
#10019=VECTOR('',#38201,1000.);
#10020=VECTOR('',#38206,1000.);
#10021=VECTOR('',#38207,1000.);
#10022=VECTOR('',#38212,1000.);
#10023=VECTOR('',#38213,1000.);
#10024=VECTOR('',#38218,1000.);
#10025=VECTOR('',#38219,1000.);
#10026=VECTOR('',#38224,1000.);
#10027=VECTOR('',#38225,1000.);
#10028=VECTOR('',#38230,1000.);
#10029=VECTOR('',#38231,1000.);
#10030=VECTOR('',#38236,1000.);
#10031=VECTOR('',#38237,1000.);
#10032=VECTOR('',#38242,1000.);
#10033=VECTOR('',#38243,1000.);
#10034=VECTOR('',#38248,1000.);
#10035=VECTOR('',#38249,1000.);
#10036=VECTOR('',#38254,1000.);
#10037=VECTOR('',#38255,1000.);
#10038=VECTOR('',#38260,1000.);
#10039=VECTOR('',#38261,1000.);
#10040=VECTOR('',#38266,1000.);
#10041=VECTOR('',#38267,1000.);
#10042=VECTOR('',#38272,1000.);
#10043=VECTOR('',#38273,1000.);
#10044=VECTOR('',#38278,1000.);
#10045=VECTOR('',#38279,1000.);
#10046=VECTOR('',#38284,1000.);
#10047=VECTOR('',#38285,1000.);
#10048=VECTOR('',#38290,1000.);
#10049=VECTOR('',#38291,1000.);
#10050=VECTOR('',#38296,1000.);
#10051=VECTOR('',#38297,1000.);
#10052=VECTOR('',#38302,1000.);
#10053=VECTOR('',#38303,1000.);
#10054=VECTOR('',#38308,1000.);
#10055=VECTOR('',#38309,1000.);
#10056=VECTOR('',#38314,1000.);
#10057=VECTOR('',#38315,1000.);
#10058=VECTOR('',#38320,1000.);
#10059=VECTOR('',#38321,1000.);
#10060=VECTOR('',#38326,1000.);
#10061=VECTOR('',#38327,1000.);
#10062=VECTOR('',#38332,1000.);
#10063=VECTOR('',#38333,1000.);
#10064=VECTOR('',#38338,1000.);
#10065=VECTOR('',#38339,1000.);
#10066=VECTOR('',#38344,1000.);
#10067=VECTOR('',#38345,1000.);
#10068=VECTOR('',#38350,1000.);
#10069=VECTOR('',#38351,1000.);
#10070=VECTOR('',#38356,1000.);
#10071=VECTOR('',#38357,1000.);
#10072=VECTOR('',#38362,1000.);
#10073=VECTOR('',#38363,1000.);
#10074=VECTOR('',#38368,1000.);
#10075=VECTOR('',#38369,1000.);
#10076=VECTOR('',#38374,1000.);
#10077=VECTOR('',#38375,1000.);
#10078=VECTOR('',#38380,1000.);
#10079=VECTOR('',#38381,1000.);
#10080=VECTOR('',#38386,1000.);
#10081=VECTOR('',#38387,1000.);
#10082=VECTOR('',#38392,1000.);
#10083=VECTOR('',#38393,1000.);
#10084=VECTOR('',#38398,1000.);
#10085=VECTOR('',#38399,1000.);
#10086=VECTOR('',#38404,1000.);
#10087=VECTOR('',#38405,1000.);
#10088=VECTOR('',#38410,1000.);
#10089=VECTOR('',#38411,1000.);
#10090=VECTOR('',#38416,1000.);
#10091=VECTOR('',#38417,1000.);
#10092=VECTOR('',#38422,1000.);
#10093=VECTOR('',#38423,1000.);
#10094=VECTOR('',#38428,1000.);
#10095=VECTOR('',#38429,1000.);
#10096=VECTOR('',#38434,1000.);
#10097=VECTOR('',#38435,1000.);
#10098=VECTOR('',#38440,1000.);
#10099=VECTOR('',#38441,1000.);
#10100=VECTOR('',#38446,1000.);
#10101=VECTOR('',#38447,1000.);
#10102=VECTOR('',#38452,1000.);
#10103=VECTOR('',#38453,1000.);
#10104=VECTOR('',#38458,1000.);
#10105=VECTOR('',#38459,1000.);
#10106=VECTOR('',#38464,1000.);
#10107=VECTOR('',#38465,1000.);
#10108=VECTOR('',#38470,1000.);
#10109=VECTOR('',#38471,1000.);
#10110=VECTOR('',#38476,1000.);
#10111=VECTOR('',#38477,1000.);
#10112=VECTOR('',#38482,1000.);
#10113=VECTOR('',#38483,1000.);
#10114=VECTOR('',#38488,1000.);
#10115=VECTOR('',#38489,1000.);
#10116=VECTOR('',#38494,1000.);
#10117=VECTOR('',#38495,1000.);
#10118=VECTOR('',#38500,1000.);
#10119=VECTOR('',#38501,1000.);
#10120=VECTOR('',#38506,1000.);
#10121=VECTOR('',#38507,1000.);
#10122=VECTOR('',#38512,1000.);
#10123=VECTOR('',#38513,1000.);
#10124=VECTOR('',#38518,1000.);
#10125=VECTOR('',#38521,1000.);
#10126=VECTOR('',#38524,1000.);
#10127=VECTOR('',#38527,1000.);
#10128=VECTOR('',#38530,1000.);
#10129=VECTOR('',#38533,1000.);
#10130=VECTOR('',#38536,1000.);
#10131=VECTOR('',#38539,1000.);
#10132=VECTOR('',#38542,1000.);
#10133=VECTOR('',#38545,1000.);
#10134=VECTOR('',#38548,1000.);
#10135=VECTOR('',#38551,1000.);
#10136=VECTOR('',#38554,1000.);
#10137=VECTOR('',#38557,1000.);
#10138=VECTOR('',#38560,1000.);
#10139=VECTOR('',#38563,1000.);
#10140=VECTOR('',#38566,1000.);
#10141=VECTOR('',#38569,1000.);
#10142=VECTOR('',#38572,1000.);
#10143=VECTOR('',#38575,1000.);
#10144=VECTOR('',#38578,1000.);
#10145=VECTOR('',#38581,1000.);
#10146=VECTOR('',#38584,1000.);
#10147=VECTOR('',#38587,1000.);
#10148=VECTOR('',#38590,1000.);
#10149=VECTOR('',#38593,1000.);
#10150=VECTOR('',#38596,1000.);
#10151=VECTOR('',#38599,1000.);
#10152=VECTOR('',#38602,1000.);
#10153=VECTOR('',#38603,1000.);
#10154=VECTOR('',#39094,1000.);
#10155=VECTOR('',#39095,1000.);
#10156=VECTOR('',#39108,1000.);
#10157=VECTOR('',#39109,1000.);
#10158=VECTOR('',#39110,1000.);
#10159=VECTOR('',#39111,1000.);
#10160=VECTOR('',#39112,1000.);
#10161=VECTOR('',#39113,1000.);
#10162=VECTOR('',#39116,1000.);
#10163=VECTOR('',#39117,1000.);
#10164=VECTOR('',#39120,1000.);
#10165=VECTOR('',#39123,1000.);
#10166=VECTOR('',#39126,1000.);
#10167=VECTOR('',#39129,1000.);
#10168=VECTOR('',#39132,10.);
#10169=VECTOR('',#39137,1000.);
#10170=VECTOR('',#39140,1000.);
#10171=VECTOR('',#39145,1000.);
#10172=VECTOR('',#39148,1000.);
#10173=VECTOR('',#39153,1000.);
#10174=VECTOR('',#39156,1000.);
#10175=VECTOR('',#39161,1000.);
#10176=VECTOR('',#39164,1000.);
#10177=VECTOR('',#39169,1000.);
#10178=VECTOR('',#39172,1000.);
#10179=VECTOR('',#39177,1000.);
#10180=VECTOR('',#39180,1000.);
#10181=VECTOR('',#39185,1000.);
#10182=VECTOR('',#39188,1000.);
#10183=VECTOR('',#39229,1000.);
#10184=VECTOR('',#39232,1000.);
#10185=VECTOR('',#39237,1000.);
#10186=VECTOR('',#39240,1000.);
#10187=VECTOR('',#39245,1000.);
#10188=VECTOR('',#39248,1000.);
#10189=VECTOR('',#39253,1000.);
#10190=VECTOR('',#39256,1000.);
#10191=VECTOR('',#39261,1000.);
#10192=VECTOR('',#39264,1000.);
#10193=VECTOR('',#39269,1000.);
#10194=VECTOR('',#39272,1000.);
#10195=VECTOR('',#39277,1000.);
#10196=VECTOR('',#39280,1000.);
#10197=VECTOR('',#39285,1000.);
#10198=VECTOR('',#39288,1000.);
#10199=VECTOR('',#39293,1000.);
#10200=VECTOR('',#39296,1000.);
#10201=VECTOR('',#39301,1000.);
#10202=VECTOR('',#39304,1000.);
#10203=VECTOR('',#39309,1000.);
#10204=VECTOR('',#39312,1000.);
#10205=VECTOR('',#39317,1000.);
#10206=VECTOR('',#39320,1000.);
#10207=VECTOR('',#39325,1000.);
#10208=VECTOR('',#39328,1000.);
#10209=VECTOR('',#39333,1000.);
#10210=VECTOR('',#39336,1000.);
#10211=VECTOR('',#39341,1000.);
#10212=VECTOR('',#39344,1000.);
#10213=VECTOR('',#39349,1000.);
#10214=VECTOR('',#39352,1000.);
#10215=VECTOR('',#39357,1000.);
#10216=VECTOR('',#39360,1000.);
#10217=VECTOR('',#39365,1000.);
#10218=VECTOR('',#39368,1000.);
#10219=VECTOR('',#39373,1000.);
#10220=VECTOR('',#39376,1000.);
#10221=VECTOR('',#39381,1000.);
#10222=VECTOR('',#39384,1000.);
#10223=VECTOR('',#39389,1000.);
#10224=VECTOR('',#39392,1000.);
#10225=VECTOR('',#39397,1000.);
#10226=VECTOR('',#39400,1000.);
#10227=VECTOR('',#39405,1000.);
#10228=VECTOR('',#39408,1000.);
#10229=VECTOR('',#39413,1000.);
#10230=VECTOR('',#39416,1000.);
#10231=VECTOR('',#39421,1000.);
#10232=VECTOR('',#39424,1000.);
#10233=VECTOR('',#39429,1000.);
#10234=VECTOR('',#39432,1000.);
#10235=VECTOR('',#39437,1000.);
#10236=VECTOR('',#39440,1000.);
#10237=VECTOR('',#39445,1000.);
#10238=VECTOR('',#39448,1000.);
#10239=VECTOR('',#39453,1000.);
#10240=VECTOR('',#39456,1000.);
#10241=VECTOR('',#39461,1000.);
#10242=VECTOR('',#39464,1000.);
#10243=VECTOR('',#39469,1000.);
#10244=VECTOR('',#39472,1000.);
#10245=VECTOR('',#39477,1000.);
#10246=VECTOR('',#39480,1000.);
#10247=VECTOR('',#39485,1000.);
#10248=VECTOR('',#39488,1000.);
#10249=VECTOR('',#39493,1000.);
#10250=VECTOR('',#39496,1000.);
#10251=VECTOR('',#39501,1000.);
#10252=VECTOR('',#39504,1000.);
#10253=VECTOR('',#39509,1000.);
#10254=VECTOR('',#39512,1000.);
#10255=VECTOR('',#39517,1000.);
#10256=VECTOR('',#39520,1000.);
#10257=VECTOR('',#39525,1000.);
#10258=VECTOR('',#39528,1000.);
#10259=VECTOR('',#39533,1000.);
#10260=VECTOR('',#39536,1000.);
#10261=VECTOR('',#39541,1000.);
#10262=VECTOR('',#39544,1000.);
#10263=VECTOR('',#39549,1000.);
#10264=VECTOR('',#39552,1000.);
#10265=VECTOR('',#39557,1000.);
#10266=VECTOR('',#39560,1000.);
#10267=VECTOR('',#39565,1000.);
#10268=VECTOR('',#39568,1000.);
#10269=VECTOR('',#39573,1000.);
#10270=VECTOR('',#39576,1000.);
#10271=VECTOR('',#39581,1000.);
#10272=VECTOR('',#39584,1000.);
#10273=VECTOR('',#39589,1000.);
#10274=VECTOR('',#39592,1000.);
#10275=VECTOR('',#39597,1000.);
#10276=VECTOR('',#39600,1000.);
#10277=VECTOR('',#39605,1000.);
#10278=VECTOR('',#39608,1000.);
#10279=VECTOR('',#39613,1000.);
#10280=VECTOR('',#39616,1000.);
#10281=VECTOR('',#39621,1000.);
#10282=VECTOR('',#39624,1000.);
#10283=VECTOR('',#39629,1000.);
#10284=VECTOR('',#39632,1000.);
#10285=VECTOR('',#39637,1000.);
#10286=VECTOR('',#39640,1000.);
#10287=VECTOR('',#39645,1000.);
#10288=VECTOR('',#39648,1000.);
#10289=VECTOR('',#39653,1000.);
#10290=VECTOR('',#39656,1000.);
#10291=VECTOR('',#39661,1000.);
#10292=VECTOR('',#39664,1000.);
#10293=VECTOR('',#39669,1000.);
#10294=VECTOR('',#39672,1000.);
#10295=VECTOR('',#39677,1000.);
#10296=VECTOR('',#39680,1000.);
#10297=VECTOR('',#39685,1000.);
#10298=VECTOR('',#39688,1000.);
#10299=VECTOR('',#39719,1.5);
#10300=VECTOR('',#39720,1.5);
#10301=VECTOR('',#39727,1.5);
#10302=VECTOR('',#39730,1.5);
#10303=VECTOR('',#39733,1.5);
#10304=VECTOR('',#39736,1.5);
#10305=VECTOR('',#39739,1.5);
#10306=VECTOR('',#39742,1.5);
#10307=VECTOR('',#39745,1.5);
#10308=VECTOR('',#39748,1.5);
#10309=VECTOR('',#39751,1.5);
#10310=VECTOR('',#39754,1.5);
#10311=VECTOR('',#39757,1.5);
#10312=VECTOR('',#39760,1.5);
#10313=VECTOR('',#39763,1.5);
#10314=VECTOR('',#39766,1.5);
#10315=VECTOR('',#39769,1.5);
#10316=VECTOR('',#39772,1.5);
#10317=VECTOR('',#39775,1.5);
#10318=VECTOR('',#39778,1.5);
#10319=VECTOR('',#39781,1.5);
#10320=VECTOR('',#39784,1.5);
#10321=VECTOR('',#39787,1.5);
#10322=VECTOR('',#39790,1.5);
#10323=VECTOR('',#39793,1.5);
#10324=VECTOR('',#39796,1.5);
#10325=VECTOR('',#39799,1.5);
#10326=VECTOR('',#39802,1.5);
#10327=VECTOR('',#39805,1.5);
#10328=VECTOR('',#39808,1.17524047358084);
#10329=VECTOR('',#39813,1.17524047358084);
#10330=VECTOR('',#39818,1.17524047358084);
#10331=VECTOR('',#39821,1.17524047358084);
#10332=VECTOR('',#39824,1.17524047358084);
#10333=VECTOR('',#39827,1.17524047358084);
#10334=VECTOR('',#39830,1.17524047358084);
#10335=VECTOR('',#39833,1.17524047358084);
#10336=VECTOR('',#39836,1.17524047358084);
#10337=VECTOR('',#39839,1.17524047358084);
#10338=VECTOR('',#39842,1.17524047358084);
#10339=VECTOR('',#39845,1.17524047358084);
#10340=VECTOR('',#39848,1.17524047358084);
#10341=VECTOR('',#39851,1.17524047358084);
#10342=VECTOR('',#39854,1.17524047358084);
#10343=VECTOR('',#39857,1.17524047358084);
#10344=VECTOR('',#39860,1.17524047358084);
#10345=VECTOR('',#39863,1.17524047358084);
#10346=VECTOR('',#39866,1.17524047358084);
#10347=VECTOR('',#39869,1.17524047358084);
#10348=VECTOR('',#39872,1.17524047358084);
#10349=VECTOR('',#39875,1.17524047358084);
#10350=VECTOR('',#39878,1.17524047358084);
#10351=VECTOR('',#39881,1.17524047358084);
#10352=VECTOR('',#39884,1.17524047358084);
#10353=VECTOR('',#39887,1.17524047358084);
#10354=VECTOR('',#39890,1.17524047358084);
#10355=VECTOR('',#39893,1.17524047358084);
#10356=VECTOR('',#39896,1.17524047358084);
#10357=VECTOR('',#39899,1.17524047358084);
#10358=VECTOR('',#39902,1.17524047358084);
#10359=VECTOR('',#39919,1000.);
#10360=VECTOR('',#39922,1000.);
#10361=VECTOR('',#39927,1000.);
#10362=VECTOR('',#39930,1000.);
#10363=VECTOR('',#39935,1000.);
#10364=VECTOR('',#39938,1000.);
#10365=VECTOR('',#39943,1000.);
#10366=VECTOR('',#39946,1000.);
#10367=VECTOR('',#39951,1000.);
#10368=VECTOR('',#39954,1000.);
#10369=VECTOR('',#39959,1000.);
#10370=VECTOR('',#39962,1000.);
#10371=VECTOR('',#39967,1000.);
#10372=VECTOR('',#39970,1000.);
#10373=VECTOR('',#39975,1000.);
#10374=VECTOR('',#39978,1000.);
#10375=VECTOR('',#39983,1000.);
#10376=VECTOR('',#39986,1000.);
#10377=VECTOR('',#39991,1000.);
#10378=VECTOR('',#39994,1000.);
#10379=VECTOR('',#39999,1000.);
#10380=VECTOR('',#40002,1000.);
#10381=VECTOR('',#40007,1000.);
#10382=VECTOR('',#40010,1000.);
#10383=VECTOR('',#40015,1000.);
#10384=VECTOR('',#40018,1000.);
#10385=VECTOR('',#40023,1000.);
#10386=VECTOR('',#40026,1000.);
#10387=VECTOR('',#40031,1000.);
#10388=VECTOR('',#40034,1000.);
#10389=VECTOR('',#40037,1.55162884844711);
#10390=VECTOR('',#40338,2.73627063036812);
#10391=VECTOR('',#40629,2.68872936963188);
#10392=VECTOR('',#40644,2.675);
#10393=VECTOR('',#41291,1000.);
#10394=VECTOR('',#41294,1000.);
#10395=VECTOR('',#41297,1000.);
#10396=VECTOR('',#41298,1000.);
#10397=VECTOR('',#41303,1000.);
#10398=VECTOR('',#41304,1000.);
#10399=VECTOR('',#41309,1000.);
#10400=VECTOR('',#41310,1000.);
#10401=VECTOR('',#41315,1000.);
#10402=VECTOR('',#41316,1000.);
#10403=VECTOR('',#41321,1000.);
#10404=VECTOR('',#41322,1000.);
#10405=VECTOR('',#41327,1000.);
#10406=VECTOR('',#41328,1000.);
#10407=VECTOR('',#41333,1000.);
#10408=VECTOR('',#41334,1000.);
#10409=VECTOR('',#41339,1000.);
#10410=VECTOR('',#41340,1000.);
#10411=VECTOR('',#41345,1000.);
#10412=VECTOR('',#41346,1000.);
#10413=VECTOR('',#41351,1000.);
#10414=VECTOR('',#41352,1000.);
#10415=VECTOR('',#41357,1000.);
#10416=VECTOR('',#41358,1000.);
#10417=VECTOR('',#41363,1000.);
#10418=VECTOR('',#41364,1000.);
#10419=VECTOR('',#41369,1000.);
#10420=VECTOR('',#41370,1000.);
#10421=VECTOR('',#41375,1000.);
#10422=VECTOR('',#41376,1000.);
#10423=VECTOR('',#41381,1000.);
#10424=VECTOR('',#41382,1000.);
#10425=VECTOR('',#41387,1000.);
#10426=VECTOR('',#41388,1000.);
#10427=VECTOR('',#41393,1000.);
#10428=VECTOR('',#41394,1000.);
#10429=VECTOR('',#41399,1000.);
#10430=VECTOR('',#41400,1000.);
#10431=VECTOR('',#41405,1000.);
#10432=VECTOR('',#41406,1000.);
#10433=VECTOR('',#41411,1000.);
#10434=VECTOR('',#41412,1000.);
#10435=VECTOR('',#41417,1000.);
#10436=VECTOR('',#41418,1000.);
#10437=VECTOR('',#41423,1000.);
#10438=VECTOR('',#41424,1000.);
#10439=VECTOR('',#41429,1000.);
#10440=VECTOR('',#41430,1000.);
#10441=VECTOR('',#41435,1000.);
#10442=VECTOR('',#41436,1000.);
#10443=VECTOR('',#41441,1000.);
#10444=VECTOR('',#41442,1000.);
#10445=VECTOR('',#41447,1000.);
#10446=VECTOR('',#41448,1000.);
#10447=VECTOR('',#41453,1000.);
#10448=VECTOR('',#41454,1000.);
#10449=VECTOR('',#41459,1000.);
#10450=VECTOR('',#41460,1000.);
#10451=VECTOR('',#41465,1000.);
#10452=VECTOR('',#41466,1000.);
#10453=VECTOR('',#41471,1000.);
#10454=VECTOR('',#41472,1000.);
#10455=VECTOR('',#41477,1000.);
#10456=VECTOR('',#41478,1000.);
#10457=VECTOR('',#41483,1000.);
#10458=VECTOR('',#41484,1000.);
#10459=VECTOR('',#41489,1000.);
#10460=VECTOR('',#41490,1000.);
#10461=VECTOR('',#41495,1000.);
#10462=VECTOR('',#41496,1000.);
#10463=VECTOR('',#41501,1000.);
#10464=VECTOR('',#41502,1000.);
#10465=VECTOR('',#41507,1000.);
#10466=VECTOR('',#41508,1000.);
#10467=VECTOR('',#41513,1000.);
#10468=VECTOR('',#41514,1000.);
#10469=VECTOR('',#41519,1000.);
#10470=VECTOR('',#41520,1000.);
#10471=VECTOR('',#41525,1000.);
#10472=VECTOR('',#41526,1000.);
#10473=VECTOR('',#41531,1000.);
#10474=VECTOR('',#41532,1000.);
#10475=VECTOR('',#41537,1000.);
#10476=VECTOR('',#41538,1000.);
#10477=VECTOR('',#41543,1000.);
#10478=VECTOR('',#41544,1000.);
#10479=VECTOR('',#41549,1000.);
#10480=VECTOR('',#41550,1000.);
#10481=VECTOR('',#41555,1000.);
#10482=VECTOR('',#41556,1000.);
#10483=VECTOR('',#41561,1000.);
#10484=VECTOR('',#41562,1000.);
#10485=VECTOR('',#41567,1000.);
#10486=VECTOR('',#41568,1000.);
#10487=VECTOR('',#41573,1000.);
#10488=VECTOR('',#41574,1000.);
#10489=VECTOR('',#41579,1000.);
#10490=VECTOR('',#41580,1000.);
#10491=VECTOR('',#41585,1000.);
#10492=VECTOR('',#41586,1000.);
#10493=VECTOR('',#41591,1000.);
#10494=VECTOR('',#41592,1000.);
#10495=VECTOR('',#41597,1000.);
#10496=VECTOR('',#41598,1000.);
#10497=VECTOR('',#41603,1000.);
#10498=VECTOR('',#41604,1000.);
#10499=VECTOR('',#41609,1000.);
#10500=VECTOR('',#41610,1000.);
#10501=VECTOR('',#41615,1000.);
#10502=VECTOR('',#41616,1000.);
#10503=VECTOR('',#41621,1000.);
#10504=VECTOR('',#41622,1000.);
#10505=VECTOR('',#41627,1000.);
#10506=VECTOR('',#41628,1000.);
#10507=VECTOR('',#41633,1000.);
#10508=VECTOR('',#41634,1000.);
#10509=VECTOR('',#41639,1000.);
#10510=VECTOR('',#41640,1000.);
#10511=VECTOR('',#41645,1000.);
#10512=VECTOR('',#41646,1000.);
#10513=VECTOR('',#41651,1000.);
#10514=VECTOR('',#41652,1000.);
#10515=VECTOR('',#41657,1000.);
#10516=VECTOR('',#41658,1000.);
#10517=VECTOR('',#41663,1000.);
#10518=VECTOR('',#41664,1000.);
#10519=VECTOR('',#41669,1000.);
#10520=VECTOR('',#41670,1000.);
#10521=VECTOR('',#41675,1000.);
#10522=VECTOR('',#41678,1000.);
#10523=VECTOR('',#41681,1000.);
#10524=VECTOR('',#41684,1000.);
#10525=VECTOR('',#41687,1000.);
#10526=VECTOR('',#41690,1000.);
#10527=VECTOR('',#41693,1000.);
#10528=VECTOR('',#41696,1000.);
#10529=VECTOR('',#41699,1000.);
#10530=VECTOR('',#41702,1000.);
#10531=VECTOR('',#41705,1000.);
#10532=VECTOR('',#41708,1000.);
#10533=VECTOR('',#41711,1000.);
#10534=VECTOR('',#41714,1000.);
#10535=VECTOR('',#41717,1000.);
#10536=VECTOR('',#41720,1000.);
#10537=VECTOR('',#41723,1000.);
#10538=VECTOR('',#41726,1000.);
#10539=VECTOR('',#41729,1000.);
#10540=VECTOR('',#41732,1000.);
#10541=VECTOR('',#41735,1000.);
#10542=VECTOR('',#41738,1000.);
#10543=VECTOR('',#41741,1000.);
#10544=VECTOR('',#41744,1000.);
#10545=VECTOR('',#41747,1000.);
#10546=VECTOR('',#41750,1000.);
#10547=VECTOR('',#41753,1000.);
#10548=VECTOR('',#41756,1000.);
#10549=VECTOR('',#41759,1000.);
#10550=VECTOR('',#41760,1000.);
#10551=VECTOR('',#42251,1000.);
#10552=VECTOR('',#42252,1000.);
#10553=VECTOR('',#42265,1000.);
#10554=VECTOR('',#42266,1000.);
#10555=VECTOR('',#42267,1000.);
#10556=VECTOR('',#42268,1000.);
#10557=VECTOR('',#42269,1000.);
#10558=VECTOR('',#42270,1000.);
#10559=VECTOR('',#42273,1000.);
#10560=VECTOR('',#42274,1000.);
#10561=VECTOR('',#42277,1000.);
#10562=VECTOR('',#42280,1000.);
#10563=VECTOR('',#42283,1000.);
#10564=VECTOR('',#42286,1000.);
#10565=VECTOR('',#42289,10.);
#10566=VECTOR('',#42294,1000.);
#10567=VECTOR('',#42297,1000.);
#10568=VECTOR('',#42302,1000.);
#10569=VECTOR('',#42305,1000.);
#10570=VECTOR('',#42310,1000.);
#10571=VECTOR('',#42313,1000.);
#10572=VECTOR('',#42318,1000.);
#10573=VECTOR('',#42321,1000.);
#10574=VECTOR('',#42326,1000.);
#10575=VECTOR('',#42329,1000.);
#10576=VECTOR('',#42334,1000.);
#10577=VECTOR('',#42337,1000.);
#10578=VECTOR('',#42342,1000.);
#10579=VECTOR('',#42345,1000.);
#10580=VECTOR('',#42386,1000.);
#10581=VECTOR('',#42389,1000.);
#10582=VECTOR('',#42394,1000.);
#10583=VECTOR('',#42397,1000.);
#10584=VECTOR('',#42402,1000.);
#10585=VECTOR('',#42405,1000.);
#10586=VECTOR('',#42410,1000.);
#10587=VECTOR('',#42413,1000.);
#10588=VECTOR('',#42418,1000.);
#10589=VECTOR('',#42421,1000.);
#10590=VECTOR('',#42426,1000.);
#10591=VECTOR('',#42429,1000.);
#10592=VECTOR('',#42434,1000.);
#10593=VECTOR('',#42437,1000.);
#10594=VECTOR('',#42442,1000.);
#10595=VECTOR('',#42445,1000.);
#10596=VECTOR('',#42450,1000.);
#10597=VECTOR('',#42453,1000.);
#10598=VECTOR('',#42458,1000.);
#10599=VECTOR('',#42461,1000.);
#10600=VECTOR('',#42466,1000.);
#10601=VECTOR('',#42469,1000.);
#10602=VECTOR('',#42474,1000.);
#10603=VECTOR('',#42477,1000.);
#10604=VECTOR('',#42482,1000.);
#10605=VECTOR('',#42485,1000.);
#10606=VECTOR('',#42490,1000.);
#10607=VECTOR('',#42493,1000.);
#10608=VECTOR('',#42498,1000.);
#10609=VECTOR('',#42501,1000.);
#10610=VECTOR('',#42506,1000.);
#10611=VECTOR('',#42509,1000.);
#10612=VECTOR('',#42514,1000.);
#10613=VECTOR('',#42517,1000.);
#10614=VECTOR('',#42522,1000.);
#10615=VECTOR('',#42525,1000.);
#10616=VECTOR('',#42530,1000.);
#10617=VECTOR('',#42533,1000.);
#10618=VECTOR('',#42538,1000.);
#10619=VECTOR('',#42541,1000.);
#10620=VECTOR('',#42546,1000.);
#10621=VECTOR('',#42549,1000.);
#10622=VECTOR('',#42554,1000.);
#10623=VECTOR('',#42557,1000.);
#10624=VECTOR('',#42562,1000.);
#10625=VECTOR('',#42565,1000.);
#10626=VECTOR('',#42570,1000.);
#10627=VECTOR('',#42573,1000.);
#10628=VECTOR('',#42578,1000.);
#10629=VECTOR('',#42581,1000.);
#10630=VECTOR('',#42586,1000.);
#10631=VECTOR('',#42589,1000.);
#10632=VECTOR('',#42594,1000.);
#10633=VECTOR('',#42597,1000.);
#10634=VECTOR('',#42602,1000.);
#10635=VECTOR('',#42605,1000.);
#10636=VECTOR('',#42610,1000.);
#10637=VECTOR('',#42613,1000.);
#10638=VECTOR('',#42618,1000.);
#10639=VECTOR('',#42621,1000.);
#10640=VECTOR('',#42626,1000.);
#10641=VECTOR('',#42629,1000.);
#10642=VECTOR('',#42634,1000.);
#10643=VECTOR('',#42637,1000.);
#10644=VECTOR('',#42642,1000.);
#10645=VECTOR('',#42645,1000.);
#10646=VECTOR('',#42650,1000.);
#10647=VECTOR('',#42653,1000.);
#10648=VECTOR('',#42658,1000.);
#10649=VECTOR('',#42661,1000.);
#10650=VECTOR('',#42666,1000.);
#10651=VECTOR('',#42669,1000.);
#10652=VECTOR('',#42674,1000.);
#10653=VECTOR('',#42677,1000.);
#10654=VECTOR('',#42682,1000.);
#10655=VECTOR('',#42685,1000.);
#10656=VECTOR('',#42690,1000.);
#10657=VECTOR('',#42693,1000.);
#10658=VECTOR('',#42698,1000.);
#10659=VECTOR('',#42701,1000.);
#10660=VECTOR('',#42706,1000.);
#10661=VECTOR('',#42709,1000.);
#10662=VECTOR('',#42714,1000.);
#10663=VECTOR('',#42717,1000.);
#10664=VECTOR('',#42722,1000.);
#10665=VECTOR('',#42725,1000.);
#10666=VECTOR('',#42730,1000.);
#10667=VECTOR('',#42733,1000.);
#10668=VECTOR('',#42738,1000.);
#10669=VECTOR('',#42741,1000.);
#10670=VECTOR('',#42746,1000.);
#10671=VECTOR('',#42749,1000.);
#10672=VECTOR('',#42754,1000.);
#10673=VECTOR('',#42757,1000.);
#10674=VECTOR('',#42762,1000.);
#10675=VECTOR('',#42765,1000.);
#10676=VECTOR('',#42770,1000.);
#10677=VECTOR('',#42773,1000.);
#10678=VECTOR('',#42778,1000.);
#10679=VECTOR('',#42781,1000.);
#10680=VECTOR('',#42786,1000.);
#10681=VECTOR('',#42789,1000.);
#10682=VECTOR('',#42794,1000.);
#10683=VECTOR('',#42797,1000.);
#10684=VECTOR('',#42802,1000.);
#10685=VECTOR('',#42805,1000.);
#10686=VECTOR('',#42810,1000.);
#10687=VECTOR('',#42813,1000.);
#10688=VECTOR('',#42818,1000.);
#10689=VECTOR('',#42821,1000.);
#10690=VECTOR('',#42826,1000.);
#10691=VECTOR('',#42829,1000.);
#10692=VECTOR('',#42834,1000.);
#10693=VECTOR('',#42837,1000.);
#10694=VECTOR('',#42842,1000.);
#10695=VECTOR('',#42845,1000.);
#10696=VECTOR('',#42876,1.5);
#10697=VECTOR('',#42877,1.5);
#10698=VECTOR('',#42884,1.5);
#10699=VECTOR('',#42887,1.5);
#10700=VECTOR('',#42890,1.5);
#10701=VECTOR('',#42893,1.5);
#10702=VECTOR('',#42896,1.5);
#10703=VECTOR('',#42899,1.5);
#10704=VECTOR('',#42902,1.5);
#10705=VECTOR('',#42905,1.5);
#10706=VECTOR('',#42908,1.5);
#10707=VECTOR('',#42911,1.5);
#10708=VECTOR('',#42914,1.5);
#10709=VECTOR('',#42917,1.5);
#10710=VECTOR('',#42920,1.5);
#10711=VECTOR('',#42923,1.5);
#10712=VECTOR('',#42926,1.5);
#10713=VECTOR('',#42929,1.5);
#10714=VECTOR('',#42932,1.5);
#10715=VECTOR('',#42935,1.5);
#10716=VECTOR('',#42938,1.5);
#10717=VECTOR('',#42941,1.5);
#10718=VECTOR('',#42944,1.5);
#10719=VECTOR('',#42947,1.5);
#10720=VECTOR('',#42950,1.5);
#10721=VECTOR('',#42953,1.5);
#10722=VECTOR('',#42956,1.5);
#10723=VECTOR('',#42959,1.5);
#10724=VECTOR('',#42962,1.5);
#10725=VECTOR('',#42965,1.17524047358084);
#10726=VECTOR('',#42970,1.17524047358084);
#10727=VECTOR('',#42975,1.17524047358084);
#10728=VECTOR('',#42978,1.17524047358084);
#10729=VECTOR('',#42981,1.17524047358084);
#10730=VECTOR('',#42984,1.17524047358084);
#10731=VECTOR('',#42987,1.17524047358084);
#10732=VECTOR('',#42990,1.17524047358084);
#10733=VECTOR('',#42993,1.17524047358084);
#10734=VECTOR('',#42996,1.17524047358084);
#10735=VECTOR('',#42999,1.17524047358084);
#10736=VECTOR('',#43002,1.17524047358084);
#10737=VECTOR('',#43005,1.17524047358084);
#10738=VECTOR('',#43008,1.17524047358084);
#10739=VECTOR('',#43011,1.17524047358084);
#10740=VECTOR('',#43014,1.17524047358084);
#10741=VECTOR('',#43017,1.17524047358084);
#10742=VECTOR('',#43020,1.17524047358084);
#10743=VECTOR('',#43023,1.17524047358084);
#10744=VECTOR('',#43026,1.17524047358084);
#10745=VECTOR('',#43029,1.17524047358084);
#10746=VECTOR('',#43032,1.17524047358084);
#10747=VECTOR('',#43035,1.17524047358084);
#10748=VECTOR('',#43038,1.17524047358084);
#10749=VECTOR('',#43041,1.17524047358084);
#10750=VECTOR('',#43044,1.17524047358084);
#10751=VECTOR('',#43047,1.17524047358084);
#10752=VECTOR('',#43050,1.17524047358084);
#10753=VECTOR('',#43053,1.17524047358084);
#10754=VECTOR('',#43056,1.17524047358084);
#10755=VECTOR('',#43059,1.17524047358084);
#10756=VECTOR('',#43076,1000.);
#10757=VECTOR('',#43079,1000.);
#10758=VECTOR('',#43084,1000.);
#10759=VECTOR('',#43087,1000.);
#10760=VECTOR('',#43092,1000.);
#10761=VECTOR('',#43095,1000.);
#10762=VECTOR('',#43100,1000.);
#10763=VECTOR('',#43103,1000.);
#10764=VECTOR('',#43108,1000.);
#10765=VECTOR('',#43111,1000.);
#10766=VECTOR('',#43116,1000.);
#10767=VECTOR('',#43119,1000.);
#10768=VECTOR('',#43124,1000.);
#10769=VECTOR('',#43127,1000.);
#10770=VECTOR('',#43132,1000.);
#10771=VECTOR('',#43135,1000.);
#10772=VECTOR('',#43140,1000.);
#10773=VECTOR('',#43143,1000.);
#10774=VECTOR('',#43148,1000.);
#10775=VECTOR('',#43151,1000.);
#10776=VECTOR('',#43156,1000.);
#10777=VECTOR('',#43159,1000.);
#10778=VECTOR('',#43164,1000.);
#10779=VECTOR('',#43167,1000.);
#10780=VECTOR('',#43172,1000.);
#10781=VECTOR('',#43175,1000.);
#10782=VECTOR('',#43180,1000.);
#10783=VECTOR('',#43183,1000.);
#10784=VECTOR('',#43188,1000.);
#10785=VECTOR('',#43191,1000.);
#10786=VECTOR('',#43194,1.55162884844711);
#10787=VECTOR('',#43495,2.73627063036812);
#10788=VECTOR('',#43786,2.68872936963188);
#10789=VECTOR('',#43801,2.675);
#10790=VECTOR('',#44448,1000.);
#10791=VECTOR('',#44451,1000.);
#10792=VECTOR('',#44454,1000.);
#10793=VECTOR('',#44455,1000.);
#10794=VECTOR('',#44460,1000.);
#10795=VECTOR('',#44461,1000.);
#10796=VECTOR('',#44466,1000.);
#10797=VECTOR('',#44467,1000.);
#10798=VECTOR('',#44472,1000.);
#10799=VECTOR('',#44473,1000.);
#10800=VECTOR('',#44478,1000.);
#10801=VECTOR('',#44479,1000.);
#10802=VECTOR('',#44484,1000.);
#10803=VECTOR('',#44485,1000.);
#10804=VECTOR('',#44490,1000.);
#10805=VECTOR('',#44491,1000.);
#10806=VECTOR('',#44496,1000.);
#10807=VECTOR('',#44497,1000.);
#10808=VECTOR('',#44502,1000.);
#10809=VECTOR('',#44503,1000.);
#10810=VECTOR('',#44508,1000.);
#10811=VECTOR('',#44509,1000.);
#10812=VECTOR('',#44514,1000.);
#10813=VECTOR('',#44515,1000.);
#10814=VECTOR('',#44520,1000.);
#10815=VECTOR('',#44521,1000.);
#10816=VECTOR('',#44526,1000.);
#10817=VECTOR('',#44527,1000.);
#10818=VECTOR('',#44532,1000.);
#10819=VECTOR('',#44533,1000.);
#10820=VECTOR('',#44538,1000.);
#10821=VECTOR('',#44539,1000.);
#10822=VECTOR('',#44544,1000.);
#10823=VECTOR('',#44545,1000.);
#10824=VECTOR('',#44550,1000.);
#10825=VECTOR('',#44551,1000.);
#10826=VECTOR('',#44556,1000.);
#10827=VECTOR('',#44557,1000.);
#10828=VECTOR('',#44562,1000.);
#10829=VECTOR('',#44563,1000.);
#10830=VECTOR('',#44568,1000.);
#10831=VECTOR('',#44569,1000.);
#10832=VECTOR('',#44574,1000.);
#10833=VECTOR('',#44575,1000.);
#10834=VECTOR('',#44580,1000.);
#10835=VECTOR('',#44581,1000.);
#10836=VECTOR('',#44586,1000.);
#10837=VECTOR('',#44587,1000.);
#10838=VECTOR('',#44592,1000.);
#10839=VECTOR('',#44593,1000.);
#10840=VECTOR('',#44598,1000.);
#10841=VECTOR('',#44599,1000.);
#10842=VECTOR('',#44604,1000.);
#10843=VECTOR('',#44605,1000.);
#10844=VECTOR('',#44610,1000.);
#10845=VECTOR('',#44611,1000.);
#10846=VECTOR('',#44616,1000.);
#10847=VECTOR('',#44617,1000.);
#10848=VECTOR('',#44622,1000.);
#10849=VECTOR('',#44623,1000.);
#10850=VECTOR('',#44628,1000.);
#10851=VECTOR('',#44629,1000.);
#10852=VECTOR('',#44634,1000.);
#10853=VECTOR('',#44635,1000.);
#10854=VECTOR('',#44640,1000.);
#10855=VECTOR('',#44641,1000.);
#10856=VECTOR('',#44646,1000.);
#10857=VECTOR('',#44647,1000.);
#10858=VECTOR('',#44652,1000.);
#10859=VECTOR('',#44653,1000.);
#10860=VECTOR('',#44658,1000.);
#10861=VECTOR('',#44659,1000.);
#10862=VECTOR('',#44664,1000.);
#10863=VECTOR('',#44665,1000.);
#10864=VECTOR('',#44670,1000.);
#10865=VECTOR('',#44671,1000.);
#10866=VECTOR('',#44676,1000.);
#10867=VECTOR('',#44677,1000.);
#10868=VECTOR('',#44682,1000.);
#10869=VECTOR('',#44683,1000.);
#10870=VECTOR('',#44688,1000.);
#10871=VECTOR('',#44689,1000.);
#10872=VECTOR('',#44694,1000.);
#10873=VECTOR('',#44695,1000.);
#10874=VECTOR('',#44700,1000.);
#10875=VECTOR('',#44701,1000.);
#10876=VECTOR('',#44706,1000.);
#10877=VECTOR('',#44707,1000.);
#10878=VECTOR('',#44712,1000.);
#10879=VECTOR('',#44713,1000.);
#10880=VECTOR('',#44718,1000.);
#10881=VECTOR('',#44719,1000.);
#10882=VECTOR('',#44724,1000.);
#10883=VECTOR('',#44725,1000.);
#10884=VECTOR('',#44730,1000.);
#10885=VECTOR('',#44731,1000.);
#10886=VECTOR('',#44736,1000.);
#10887=VECTOR('',#44737,1000.);
#10888=VECTOR('',#44742,1000.);
#10889=VECTOR('',#44743,1000.);
#10890=VECTOR('',#44748,1000.);
#10891=VECTOR('',#44749,1000.);
#10892=VECTOR('',#44754,1000.);
#10893=VECTOR('',#44755,1000.);
#10894=VECTOR('',#44760,1000.);
#10895=VECTOR('',#44761,1000.);
#10896=VECTOR('',#44766,1000.);
#10897=VECTOR('',#44767,1000.);
#10898=VECTOR('',#44772,1000.);
#10899=VECTOR('',#44773,1000.);
#10900=VECTOR('',#44778,1000.);
#10901=VECTOR('',#44779,1000.);
#10902=VECTOR('',#44784,1000.);
#10903=VECTOR('',#44785,1000.);
#10904=VECTOR('',#44790,1000.);
#10905=VECTOR('',#44791,1000.);
#10906=VECTOR('',#44796,1000.);
#10907=VECTOR('',#44797,1000.);
#10908=VECTOR('',#44802,1000.);
#10909=VECTOR('',#44803,1000.);
#10910=VECTOR('',#44808,1000.);
#10911=VECTOR('',#44809,1000.);
#10912=VECTOR('',#44814,1000.);
#10913=VECTOR('',#44815,1000.);
#10914=VECTOR('',#44820,1000.);
#10915=VECTOR('',#44821,1000.);
#10916=VECTOR('',#44826,1000.);
#10917=VECTOR('',#44827,1000.);
#10918=VECTOR('',#44832,1000.);
#10919=VECTOR('',#44835,1000.);
#10920=VECTOR('',#44838,1000.);
#10921=VECTOR('',#44841,1000.);
#10922=VECTOR('',#44844,1000.);
#10923=VECTOR('',#44847,1000.);
#10924=VECTOR('',#44850,1000.);
#10925=VECTOR('',#44853,1000.);
#10926=VECTOR('',#44856,1000.);
#10927=VECTOR('',#44859,1000.);
#10928=VECTOR('',#44862,1000.);
#10929=VECTOR('',#44865,1000.);
#10930=VECTOR('',#44868,1000.);
#10931=VECTOR('',#44871,1000.);
#10932=VECTOR('',#44874,1000.);
#10933=VECTOR('',#44877,1000.);
#10934=VECTOR('',#44880,1000.);
#10935=VECTOR('',#44883,1000.);
#10936=VECTOR('',#44886,1000.);
#10937=VECTOR('',#44889,1000.);
#10938=VECTOR('',#44892,1000.);
#10939=VECTOR('',#44895,1000.);
#10940=VECTOR('',#44898,1000.);
#10941=VECTOR('',#44901,1000.);
#10942=VECTOR('',#44904,1000.);
#10943=VECTOR('',#44907,1000.);
#10944=VECTOR('',#44910,1000.);
#10945=VECTOR('',#44913,1000.);
#10946=VECTOR('',#44916,1000.);
#10947=VECTOR('',#44917,1000.);
#10948=VECTOR('',#45408,1000.);
#10949=VECTOR('',#45409,1000.);
#10950=VECTOR('',#45422,1000.);
#10951=VECTOR('',#45423,1000.);
#10952=VECTOR('',#45424,1000.);
#10953=VECTOR('',#45425,1000.);
#10954=VECTOR('',#45426,1000.);
#10955=VECTOR('',#45427,1000.);
#10956=VECTOR('',#45430,1000.);
#10957=VECTOR('',#45431,1000.);
#10958=VECTOR('',#45434,1000.);
#10959=VECTOR('',#45437,1000.);
#10960=VECTOR('',#45440,1000.);
#10961=VECTOR('',#45443,1000.);
#10962=VECTOR('',#45446,10.);
#10963=VECTOR('',#45451,1000.);
#10964=VECTOR('',#45454,1000.);
#10965=VECTOR('',#45459,1000.);
#10966=VECTOR('',#45462,1000.);
#10967=VECTOR('',#45467,1000.);
#10968=VECTOR('',#45470,1000.);
#10969=VECTOR('',#45475,1000.);
#10970=VECTOR('',#45478,1000.);
#10971=VECTOR('',#45483,1000.);
#10972=VECTOR('',#45486,1000.);
#10973=VECTOR('',#45491,1000.);
#10974=VECTOR('',#45494,1000.);
#10975=VECTOR('',#45499,1000.);
#10976=VECTOR('',#45502,1000.);
#10977=VECTOR('',#45543,1000.);
#10978=VECTOR('',#45546,1000.);
#10979=VECTOR('',#45551,1000.);
#10980=VECTOR('',#45554,1000.);
#10981=VECTOR('',#45559,1000.);
#10982=VECTOR('',#45562,1000.);
#10983=VECTOR('',#45567,1000.);
#10984=VECTOR('',#45570,1000.);
#10985=VECTOR('',#45575,1000.);
#10986=VECTOR('',#45578,1000.);
#10987=VECTOR('',#45583,1000.);
#10988=VECTOR('',#45586,1000.);
#10989=VECTOR('',#45591,1000.);
#10990=VECTOR('',#45594,1000.);
#10991=VECTOR('',#45599,1000.);
#10992=VECTOR('',#45602,1000.);
#10993=VECTOR('',#45607,1000.);
#10994=VECTOR('',#45610,1000.);
#10995=VECTOR('',#45615,1000.);
#10996=VECTOR('',#45618,1000.);
#10997=VECTOR('',#45623,1000.);
#10998=VECTOR('',#45626,1000.);
#10999=VECTOR('',#45631,1000.);
#11000=VECTOR('',#45634,1000.);
#11001=VECTOR('',#45639,1000.);
#11002=VECTOR('',#45642,1000.);
#11003=VECTOR('',#45647,1000.);
#11004=VECTOR('',#45650,1000.);
#11005=VECTOR('',#45655,1000.);
#11006=VECTOR('',#45658,1000.);
#11007=VECTOR('',#45663,1000.);
#11008=VECTOR('',#45666,1000.);
#11009=VECTOR('',#45671,1000.);
#11010=VECTOR('',#45674,1000.);
#11011=VECTOR('',#45679,1000.);
#11012=VECTOR('',#45682,1000.);
#11013=VECTOR('',#45687,1000.);
#11014=VECTOR('',#45690,1000.);
#11015=VECTOR('',#45695,1000.);
#11016=VECTOR('',#45698,1000.);
#11017=VECTOR('',#45703,1000.);
#11018=VECTOR('',#45706,1000.);
#11019=VECTOR('',#45711,1000.);
#11020=VECTOR('',#45714,1000.);
#11021=VECTOR('',#45719,1000.);
#11022=VECTOR('',#45722,1000.);
#11023=VECTOR('',#45727,1000.);
#11024=VECTOR('',#45730,1000.);
#11025=VECTOR('',#45735,1000.);
#11026=VECTOR('',#45738,1000.);
#11027=VECTOR('',#45743,1000.);
#11028=VECTOR('',#45746,1000.);
#11029=VECTOR('',#45751,1000.);
#11030=VECTOR('',#45754,1000.);
#11031=VECTOR('',#45759,1000.);
#11032=VECTOR('',#45762,1000.);
#11033=VECTOR('',#45767,1000.);
#11034=VECTOR('',#45770,1000.);
#11035=VECTOR('',#45775,1000.);
#11036=VECTOR('',#45778,1000.);
#11037=VECTOR('',#45783,1000.);
#11038=VECTOR('',#45786,1000.);
#11039=VECTOR('',#45791,1000.);
#11040=VECTOR('',#45794,1000.);
#11041=VECTOR('',#45799,1000.);
#11042=VECTOR('',#45802,1000.);
#11043=VECTOR('',#45807,1000.);
#11044=VECTOR('',#45810,1000.);
#11045=VECTOR('',#45815,1000.);
#11046=VECTOR('',#45818,1000.);
#11047=VECTOR('',#45823,1000.);
#11048=VECTOR('',#45826,1000.);
#11049=VECTOR('',#45831,1000.);
#11050=VECTOR('',#45834,1000.);
#11051=VECTOR('',#45839,1000.);
#11052=VECTOR('',#45842,1000.);
#11053=VECTOR('',#45847,1000.);
#11054=VECTOR('',#45850,1000.);
#11055=VECTOR('',#45855,1000.);
#11056=VECTOR('',#45858,1000.);
#11057=VECTOR('',#45863,1000.);
#11058=VECTOR('',#45866,1000.);
#11059=VECTOR('',#45871,1000.);
#11060=VECTOR('',#45874,1000.);
#11061=VECTOR('',#45879,1000.);
#11062=VECTOR('',#45882,1000.);
#11063=VECTOR('',#45887,1000.);
#11064=VECTOR('',#45890,1000.);
#11065=VECTOR('',#45895,1000.);
#11066=VECTOR('',#45898,1000.);
#11067=VECTOR('',#45903,1000.);
#11068=VECTOR('',#45906,1000.);
#11069=VECTOR('',#45911,1000.);
#11070=VECTOR('',#45914,1000.);
#11071=VECTOR('',#45919,1000.);
#11072=VECTOR('',#45922,1000.);
#11073=VECTOR('',#45927,1000.);
#11074=VECTOR('',#45930,1000.);
#11075=VECTOR('',#45935,1000.);
#11076=VECTOR('',#45938,1000.);
#11077=VECTOR('',#45943,1000.);
#11078=VECTOR('',#45946,1000.);
#11079=VECTOR('',#45951,1000.);
#11080=VECTOR('',#45954,1000.);
#11081=VECTOR('',#45959,1000.);
#11082=VECTOR('',#45962,1000.);
#11083=VECTOR('',#45967,1000.);
#11084=VECTOR('',#45970,1000.);
#11085=VECTOR('',#45975,1000.);
#11086=VECTOR('',#45978,1000.);
#11087=VECTOR('',#45983,1000.);
#11088=VECTOR('',#45986,1000.);
#11089=VECTOR('',#45991,1000.);
#11090=VECTOR('',#45994,1000.);
#11091=VECTOR('',#45999,1000.);
#11092=VECTOR('',#46002,1000.);
#11093=VERTEX_POINT('',#46048);
#11094=VERTEX_POINT('',#46049);
#11095=VERTEX_POINT('',#46051);
#11096=VERTEX_POINT('',#46053);
#11097=VERTEX_POINT('',#46057);
#11098=VERTEX_POINT('',#46059);
#11099=VERTEX_POINT('',#46061);
#11100=VERTEX_POINT('',#46065);
#11101=VERTEX_POINT('',#46067);
#11102=VERTEX_POINT('',#46073);
#11103=VERTEX_POINT('',#46079);
#11104=VERTEX_POINT('',#46081);
#11105=VERTEX_POINT('',#46085);
#11106=VERTEX_POINT('',#46091);
#11107=VERTEX_POINT('',#46093);
#11108=VERTEX_POINT('',#46100);
#11109=VERTEX_POINT('',#46101);
#11110=VERTEX_POINT('',#46105);
#11111=VERTEX_POINT('',#46106);
#11112=VERTEX_POINT('',#46110);
#11113=VERTEX_POINT('',#46111);
#11114=VERTEX_POINT('',#46115);
#11115=VERTEX_POINT('',#46117);
#11116=VERTEX_POINT('',#46121);
#11117=VERTEX_POINT('',#46123);
#11118=VERTEX_POINT('',#46127);
#11119=VERTEX_POINT('',#46129);
#11120=VERTEX_POINT('',#46133);
#11121=VERTEX_POINT('',#46134);
#11122=VERTEX_POINT('',#46136);
#11123=VERTEX_POINT('',#46138);
#11124=VERTEX_POINT('',#46142);
#11125=VERTEX_POINT('',#46144);
#11126=VERTEX_POINT('',#46148);
#11127=VERTEX_POINT('',#46149);
#11128=VERTEX_POINT('',#46151);
#11129=VERTEX_POINT('',#46153);
#11130=VERTEX_POINT('',#46157);
#11131=VERTEX_POINT('',#46159);
#11132=VERTEX_POINT('',#46163);
#11133=VERTEX_POINT('',#46164);
#11134=VERTEX_POINT('',#46166);
#11135=VERTEX_POINT('',#46168);
#11136=VERTEX_POINT('',#46172);
#11137=VERTEX_POINT('',#46174);
#11138=VERTEX_POINT('',#46178);
#11139=VERTEX_POINT('',#46179);
#11140=VERTEX_POINT('',#46181);
#11141=VERTEX_POINT('',#46183);
#11142=VERTEX_POINT('',#46187);
#11143=VERTEX_POINT('',#46189);
#11144=VERTEX_POINT('',#46194);
#11145=VERTEX_POINT('',#46196);
#11146=VERTEX_POINT('',#46198);
#11147=VERTEX_POINT('',#46201);
#11148=VERTEX_POINT('',#46203);
#11149=VERTEX_POINT('',#46205);
#11150=VERTEX_POINT('',#46210);
#11151=VERTEX_POINT('',#46214);
#11152=VERTEX_POINT('',#46218);
#11153=VERTEX_POINT('',#46222);
#11154=VERTEX_POINT('',#46228);
#11155=VERTEX_POINT('',#46230);
#11156=VERTEX_POINT('',#46244);
#11157=VERTEX_POINT('',#46245);
#11158=VERTEX_POINT('',#46247);
#11159=VERTEX_POINT('',#46284);
#11160=VERTEX_POINT('',#46287);
#11161=VERTEX_POINT('',#46324);
#11162=VERTEX_POINT('',#46325);
#11163=VERTEX_POINT('',#46400);
#11164=VERTEX_POINT('',#46401);
#11165=VERTEX_POINT('',#46478);
#11166=VERTEX_POINT('',#46479);
#11167=VERTEX_POINT('',#46554);
#11168=VERTEX_POINT('',#46555);
#11169=VERTEX_POINT('',#46630);
#11170=VERTEX_POINT('',#46631);
#11171=VERTEX_POINT('',#46706);
#11172=VERTEX_POINT('',#46707);
#11173=VERTEX_POINT('',#46782);
#11174=VERTEX_POINT('',#46783);
#11175=VERTEX_POINT('',#46860);
#11176=VERTEX_POINT('',#46861);
#11177=VERTEX_POINT('',#46938);
#11178=VERTEX_POINT('',#46939);
#11179=VERTEX_POINT('',#47014);
#11180=VERTEX_POINT('',#47015);
#11181=VERTEX_POINT('',#47090);
#11182=VERTEX_POINT('',#47091);
#11183=VERTEX_POINT('',#47166);
#11184=VERTEX_POINT('',#47167);
#11185=VERTEX_POINT('',#47242);
#11186=VERTEX_POINT('',#47243);
#11187=VERTEX_POINT('',#47320);
#11188=VERTEX_POINT('',#47321);
#11189=VERTEX_POINT('',#47396);
#11190=VERTEX_POINT('',#47397);
#11191=VERTEX_POINT('',#47474);
#11192=VERTEX_POINT('',#47475);
#11193=VERTEX_POINT('',#47550);
#11194=VERTEX_POINT('',#47551);
#11195=VERTEX_POINT('',#47626);
#11196=VERTEX_POINT('',#47627);
#11197=VERTEX_POINT('',#47702);
#11198=VERTEX_POINT('',#47703);
#11199=VERTEX_POINT('',#47778);
#11200=VERTEX_POINT('',#47779);
#11201=VERTEX_POINT('',#47856);
#11202=VERTEX_POINT('',#47857);
#11203=VERTEX_POINT('',#47934);
#11204=VERTEX_POINT('',#47935);
#11205=VERTEX_POINT('',#48010);
#11206=VERTEX_POINT('',#48011);
#11207=VERTEX_POINT('',#48086);
#11208=VERTEX_POINT('',#48087);
#11209=VERTEX_POINT('',#48162);
#11210=VERTEX_POINT('',#48163);
#11211=VERTEX_POINT('',#48238);
#11212=VERTEX_POINT('',#48239);
#11213=VERTEX_POINT('',#48316);
#11214=VERTEX_POINT('',#48317);
#11215=VERTEX_POINT('',#48392);
#11216=VERTEX_POINT('',#48393);
#11217=VERTEX_POINT('',#48395);
#11218=VERTEX_POINT('',#48418);
#11219=VERTEX_POINT('',#48420);
#11220=VERTEX_POINT('',#48431);
#11221=VERTEX_POINT('',#48432);
#11222=VERTEX_POINT('',#48507);
#11223=VERTEX_POINT('',#48508);
#11224=VERTEX_POINT('',#48583);
#11225=VERTEX_POINT('',#48584);
#11226=VERTEX_POINT('',#48661);
#11227=VERTEX_POINT('',#48662);
#11228=VERTEX_POINT('',#48737);
#11229=VERTEX_POINT('',#48738);
#11230=VERTEX_POINT('',#48815);
#11231=VERTEX_POINT('',#48816);
#11232=VERTEX_POINT('',#48891);
#11233=VERTEX_POINT('',#48892);
#11234=VERTEX_POINT('',#48967);
#11235=VERTEX_POINT('',#48968);
#11236=VERTEX_POINT('',#49043);
#11237=VERTEX_POINT('',#49044);
#11238=VERTEX_POINT('',#49119);
#11239=VERTEX_POINT('',#49120);
#11240=VERTEX_POINT('',#49197);
#11241=VERTEX_POINT('',#49198);
#11242=VERTEX_POINT('',#49273);
#11243=VERTEX_POINT('',#49274);
#11244=VERTEX_POINT('',#49351);
#11245=VERTEX_POINT('',#49352);
#11246=VERTEX_POINT('',#49427);
#11247=VERTEX_POINT('',#49428);
#11248=VERTEX_POINT('',#49503);
#11249=VERTEX_POINT('',#49504);
#11250=VERTEX_POINT('',#49579);
#11251=VERTEX_POINT('',#49580);
#11252=VERTEX_POINT('',#49655);
#11253=VERTEX_POINT('',#49656);
#11254=VERTEX_POINT('',#49731);
#11255=VERTEX_POINT('',#49732);
#11256=VERTEX_POINT('',#49809);
#11257=VERTEX_POINT('',#49810);
#11258=VERTEX_POINT('',#49885);
#11259=VERTEX_POINT('',#49886);
#11260=VERTEX_POINT('',#49963);
#11261=VERTEX_POINT('',#49964);
#11262=VERTEX_POINT('',#50039);
#11263=VERTEX_POINT('',#50040);
#11264=VERTEX_POINT('',#50115);
#11265=VERTEX_POINT('',#50116);
#11266=VERTEX_POINT('',#50191);
#11267=VERTEX_POINT('',#50192);
#11268=VERTEX_POINT('',#50267);
#11269=VERTEX_POINT('',#50268);
#11270=VERTEX_POINT('',#50345);
#11271=VERTEX_POINT('',#50346);
#11272=VERTEX_POINT('',#50421);
#11273=VERTEX_POINT('',#50422);
#11274=VERTEX_POINT('',#50499);
#11275=VERTEX_POINT('',#50500);
#11276=VERTEX_POINT('',#50575);
#11277=VERTEX_POINT('',#50576);
#11278=VERTEX_POINT('',#50651);
#11279=VERTEX_POINT('',#50663);
#11280=VERTEX_POINT('',#50676);
#11281=VERTEX_POINT('',#50768);
#11282=VERTEX_POINT('',#50769);
#11283=VERTEX_POINT('',#50771);
#11284=VERTEX_POINT('',#50773);
#11285=VERTEX_POINT('',#50777);
#11286=VERTEX_POINT('',#50778);
#11287=VERTEX_POINT('',#50780);
#11288=VERTEX_POINT('',#50782);
#11289=VERTEX_POINT('',#50786);
#11290=VERTEX_POINT('',#50787);
#11291=VERTEX_POINT('',#50789);
#11292=VERTEX_POINT('',#50791);
#11293=VERTEX_POINT('',#50795);
#11294=VERTEX_POINT('',#50796);
#11295=VERTEX_POINT('',#50798);
#11296=VERTEX_POINT('',#50800);
#11297=VERTEX_POINT('',#50804);
#11298=VERTEX_POINT('',#50805);
#11299=VERTEX_POINT('',#50807);
#11300=VERTEX_POINT('',#50809);
#11301=VERTEX_POINT('',#50813);
#11302=VERTEX_POINT('',#50814);
#11303=VERTEX_POINT('',#50816);
#11304=VERTEX_POINT('',#50818);
#11305=VERTEX_POINT('',#50822);
#11306=VERTEX_POINT('',#50823);
#11307=VERTEX_POINT('',#50825);
#11308=VERTEX_POINT('',#50827);
#11309=VERTEX_POINT('',#50831);
#11310=VERTEX_POINT('',#50832);
#11311=VERTEX_POINT('',#50834);
#11312=VERTEX_POINT('',#50836);
#11313=VERTEX_POINT('',#50840);
#11314=VERTEX_POINT('',#50841);
#11315=VERTEX_POINT('',#50843);
#11316=VERTEX_POINT('',#50845);
#11317=VERTEX_POINT('',#50849);
#11318=VERTEX_POINT('',#50850);
#11319=VERTEX_POINT('',#50852);
#11320=VERTEX_POINT('',#50854);
#11321=VERTEX_POINT('',#50858);
#11322=VERTEX_POINT('',#50859);
#11323=VERTEX_POINT('',#50861);
#11324=VERTEX_POINT('',#50863);
#11325=VERTEX_POINT('',#50867);
#11326=VERTEX_POINT('',#50868);
#11327=VERTEX_POINT('',#50870);
#11328=VERTEX_POINT('',#50872);
#11329=VERTEX_POINT('',#50876);
#11330=VERTEX_POINT('',#50877);
#11331=VERTEX_POINT('',#50879);
#11332=VERTEX_POINT('',#50881);
#11333=VERTEX_POINT('',#50885);
#11334=VERTEX_POINT('',#50886);
#11335=VERTEX_POINT('',#50888);
#11336=VERTEX_POINT('',#50890);
#11337=VERTEX_POINT('',#50894);
#11338=VERTEX_POINT('',#50895);
#11339=VERTEX_POINT('',#50897);
#11340=VERTEX_POINT('',#50899);
#11341=VERTEX_POINT('',#50903);
#11342=VERTEX_POINT('',#50904);
#11343=VERTEX_POINT('',#50908);
#11344=VERTEX_POINT('',#50912);
#11345=VERTEX_POINT('',#50916);
#11346=VERTEX_POINT('',#50920);
#11347=VERTEX_POINT('',#50924);
#11348=VERTEX_POINT('',#50931);
#11349=VERTEX_POINT('',#50935);
#11350=VERTEX_POINT('',#50937);
#11351=VERTEX_POINT('',#50941);
#11352=VERTEX_POINT('',#50942);
#11353=VERTEX_POINT('',#50951);
#11354=VERTEX_POINT('',#50955);
#11355=VERTEX_POINT('',#50957);
#11356=VERTEX_POINT('',#50961);
#11357=VERTEX_POINT('',#50963);
#11358=VERTEX_POINT('',#50967);
#11359=VERTEX_POINT('',#50969);
#11360=VERTEX_POINT('',#50973);
#11361=VERTEX_POINT('',#50975);
#11362=VERTEX_POINT('',#50979);
#11363=VERTEX_POINT('',#50981);
#11364=VERTEX_POINT('',#50985);
#11365=VERTEX_POINT('',#50987);
#11366=VERTEX_POINT('',#50991);
#11367=VERTEX_POINT('',#50993);
#11368=VERTEX_POINT('',#50997);
#11369=VERTEX_POINT('',#50999);
#11370=VERTEX_POINT('',#51003);
#11371=VERTEX_POINT('',#51005);
#11372=VERTEX_POINT('',#51009);
#11373=VERTEX_POINT('',#51011);
#11374=VERTEX_POINT('',#51015);
#11375=VERTEX_POINT('',#51017);
#11376=VERTEX_POINT('',#51021);
#11377=VERTEX_POINT('',#51023);
#11378=VERTEX_POINT('',#51027);
#11379=VERTEX_POINT('',#51029);
#11380=VERTEX_POINT('',#51033);
#11381=VERTEX_POINT('',#51035);
#11382=VERTEX_POINT('',#51039);
#11383=VERTEX_POINT('',#51041);
#11384=VERTEX_POINT('',#51045);
#11385=VERTEX_POINT('',#51047);
#11386=VERTEX_POINT('',#51051);
#11387=VERTEX_POINT('',#51053);
#11388=VERTEX_POINT('',#51057);
#11389=VERTEX_POINT('',#51059);
#11390=VERTEX_POINT('',#51063);
#11391=VERTEX_POINT('',#51065);
#11392=VERTEX_POINT('',#51069);
#11393=VERTEX_POINT('',#51071);
#11394=VERTEX_POINT('',#51075);
#11395=VERTEX_POINT('',#51077);
#11396=VERTEX_POINT('',#51081);
#11397=VERTEX_POINT('',#51083);
#11398=VERTEX_POINT('',#51087);
#11399=VERTEX_POINT('',#51089);
#11400=VERTEX_POINT('',#51093);
#11401=VERTEX_POINT('',#51095);
#11402=VERTEX_POINT('',#51099);
#11403=VERTEX_POINT('',#51101);
#11404=VERTEX_POINT('',#51105);
#11405=VERTEX_POINT('',#51107);
#11406=VERTEX_POINT('',#51111);
#11407=VERTEX_POINT('',#51113);
#11408=VERTEX_POINT('',#51117);
#11409=VERTEX_POINT('',#51119);
#11410=VERTEX_POINT('',#51123);
#11411=VERTEX_POINT('',#51125);
#11412=VERTEX_POINT('',#51129);
#11413=VERTEX_POINT('',#51131);
#11414=VERTEX_POINT('',#51135);
#11415=VERTEX_POINT('',#51137);
#11416=VERTEX_POINT('',#51141);
#11417=VERTEX_POINT('',#51143);
#11418=VERTEX_POINT('',#51147);
#11419=VERTEX_POINT('',#51149);
#11420=VERTEX_POINT('',#51153);
#11421=VERTEX_POINT('',#51155);
#11422=VERTEX_POINT('',#51159);
#11423=VERTEX_POINT('',#51161);
#11424=VERTEX_POINT('',#51165);
#11425=VERTEX_POINT('',#51167);
#11426=VERTEX_POINT('',#51171);
#11427=VERTEX_POINT('',#51173);
#11428=VERTEX_POINT('',#51177);
#11429=VERTEX_POINT('',#51179);
#11430=VERTEX_POINT('',#51183);
#11431=VERTEX_POINT('',#51185);
#11432=VERTEX_POINT('',#51189);
#11433=VERTEX_POINT('',#51191);
#11434=VERTEX_POINT('',#51195);
#11435=VERTEX_POINT('',#51197);
#11436=VERTEX_POINT('',#51201);
#11437=VERTEX_POINT('',#51203);
#11438=VERTEX_POINT('',#51207);
#11439=VERTEX_POINT('',#51209);
#11440=VERTEX_POINT('',#51213);
#11441=VERTEX_POINT('',#51215);
#11442=VERTEX_POINT('',#51219);
#11443=VERTEX_POINT('',#51221);
#11444=VERTEX_POINT('',#51225);
#11445=VERTEX_POINT('',#51227);
#11446=VERTEX_POINT('',#51231);
#11447=VERTEX_POINT('',#51233);
#11448=VERTEX_POINT('',#51237);
#11449=VERTEX_POINT('',#51239);
#11450=VERTEX_POINT('',#51243);
#11451=VERTEX_POINT('',#51245);
#11452=VERTEX_POINT('',#51249);
#11453=VERTEX_POINT('',#51251);
#11454=VERTEX_POINT('',#51255);
#11455=VERTEX_POINT('',#51257);
#11456=VERTEX_POINT('',#51261);
#11457=VERTEX_POINT('',#51263);
#11458=VERTEX_POINT('',#51267);
#11459=VERTEX_POINT('',#51269);
#11460=VERTEX_POINT('',#51273);
#11461=VERTEX_POINT('',#51275);
#11462=VERTEX_POINT('',#51279);
#11463=VERTEX_POINT('',#51281);
#11464=VERTEX_POINT('',#51285);
#11465=VERTEX_POINT('',#51287);
#11466=VERTEX_POINT('',#51291);
#11467=VERTEX_POINT('',#51293);
#11468=VERTEX_POINT('',#51297);
#11469=VERTEX_POINT('',#51299);
#11470=VERTEX_POINT('',#51303);
#11471=VERTEX_POINT('',#51305);
#11472=VERTEX_POINT('',#51309);
#11473=VERTEX_POINT('',#51311);
#11474=VERTEX_POINT('',#51315);
#11475=VERTEX_POINT('',#51317);
#11476=VERTEX_POINT('',#51321);
#11477=VERTEX_POINT('',#51323);
#11478=VERTEX_POINT('',#51327);
#11479=VERTEX_POINT('',#51329);
#11480=VERTEX_POINT('',#51333);
#11481=VERTEX_POINT('',#51335);
#11482=VERTEX_POINT('',#51339);
#11483=VERTEX_POINT('',#51341);
#11484=VERTEX_POINT('',#51345);
#11485=VERTEX_POINT('',#51347);
#11486=VERTEX_POINT('',#51351);
#11487=VERTEX_POINT('',#51353);
#11488=VERTEX_POINT('',#51357);
#11489=VERTEX_POINT('',#51359);
#11490=VERTEX_POINT('',#51363);
#11491=VERTEX_POINT('',#51365);
#11492=VERTEX_POINT('',#51369);
#11493=VERTEX_POINT('',#51371);
#11494=VERTEX_POINT('',#51375);
#11495=VERTEX_POINT('',#51377);
#11496=VERTEX_POINT('',#51381);
#11497=VERTEX_POINT('',#51383);
#11498=VERTEX_POINT('',#51387);
#11499=VERTEX_POINT('',#51389);
#11500=VERTEX_POINT('',#51393);
#11501=VERTEX_POINT('',#51395);
#11502=VERTEX_POINT('',#51399);
#11503=VERTEX_POINT('',#51401);
#11504=VERTEX_POINT('',#51405);
#11505=VERTEX_POINT('',#51407);
#11506=VERTEX_POINT('',#51411);
#11507=VERTEX_POINT('',#51413);
#11508=VERTEX_POINT('',#51417);
#11509=VERTEX_POINT('',#51419);
#11510=VERTEX_POINT('',#51423);
#11511=VERTEX_POINT('',#51425);
#11512=VERTEX_POINT('',#51429);
#11513=VERTEX_POINT('',#51431);
#11514=VERTEX_POINT('',#51435);
#11515=VERTEX_POINT('',#51437);
#11516=VERTEX_POINT('',#51441);
#11517=VERTEX_POINT('',#51443);
#11518=VERTEX_POINT('',#51447);
#11519=VERTEX_POINT('',#51449);
#11520=VERTEX_POINT('',#51453);
#11521=VERTEX_POINT('',#51455);
#11522=VERTEX_POINT('',#51459);
#11523=VERTEX_POINT('',#51461);
#11524=VERTEX_POINT('',#51465);
#11525=VERTEX_POINT('',#51467);
#11526=VERTEX_POINT('',#51471);
#11527=VERTEX_POINT('',#51473);
#11528=VERTEX_POINT('',#51477);
#11529=VERTEX_POINT('',#51479);
#11530=VERTEX_POINT('',#51483);
#11531=VERTEX_POINT('',#51485);
#11532=VERTEX_POINT('',#51489);
#11533=VERTEX_POINT('',#51491);
#11534=VERTEX_POINT('',#51495);
#11535=VERTEX_POINT('',#51500);
#11536=VERTEX_POINT('',#51504);
#11537=VERTEX_POINT('',#51509);
#11538=VERTEX_POINT('',#51513);
#11539=VERTEX_POINT('',#51518);
#11540=VERTEX_POINT('',#51522);
#11541=VERTEX_POINT('',#51527);
#11542=VERTEX_POINT('',#51531);
#11543=VERTEX_POINT('',#51536);
#11544=VERTEX_POINT('',#51540);
#11545=VERTEX_POINT('',#51545);
#11546=VERTEX_POINT('',#51549);
#11547=VERTEX_POINT('',#51554);
#11548=VERTEX_POINT('',#51558);
#11549=VERTEX_POINT('',#51563);
#11550=VERTEX_POINT('',#51567);
#11551=VERTEX_POINT('',#51572);
#11552=VERTEX_POINT('',#51576);
#11553=VERTEX_POINT('',#51581);
#11554=VERTEX_POINT('',#51585);
#11555=VERTEX_POINT('',#51590);
#11556=VERTEX_POINT('',#51594);
#11557=VERTEX_POINT('',#51599);
#11558=VERTEX_POINT('',#51603);
#11559=VERTEX_POINT('',#51608);
#11560=VERTEX_POINT('',#51612);
#11561=VERTEX_POINT('',#51617);
#11562=VERTEX_POINT('',#51621);
#11563=VERTEX_POINT('',#51626);
#11564=VERTEX_POINT('',#51630);
#11565=VERTEX_POINT('',#51632);
#11566=VERTEX_POINT('',#51636);
#11567=VERTEX_POINT('',#51638);
#11568=VERTEX_POINT('',#51642);
#11569=VERTEX_POINT('',#51644);
#11570=VERTEX_POINT('',#51648);
#11571=VERTEX_POINT('',#51650);
#11572=VERTEX_POINT('',#51654);
#11573=VERTEX_POINT('',#51656);
#11574=VERTEX_POINT('',#51660);
#11575=VERTEX_POINT('',#51662);
#11576=VERTEX_POINT('',#51666);
#11577=VERTEX_POINT('',#51668);
#11578=VERTEX_POINT('',#51672);
#11579=VERTEX_POINT('',#51674);
#11580=VERTEX_POINT('',#51678);
#11581=VERTEX_POINT('',#51680);
#11582=VERTEX_POINT('',#51684);
#11583=VERTEX_POINT('',#51686);
#11584=VERTEX_POINT('',#51690);
#11585=VERTEX_POINT('',#51692);
#11586=VERTEX_POINT('',#51696);
#11587=VERTEX_POINT('',#51698);
#11588=VERTEX_POINT('',#51702);
#11589=VERTEX_POINT('',#51704);
#11590=VERTEX_POINT('',#51708);
#11591=VERTEX_POINT('',#51710);
#11592=VERTEX_POINT('',#51714);
#11593=VERTEX_POINT('',#51716);
#11594=VERTEX_POINT('',#51720);
#11595=VERTEX_POINT('',#51722);
#11596=VERTEX_POINT('',#51726);
#11597=VERTEX_POINT('',#51728);
#11598=VERTEX_POINT('',#51732);
#11599=VERTEX_POINT('',#51734);
#11600=VERTEX_POINT('',#51738);
#11601=VERTEX_POINT('',#51740);
#11602=VERTEX_POINT('',#51744);
#11603=VERTEX_POINT('',#51746);
#11604=VERTEX_POINT('',#51750);
#11605=VERTEX_POINT('',#51752);
#11606=VERTEX_POINT('',#51756);
#11607=VERTEX_POINT('',#51758);
#11608=VERTEX_POINT('',#51762);
#11609=VERTEX_POINT('',#51764);
#11610=VERTEX_POINT('',#51768);
#11611=VERTEX_POINT('',#51770);
#11612=VERTEX_POINT('',#51774);
#11613=VERTEX_POINT('',#51776);
#11614=VERTEX_POINT('',#51780);
#11615=VERTEX_POINT('',#51782);
#11616=VERTEX_POINT('',#51786);
#11617=VERTEX_POINT('',#51788);
#11618=VERTEX_POINT('',#51792);
#11619=VERTEX_POINT('',#51794);
#11620=VERTEX_POINT('',#51798);
#11621=VERTEX_POINT('',#51800);
#11622=VERTEX_POINT('',#51804);
#11623=VERTEX_POINT('',#51806);
#11624=VERTEX_POINT('',#51810);
#11625=VERTEX_POINT('',#51812);
#11626=VERTEX_POINT('',#51816);
#11627=VERTEX_POINT('',#51818);
#11628=VERTEX_POINT('',#51822);
#11629=VERTEX_POINT('',#51824);
#11630=VERTEX_POINT('',#51828);
#11631=VERTEX_POINT('',#51830);
#11632=VERTEX_POINT('',#51834);
#11633=VERTEX_POINT('',#51836);
#11634=VERTEX_POINT('',#51840);
#11635=VERTEX_POINT('',#51842);
#11636=VERTEX_POINT('',#51846);
#11637=VERTEX_POINT('',#51848);
#11638=VERTEX_POINT('',#51852);
#11639=VERTEX_POINT('',#51854);
#11640=VERTEX_POINT('',#51858);
#11641=VERTEX_POINT('',#51860);
#11642=VERTEX_POINT('',#51874);
#11643=VERTEX_POINT('',#51875);
#11644=VERTEX_POINT('',#51884);
#11645=VERTEX_POINT('',#51888);
#11646=VERTEX_POINT('',#51890);
#11647=VERTEX_POINT('',#51894);
#11648=VERTEX_POINT('',#51896);
#11649=VERTEX_POINT('',#51900);
#11650=VERTEX_POINT('',#51902);
#11651=VERTEX_POINT('',#51906);
#11652=VERTEX_POINT('',#51908);
#11653=VERTEX_POINT('',#51912);
#11654=VERTEX_POINT('',#51914);
#11655=VERTEX_POINT('',#51918);
#11656=VERTEX_POINT('',#51920);
#11657=VERTEX_POINT('',#51924);
#11658=VERTEX_POINT('',#51926);
#11659=VERTEX_POINT('',#51930);
#11660=VERTEX_POINT('',#51932);
#11661=VERTEX_POINT('',#51936);
#11662=VERTEX_POINT('',#51938);
#11663=VERTEX_POINT('',#51942);
#11664=VERTEX_POINT('',#51944);
#11665=VERTEX_POINT('',#51948);
#11666=VERTEX_POINT('',#51950);
#11667=VERTEX_POINT('',#51954);
#11668=VERTEX_POINT('',#51956);
#11669=VERTEX_POINT('',#51960);
#11670=VERTEX_POINT('',#51962);
#11671=VERTEX_POINT('',#51966);
#11672=VERTEX_POINT('',#51968);
#11673=VERTEX_POINT('',#51972);
#11674=VERTEX_POINT('',#51974);
#11675=VERTEX_POINT('',#51978);
#11676=VERTEX_POINT('',#51980);
#11677=VERTEX_POINT('',#51984);
#11678=VERTEX_POINT('',#51986);
#11679=VERTEX_POINT('',#51990);
#11680=VERTEX_POINT('',#51992);
#11681=VERTEX_POINT('',#51996);
#11682=VERTEX_POINT('',#51998);
#11683=VERTEX_POINT('',#52002);
#11684=VERTEX_POINT('',#52004);
#11685=VERTEX_POINT('',#52008);
#11686=VERTEX_POINT('',#52010);
#11687=VERTEX_POINT('',#52014);
#11688=VERTEX_POINT('',#52016);
#11689=VERTEX_POINT('',#52020);
#11690=VERTEX_POINT('',#52022);
#11691=VERTEX_POINT('',#52026);
#11692=VERTEX_POINT('',#52028);
#11693=VERTEX_POINT('',#52032);
#11694=VERTEX_POINT('',#52034);
#11695=VERTEX_POINT('',#52038);
#11696=VERTEX_POINT('',#52040);
#11697=VERTEX_POINT('',#52044);
#11698=VERTEX_POINT('',#52046);
#11699=VERTEX_POINT('',#52050);
#11700=VERTEX_POINT('',#52052);
#11701=VERTEX_POINT('',#52056);
#11702=VERTEX_POINT('',#52058);
#11703=VERTEX_POINT('',#52062);
#11704=VERTEX_POINT('',#52064);
#11705=VERTEX_POINT('',#52068);
#11706=VERTEX_POINT('',#52070);
#11707=VERTEX_POINT('',#52074);
#11708=VERTEX_POINT('',#52076);
#11709=VERTEX_POINT('',#52080);
#11710=VERTEX_POINT('',#52082);
#11711=VERTEX_POINT('',#52086);
#11712=VERTEX_POINT('',#52088);
#11713=VERTEX_POINT('',#52092);
#11714=VERTEX_POINT('',#52094);
#11715=VERTEX_POINT('',#52098);
#11716=VERTEX_POINT('',#52100);
#11717=VERTEX_POINT('',#52104);
#11718=VERTEX_POINT('',#52106);
#11719=VERTEX_POINT('',#52110);
#11720=VERTEX_POINT('',#52112);
#11721=VERTEX_POINT('',#52116);
#11722=VERTEX_POINT('',#52118);
#11723=VERTEX_POINT('',#52122);
#11724=VERTEX_POINT('',#52124);
#11725=VERTEX_POINT('',#52128);
#11726=VERTEX_POINT('',#52130);
#11727=VERTEX_POINT('',#52134);
#11728=VERTEX_POINT('',#52136);
#11729=VERTEX_POINT('',#52140);
#11730=VERTEX_POINT('',#52142);
#11731=VERTEX_POINT('',#52146);
#11732=VERTEX_POINT('',#52148);
#11733=VERTEX_POINT('',#52152);
#11734=VERTEX_POINT('',#52154);
#11735=VERTEX_POINT('',#52158);
#11736=VERTEX_POINT('',#52160);
#11737=VERTEX_POINT('',#52164);
#11738=VERTEX_POINT('',#52166);
#11739=VERTEX_POINT('',#52170);
#11740=VERTEX_POINT('',#52172);
#11741=VERTEX_POINT('',#52176);
#11742=VERTEX_POINT('',#52178);
#11743=VERTEX_POINT('',#52182);
#11744=VERTEX_POINT('',#52184);
#11745=VERTEX_POINT('',#52188);
#11746=VERTEX_POINT('',#52190);
#11747=VERTEX_POINT('',#52194);
#11748=VERTEX_POINT('',#52196);
#11749=VERTEX_POINT('',#52200);
#11750=VERTEX_POINT('',#52202);
#11751=VERTEX_POINT('',#52206);
#11752=VERTEX_POINT('',#52208);
#11753=VERTEX_POINT('',#52212);
#11754=VERTEX_POINT('',#52214);
#11755=VERTEX_POINT('',#52218);
#11756=VERTEX_POINT('',#52220);
#11757=VERTEX_POINT('',#52224);
#11758=VERTEX_POINT('',#52226);
#11759=VERTEX_POINT('',#52230);
#11760=VERTEX_POINT('',#52232);
#11761=VERTEX_POINT('',#52236);
#11762=VERTEX_POINT('',#52238);
#11763=VERTEX_POINT('',#52242);
#11764=VERTEX_POINT('',#52244);
#11765=VERTEX_POINT('',#52248);
#11766=VERTEX_POINT('',#52250);
#11767=VERTEX_POINT('',#52254);
#11768=VERTEX_POINT('',#52256);
#11769=VERTEX_POINT('',#52260);
#11770=VERTEX_POINT('',#52262);
#11771=VERTEX_POINT('',#52266);
#11772=VERTEX_POINT('',#52268);
#11773=VERTEX_POINT('',#52272);
#11774=VERTEX_POINT('',#52274);
#11775=VERTEX_POINT('',#52278);
#11776=VERTEX_POINT('',#52280);
#11777=VERTEX_POINT('',#52284);
#11778=VERTEX_POINT('',#52286);
#11779=VERTEX_POINT('',#52290);
#11780=VERTEX_POINT('',#52292);
#11781=VERTEX_POINT('',#52296);
#11782=VERTEX_POINT('',#52298);
#11783=VERTEX_POINT('',#52302);
#11784=VERTEX_POINT('',#52304);
#11785=VERTEX_POINT('',#52308);
#11786=VERTEX_POINT('',#52310);
#11787=VERTEX_POINT('',#52314);
#11788=VERTEX_POINT('',#52316);
#11789=VERTEX_POINT('',#52320);
#11790=VERTEX_POINT('',#52322);
#11791=VERTEX_POINT('',#52326);
#11792=VERTEX_POINT('',#52328);
#11793=VERTEX_POINT('',#52332);
#11794=VERTEX_POINT('',#52334);
#11795=VERTEX_POINT('',#52338);
#11796=VERTEX_POINT('',#52340);
#11797=VERTEX_POINT('',#52344);
#11798=VERTEX_POINT('',#52346);
#11799=VERTEX_POINT('',#52350);
#11800=VERTEX_POINT('',#52352);
#11801=VERTEX_POINT('',#52356);
#11802=VERTEX_POINT('',#52358);
#11803=VERTEX_POINT('',#52362);
#11804=VERTEX_POINT('',#52364);
#11805=VERTEX_POINT('',#52368);
#11806=VERTEX_POINT('',#52370);
#11807=VERTEX_POINT('',#52374);
#11808=VERTEX_POINT('',#52376);
#11809=VERTEX_POINT('',#52380);
#11810=VERTEX_POINT('',#52382);
#11811=VERTEX_POINT('',#52386);
#11812=VERTEX_POINT('',#52388);
#11813=VERTEX_POINT('',#52392);
#11814=VERTEX_POINT('',#52394);
#11815=VERTEX_POINT('',#52398);
#11816=VERTEX_POINT('',#52400);
#11817=VERTEX_POINT('',#52404);
#11818=VERTEX_POINT('',#52406);
#11819=VERTEX_POINT('',#52410);
#11820=VERTEX_POINT('',#52412);
#11821=VERTEX_POINT('',#52416);
#11822=VERTEX_POINT('',#52418);
#11823=VERTEX_POINT('',#52422);
#11824=VERTEX_POINT('',#52424);
#11825=VERTEX_POINT('',#52428);
#11826=VERTEX_POINT('',#52430);
#11827=VERTEX_POINT('',#52434);
#11828=VERTEX_POINT('',#52436);
#11829=VERTEX_POINT('',#52440);
#11830=VERTEX_POINT('',#52442);
#11831=VERTEX_POINT('',#52446);
#11832=VERTEX_POINT('',#52448);
#11833=VERTEX_POINT('',#52452);
#11834=VERTEX_POINT('',#52454);
#11835=VERTEX_POINT('',#52458);
#11836=VERTEX_POINT('',#52460);
#11837=VERTEX_POINT('',#52464);
#11838=VERTEX_POINT('',#52466);
#11839=VERTEX_POINT('',#52470);
#11840=VERTEX_POINT('',#52472);
#11841=VERTEX_POINT('',#52476);
#11842=VERTEX_POINT('',#52478);
#11843=VERTEX_POINT('',#52482);
#11844=VERTEX_POINT('',#52484);
#11845=VERTEX_POINT('',#52488);
#11846=VERTEX_POINT('',#52490);
#11847=VERTEX_POINT('',#52494);
#11848=VERTEX_POINT('',#52496);
#11849=VERTEX_POINT('',#52500);
#11850=VERTEX_POINT('',#52502);
#11851=VERTEX_POINT('',#52506);
#11852=VERTEX_POINT('',#52508);
#11853=VERTEX_POINT('',#52512);
#11854=VERTEX_POINT('',#52514);
#11855=VERTEX_POINT('',#52518);
#11856=VERTEX_POINT('',#52520);
#11857=VERTEX_POINT('',#52524);
#11858=VERTEX_POINT('',#52526);
#11859=VERTEX_POINT('',#52530);
#11860=VERTEX_POINT('',#52532);
#11861=VERTEX_POINT('',#52536);
#11862=VERTEX_POINT('',#52538);
#11863=VERTEX_POINT('',#52542);
#11864=VERTEX_POINT('',#52544);
#11865=VERTEX_POINT('',#52548);
#11866=VERTEX_POINT('',#52550);
#11867=VERTEX_POINT('',#52554);
#11868=VERTEX_POINT('',#52556);
#11869=VERTEX_POINT('',#52560);
#11870=VERTEX_POINT('',#52562);
#11871=VERTEX_POINT('',#52566);
#11872=VERTEX_POINT('',#52568);
#11873=VERTEX_POINT('',#52572);
#11874=VERTEX_POINT('',#52574);
#11875=VERTEX_POINT('',#52578);
#11876=VERTEX_POINT('',#52580);
#11877=VERTEX_POINT('',#52584);
#11878=VERTEX_POINT('',#52586);
#11879=VERTEX_POINT('',#52590);
#11880=VERTEX_POINT('',#52592);
#11881=VERTEX_POINT('',#52596);
#11882=VERTEX_POINT('',#52601);
#11883=VERTEX_POINT('',#52605);
#11884=VERTEX_POINT('',#52610);
#11885=VERTEX_POINT('',#52614);
#11886=VERTEX_POINT('',#52619);
#11887=VERTEX_POINT('',#52623);
#11888=VERTEX_POINT('',#52628);
#11889=VERTEX_POINT('',#52632);
#11890=VERTEX_POINT('',#52637);
#11891=VERTEX_POINT('',#52641);
#11892=VERTEX_POINT('',#52646);
#11893=VERTEX_POINT('',#52650);
#11894=VERTEX_POINT('',#52655);
#11895=VERTEX_POINT('',#52659);
#11896=VERTEX_POINT('',#52664);
#11897=VERTEX_POINT('',#52668);
#11898=VERTEX_POINT('',#52673);
#11899=VERTEX_POINT('',#52677);
#11900=VERTEX_POINT('',#52682);
#11901=VERTEX_POINT('',#52686);
#11902=VERTEX_POINT('',#52691);
#11903=VERTEX_POINT('',#52695);
#11904=VERTEX_POINT('',#52700);
#11905=VERTEX_POINT('',#52704);
#11906=VERTEX_POINT('',#52709);
#11907=VERTEX_POINT('',#52713);
#11908=VERTEX_POINT('',#52718);
#11909=VERTEX_POINT('',#52722);
#11910=VERTEX_POINT('',#52727);
#11911=VERTEX_POINT('',#52731);
#11912=VERTEX_POINT('',#52733);
#11913=VERTEX_POINT('',#52737);
#11914=VERTEX_POINT('',#52739);
#11915=VERTEX_POINT('',#52743);
#11916=VERTEX_POINT('',#52745);
#11917=VERTEX_POINT('',#52749);
#11918=VERTEX_POINT('',#52751);
#11919=VERTEX_POINT('',#52755);
#11920=VERTEX_POINT('',#52757);
#11921=VERTEX_POINT('',#52761);
#11922=VERTEX_POINT('',#52763);
#11923=VERTEX_POINT('',#52767);
#11924=VERTEX_POINT('',#52769);
#11925=VERTEX_POINT('',#52773);
#11926=VERTEX_POINT('',#52775);
#11927=VERTEX_POINT('',#52779);
#11928=VERTEX_POINT('',#52781);
#11929=VERTEX_POINT('',#52785);
#11930=VERTEX_POINT('',#52787);
#11931=VERTEX_POINT('',#52791);
#11932=VERTEX_POINT('',#52793);
#11933=VERTEX_POINT('',#52805);
#11934=VERTEX_POINT('',#52807);
#11935=VERTEX_POINT('',#52811);
#11936=VERTEX_POINT('',#52815);
#11937=VERTEX_POINT('',#52819);
#11938=VERTEX_POINT('',#52823);
#11939=VERTEX_POINT('',#52827);
#11940=VERTEX_POINT('',#52829);
#11941=VERTEX_POINT('',#52833);
#11942=VERTEX_POINT('',#52835);
#11943=VERTEX_POINT('',#52839);
#11944=VERTEX_POINT('',#52841);
#11945=VERTEX_POINT('',#52845);
#11946=VERTEX_POINT('',#52847);
#11947=VERTEX_POINT('',#52851);
#11948=VERTEX_POINT('',#52853);
#11949=VERTEX_POINT('',#52857);
#11950=VERTEX_POINT('',#52859);
#11951=VERTEX_POINT('',#52863);
#11952=VERTEX_POINT('',#52865);
#11953=VERTEX_POINT('',#52869);
#11954=VERTEX_POINT('',#52871);
#11955=VERTEX_POINT('',#52875);
#11956=VERTEX_POINT('',#52877);
#11957=VERTEX_POINT('',#52881);
#11958=VERTEX_POINT('',#52883);
#11959=VERTEX_POINT('',#52887);
#11960=VERTEX_POINT('',#52889);
#11961=VERTEX_POINT('',#52893);
#11962=VERTEX_POINT('',#52895);
#11963=VERTEX_POINT('',#52899);
#11964=VERTEX_POINT('',#52901);
#11965=VERTEX_POINT('',#52905);
#11966=VERTEX_POINT('',#52907);
#11967=VERTEX_POINT('',#52911);
#11968=VERTEX_POINT('',#52913);
#11969=VERTEX_POINT('',#52917);
#11970=VERTEX_POINT('',#52919);
#11971=VERTEX_POINT('',#52923);
#11972=VERTEX_POINT('',#52925);
#11973=VERTEX_POINT('',#52929);
#11974=VERTEX_POINT('',#52931);
#11975=VERTEX_POINT('',#52935);
#11976=VERTEX_POINT('',#52937);
#11977=VERTEX_POINT('',#52941);
#11978=VERTEX_POINT('',#52943);
#11979=VERTEX_POINT('',#52947);
#11980=VERTEX_POINT('',#52949);
#11981=VERTEX_POINT('',#52953);
#11982=VERTEX_POINT('',#52955);
#11983=VERTEX_POINT('',#52959);
#11984=VERTEX_POINT('',#52961);
#11985=VERTEX_POINT('',#52965);
#11986=VERTEX_POINT('',#52967);
#11987=VERTEX_POINT('',#52971);
#11988=VERTEX_POINT('',#52973);
#11989=VERTEX_POINT('',#52977);
#11990=VERTEX_POINT('',#52979);
#11991=VERTEX_POINT('',#52983);
#11992=VERTEX_POINT('',#52985);
#11993=VERTEX_POINT('',#52989);
#11994=VERTEX_POINT('',#52991);
#11995=VERTEX_POINT('',#52995);
#11996=VERTEX_POINT('',#52997);
#11997=VERTEX_POINT('',#53001);
#11998=VERTEX_POINT('',#53003);
#11999=VERTEX_POINT('',#53007);
#12000=VERTEX_POINT('',#53009);
#12001=VERTEX_POINT('',#53013);
#12002=VERTEX_POINT('',#53015);
#12003=VERTEX_POINT('',#53019);
#12004=VERTEX_POINT('',#53021);
#12005=VERTEX_POINT('',#53025);
#12006=VERTEX_POINT('',#53027);
#12007=VERTEX_POINT('',#53031);
#12008=VERTEX_POINT('',#53033);
#12009=VERTEX_POINT('',#53037);
#12010=VERTEX_POINT('',#53039);
#12011=VERTEX_POINT('',#53043);
#12012=VERTEX_POINT('',#53045);
#12013=VERTEX_POINT('',#53049);
#12014=VERTEX_POINT('',#53051);
#12015=VERTEX_POINT('',#53055);
#12016=VERTEX_POINT('',#53057);
#12017=VERTEX_POINT('',#53061);
#12018=VERTEX_POINT('',#53063);
#12019=VERTEX_POINT('',#53067);
#12020=VERTEX_POINT('',#53069);
#12021=VERTEX_POINT('',#53073);
#12022=VERTEX_POINT('',#53075);
#12023=VERTEX_POINT('',#53079);
#12024=VERTEX_POINT('',#53081);
#12025=VERTEX_POINT('',#53085);
#12026=VERTEX_POINT('',#53087);
#12027=VERTEX_POINT('',#53091);
#12028=VERTEX_POINT('',#53093);
#12029=VERTEX_POINT('',#53097);
#12030=VERTEX_POINT('',#53099);
#12031=VERTEX_POINT('',#53103);
#12032=VERTEX_POINT('',#53105);
#12033=VERTEX_POINT('',#53109);
#12034=VERTEX_POINT('',#53111);
#12035=VERTEX_POINT('',#53115);
#12036=VERTEX_POINT('',#53117);
#12037=VERTEX_POINT('',#53121);
#12038=VERTEX_POINT('',#53123);
#12039=VERTEX_POINT('',#53127);
#12040=VERTEX_POINT('',#53129);
#12041=VERTEX_POINT('',#53133);
#12042=VERTEX_POINT('',#53135);
#12043=VERTEX_POINT('',#53139);
#12044=VERTEX_POINT('',#53141);
#12045=VERTEX_POINT('',#53145);
#12046=VERTEX_POINT('',#53147);
#12047=VERTEX_POINT('',#53151);
#12048=VERTEX_POINT('',#53153);
#12049=VERTEX_POINT('',#53157);
#12050=VERTEX_POINT('',#53159);
#12051=VERTEX_POINT('',#53163);
#12052=VERTEX_POINT('',#53165);
#12053=VERTEX_POINT('',#53169);
#12054=VERTEX_POINT('',#53171);
#12055=VERTEX_POINT('',#53175);
#12056=VERTEX_POINT('',#53177);
#12057=VERTEX_POINT('',#53181);
#12058=VERTEX_POINT('',#53183);
#12059=VERTEX_POINT('',#53187);
#12060=VERTEX_POINT('',#53189);
#12061=VERTEX_POINT('',#53193);
#12062=VERTEX_POINT('',#53195);
#12063=VERTEX_POINT('',#53199);
#12064=VERTEX_POINT('',#53201);
#12065=VERTEX_POINT('',#53205);
#12066=VERTEX_POINT('',#53207);
#12067=VERTEX_POINT('',#53211);
#12068=VERTEX_POINT('',#53213);
#12069=VERTEX_POINT('',#53217);
#12070=VERTEX_POINT('',#53219);
#12071=VERTEX_POINT('',#53223);
#12072=VERTEX_POINT('',#53225);
#12073=VERTEX_POINT('',#53229);
#12074=VERTEX_POINT('',#53231);
#12075=VERTEX_POINT('',#53235);
#12076=VERTEX_POINT('',#53237);
#12077=VERTEX_POINT('',#53241);
#12078=VERTEX_POINT('',#53243);
#12079=VERTEX_POINT('',#53247);
#12080=VERTEX_POINT('',#53249);
#12081=VERTEX_POINT('',#53253);
#12082=VERTEX_POINT('',#53255);
#12083=VERTEX_POINT('',#53259);
#12084=VERTEX_POINT('',#53261);
#12085=VERTEX_POINT('',#53265);
#12086=VERTEX_POINT('',#53267);
#12087=VERTEX_POINT('',#53271);
#12088=VERTEX_POINT('',#53273);
#12089=VERTEX_POINT('',#53277);
#12090=VERTEX_POINT('',#53279);
#12091=VERTEX_POINT('',#53283);
#12092=VERTEX_POINT('',#53285);
#12093=VERTEX_POINT('',#53289);
#12094=VERTEX_POINT('',#53291);
#12095=VERTEX_POINT('',#53295);
#12096=VERTEX_POINT('',#53297);
#12097=VERTEX_POINT('',#53301);
#12098=VERTEX_POINT('',#53303);
#12099=VERTEX_POINT('',#53307);
#12100=VERTEX_POINT('',#53309);
#12101=VERTEX_POINT('',#53313);
#12102=VERTEX_POINT('',#53315);
#12103=VERTEX_POINT('',#53319);
#12104=VERTEX_POINT('',#53321);
#12105=VERTEX_POINT('',#53325);
#12106=VERTEX_POINT('',#53327);
#12107=VERTEX_POINT('',#53331);
#12108=VERTEX_POINT('',#53333);
#12109=VERTEX_POINT('',#53337);
#12110=VERTEX_POINT('',#53339);
#12111=VERTEX_POINT('',#53343);
#12112=VERTEX_POINT('',#53345);
#12113=VERTEX_POINT('',#53349);
#12114=VERTEX_POINT('',#53351);
#12115=VERTEX_POINT('',#53355);
#12116=VERTEX_POINT('',#53357);
#12117=VERTEX_POINT('',#53361);
#12118=VERTEX_POINT('',#53363);
#12119=VERTEX_POINT('',#53367);
#12120=VERTEX_POINT('',#53369);
#12121=VERTEX_POINT('',#53373);
#12122=VERTEX_POINT('',#53375);
#12123=VERTEX_POINT('',#53379);
#12124=VERTEX_POINT('',#53381);
#12125=VERTEX_POINT('',#53385);
#12126=VERTEX_POINT('',#53387);
#12127=VERTEX_POINT('',#53391);
#12128=VERTEX_POINT('',#53393);
#12129=VERTEX_POINT('',#53397);
#12130=VERTEX_POINT('',#53399);
#12131=VERTEX_POINT('',#53403);
#12132=VERTEX_POINT('',#53405);
#12133=VERTEX_POINT('',#53409);
#12134=VERTEX_POINT('',#53411);
#12135=VERTEX_POINT('',#53415);
#12136=VERTEX_POINT('',#53417);
#12137=VERTEX_POINT('',#53421);
#12138=VERTEX_POINT('',#53423);
#12139=VERTEX_POINT('',#53427);
#12140=VERTEX_POINT('',#53429);
#12141=VERTEX_POINT('',#53433);
#12142=VERTEX_POINT('',#53435);
#12143=VERTEX_POINT('',#53439);
#12144=VERTEX_POINT('',#53441);
#12145=VERTEX_POINT('',#53445);
#12146=VERTEX_POINT('',#53447);
#12147=VERTEX_POINT('',#53451);
#12148=VERTEX_POINT('',#53453);
#12149=VERTEX_POINT('',#53457);
#12150=VERTEX_POINT('',#53459);
#12151=VERTEX_POINT('',#53463);
#12152=VERTEX_POINT('',#53465);
#12153=VERTEX_POINT('',#53469);
#12154=VERTEX_POINT('',#53471);
#12155=VERTEX_POINT('',#53475);
#12156=VERTEX_POINT('',#53477);
#12157=VERTEX_POINT('',#53481);
#12158=VERTEX_POINT('',#53483);
#12159=VERTEX_POINT('',#53487);
#12160=VERTEX_POINT('',#53489);
#12161=VERTEX_POINT('',#53493);
#12162=VERTEX_POINT('',#53495);
#12163=VERTEX_POINT('',#53499);
#12164=VERTEX_POINT('',#53501);
#12165=VERTEX_POINT('',#53505);
#12166=VERTEX_POINT('',#53507);
#12167=VERTEX_POINT('',#53511);
#12168=VERTEX_POINT('',#53513);
#12169=VERTEX_POINT('',#53517);
#12170=VERTEX_POINT('',#53519);
#12171=VERTEX_POINT('',#53523);
#12172=VERTEX_POINT('',#53525);
#12173=VERTEX_POINT('',#53529);
#12174=VERTEX_POINT('',#53531);
#12175=VERTEX_POINT('',#53535);
#12176=VERTEX_POINT('',#53537);
#12177=VERTEX_POINT('',#53541);
#12178=VERTEX_POINT('',#53543);
#12179=VERTEX_POINT('',#53547);
#12180=VERTEX_POINT('',#53549);
#12181=VERTEX_POINT('',#53553);
#12182=VERTEX_POINT('',#53555);
#12183=VERTEX_POINT('',#53559);
#12184=VERTEX_POINT('',#53561);
#12185=VERTEX_POINT('',#53565);
#12186=VERTEX_POINT('',#53567);
#12187=VERTEX_POINT('',#53571);
#12188=VERTEX_POINT('',#53573);
#12189=VERTEX_POINT('',#53577);
#12190=VERTEX_POINT('',#53579);
#12191=VERTEX_POINT('',#53583);
#12192=VERTEX_POINT('',#53585);
#12193=VERTEX_POINT('',#53589);
#12194=VERTEX_POINT('',#53591);
#12195=VERTEX_POINT('',#53595);
#12196=VERTEX_POINT('',#53597);
#12197=VERTEX_POINT('',#53601);
#12198=VERTEX_POINT('',#53603);
#12199=VERTEX_POINT('',#53607);
#12200=VERTEX_POINT('',#53609);
#12201=VERTEX_POINT('',#53613);
#12202=VERTEX_POINT('',#53615);
#12203=VERTEX_POINT('',#53619);
#12204=VERTEX_POINT('',#53621);
#12205=VERTEX_POINT('',#53625);
#12206=VERTEX_POINT('',#53627);
#12207=VERTEX_POINT('',#53631);
#12208=VERTEX_POINT('',#53633);
#12209=VERTEX_POINT('',#53637);
#12210=VERTEX_POINT('',#53639);
#12211=VERTEX_POINT('',#53643);
#12212=VERTEX_POINT('',#53645);
#12213=VERTEX_POINT('',#53649);
#12214=VERTEX_POINT('',#53651);
#12215=VERTEX_POINT('',#53655);
#12216=VERTEX_POINT('',#53657);
#12217=VERTEX_POINT('',#53661);
#12218=VERTEX_POINT('',#53663);
#12219=VERTEX_POINT('',#53667);
#12220=VERTEX_POINT('',#53669);
#12221=VERTEX_POINT('',#53673);
#12222=VERTEX_POINT('',#53675);
#12223=VERTEX_POINT('',#53679);
#12224=VERTEX_POINT('',#53681);
#12225=VERTEX_POINT('',#53685);
#12226=VERTEX_POINT('',#53687);
#12227=VERTEX_POINT('',#53691);
#12228=VERTEX_POINT('',#53693);
#12229=VERTEX_POINT('',#53697);
#12230=VERTEX_POINT('',#53699);
#12231=VERTEX_POINT('',#53703);
#12232=VERTEX_POINT('',#53705);
#12233=VERTEX_POINT('',#53709);
#12234=VERTEX_POINT('',#53711);
#12235=VERTEX_POINT('',#53715);
#12236=VERTEX_POINT('',#53717);
#12237=VERTEX_POINT('',#53721);
#12238=VERTEX_POINT('',#53723);
#12239=VERTEX_POINT('',#53727);
#12240=VERTEX_POINT('',#53729);
#12241=VERTEX_POINT('',#53733);
#12242=VERTEX_POINT('',#53735);
#12243=VERTEX_POINT('',#53739);
#12244=VERTEX_POINT('',#53741);
#12245=VERTEX_POINT('',#53745);
#12246=VERTEX_POINT('',#53747);
#12247=VERTEX_POINT('',#53751);
#12248=VERTEX_POINT('',#53753);
#12249=VERTEX_POINT('',#53757);
#12250=VERTEX_POINT('',#53759);
#12251=VERTEX_POINT('',#53763);
#12252=VERTEX_POINT('',#53765);
#12253=VERTEX_POINT('',#53769);
#12254=VERTEX_POINT('',#53771);
#12255=VERTEX_POINT('',#54014);
#12256=VERTEX_POINT('',#54016);
#12257=VERTEX_POINT('',#54020);
#12258=VERTEX_POINT('',#54022);
#12259=VERTEX_POINT('',#54030);
#12260=VERTEX_POINT('',#54031);
#12261=VERTEX_POINT('',#54033);
#12262=VERTEX_POINT('',#54035);
#12263=VERTEX_POINT('',#54037);
#12264=VERTEX_POINT('',#54039);
#12265=VERTEX_POINT('',#55933);
#12266=VERTEX_POINT('',#55934);
#12267=VERTEX_POINT('',#55936);
#12268=VERTEX_POINT('',#55973);
#12269=VERTEX_POINT('',#55976);
#12270=VERTEX_POINT('',#56013);
#12271=VERTEX_POINT('',#56014);
#12272=VERTEX_POINT('',#56089);
#12273=VERTEX_POINT('',#56090);
#12274=VERTEX_POINT('',#56167);
#12275=VERTEX_POINT('',#56168);
#12276=VERTEX_POINT('',#56243);
#12277=VERTEX_POINT('',#56244);
#12278=VERTEX_POINT('',#56319);
#12279=VERTEX_POINT('',#56320);
#12280=VERTEX_POINT('',#56395);
#12281=VERTEX_POINT('',#56396);
#12282=VERTEX_POINT('',#56471);
#12283=VERTEX_POINT('',#56472);
#12284=VERTEX_POINT('',#56549);
#12285=VERTEX_POINT('',#56550);
#12286=VERTEX_POINT('',#56627);
#12287=VERTEX_POINT('',#56628);
#12288=VERTEX_POINT('',#56703);
#12289=VERTEX_POINT('',#56704);
#12290=VERTEX_POINT('',#56779);
#12291=VERTEX_POINT('',#56780);
#12292=VERTEX_POINT('',#56855);
#12293=VERTEX_POINT('',#56856);
#12294=VERTEX_POINT('',#56931);
#12295=VERTEX_POINT('',#56932);
#12296=VERTEX_POINT('',#57009);
#12297=VERTEX_POINT('',#57010);
#12298=VERTEX_POINT('',#57085);
#12299=VERTEX_POINT('',#57086);
#12300=VERTEX_POINT('',#57163);
#12301=VERTEX_POINT('',#57164);
#12302=VERTEX_POINT('',#57239);
#12303=VERTEX_POINT('',#57240);
#12304=VERTEX_POINT('',#57315);
#12305=VERTEX_POINT('',#57316);
#12306=VERTEX_POINT('',#57391);
#12307=VERTEX_POINT('',#57392);
#12308=VERTEX_POINT('',#57467);
#12309=VERTEX_POINT('',#57468);
#12310=VERTEX_POINT('',#57545);
#12311=VERTEX_POINT('',#57546);
#12312=VERTEX_POINT('',#57623);
#12313=VERTEX_POINT('',#57624);
#12314=VERTEX_POINT('',#57699);
#12315=VERTEX_POINT('',#57700);
#12316=VERTEX_POINT('',#57775);
#12317=VERTEX_POINT('',#57776);
#12318=VERTEX_POINT('',#57851);
#12319=VERTEX_POINT('',#57852);
#12320=VERTEX_POINT('',#57927);
#12321=VERTEX_POINT('',#57928);
#12322=VERTEX_POINT('',#58005);
#12323=VERTEX_POINT('',#58006);
#12324=VERTEX_POINT('',#58081);
#12325=VERTEX_POINT('',#58082);
#12326=VERTEX_POINT('',#58084);
#12327=VERTEX_POINT('',#58107);
#12328=VERTEX_POINT('',#58109);
#12329=VERTEX_POINT('',#58120);
#12330=VERTEX_POINT('',#58121);
#12331=VERTEX_POINT('',#58196);
#12332=VERTEX_POINT('',#58197);
#12333=VERTEX_POINT('',#58272);
#12334=VERTEX_POINT('',#58273);
#12335=VERTEX_POINT('',#58350);
#12336=VERTEX_POINT('',#58351);
#12337=VERTEX_POINT('',#58426);
#12338=VERTEX_POINT('',#58427);
#12339=VERTEX_POINT('',#58504);
#12340=VERTEX_POINT('',#58505);
#12341=VERTEX_POINT('',#58580);
#12342=VERTEX_POINT('',#58581);
#12343=VERTEX_POINT('',#58656);
#12344=VERTEX_POINT('',#58657);
#12345=VERTEX_POINT('',#58732);
#12346=VERTEX_POINT('',#58733);
#12347=VERTEX_POINT('',#58808);
#12348=VERTEX_POINT('',#58809);
#12349=VERTEX_POINT('',#58886);
#12350=VERTEX_POINT('',#58887);
#12351=VERTEX_POINT('',#58962);
#12352=VERTEX_POINT('',#58963);
#12353=VERTEX_POINT('',#59040);
#12354=VERTEX_POINT('',#59041);
#12355=VERTEX_POINT('',#59116);
#12356=VERTEX_POINT('',#59117);
#12357=VERTEX_POINT('',#59192);
#12358=VERTEX_POINT('',#59193);
#12359=VERTEX_POINT('',#59268);
#12360=VERTEX_POINT('',#59269);
#12361=VERTEX_POINT('',#59344);
#12362=VERTEX_POINT('',#59345);
#12363=VERTEX_POINT('',#59420);
#12364=VERTEX_POINT('',#59421);
#12365=VERTEX_POINT('',#59498);
#12366=VERTEX_POINT('',#59499);
#12367=VERTEX_POINT('',#59574);
#12368=VERTEX_POINT('',#59575);
#12369=VERTEX_POINT('',#59652);
#12370=VERTEX_POINT('',#59653);
#12371=VERTEX_POINT('',#59728);
#12372=VERTEX_POINT('',#59729);
#12373=VERTEX_POINT('',#59804);
#12374=VERTEX_POINT('',#59805);
#12375=VERTEX_POINT('',#59880);
#12376=VERTEX_POINT('',#59881);
#12377=VERTEX_POINT('',#59956);
#12378=VERTEX_POINT('',#59957);
#12379=VERTEX_POINT('',#60034);
#12380=VERTEX_POINT('',#60035);
#12381=VERTEX_POINT('',#60110);
#12382=VERTEX_POINT('',#60111);
#12383=VERTEX_POINT('',#60188);
#12384=VERTEX_POINT('',#60189);
#12385=VERTEX_POINT('',#60264);
#12386=VERTEX_POINT('',#60265);
#12387=VERTEX_POINT('',#60340);
#12388=VERTEX_POINT('',#60352);
#12389=VERTEX_POINT('',#60365);
#12390=VERTEX_POINT('',#60457);
#12391=VERTEX_POINT('',#60458);
#12392=VERTEX_POINT('',#60460);
#12393=VERTEX_POINT('',#60462);
#12394=VERTEX_POINT('',#60466);
#12395=VERTEX_POINT('',#60467);
#12396=VERTEX_POINT('',#60469);
#12397=VERTEX_POINT('',#60471);
#12398=VERTEX_POINT('',#60475);
#12399=VERTEX_POINT('',#60476);
#12400=VERTEX_POINT('',#60478);
#12401=VERTEX_POINT('',#60480);
#12402=VERTEX_POINT('',#60484);
#12403=VERTEX_POINT('',#60485);
#12404=VERTEX_POINT('',#60487);
#12405=VERTEX_POINT('',#60489);
#12406=VERTEX_POINT('',#60493);
#12407=VERTEX_POINT('',#60494);
#12408=VERTEX_POINT('',#60496);
#12409=VERTEX_POINT('',#60498);
#12410=VERTEX_POINT('',#60502);
#12411=VERTEX_POINT('',#60503);
#12412=VERTEX_POINT('',#60505);
#12413=VERTEX_POINT('',#60507);
#12414=VERTEX_POINT('',#60511);
#12415=VERTEX_POINT('',#60512);
#12416=VERTEX_POINT('',#60514);
#12417=VERTEX_POINT('',#60516);
#12418=VERTEX_POINT('',#60520);
#12419=VERTEX_POINT('',#60521);
#12420=VERTEX_POINT('',#60523);
#12421=VERTEX_POINT('',#60525);
#12422=VERTEX_POINT('',#60529);
#12423=VERTEX_POINT('',#60530);
#12424=VERTEX_POINT('',#60532);
#12425=VERTEX_POINT('',#60534);
#12426=VERTEX_POINT('',#60538);
#12427=VERTEX_POINT('',#60539);
#12428=VERTEX_POINT('',#60541);
#12429=VERTEX_POINT('',#60543);
#12430=VERTEX_POINT('',#60547);
#12431=VERTEX_POINT('',#60548);
#12432=VERTEX_POINT('',#60550);
#12433=VERTEX_POINT('',#60552);
#12434=VERTEX_POINT('',#60556);
#12435=VERTEX_POINT('',#60557);
#12436=VERTEX_POINT('',#60559);
#12437=VERTEX_POINT('',#60561);
#12438=VERTEX_POINT('',#60565);
#12439=VERTEX_POINT('',#60566);
#12440=VERTEX_POINT('',#60568);
#12441=VERTEX_POINT('',#60570);
#12442=VERTEX_POINT('',#60574);
#12443=VERTEX_POINT('',#60575);
#12444=VERTEX_POINT('',#60577);
#12445=VERTEX_POINT('',#60579);
#12446=VERTEX_POINT('',#60583);
#12447=VERTEX_POINT('',#60584);
#12448=VERTEX_POINT('',#60586);
#12449=VERTEX_POINT('',#60588);
#12450=VERTEX_POINT('',#60592);
#12451=VERTEX_POINT('',#60593);
#12452=VERTEX_POINT('',#60597);
#12453=VERTEX_POINT('',#60601);
#12454=VERTEX_POINT('',#60605);
#12455=VERTEX_POINT('',#60609);
#12456=VERTEX_POINT('',#60613);
#12457=VERTEX_POINT('',#60620);
#12458=VERTEX_POINT('',#60624);
#12459=VERTEX_POINT('',#60626);
#12460=VERTEX_POINT('',#60630);
#12461=VERTEX_POINT('',#60631);
#12462=VERTEX_POINT('',#60640);
#12463=VERTEX_POINT('',#60644);
#12464=VERTEX_POINT('',#60646);
#12465=VERTEX_POINT('',#60650);
#12466=VERTEX_POINT('',#60652);
#12467=VERTEX_POINT('',#60656);
#12468=VERTEX_POINT('',#60658);
#12469=VERTEX_POINT('',#60662);
#12470=VERTEX_POINT('',#60664);
#12471=VERTEX_POINT('',#60668);
#12472=VERTEX_POINT('',#60670);
#12473=VERTEX_POINT('',#60674);
#12474=VERTEX_POINT('',#60676);
#12475=VERTEX_POINT('',#60680);
#12476=VERTEX_POINT('',#60682);
#12477=VERTEX_POINT('',#60686);
#12478=VERTEX_POINT('',#60688);
#12479=VERTEX_POINT('',#60692);
#12480=VERTEX_POINT('',#60694);
#12481=VERTEX_POINT('',#60698);
#12482=VERTEX_POINT('',#60700);
#12483=VERTEX_POINT('',#60704);
#12484=VERTEX_POINT('',#60706);
#12485=VERTEX_POINT('',#60710);
#12486=VERTEX_POINT('',#60712);
#12487=VERTEX_POINT('',#60716);
#12488=VERTEX_POINT('',#60718);
#12489=VERTEX_POINT('',#60722);
#12490=VERTEX_POINT('',#60724);
#12491=VERTEX_POINT('',#60728);
#12492=VERTEX_POINT('',#60730);
#12493=VERTEX_POINT('',#60734);
#12494=VERTEX_POINT('',#60736);
#12495=VERTEX_POINT('',#60740);
#12496=VERTEX_POINT('',#60742);
#12497=VERTEX_POINT('',#60746);
#12498=VERTEX_POINT('',#60748);
#12499=VERTEX_POINT('',#60752);
#12500=VERTEX_POINT('',#60754);
#12501=VERTEX_POINT('',#60758);
#12502=VERTEX_POINT('',#60760);
#12503=VERTEX_POINT('',#60764);
#12504=VERTEX_POINT('',#60766);
#12505=VERTEX_POINT('',#60770);
#12506=VERTEX_POINT('',#60772);
#12507=VERTEX_POINT('',#60776);
#12508=VERTEX_POINT('',#60778);
#12509=VERTEX_POINT('',#60782);
#12510=VERTEX_POINT('',#60784);
#12511=VERTEX_POINT('',#60788);
#12512=VERTEX_POINT('',#60790);
#12513=VERTEX_POINT('',#60794);
#12514=VERTEX_POINT('',#60796);
#12515=VERTEX_POINT('',#60800);
#12516=VERTEX_POINT('',#60802);
#12517=VERTEX_POINT('',#60806);
#12518=VERTEX_POINT('',#60808);
#12519=VERTEX_POINT('',#60812);
#12520=VERTEX_POINT('',#60814);
#12521=VERTEX_POINT('',#60818);
#12522=VERTEX_POINT('',#60820);
#12523=VERTEX_POINT('',#60824);
#12524=VERTEX_POINT('',#60826);
#12525=VERTEX_POINT('',#60830);
#12526=VERTEX_POINT('',#60832);
#12527=VERTEX_POINT('',#60836);
#12528=VERTEX_POINT('',#60838);
#12529=VERTEX_POINT('',#60842);
#12530=VERTEX_POINT('',#60844);
#12531=VERTEX_POINT('',#60848);
#12532=VERTEX_POINT('',#60850);
#12533=VERTEX_POINT('',#60854);
#12534=VERTEX_POINT('',#60856);
#12535=VERTEX_POINT('',#60860);
#12536=VERTEX_POINT('',#60862);
#12537=VERTEX_POINT('',#60866);
#12538=VERTEX_POINT('',#60868);
#12539=VERTEX_POINT('',#60872);
#12540=VERTEX_POINT('',#60874);
#12541=VERTEX_POINT('',#60878);
#12542=VERTEX_POINT('',#60880);
#12543=VERTEX_POINT('',#60884);
#12544=VERTEX_POINT('',#60886);
#12545=VERTEX_POINT('',#60890);
#12546=VERTEX_POINT('',#60892);
#12547=VERTEX_POINT('',#60896);
#12548=VERTEX_POINT('',#60898);
#12549=VERTEX_POINT('',#60902);
#12550=VERTEX_POINT('',#60904);
#12551=VERTEX_POINT('',#60908);
#12552=VERTEX_POINT('',#60910);
#12553=VERTEX_POINT('',#60914);
#12554=VERTEX_POINT('',#60916);
#12555=VERTEX_POINT('',#60920);
#12556=VERTEX_POINT('',#60922);
#12557=VERTEX_POINT('',#60926);
#12558=VERTEX_POINT('',#60928);
#12559=VERTEX_POINT('',#60932);
#12560=VERTEX_POINT('',#60934);
#12561=VERTEX_POINT('',#60938);
#12562=VERTEX_POINT('',#60940);
#12563=VERTEX_POINT('',#60944);
#12564=VERTEX_POINT('',#60946);
#12565=VERTEX_POINT('',#60950);
#12566=VERTEX_POINT('',#60952);
#12567=VERTEX_POINT('',#60956);
#12568=VERTEX_POINT('',#60958);
#12569=VERTEX_POINT('',#60962);
#12570=VERTEX_POINT('',#60964);
#12571=VERTEX_POINT('',#60968);
#12572=VERTEX_POINT('',#60970);
#12573=VERTEX_POINT('',#60974);
#12574=VERTEX_POINT('',#60976);
#12575=VERTEX_POINT('',#60980);
#12576=VERTEX_POINT('',#60982);
#12577=VERTEX_POINT('',#60986);
#12578=VERTEX_POINT('',#60988);
#12579=VERTEX_POINT('',#60992);
#12580=VERTEX_POINT('',#60994);
#12581=VERTEX_POINT('',#60998);
#12582=VERTEX_POINT('',#61000);
#12583=VERTEX_POINT('',#61004);
#12584=VERTEX_POINT('',#61006);
#12585=VERTEX_POINT('',#61010);
#12586=VERTEX_POINT('',#61012);
#12587=VERTEX_POINT('',#61016);
#12588=VERTEX_POINT('',#61018);
#12589=VERTEX_POINT('',#61022);
#12590=VERTEX_POINT('',#61024);
#12591=VERTEX_POINT('',#61028);
#12592=VERTEX_POINT('',#61030);
#12593=VERTEX_POINT('',#61034);
#12594=VERTEX_POINT('',#61036);
#12595=VERTEX_POINT('',#61040);
#12596=VERTEX_POINT('',#61042);
#12597=VERTEX_POINT('',#61046);
#12598=VERTEX_POINT('',#61048);
#12599=VERTEX_POINT('',#61052);
#12600=VERTEX_POINT('',#61054);
#12601=VERTEX_POINT('',#61058);
#12602=VERTEX_POINT('',#61060);
#12603=VERTEX_POINT('',#61064);
#12604=VERTEX_POINT('',#61066);
#12605=VERTEX_POINT('',#61070);
#12606=VERTEX_POINT('',#61072);
#12607=VERTEX_POINT('',#61076);
#12608=VERTEX_POINT('',#61078);
#12609=VERTEX_POINT('',#61082);
#12610=VERTEX_POINT('',#61084);
#12611=VERTEX_POINT('',#61088);
#12612=VERTEX_POINT('',#61090);
#12613=VERTEX_POINT('',#61094);
#12614=VERTEX_POINT('',#61096);
#12615=VERTEX_POINT('',#61100);
#12616=VERTEX_POINT('',#61102);
#12617=VERTEX_POINT('',#61106);
#12618=VERTEX_POINT('',#61108);
#12619=VERTEX_POINT('',#61112);
#12620=VERTEX_POINT('',#61114);
#12621=VERTEX_POINT('',#61118);
#12622=VERTEX_POINT('',#61120);
#12623=VERTEX_POINT('',#61124);
#12624=VERTEX_POINT('',#61126);
#12625=VERTEX_POINT('',#61130);
#12626=VERTEX_POINT('',#61132);
#12627=VERTEX_POINT('',#61136);
#12628=VERTEX_POINT('',#61138);
#12629=VERTEX_POINT('',#61142);
#12630=VERTEX_POINT('',#61144);
#12631=VERTEX_POINT('',#61148);
#12632=VERTEX_POINT('',#61150);
#12633=VERTEX_POINT('',#61154);
#12634=VERTEX_POINT('',#61156);
#12635=VERTEX_POINT('',#61160);
#12636=VERTEX_POINT('',#61162);
#12637=VERTEX_POINT('',#61166);
#12638=VERTEX_POINT('',#61168);
#12639=VERTEX_POINT('',#61172);
#12640=VERTEX_POINT('',#61174);
#12641=VERTEX_POINT('',#61178);
#12642=VERTEX_POINT('',#61180);
#12643=VERTEX_POINT('',#61184);
#12644=VERTEX_POINT('',#61189);
#12645=VERTEX_POINT('',#61193);
#12646=VERTEX_POINT('',#61198);
#12647=VERTEX_POINT('',#61202);
#12648=VERTEX_POINT('',#61207);
#12649=VERTEX_POINT('',#61211);
#12650=VERTEX_POINT('',#61216);
#12651=VERTEX_POINT('',#61220);
#12652=VERTEX_POINT('',#61225);
#12653=VERTEX_POINT('',#61229);
#12654=VERTEX_POINT('',#61234);
#12655=VERTEX_POINT('',#61238);
#12656=VERTEX_POINT('',#61243);
#12657=VERTEX_POINT('',#61247);
#12658=VERTEX_POINT('',#61252);
#12659=VERTEX_POINT('',#61256);
#12660=VERTEX_POINT('',#61261);
#12661=VERTEX_POINT('',#61265);
#12662=VERTEX_POINT('',#61270);
#12663=VERTEX_POINT('',#61274);
#12664=VERTEX_POINT('',#61279);
#12665=VERTEX_POINT('',#61283);
#12666=VERTEX_POINT('',#61288);
#12667=VERTEX_POINT('',#61292);
#12668=VERTEX_POINT('',#61297);
#12669=VERTEX_POINT('',#61301);
#12670=VERTEX_POINT('',#61306);
#12671=VERTEX_POINT('',#61310);
#12672=VERTEX_POINT('',#61315);
#12673=VERTEX_POINT('',#61319);
#12674=VERTEX_POINT('',#61321);
#12675=VERTEX_POINT('',#61325);
#12676=VERTEX_POINT('',#61327);
#12677=VERTEX_POINT('',#61331);
#12678=VERTEX_POINT('',#61333);
#12679=VERTEX_POINT('',#61337);
#12680=VERTEX_POINT('',#61339);
#12681=VERTEX_POINT('',#61343);
#12682=VERTEX_POINT('',#61345);
#12683=VERTEX_POINT('',#61349);
#12684=VERTEX_POINT('',#61351);
#12685=VERTEX_POINT('',#61355);
#12686=VERTEX_POINT('',#61357);
#12687=VERTEX_POINT('',#61361);
#12688=VERTEX_POINT('',#61363);
#12689=VERTEX_POINT('',#61367);
#12690=VERTEX_POINT('',#61369);
#12691=VERTEX_POINT('',#61373);
#12692=VERTEX_POINT('',#61375);
#12693=VERTEX_POINT('',#61379);
#12694=VERTEX_POINT('',#61381);
#12695=VERTEX_POINT('',#61385);
#12696=VERTEX_POINT('',#61387);
#12697=VERTEX_POINT('',#61391);
#12698=VERTEX_POINT('',#61393);
#12699=VERTEX_POINT('',#61397);
#12700=VERTEX_POINT('',#61399);
#12701=VERTEX_POINT('',#61403);
#12702=VERTEX_POINT('',#61405);
#12703=VERTEX_POINT('',#61409);
#12704=VERTEX_POINT('',#61411);
#12705=VERTEX_POINT('',#61415);
#12706=VERTEX_POINT('',#61417);
#12707=VERTEX_POINT('',#61421);
#12708=VERTEX_POINT('',#61423);
#12709=VERTEX_POINT('',#61427);
#12710=VERTEX_POINT('',#61429);
#12711=VERTEX_POINT('',#61433);
#12712=VERTEX_POINT('',#61435);
#12713=VERTEX_POINT('',#61439);
#12714=VERTEX_POINT('',#61441);
#12715=VERTEX_POINT('',#61445);
#12716=VERTEX_POINT('',#61447);
#12717=VERTEX_POINT('',#61451);
#12718=VERTEX_POINT('',#61453);
#12719=VERTEX_POINT('',#61457);
#12720=VERTEX_POINT('',#61459);
#12721=VERTEX_POINT('',#61463);
#12722=VERTEX_POINT('',#61465);
#12723=VERTEX_POINT('',#61469);
#12724=VERTEX_POINT('',#61471);
#12725=VERTEX_POINT('',#61475);
#12726=VERTEX_POINT('',#61477);
#12727=VERTEX_POINT('',#61481);
#12728=VERTEX_POINT('',#61483);
#12729=VERTEX_POINT('',#61487);
#12730=VERTEX_POINT('',#61489);
#12731=VERTEX_POINT('',#61493);
#12732=VERTEX_POINT('',#61495);
#12733=VERTEX_POINT('',#61499);
#12734=VERTEX_POINT('',#61501);
#12735=VERTEX_POINT('',#61505);
#12736=VERTEX_POINT('',#61507);
#12737=VERTEX_POINT('',#61511);
#12738=VERTEX_POINT('',#61513);
#12739=VERTEX_POINT('',#61517);
#12740=VERTEX_POINT('',#61519);
#12741=VERTEX_POINT('',#61523);
#12742=VERTEX_POINT('',#61525);
#12743=VERTEX_POINT('',#61529);
#12744=VERTEX_POINT('',#61531);
#12745=VERTEX_POINT('',#61535);
#12746=VERTEX_POINT('',#61537);
#12747=VERTEX_POINT('',#61541);
#12748=VERTEX_POINT('',#61543);
#12749=VERTEX_POINT('',#61547);
#12750=VERTEX_POINT('',#61549);
#12751=VERTEX_POINT('',#61563);
#12752=VERTEX_POINT('',#61564);
#12753=VERTEX_POINT('',#61573);
#12754=VERTEX_POINT('',#61577);
#12755=VERTEX_POINT('',#61579);
#12756=VERTEX_POINT('',#61583);
#12757=VERTEX_POINT('',#61585);
#12758=VERTEX_POINT('',#61589);
#12759=VERTEX_POINT('',#61591);
#12760=VERTEX_POINT('',#61595);
#12761=VERTEX_POINT('',#61597);
#12762=VERTEX_POINT('',#61601);
#12763=VERTEX_POINT('',#61603);
#12764=VERTEX_POINT('',#61607);
#12765=VERTEX_POINT('',#61609);
#12766=VERTEX_POINT('',#61613);
#12767=VERTEX_POINT('',#61615);
#12768=VERTEX_POINT('',#61619);
#12769=VERTEX_POINT('',#61621);
#12770=VERTEX_POINT('',#61625);
#12771=VERTEX_POINT('',#61627);
#12772=VERTEX_POINT('',#61631);
#12773=VERTEX_POINT('',#61633);
#12774=VERTEX_POINT('',#61637);
#12775=VERTEX_POINT('',#61639);
#12776=VERTEX_POINT('',#61643);
#12777=VERTEX_POINT('',#61645);
#12778=VERTEX_POINT('',#61649);
#12779=VERTEX_POINT('',#61651);
#12780=VERTEX_POINT('',#61655);
#12781=VERTEX_POINT('',#61657);
#12782=VERTEX_POINT('',#61661);
#12783=VERTEX_POINT('',#61663);
#12784=VERTEX_POINT('',#61667);
#12785=VERTEX_POINT('',#61669);
#12786=VERTEX_POINT('',#61673);
#12787=VERTEX_POINT('',#61675);
#12788=VERTEX_POINT('',#61679);
#12789=VERTEX_POINT('',#61681);
#12790=VERTEX_POINT('',#61685);
#12791=VERTEX_POINT('',#61687);
#12792=VERTEX_POINT('',#61691);
#12793=VERTEX_POINT('',#61693);
#12794=VERTEX_POINT('',#61697);
#12795=VERTEX_POINT('',#61699);
#12796=VERTEX_POINT('',#61703);
#12797=VERTEX_POINT('',#61705);
#12798=VERTEX_POINT('',#61709);
#12799=VERTEX_POINT('',#61711);
#12800=VERTEX_POINT('',#61715);
#12801=VERTEX_POINT('',#61717);
#12802=VERTEX_POINT('',#61721);
#12803=VERTEX_POINT('',#61723);
#12804=VERTEX_POINT('',#61727);
#12805=VERTEX_POINT('',#61729);
#12806=VERTEX_POINT('',#61733);
#12807=VERTEX_POINT('',#61735);
#12808=VERTEX_POINT('',#61739);
#12809=VERTEX_POINT('',#61741);
#12810=VERTEX_POINT('',#61745);
#12811=VERTEX_POINT('',#61747);
#12812=VERTEX_POINT('',#61751);
#12813=VERTEX_POINT('',#61753);
#12814=VERTEX_POINT('',#61757);
#12815=VERTEX_POINT('',#61759);
#12816=VERTEX_POINT('',#61763);
#12817=VERTEX_POINT('',#61765);
#12818=VERTEX_POINT('',#61769);
#12819=VERTEX_POINT('',#61771);
#12820=VERTEX_POINT('',#61775);
#12821=VERTEX_POINT('',#61777);
#12822=VERTEX_POINT('',#61781);
#12823=VERTEX_POINT('',#61783);
#12824=VERTEX_POINT('',#61787);
#12825=VERTEX_POINT('',#61789);
#12826=VERTEX_POINT('',#61793);
#12827=VERTEX_POINT('',#61795);
#12828=VERTEX_POINT('',#61799);
#12829=VERTEX_POINT('',#61801);
#12830=VERTEX_POINT('',#61805);
#12831=VERTEX_POINT('',#61807);
#12832=VERTEX_POINT('',#61811);
#12833=VERTEX_POINT('',#61813);
#12834=VERTEX_POINT('',#61817);
#12835=VERTEX_POINT('',#61819);
#12836=VERTEX_POINT('',#61823);
#12837=VERTEX_POINT('',#61825);
#12838=VERTEX_POINT('',#61829);
#12839=VERTEX_POINT('',#61831);
#12840=VERTEX_POINT('',#61835);
#12841=VERTEX_POINT('',#61837);
#12842=VERTEX_POINT('',#61841);
#12843=VERTEX_POINT('',#61843);
#12844=VERTEX_POINT('',#61847);
#12845=VERTEX_POINT('',#61849);
#12846=VERTEX_POINT('',#61853);
#12847=VERTEX_POINT('',#61855);
#12848=VERTEX_POINT('',#61859);
#12849=VERTEX_POINT('',#61861);
#12850=VERTEX_POINT('',#61865);
#12851=VERTEX_POINT('',#61867);
#12852=VERTEX_POINT('',#61871);
#12853=VERTEX_POINT('',#61873);
#12854=VERTEX_POINT('',#61877);
#12855=VERTEX_POINT('',#61879);
#12856=VERTEX_POINT('',#61883);
#12857=VERTEX_POINT('',#61885);
#12858=VERTEX_POINT('',#61889);
#12859=VERTEX_POINT('',#61891);
#12860=VERTEX_POINT('',#61895);
#12861=VERTEX_POINT('',#61897);
#12862=VERTEX_POINT('',#61901);
#12863=VERTEX_POINT('',#61903);
#12864=VERTEX_POINT('',#61907);
#12865=VERTEX_POINT('',#61909);
#12866=VERTEX_POINT('',#61913);
#12867=VERTEX_POINT('',#61915);
#12868=VERTEX_POINT('',#61919);
#12869=VERTEX_POINT('',#61921);
#12870=VERTEX_POINT('',#61925);
#12871=VERTEX_POINT('',#61927);
#12872=VERTEX_POINT('',#61931);
#12873=VERTEX_POINT('',#61933);
#12874=VERTEX_POINT('',#61937);
#12875=VERTEX_POINT('',#61939);
#12876=VERTEX_POINT('',#61943);
#12877=VERTEX_POINT('',#61945);
#12878=VERTEX_POINT('',#61949);
#12879=VERTEX_POINT('',#61951);
#12880=VERTEX_POINT('',#61955);
#12881=VERTEX_POINT('',#61957);
#12882=VERTEX_POINT('',#61961);
#12883=VERTEX_POINT('',#61963);
#12884=VERTEX_POINT('',#61967);
#12885=VERTEX_POINT('',#61969);
#12886=VERTEX_POINT('',#61973);
#12887=VERTEX_POINT('',#61975);
#12888=VERTEX_POINT('',#61979);
#12889=VERTEX_POINT('',#61981);
#12890=VERTEX_POINT('',#61985);
#12891=VERTEX_POINT('',#61987);
#12892=VERTEX_POINT('',#61991);
#12893=VERTEX_POINT('',#61993);
#12894=VERTEX_POINT('',#61997);
#12895=VERTEX_POINT('',#61999);
#12896=VERTEX_POINT('',#62003);
#12897=VERTEX_POINT('',#62005);
#12898=VERTEX_POINT('',#62009);
#12899=VERTEX_POINT('',#62011);
#12900=VERTEX_POINT('',#62015);
#12901=VERTEX_POINT('',#62017);
#12902=VERTEX_POINT('',#62021);
#12903=VERTEX_POINT('',#62023);
#12904=VERTEX_POINT('',#62027);
#12905=VERTEX_POINT('',#62029);
#12906=VERTEX_POINT('',#62033);
#12907=VERTEX_POINT('',#62035);
#12908=VERTEX_POINT('',#62039);
#12909=VERTEX_POINT('',#62041);
#12910=VERTEX_POINT('',#62045);
#12911=VERTEX_POINT('',#62047);
#12912=VERTEX_POINT('',#62051);
#12913=VERTEX_POINT('',#62053);
#12914=VERTEX_POINT('',#62057);
#12915=VERTEX_POINT('',#62059);
#12916=VERTEX_POINT('',#62063);
#12917=VERTEX_POINT('',#62065);
#12918=VERTEX_POINT('',#62069);
#12919=VERTEX_POINT('',#62071);
#12920=VERTEX_POINT('',#62075);
#12921=VERTEX_POINT('',#62077);
#12922=VERTEX_POINT('',#62081);
#12923=VERTEX_POINT('',#62083);
#12924=VERTEX_POINT('',#62087);
#12925=VERTEX_POINT('',#62089);
#12926=VERTEX_POINT('',#62093);
#12927=VERTEX_POINT('',#62095);
#12928=VERTEX_POINT('',#62099);
#12929=VERTEX_POINT('',#62101);
#12930=VERTEX_POINT('',#62105);
#12931=VERTEX_POINT('',#62107);
#12932=VERTEX_POINT('',#62111);
#12933=VERTEX_POINT('',#62113);
#12934=VERTEX_POINT('',#62117);
#12935=VERTEX_POINT('',#62119);
#12936=VERTEX_POINT('',#62123);
#12937=VERTEX_POINT('',#62125);
#12938=VERTEX_POINT('',#62129);
#12939=VERTEX_POINT('',#62131);
#12940=VERTEX_POINT('',#62135);
#12941=VERTEX_POINT('',#62137);
#12942=VERTEX_POINT('',#62141);
#12943=VERTEX_POINT('',#62143);
#12944=VERTEX_POINT('',#62147);
#12945=VERTEX_POINT('',#62149);
#12946=VERTEX_POINT('',#62153);
#12947=VERTEX_POINT('',#62155);
#12948=VERTEX_POINT('',#62159);
#12949=VERTEX_POINT('',#62161);
#12950=VERTEX_POINT('',#62165);
#12951=VERTEX_POINT('',#62167);
#12952=VERTEX_POINT('',#62171);
#12953=VERTEX_POINT('',#62173);
#12954=VERTEX_POINT('',#62177);
#12955=VERTEX_POINT('',#62179);
#12956=VERTEX_POINT('',#62183);
#12957=VERTEX_POINT('',#62185);
#12958=VERTEX_POINT('',#62189);
#12959=VERTEX_POINT('',#62191);
#12960=VERTEX_POINT('',#62195);
#12961=VERTEX_POINT('',#62197);
#12962=VERTEX_POINT('',#62201);
#12963=VERTEX_POINT('',#62203);
#12964=VERTEX_POINT('',#62207);
#12965=VERTEX_POINT('',#62209);
#12966=VERTEX_POINT('',#62213);
#12967=VERTEX_POINT('',#62215);
#12968=VERTEX_POINT('',#62219);
#12969=VERTEX_POINT('',#62221);
#12970=VERTEX_POINT('',#62225);
#12971=VERTEX_POINT('',#62227);
#12972=VERTEX_POINT('',#62231);
#12973=VERTEX_POINT('',#62233);
#12974=VERTEX_POINT('',#62237);
#12975=VERTEX_POINT('',#62239);
#12976=VERTEX_POINT('',#62243);
#12977=VERTEX_POINT('',#62245);
#12978=VERTEX_POINT('',#62249);
#12979=VERTEX_POINT('',#62251);
#12980=VERTEX_POINT('',#62255);
#12981=VERTEX_POINT('',#62257);
#12982=VERTEX_POINT('',#62261);
#12983=VERTEX_POINT('',#62263);
#12984=VERTEX_POINT('',#62267);
#12985=VERTEX_POINT('',#62269);
#12986=VERTEX_POINT('',#62273);
#12987=VERTEX_POINT('',#62275);
#12988=VERTEX_POINT('',#62279);
#12989=VERTEX_POINT('',#62281);
#12990=VERTEX_POINT('',#62285);
#12991=VERTEX_POINT('',#62290);
#12992=VERTEX_POINT('',#62294);
#12993=VERTEX_POINT('',#62299);
#12994=VERTEX_POINT('',#62303);
#12995=VERTEX_POINT('',#62308);
#12996=VERTEX_POINT('',#62312);
#12997=VERTEX_POINT('',#62317);
#12998=VERTEX_POINT('',#62321);
#12999=VERTEX_POINT('',#62326);
#13000=VERTEX_POINT('',#62330);
#13001=VERTEX_POINT('',#62335);
#13002=VERTEX_POINT('',#62339);
#13003=VERTEX_POINT('',#62344);
#13004=VERTEX_POINT('',#62348);
#13005=VERTEX_POINT('',#62353);
#13006=VERTEX_POINT('',#62357);
#13007=VERTEX_POINT('',#62362);
#13008=VERTEX_POINT('',#62366);
#13009=VERTEX_POINT('',#62371);
#13010=VERTEX_POINT('',#62375);
#13011=VERTEX_POINT('',#62380);
#13012=VERTEX_POINT('',#62384);
#13013=VERTEX_POINT('',#62389);
#13014=VERTEX_POINT('',#62393);
#13015=VERTEX_POINT('',#62398);
#13016=VERTEX_POINT('',#62402);
#13017=VERTEX_POINT('',#62407);
#13018=VERTEX_POINT('',#62411);
#13019=VERTEX_POINT('',#62416);
#13020=VERTEX_POINT('',#62420);
#13021=VERTEX_POINT('',#62422);
#13022=VERTEX_POINT('',#62426);
#13023=VERTEX_POINT('',#62428);
#13024=VERTEX_POINT('',#62432);
#13025=VERTEX_POINT('',#62434);
#13026=VERTEX_POINT('',#62438);
#13027=VERTEX_POINT('',#62440);
#13028=VERTEX_POINT('',#62444);
#13029=VERTEX_POINT('',#62446);
#13030=VERTEX_POINT('',#62450);
#13031=VERTEX_POINT('',#62452);
#13032=VERTEX_POINT('',#62456);
#13033=VERTEX_POINT('',#62458);
#13034=VERTEX_POINT('',#62462);
#13035=VERTEX_POINT('',#62464);
#13036=VERTEX_POINT('',#62468);
#13037=VERTEX_POINT('',#62470);
#13038=VERTEX_POINT('',#62474);
#13039=VERTEX_POINT('',#62476);
#13040=VERTEX_POINT('',#62480);
#13041=VERTEX_POINT('',#62482);
#13042=VERTEX_POINT('',#62494);
#13043=VERTEX_POINT('',#62496);
#13044=VERTEX_POINT('',#62500);
#13045=VERTEX_POINT('',#62504);
#13046=VERTEX_POINT('',#62508);
#13047=VERTEX_POINT('',#62512);
#13048=VERTEX_POINT('',#62516);
#13049=VERTEX_POINT('',#62518);
#13050=VERTEX_POINT('',#62522);
#13051=VERTEX_POINT('',#62524);
#13052=VERTEX_POINT('',#62528);
#13053=VERTEX_POINT('',#62530);
#13054=VERTEX_POINT('',#62534);
#13055=VERTEX_POINT('',#62536);
#13056=VERTEX_POINT('',#62540);
#13057=VERTEX_POINT('',#62542);
#13058=VERTEX_POINT('',#62546);
#13059=VERTEX_POINT('',#62548);
#13060=VERTEX_POINT('',#62552);
#13061=VERTEX_POINT('',#62554);
#13062=VERTEX_POINT('',#62558);
#13063=VERTEX_POINT('',#62560);
#13064=VERTEX_POINT('',#62564);
#13065=VERTEX_POINT('',#62566);
#13066=VERTEX_POINT('',#62570);
#13067=VERTEX_POINT('',#62572);
#13068=VERTEX_POINT('',#62576);
#13069=VERTEX_POINT('',#62578);
#13070=VERTEX_POINT('',#62582);
#13071=VERTEX_POINT('',#62584);
#13072=VERTEX_POINT('',#62588);
#13073=VERTEX_POINT('',#62590);
#13074=VERTEX_POINT('',#62594);
#13075=VERTEX_POINT('',#62596);
#13076=VERTEX_POINT('',#62600);
#13077=VERTEX_POINT('',#62602);
#13078=VERTEX_POINT('',#62606);
#13079=VERTEX_POINT('',#62608);
#13080=VERTEX_POINT('',#62612);
#13081=VERTEX_POINT('',#62614);
#13082=VERTEX_POINT('',#62618);
#13083=VERTEX_POINT('',#62620);
#13084=VERTEX_POINT('',#62624);
#13085=VERTEX_POINT('',#62626);
#13086=VERTEX_POINT('',#62630);
#13087=VERTEX_POINT('',#62632);
#13088=VERTEX_POINT('',#62636);
#13089=VERTEX_POINT('',#62638);
#13090=VERTEX_POINT('',#62642);
#13091=VERTEX_POINT('',#62644);
#13092=VERTEX_POINT('',#62648);
#13093=VERTEX_POINT('',#62650);
#13094=VERTEX_POINT('',#62654);
#13095=VERTEX_POINT('',#62656);
#13096=VERTEX_POINT('',#62660);
#13097=VERTEX_POINT('',#62662);
#13098=VERTEX_POINT('',#62666);
#13099=VERTEX_POINT('',#62668);
#13100=VERTEX_POINT('',#62672);
#13101=VERTEX_POINT('',#62674);
#13102=VERTEX_POINT('',#62678);
#13103=VERTEX_POINT('',#62680);
#13104=VERTEX_POINT('',#62684);
#13105=VERTEX_POINT('',#62686);
#13106=VERTEX_POINT('',#62690);
#13107=VERTEX_POINT('',#62692);
#13108=VERTEX_POINT('',#62696);
#13109=VERTEX_POINT('',#62698);
#13110=VERTEX_POINT('',#62702);
#13111=VERTEX_POINT('',#62704);
#13112=VERTEX_POINT('',#62708);
#13113=VERTEX_POINT('',#62710);
#13114=VERTEX_POINT('',#62714);
#13115=VERTEX_POINT('',#62716);
#13116=VERTEX_POINT('',#62720);
#13117=VERTEX_POINT('',#62722);
#13118=VERTEX_POINT('',#62726);
#13119=VERTEX_POINT('',#62728);
#13120=VERTEX_POINT('',#62732);
#13121=VERTEX_POINT('',#62734);
#13122=VERTEX_POINT('',#62738);
#13123=VERTEX_POINT('',#62740);
#13124=VERTEX_POINT('',#62744);
#13125=VERTEX_POINT('',#62746);
#13126=VERTEX_POINT('',#62750);
#13127=VERTEX_POINT('',#62752);
#13128=VERTEX_POINT('',#62756);
#13129=VERTEX_POINT('',#62758);
#13130=VERTEX_POINT('',#62762);
#13131=VERTEX_POINT('',#62764);
#13132=VERTEX_POINT('',#62768);
#13133=VERTEX_POINT('',#62770);
#13134=VERTEX_POINT('',#62774);
#13135=VERTEX_POINT('',#62776);
#13136=VERTEX_POINT('',#62780);
#13137=VERTEX_POINT('',#62782);
#13138=VERTEX_POINT('',#62786);
#13139=VERTEX_POINT('',#62788);
#13140=VERTEX_POINT('',#62792);
#13141=VERTEX_POINT('',#62794);
#13142=VERTEX_POINT('',#62798);
#13143=VERTEX_POINT('',#62800);
#13144=VERTEX_POINT('',#62804);
#13145=VERTEX_POINT('',#62806);
#13146=VERTEX_POINT('',#62810);
#13147=VERTEX_POINT('',#62812);
#13148=VERTEX_POINT('',#62816);
#13149=VERTEX_POINT('',#62818);
#13150=VERTEX_POINT('',#62822);
#13151=VERTEX_POINT('',#62824);
#13152=VERTEX_POINT('',#62828);
#13153=VERTEX_POINT('',#62830);
#13154=VERTEX_POINT('',#62834);
#13155=VERTEX_POINT('',#62836);
#13156=VERTEX_POINT('',#62840);
#13157=VERTEX_POINT('',#62842);
#13158=VERTEX_POINT('',#62846);
#13159=VERTEX_POINT('',#62848);
#13160=VERTEX_POINT('',#62852);
#13161=VERTEX_POINT('',#62854);
#13162=VERTEX_POINT('',#62858);
#13163=VERTEX_POINT('',#62860);
#13164=VERTEX_POINT('',#62864);
#13165=VERTEX_POINT('',#62866);
#13166=VERTEX_POINT('',#62870);
#13167=VERTEX_POINT('',#62872);
#13168=VERTEX_POINT('',#62876);
#13169=VERTEX_POINT('',#62878);
#13170=VERTEX_POINT('',#62882);
#13171=VERTEX_POINT('',#62884);
#13172=VERTEX_POINT('',#62888);
#13173=VERTEX_POINT('',#62890);
#13174=VERTEX_POINT('',#62894);
#13175=VERTEX_POINT('',#62896);
#13176=VERTEX_POINT('',#62900);
#13177=VERTEX_POINT('',#62902);
#13178=VERTEX_POINT('',#62906);
#13179=VERTEX_POINT('',#62908);
#13180=VERTEX_POINT('',#62912);
#13181=VERTEX_POINT('',#62914);
#13182=VERTEX_POINT('',#62918);
#13183=VERTEX_POINT('',#62920);
#13184=VERTEX_POINT('',#62924);
#13185=VERTEX_POINT('',#62926);
#13186=VERTEX_POINT('',#62930);
#13187=VERTEX_POINT('',#62932);
#13188=VERTEX_POINT('',#62936);
#13189=VERTEX_POINT('',#62938);
#13190=VERTEX_POINT('',#62942);
#13191=VERTEX_POINT('',#62944);
#13192=VERTEX_POINT('',#62948);
#13193=VERTEX_POINT('',#62950);
#13194=VERTEX_POINT('',#62954);
#13195=VERTEX_POINT('',#62956);
#13196=VERTEX_POINT('',#62960);
#13197=VERTEX_POINT('',#62962);
#13198=VERTEX_POINT('',#62966);
#13199=VERTEX_POINT('',#62968);
#13200=VERTEX_POINT('',#62972);
#13201=VERTEX_POINT('',#62974);
#13202=VERTEX_POINT('',#62978);
#13203=VERTEX_POINT('',#62980);
#13204=VERTEX_POINT('',#62984);
#13205=VERTEX_POINT('',#62986);
#13206=VERTEX_POINT('',#62990);
#13207=VERTEX_POINT('',#62992);
#13208=VERTEX_POINT('',#62996);
#13209=VERTEX_POINT('',#62998);
#13210=VERTEX_POINT('',#63002);
#13211=VERTEX_POINT('',#63004);
#13212=VERTEX_POINT('',#63008);
#13213=VERTEX_POINT('',#63010);
#13214=VERTEX_POINT('',#63014);
#13215=VERTEX_POINT('',#63016);
#13216=VERTEX_POINT('',#63020);
#13217=VERTEX_POINT('',#63022);
#13218=VERTEX_POINT('',#63026);
#13219=VERTEX_POINT('',#63028);
#13220=VERTEX_POINT('',#63032);
#13221=VERTEX_POINT('',#63034);
#13222=VERTEX_POINT('',#63038);
#13223=VERTEX_POINT('',#63040);
#13224=VERTEX_POINT('',#63044);
#13225=VERTEX_POINT('',#63046);
#13226=VERTEX_POINT('',#63050);
#13227=VERTEX_POINT('',#63052);
#13228=VERTEX_POINT('',#63056);
#13229=VERTEX_POINT('',#63058);
#13230=VERTEX_POINT('',#63062);
#13231=VERTEX_POINT('',#63064);
#13232=VERTEX_POINT('',#63068);
#13233=VERTEX_POINT('',#63070);
#13234=VERTEX_POINT('',#63074);
#13235=VERTEX_POINT('',#63076);
#13236=VERTEX_POINT('',#63080);
#13237=VERTEX_POINT('',#63082);
#13238=VERTEX_POINT('',#63086);
#13239=VERTEX_POINT('',#63088);
#13240=VERTEX_POINT('',#63092);
#13241=VERTEX_POINT('',#63094);
#13242=VERTEX_POINT('',#63098);
#13243=VERTEX_POINT('',#63100);
#13244=VERTEX_POINT('',#63104);
#13245=VERTEX_POINT('',#63106);
#13246=VERTEX_POINT('',#63110);
#13247=VERTEX_POINT('',#63112);
#13248=VERTEX_POINT('',#63116);
#13249=VERTEX_POINT('',#63118);
#13250=VERTEX_POINT('',#63122);
#13251=VERTEX_POINT('',#63124);
#13252=VERTEX_POINT('',#63128);
#13253=VERTEX_POINT('',#63130);
#13254=VERTEX_POINT('',#63134);
#13255=VERTEX_POINT('',#63136);
#13256=VERTEX_POINT('',#63140);
#13257=VERTEX_POINT('',#63142);
#13258=VERTEX_POINT('',#63146);
#13259=VERTEX_POINT('',#63148);
#13260=VERTEX_POINT('',#63152);
#13261=VERTEX_POINT('',#63154);
#13262=VERTEX_POINT('',#63158);
#13263=VERTEX_POINT('',#63160);
#13264=VERTEX_POINT('',#63164);
#13265=VERTEX_POINT('',#63166);
#13266=VERTEX_POINT('',#63170);
#13267=VERTEX_POINT('',#63172);
#13268=VERTEX_POINT('',#63176);
#13269=VERTEX_POINT('',#63178);
#13270=VERTEX_POINT('',#63182);
#13271=VERTEX_POINT('',#63184);
#13272=VERTEX_POINT('',#63188);
#13273=VERTEX_POINT('',#63190);
#13274=VERTEX_POINT('',#63194);
#13275=VERTEX_POINT('',#63196);
#13276=VERTEX_POINT('',#63200);
#13277=VERTEX_POINT('',#63202);
#13278=VERTEX_POINT('',#63206);
#13279=VERTEX_POINT('',#63208);
#13280=VERTEX_POINT('',#63212);
#13281=VERTEX_POINT('',#63214);
#13282=VERTEX_POINT('',#63218);
#13283=VERTEX_POINT('',#63220);
#13284=VERTEX_POINT('',#63224);
#13285=VERTEX_POINT('',#63226);
#13286=VERTEX_POINT('',#63230);
#13287=VERTEX_POINT('',#63232);
#13288=VERTEX_POINT('',#63236);
#13289=VERTEX_POINT('',#63238);
#13290=VERTEX_POINT('',#63242);
#13291=VERTEX_POINT('',#63244);
#13292=VERTEX_POINT('',#63248);
#13293=VERTEX_POINT('',#63250);
#13294=VERTEX_POINT('',#63254);
#13295=VERTEX_POINT('',#63256);
#13296=VERTEX_POINT('',#63260);
#13297=VERTEX_POINT('',#63262);
#13298=VERTEX_POINT('',#63266);
#13299=VERTEX_POINT('',#63268);
#13300=VERTEX_POINT('',#63272);
#13301=VERTEX_POINT('',#63274);
#13302=VERTEX_POINT('',#63278);
#13303=VERTEX_POINT('',#63280);
#13304=VERTEX_POINT('',#63284);
#13305=VERTEX_POINT('',#63286);
#13306=VERTEX_POINT('',#63290);
#13307=VERTEX_POINT('',#63292);
#13308=VERTEX_POINT('',#63296);
#13309=VERTEX_POINT('',#63298);
#13310=VERTEX_POINT('',#63302);
#13311=VERTEX_POINT('',#63304);
#13312=VERTEX_POINT('',#63308);
#13313=VERTEX_POINT('',#63310);
#13314=VERTEX_POINT('',#63314);
#13315=VERTEX_POINT('',#63316);
#13316=VERTEX_POINT('',#63320);
#13317=VERTEX_POINT('',#63322);
#13318=VERTEX_POINT('',#63326);
#13319=VERTEX_POINT('',#63328);
#13320=VERTEX_POINT('',#63332);
#13321=VERTEX_POINT('',#63334);
#13322=VERTEX_POINT('',#63338);
#13323=VERTEX_POINT('',#63340);
#13324=VERTEX_POINT('',#63344);
#13325=VERTEX_POINT('',#63346);
#13326=VERTEX_POINT('',#63350);
#13327=VERTEX_POINT('',#63352);
#13328=VERTEX_POINT('',#63356);
#13329=VERTEX_POINT('',#63358);
#13330=VERTEX_POINT('',#63362);
#13331=VERTEX_POINT('',#63364);
#13332=VERTEX_POINT('',#63368);
#13333=VERTEX_POINT('',#63370);
#13334=VERTEX_POINT('',#63374);
#13335=VERTEX_POINT('',#63376);
#13336=VERTEX_POINT('',#63380);
#13337=VERTEX_POINT('',#63382);
#13338=VERTEX_POINT('',#63386);
#13339=VERTEX_POINT('',#63388);
#13340=VERTEX_POINT('',#63392);
#13341=VERTEX_POINT('',#63394);
#13342=VERTEX_POINT('',#63398);
#13343=VERTEX_POINT('',#63400);
#13344=VERTEX_POINT('',#63404);
#13345=VERTEX_POINT('',#63406);
#13346=VERTEX_POINT('',#63410);
#13347=VERTEX_POINT('',#63412);
#13348=VERTEX_POINT('',#63416);
#13349=VERTEX_POINT('',#63418);
#13350=VERTEX_POINT('',#63422);
#13351=VERTEX_POINT('',#63424);
#13352=VERTEX_POINT('',#63428);
#13353=VERTEX_POINT('',#63430);
#13354=VERTEX_POINT('',#63434);
#13355=VERTEX_POINT('',#63436);
#13356=VERTEX_POINT('',#63440);
#13357=VERTEX_POINT('',#63442);
#13358=VERTEX_POINT('',#63446);
#13359=VERTEX_POINT('',#63448);
#13360=VERTEX_POINT('',#63452);
#13361=VERTEX_POINT('',#63454);
#13362=VERTEX_POINT('',#63458);
#13363=VERTEX_POINT('',#63460);
#13364=VERTEX_POINT('',#63703);
#13365=VERTEX_POINT('',#63705);
#13366=VERTEX_POINT('',#63709);
#13367=VERTEX_POINT('',#63711);
#13368=VERTEX_POINT('',#63719);
#13369=VERTEX_POINT('',#63720);
#13370=VERTEX_POINT('',#63722);
#13371=VERTEX_POINT('',#63724);
#13372=VERTEX_POINT('',#63726);
#13373=VERTEX_POINT('',#63728);
#13374=VERTEX_POINT('',#65622);
#13375=VERTEX_POINT('',#65623);
#13376=VERTEX_POINT('',#65625);
#13377=VERTEX_POINT('',#65662);
#13378=VERTEX_POINT('',#65665);
#13379=VERTEX_POINT('',#65702);
#13380=VERTEX_POINT('',#65703);
#13381=VERTEX_POINT('',#65778);
#13382=VERTEX_POINT('',#65779);
#13383=VERTEX_POINT('',#65856);
#13384=VERTEX_POINT('',#65857);
#13385=VERTEX_POINT('',#65932);
#13386=VERTEX_POINT('',#65933);
#13387=VERTEX_POINT('',#66008);
#13388=VERTEX_POINT('',#66009);
#13389=VERTEX_POINT('',#66084);
#13390=VERTEX_POINT('',#66085);
#13391=VERTEX_POINT('',#66160);
#13392=VERTEX_POINT('',#66161);
#13393=VERTEX_POINT('',#66238);
#13394=VERTEX_POINT('',#66239);
#13395=VERTEX_POINT('',#66316);
#13396=VERTEX_POINT('',#66317);
#13397=VERTEX_POINT('',#66392);
#13398=VERTEX_POINT('',#66393);
#13399=VERTEX_POINT('',#66468);
#13400=VERTEX_POINT('',#66469);
#13401=VERTEX_POINT('',#66544);
#13402=VERTEX_POINT('',#66545);
#13403=VERTEX_POINT('',#66620);
#13404=VERTEX_POINT('',#66621);
#13405=VERTEX_POINT('',#66698);
#13406=VERTEX_POINT('',#66699);
#13407=VERTEX_POINT('',#66774);
#13408=VERTEX_POINT('',#66775);
#13409=VERTEX_POINT('',#66852);
#13410=VERTEX_POINT('',#66853);
#13411=VERTEX_POINT('',#66928);
#13412=VERTEX_POINT('',#66929);
#13413=VERTEX_POINT('',#67004);
#13414=VERTEX_POINT('',#67005);
#13415=VERTEX_POINT('',#67080);
#13416=VERTEX_POINT('',#67081);
#13417=VERTEX_POINT('',#67156);
#13418=VERTEX_POINT('',#67157);
#13419=VERTEX_POINT('',#67234);
#13420=VERTEX_POINT('',#67235);
#13421=VERTEX_POINT('',#67312);
#13422=VERTEX_POINT('',#67313);
#13423=VERTEX_POINT('',#67388);
#13424=VERTEX_POINT('',#67389);
#13425=VERTEX_POINT('',#67464);
#13426=VERTEX_POINT('',#67465);
#13427=VERTEX_POINT('',#67540);
#13428=VERTEX_POINT('',#67541);
#13429=VERTEX_POINT('',#67616);
#13430=VERTEX_POINT('',#67617);
#13431=VERTEX_POINT('',#67694);
#13432=VERTEX_POINT('',#67695);
#13433=VERTEX_POINT('',#67770);
#13434=VERTEX_POINT('',#67771);
#13435=VERTEX_POINT('',#67773);
#13436=VERTEX_POINT('',#67796);
#13437=VERTEX_POINT('',#67798);
#13438=VERTEX_POINT('',#67809);
#13439=VERTEX_POINT('',#67810);
#13440=VERTEX_POINT('',#67885);
#13441=VERTEX_POINT('',#67886);
#13442=VERTEX_POINT('',#67961);
#13443=VERTEX_POINT('',#67962);
#13444=VERTEX_POINT('',#68039);
#13445=VERTEX_POINT('',#68040);
#13446=VERTEX_POINT('',#68115);
#13447=VERTEX_POINT('',#68116);
#13448=VERTEX_POINT('',#68193);
#13449=VERTEX_POINT('',#68194);
#13450=VERTEX_POINT('',#68269);
#13451=VERTEX_POINT('',#68270);
#13452=VERTEX_POINT('',#68345);
#13453=VERTEX_POINT('',#68346);
#13454=VERTEX_POINT('',#68421);
#13455=VERTEX_POINT('',#68422);
#13456=VERTEX_POINT('',#68497);
#13457=VERTEX_POINT('',#68498);
#13458=VERTEX_POINT('',#68575);
#13459=VERTEX_POINT('',#68576);
#13460=VERTEX_POINT('',#68651);
#13461=VERTEX_POINT('',#68652);
#13462=VERTEX_POINT('',#68729);
#13463=VERTEX_POINT('',#68730);
#13464=VERTEX_POINT('',#68805);
#13465=VERTEX_POINT('',#68806);
#13466=VERTEX_POINT('',#68881);
#13467=VERTEX_POINT('',#68882);
#13468=VERTEX_POINT('',#68957);
#13469=VERTEX_POINT('',#68958);
#13470=VERTEX_POINT('',#69033);
#13471=VERTEX_POINT('',#69034);
#13472=VERTEX_POINT('',#69109);
#13473=VERTEX_POINT('',#69110);
#13474=VERTEX_POINT('',#69187);
#13475=VERTEX_POINT('',#69188);
#13476=VERTEX_POINT('',#69263);
#13477=VERTEX_POINT('',#69264);
#13478=VERTEX_POINT('',#69341);
#13479=VERTEX_POINT('',#69342);
#13480=VERTEX_POINT('',#69417);
#13481=VERTEX_POINT('',#69418);
#13482=VERTEX_POINT('',#69493);
#13483=VERTEX_POINT('',#69494);
#13484=VERTEX_POINT('',#69569);
#13485=VERTEX_POINT('',#69570);
#13486=VERTEX_POINT('',#69645);
#13487=VERTEX_POINT('',#69646);
#13488=VERTEX_POINT('',#69723);
#13489=VERTEX_POINT('',#69724);
#13490=VERTEX_POINT('',#69799);
#13491=VERTEX_POINT('',#69800);
#13492=VERTEX_POINT('',#69877);
#13493=VERTEX_POINT('',#69878);
#13494=VERTEX_POINT('',#69953);
#13495=VERTEX_POINT('',#69954);
#13496=VERTEX_POINT('',#70029);
#13497=VERTEX_POINT('',#70041);
#13498=VERTEX_POINT('',#70054);
#13499=VERTEX_POINT('',#70146);
#13500=VERTEX_POINT('',#70147);
#13501=VERTEX_POINT('',#70149);
#13502=VERTEX_POINT('',#70151);
#13503=VERTEX_POINT('',#70155);
#13504=VERTEX_POINT('',#70156);
#13505=VERTEX_POINT('',#70158);
#13506=VERTEX_POINT('',#70160);
#13507=VERTEX_POINT('',#70164);
#13508=VERTEX_POINT('',#70165);
#13509=VERTEX_POINT('',#70167);
#13510=VERTEX_POINT('',#70169);
#13511=VERTEX_POINT('',#70173);
#13512=VERTEX_POINT('',#70174);
#13513=VERTEX_POINT('',#70176);
#13514=VERTEX_POINT('',#70178);
#13515=VERTEX_POINT('',#70182);
#13516=VERTEX_POINT('',#70183);
#13517=VERTEX_POINT('',#70185);
#13518=VERTEX_POINT('',#70187);
#13519=VERTEX_POINT('',#70191);
#13520=VERTEX_POINT('',#70192);
#13521=VERTEX_POINT('',#70194);
#13522=VERTEX_POINT('',#70196);
#13523=VERTEX_POINT('',#70200);
#13524=VERTEX_POINT('',#70201);
#13525=VERTEX_POINT('',#70203);
#13526=VERTEX_POINT('',#70205);
#13527=VERTEX_POINT('',#70209);
#13528=VERTEX_POINT('',#70210);
#13529=VERTEX_POINT('',#70212);
#13530=VERTEX_POINT('',#70214);
#13531=VERTEX_POINT('',#70218);
#13532=VERTEX_POINT('',#70219);
#13533=VERTEX_POINT('',#70221);
#13534=VERTEX_POINT('',#70223);
#13535=VERTEX_POINT('',#70227);
#13536=VERTEX_POINT('',#70228);
#13537=VERTEX_POINT('',#70230);
#13538=VERTEX_POINT('',#70232);
#13539=VERTEX_POINT('',#70236);
#13540=VERTEX_POINT('',#70237);
#13541=VERTEX_POINT('',#70239);
#13542=VERTEX_POINT('',#70241);
#13543=VERTEX_POINT('',#70245);
#13544=VERTEX_POINT('',#70246);
#13545=VERTEX_POINT('',#70248);
#13546=VERTEX_POINT('',#70250);
#13547=VERTEX_POINT('',#70254);
#13548=VERTEX_POINT('',#70255);
#13549=VERTEX_POINT('',#70257);
#13550=VERTEX_POINT('',#70259);
#13551=VERTEX_POINT('',#70263);
#13552=VERTEX_POINT('',#70264);
#13553=VERTEX_POINT('',#70266);
#13554=VERTEX_POINT('',#70268);
#13555=VERTEX_POINT('',#70272);
#13556=VERTEX_POINT('',#70273);
#13557=VERTEX_POINT('',#70275);
#13558=VERTEX_POINT('',#70277);
#13559=VERTEX_POINT('',#70281);
#13560=VERTEX_POINT('',#70282);
#13561=VERTEX_POINT('',#70286);
#13562=VERTEX_POINT('',#70290);
#13563=VERTEX_POINT('',#70294);
#13564=VERTEX_POINT('',#70298);
#13565=VERTEX_POINT('',#70302);
#13566=VERTEX_POINT('',#70309);
#13567=VERTEX_POINT('',#70313);
#13568=VERTEX_POINT('',#70315);
#13569=VERTEX_POINT('',#70319);
#13570=VERTEX_POINT('',#70320);
#13571=VERTEX_POINT('',#70329);
#13572=VERTEX_POINT('',#70333);
#13573=VERTEX_POINT('',#70335);
#13574=VERTEX_POINT('',#70339);
#13575=VERTEX_POINT('',#70341);
#13576=VERTEX_POINT('',#70345);
#13577=VERTEX_POINT('',#70347);
#13578=VERTEX_POINT('',#70351);
#13579=VERTEX_POINT('',#70353);
#13580=VERTEX_POINT('',#70357);
#13581=VERTEX_POINT('',#70359);
#13582=VERTEX_POINT('',#70363);
#13583=VERTEX_POINT('',#70365);
#13584=VERTEX_POINT('',#70369);
#13585=VERTEX_POINT('',#70371);
#13586=VERTEX_POINT('',#70375);
#13587=VERTEX_POINT('',#70377);
#13588=VERTEX_POINT('',#70381);
#13589=VERTEX_POINT('',#70383);
#13590=VERTEX_POINT('',#70387);
#13591=VERTEX_POINT('',#70389);
#13592=VERTEX_POINT('',#70393);
#13593=VERTEX_POINT('',#70395);
#13594=VERTEX_POINT('',#70399);
#13595=VERTEX_POINT('',#70401);
#13596=VERTEX_POINT('',#70405);
#13597=VERTEX_POINT('',#70407);
#13598=VERTEX_POINT('',#70411);
#13599=VERTEX_POINT('',#70413);
#13600=VERTEX_POINT('',#70417);
#13601=VERTEX_POINT('',#70419);
#13602=VERTEX_POINT('',#70423);
#13603=VERTEX_POINT('',#70425);
#13604=VERTEX_POINT('',#70429);
#13605=VERTEX_POINT('',#70431);
#13606=VERTEX_POINT('',#70435);
#13607=VERTEX_POINT('',#70437);
#13608=VERTEX_POINT('',#70441);
#13609=VERTEX_POINT('',#70443);
#13610=VERTEX_POINT('',#70447);
#13611=VERTEX_POINT('',#70449);
#13612=VERTEX_POINT('',#70453);
#13613=VERTEX_POINT('',#70455);
#13614=VERTEX_POINT('',#70459);
#13615=VERTEX_POINT('',#70461);
#13616=VERTEX_POINT('',#70465);
#13617=VERTEX_POINT('',#70467);
#13618=VERTEX_POINT('',#70471);
#13619=VERTEX_POINT('',#70473);
#13620=VERTEX_POINT('',#70477);
#13621=VERTEX_POINT('',#70479);
#13622=VERTEX_POINT('',#70483);
#13623=VERTEX_POINT('',#70485);
#13624=VERTEX_POINT('',#70489);
#13625=VERTEX_POINT('',#70491);
#13626=VERTEX_POINT('',#70495);
#13627=VERTEX_POINT('',#70497);
#13628=VERTEX_POINT('',#70501);
#13629=VERTEX_POINT('',#70503);
#13630=VERTEX_POINT('',#70507);
#13631=VERTEX_POINT('',#70509);
#13632=VERTEX_POINT('',#70513);
#13633=VERTEX_POINT('',#70515);
#13634=VERTEX_POINT('',#70519);
#13635=VERTEX_POINT('',#70521);
#13636=VERTEX_POINT('',#70525);
#13637=VERTEX_POINT('',#70527);
#13638=VERTEX_POINT('',#70531);
#13639=VERTEX_POINT('',#70533);
#13640=VERTEX_POINT('',#70537);
#13641=VERTEX_POINT('',#70539);
#13642=VERTEX_POINT('',#70543);
#13643=VERTEX_POINT('',#70545);
#13644=VERTEX_POINT('',#70549);
#13645=VERTEX_POINT('',#70551);
#13646=VERTEX_POINT('',#70555);
#13647=VERTEX_POINT('',#70557);
#13648=VERTEX_POINT('',#70561);
#13649=VERTEX_POINT('',#70563);
#13650=VERTEX_POINT('',#70567);
#13651=VERTEX_POINT('',#70569);
#13652=VERTEX_POINT('',#70573);
#13653=VERTEX_POINT('',#70575);
#13654=VERTEX_POINT('',#70579);
#13655=VERTEX_POINT('',#70581);
#13656=VERTEX_POINT('',#70585);
#13657=VERTEX_POINT('',#70587);
#13658=VERTEX_POINT('',#70591);
#13659=VERTEX_POINT('',#70593);
#13660=VERTEX_POINT('',#70597);
#13661=VERTEX_POINT('',#70599);
#13662=VERTEX_POINT('',#70603);
#13663=VERTEX_POINT('',#70605);
#13664=VERTEX_POINT('',#70609);
#13665=VERTEX_POINT('',#70611);
#13666=VERTEX_POINT('',#70615);
#13667=VERTEX_POINT('',#70617);
#13668=VERTEX_POINT('',#70621);
#13669=VERTEX_POINT('',#70623);
#13670=VERTEX_POINT('',#70627);
#13671=VERTEX_POINT('',#70629);
#13672=VERTEX_POINT('',#70633);
#13673=VERTEX_POINT('',#70635);
#13674=VERTEX_POINT('',#70639);
#13675=VERTEX_POINT('',#70641);
#13676=VERTEX_POINT('',#70645);
#13677=VERTEX_POINT('',#70647);
#13678=VERTEX_POINT('',#70651);
#13679=VERTEX_POINT('',#70653);
#13680=VERTEX_POINT('',#70657);
#13681=VERTEX_POINT('',#70659);
#13682=VERTEX_POINT('',#70663);
#13683=VERTEX_POINT('',#70665);
#13684=VERTEX_POINT('',#70669);
#13685=VERTEX_POINT('',#70671);
#13686=VERTEX_POINT('',#70675);
#13687=VERTEX_POINT('',#70677);
#13688=VERTEX_POINT('',#70681);
#13689=VERTEX_POINT('',#70683);
#13690=VERTEX_POINT('',#70687);
#13691=VERTEX_POINT('',#70689);
#13692=VERTEX_POINT('',#70693);
#13693=VERTEX_POINT('',#70695);
#13694=VERTEX_POINT('',#70699);
#13695=VERTEX_POINT('',#70701);
#13696=VERTEX_POINT('',#70705);
#13697=VERTEX_POINT('',#70707);
#13698=VERTEX_POINT('',#70711);
#13699=VERTEX_POINT('',#70713);
#13700=VERTEX_POINT('',#70717);
#13701=VERTEX_POINT('',#70719);
#13702=VERTEX_POINT('',#70723);
#13703=VERTEX_POINT('',#70725);
#13704=VERTEX_POINT('',#70729);
#13705=VERTEX_POINT('',#70731);
#13706=VERTEX_POINT('',#70735);
#13707=VERTEX_POINT('',#70737);
#13708=VERTEX_POINT('',#70741);
#13709=VERTEX_POINT('',#70743);
#13710=VERTEX_POINT('',#70747);
#13711=VERTEX_POINT('',#70749);
#13712=VERTEX_POINT('',#70753);
#13713=VERTEX_POINT('',#70755);
#13714=VERTEX_POINT('',#70759);
#13715=VERTEX_POINT('',#70761);
#13716=VERTEX_POINT('',#70765);
#13717=VERTEX_POINT('',#70767);
#13718=VERTEX_POINT('',#70771);
#13719=VERTEX_POINT('',#70773);
#13720=VERTEX_POINT('',#70777);
#13721=VERTEX_POINT('',#70779);
#13722=VERTEX_POINT('',#70783);
#13723=VERTEX_POINT('',#70785);
#13724=VERTEX_POINT('',#70789);
#13725=VERTEX_POINT('',#70791);
#13726=VERTEX_POINT('',#70795);
#13727=VERTEX_POINT('',#70797);
#13728=VERTEX_POINT('',#70801);
#13729=VERTEX_POINT('',#70803);
#13730=VERTEX_POINT('',#70807);
#13731=VERTEX_POINT('',#70809);
#13732=VERTEX_POINT('',#70813);
#13733=VERTEX_POINT('',#70815);
#13734=VERTEX_POINT('',#70819);
#13735=VERTEX_POINT('',#70821);
#13736=VERTEX_POINT('',#70825);
#13737=VERTEX_POINT('',#70827);
#13738=VERTEX_POINT('',#70831);
#13739=VERTEX_POINT('',#70833);
#13740=VERTEX_POINT('',#70837);
#13741=VERTEX_POINT('',#70839);
#13742=VERTEX_POINT('',#70843);
#13743=VERTEX_POINT('',#70845);
#13744=VERTEX_POINT('',#70849);
#13745=VERTEX_POINT('',#70851);
#13746=VERTEX_POINT('',#70855);
#13747=VERTEX_POINT('',#70857);
#13748=VERTEX_POINT('',#70861);
#13749=VERTEX_POINT('',#70863);
#13750=VERTEX_POINT('',#70867);
#13751=VERTEX_POINT('',#70869);
#13752=VERTEX_POINT('',#70873);
#13753=VERTEX_POINT('',#70878);
#13754=VERTEX_POINT('',#70882);
#13755=VERTEX_POINT('',#70887);
#13756=VERTEX_POINT('',#70891);
#13757=VERTEX_POINT('',#70896);
#13758=VERTEX_POINT('',#70900);
#13759=VERTEX_POINT('',#70905);
#13760=VERTEX_POINT('',#70909);
#13761=VERTEX_POINT('',#70914);
#13762=VERTEX_POINT('',#70918);
#13763=VERTEX_POINT('',#70923);
#13764=VERTEX_POINT('',#70927);
#13765=VERTEX_POINT('',#70932);
#13766=VERTEX_POINT('',#70936);
#13767=VERTEX_POINT('',#70941);
#13768=VERTEX_POINT('',#70945);
#13769=VERTEX_POINT('',#70950);
#13770=VERTEX_POINT('',#70954);
#13771=VERTEX_POINT('',#70959);
#13772=VERTEX_POINT('',#70963);
#13773=VERTEX_POINT('',#70968);
#13774=VERTEX_POINT('',#70972);
#13775=VERTEX_POINT('',#70977);
#13776=VERTEX_POINT('',#70981);
#13777=VERTEX_POINT('',#70986);
#13778=VERTEX_POINT('',#70990);
#13779=VERTEX_POINT('',#70995);
#13780=VERTEX_POINT('',#70999);
#13781=VERTEX_POINT('',#71004);
#13782=VERTEX_POINT('',#71008);
#13783=VERTEX_POINT('',#71010);
#13784=VERTEX_POINT('',#71014);
#13785=VERTEX_POINT('',#71016);
#13786=VERTEX_POINT('',#71020);
#13787=VERTEX_POINT('',#71022);
#13788=VERTEX_POINT('',#71026);
#13789=VERTEX_POINT('',#71028);
#13790=VERTEX_POINT('',#71032);
#13791=VERTEX_POINT('',#71034);
#13792=VERTEX_POINT('',#71038);
#13793=VERTEX_POINT('',#71040);
#13794=VERTEX_POINT('',#71044);
#13795=VERTEX_POINT('',#71046);
#13796=VERTEX_POINT('',#71050);
#13797=VERTEX_POINT('',#71052);
#13798=VERTEX_POINT('',#71056);
#13799=VERTEX_POINT('',#71058);
#13800=VERTEX_POINT('',#71062);
#13801=VERTEX_POINT('',#71064);
#13802=VERTEX_POINT('',#71068);
#13803=VERTEX_POINT('',#71070);
#13804=VERTEX_POINT('',#71074);
#13805=VERTEX_POINT('',#71076);
#13806=VERTEX_POINT('',#71080);
#13807=VERTEX_POINT('',#71082);
#13808=VERTEX_POINT('',#71086);
#13809=VERTEX_POINT('',#71088);
#13810=VERTEX_POINT('',#71092);
#13811=VERTEX_POINT('',#71094);
#13812=VERTEX_POINT('',#71098);
#13813=VERTEX_POINT('',#71100);
#13814=VERTEX_POINT('',#71104);
#13815=VERTEX_POINT('',#71106);
#13816=VERTEX_POINT('',#71110);
#13817=VERTEX_POINT('',#71112);
#13818=VERTEX_POINT('',#71116);
#13819=VERTEX_POINT('',#71118);
#13820=VERTEX_POINT('',#71122);
#13821=VERTEX_POINT('',#71124);
#13822=VERTEX_POINT('',#71128);
#13823=VERTEX_POINT('',#71130);
#13824=VERTEX_POINT('',#71134);
#13825=VERTEX_POINT('',#71136);
#13826=VERTEX_POINT('',#71140);
#13827=VERTEX_POINT('',#71142);
#13828=VERTEX_POINT('',#71146);
#13829=VERTEX_POINT('',#71148);
#13830=VERTEX_POINT('',#71152);
#13831=VERTEX_POINT('',#71154);
#13832=VERTEX_POINT('',#71158);
#13833=VERTEX_POINT('',#71160);
#13834=VERTEX_POINT('',#71164);
#13835=VERTEX_POINT('',#71166);
#13836=VERTEX_POINT('',#71170);
#13837=VERTEX_POINT('',#71172);
#13838=VERTEX_POINT('',#71176);
#13839=VERTEX_POINT('',#71178);
#13840=VERTEX_POINT('',#71182);
#13841=VERTEX_POINT('',#71184);
#13842=VERTEX_POINT('',#71188);
#13843=VERTEX_POINT('',#71190);
#13844=VERTEX_POINT('',#71194);
#13845=VERTEX_POINT('',#71196);
#13846=VERTEX_POINT('',#71200);
#13847=VERTEX_POINT('',#71202);
#13848=VERTEX_POINT('',#71206);
#13849=VERTEX_POINT('',#71208);
#13850=VERTEX_POINT('',#71212);
#13851=VERTEX_POINT('',#71214);
#13852=VERTEX_POINT('',#71218);
#13853=VERTEX_POINT('',#71220);
#13854=VERTEX_POINT('',#71224);
#13855=VERTEX_POINT('',#71226);
#13856=VERTEX_POINT('',#71230);
#13857=VERTEX_POINT('',#71232);
#13858=VERTEX_POINT('',#71236);
#13859=VERTEX_POINT('',#71238);
#13860=VERTEX_POINT('',#71252);
#13861=VERTEX_POINT('',#71253);
#13862=VERTEX_POINT('',#71262);
#13863=VERTEX_POINT('',#71266);
#13864=VERTEX_POINT('',#71268);
#13865=VERTEX_POINT('',#71272);
#13866=VERTEX_POINT('',#71274);
#13867=VERTEX_POINT('',#71278);
#13868=VERTEX_POINT('',#71280);
#13869=VERTEX_POINT('',#71284);
#13870=VERTEX_POINT('',#71286);
#13871=VERTEX_POINT('',#71290);
#13872=VERTEX_POINT('',#71292);
#13873=VERTEX_POINT('',#71296);
#13874=VERTEX_POINT('',#71298);
#13875=VERTEX_POINT('',#71302);
#13876=VERTEX_POINT('',#71304);
#13877=VERTEX_POINT('',#71308);
#13878=VERTEX_POINT('',#71310);
#13879=VERTEX_POINT('',#71314);
#13880=VERTEX_POINT('',#71316);
#13881=VERTEX_POINT('',#71320);
#13882=VERTEX_POINT('',#71322);
#13883=VERTEX_POINT('',#71326);
#13884=VERTEX_POINT('',#71328);
#13885=VERTEX_POINT('',#71332);
#13886=VERTEX_POINT('',#71334);
#13887=VERTEX_POINT('',#71338);
#13888=VERTEX_POINT('',#71340);
#13889=VERTEX_POINT('',#71344);
#13890=VERTEX_POINT('',#71346);
#13891=VERTEX_POINT('',#71350);
#13892=VERTEX_POINT('',#71352);
#13893=VERTEX_POINT('',#71356);
#13894=VERTEX_POINT('',#71358);
#13895=VERTEX_POINT('',#71362);
#13896=VERTEX_POINT('',#71364);
#13897=VERTEX_POINT('',#71368);
#13898=VERTEX_POINT('',#71370);
#13899=VERTEX_POINT('',#71374);
#13900=VERTEX_POINT('',#71376);
#13901=VERTEX_POINT('',#71380);
#13902=VERTEX_POINT('',#71382);
#13903=VERTEX_POINT('',#71386);
#13904=VERTEX_POINT('',#71388);
#13905=VERTEX_POINT('',#71392);
#13906=VERTEX_POINT('',#71394);
#13907=VERTEX_POINT('',#71398);
#13908=VERTEX_POINT('',#71400);
#13909=VERTEX_POINT('',#71404);
#13910=VERTEX_POINT('',#71406);
#13911=VERTEX_POINT('',#71410);
#13912=VERTEX_POINT('',#71412);
#13913=VERTEX_POINT('',#71416);
#13914=VERTEX_POINT('',#71418);
#13915=VERTEX_POINT('',#71422);
#13916=VERTEX_POINT('',#71424);
#13917=VERTEX_POINT('',#71428);
#13918=VERTEX_POINT('',#71430);
#13919=VERTEX_POINT('',#71434);
#13920=VERTEX_POINT('',#71436);
#13921=VERTEX_POINT('',#71440);
#13922=VERTEX_POINT('',#71442);
#13923=VERTEX_POINT('',#71446);
#13924=VERTEX_POINT('',#71448);
#13925=VERTEX_POINT('',#71452);
#13926=VERTEX_POINT('',#71454);
#13927=VERTEX_POINT('',#71458);
#13928=VERTEX_POINT('',#71460);
#13929=VERTEX_POINT('',#71464);
#13930=VERTEX_POINT('',#71466);
#13931=VERTEX_POINT('',#71470);
#13932=VERTEX_POINT('',#71472);
#13933=VERTEX_POINT('',#71476);
#13934=VERTEX_POINT('',#71478);
#13935=VERTEX_POINT('',#71482);
#13936=VERTEX_POINT('',#71484);
#13937=VERTEX_POINT('',#71488);
#13938=VERTEX_POINT('',#71490);
#13939=VERTEX_POINT('',#71494);
#13940=VERTEX_POINT('',#71496);
#13941=VERTEX_POINT('',#71500);
#13942=VERTEX_POINT('',#71502);
#13943=VERTEX_POINT('',#71506);
#13944=VERTEX_POINT('',#71508);
#13945=VERTEX_POINT('',#71512);
#13946=VERTEX_POINT('',#71514);
#13947=VERTEX_POINT('',#71518);
#13948=VERTEX_POINT('',#71520);
#13949=VERTEX_POINT('',#71524);
#13950=VERTEX_POINT('',#71526);
#13951=VERTEX_POINT('',#71530);
#13952=VERTEX_POINT('',#71532);
#13953=VERTEX_POINT('',#71536);
#13954=VERTEX_POINT('',#71538);
#13955=VERTEX_POINT('',#71542);
#13956=VERTEX_POINT('',#71544);
#13957=VERTEX_POINT('',#71548);
#13958=VERTEX_POINT('',#71550);
#13959=VERTEX_POINT('',#71554);
#13960=VERTEX_POINT('',#71556);
#13961=VERTEX_POINT('',#71560);
#13962=VERTEX_POINT('',#71562);
#13963=VERTEX_POINT('',#71566);
#13964=VERTEX_POINT('',#71568);
#13965=VERTEX_POINT('',#71572);
#13966=VERTEX_POINT('',#71574);
#13967=VERTEX_POINT('',#71578);
#13968=VERTEX_POINT('',#71580);
#13969=VERTEX_POINT('',#71584);
#13970=VERTEX_POINT('',#71586);
#13971=VERTEX_POINT('',#71590);
#13972=VERTEX_POINT('',#71592);
#13973=VERTEX_POINT('',#71596);
#13974=VERTEX_POINT('',#71598);
#13975=VERTEX_POINT('',#71602);
#13976=VERTEX_POINT('',#71604);
#13977=VERTEX_POINT('',#71608);
#13978=VERTEX_POINT('',#71610);
#13979=VERTEX_POINT('',#71614);
#13980=VERTEX_POINT('',#71616);
#13981=VERTEX_POINT('',#71620);
#13982=VERTEX_POINT('',#71622);
#13983=VERTEX_POINT('',#71626);
#13984=VERTEX_POINT('',#71628);
#13985=VERTEX_POINT('',#71632);
#13986=VERTEX_POINT('',#71634);
#13987=VERTEX_POINT('',#71638);
#13988=VERTEX_POINT('',#71640);
#13989=VERTEX_POINT('',#71644);
#13990=VERTEX_POINT('',#71646);
#13991=VERTEX_POINT('',#71650);
#13992=VERTEX_POINT('',#71652);
#13993=VERTEX_POINT('',#71656);
#13994=VERTEX_POINT('',#71658);
#13995=VERTEX_POINT('',#71662);
#13996=VERTEX_POINT('',#71664);
#13997=VERTEX_POINT('',#71668);
#13998=VERTEX_POINT('',#71670);
#13999=VERTEX_POINT('',#71674);
#14000=VERTEX_POINT('',#71676);
#14001=VERTEX_POINT('',#71680);
#14002=VERTEX_POINT('',#71682);
#14003=VERTEX_POINT('',#71686);
#14004=VERTEX_POINT('',#71688);
#14005=VERTEX_POINT('',#71692);
#14006=VERTEX_POINT('',#71694);
#14007=VERTEX_POINT('',#71698);
#14008=VERTEX_POINT('',#71700);
#14009=VERTEX_POINT('',#71704);
#14010=VERTEX_POINT('',#71706);
#14011=VERTEX_POINT('',#71710);
#14012=VERTEX_POINT('',#71712);
#14013=VERTEX_POINT('',#71716);
#14014=VERTEX_POINT('',#71718);
#14015=VERTEX_POINT('',#71722);
#14016=VERTEX_POINT('',#71724);
#14017=VERTEX_POINT('',#71728);
#14018=VERTEX_POINT('',#71730);
#14019=VERTEX_POINT('',#71734);
#14020=VERTEX_POINT('',#71736);
#14021=VERTEX_POINT('',#71740);
#14022=VERTEX_POINT('',#71742);
#14023=VERTEX_POINT('',#71746);
#14024=VERTEX_POINT('',#71748);
#14025=VERTEX_POINT('',#71752);
#14026=VERTEX_POINT('',#71754);
#14027=VERTEX_POINT('',#71758);
#14028=VERTEX_POINT('',#71760);
#14029=VERTEX_POINT('',#71764);
#14030=VERTEX_POINT('',#71766);
#14031=VERTEX_POINT('',#71770);
#14032=VERTEX_POINT('',#71772);
#14033=VERTEX_POINT('',#71776);
#14034=VERTEX_POINT('',#71778);
#14035=VERTEX_POINT('',#71782);
#14036=VERTEX_POINT('',#71784);
#14037=VERTEX_POINT('',#71788);
#14038=VERTEX_POINT('',#71790);
#14039=VERTEX_POINT('',#71794);
#14040=VERTEX_POINT('',#71796);
#14041=VERTEX_POINT('',#71800);
#14042=VERTEX_POINT('',#71802);
#14043=VERTEX_POINT('',#71806);
#14044=VERTEX_POINT('',#71808);
#14045=VERTEX_POINT('',#71812);
#14046=VERTEX_POINT('',#71814);
#14047=VERTEX_POINT('',#71818);
#14048=VERTEX_POINT('',#71820);
#14049=VERTEX_POINT('',#71824);
#14050=VERTEX_POINT('',#71826);
#14051=VERTEX_POINT('',#71830);
#14052=VERTEX_POINT('',#71832);
#14053=VERTEX_POINT('',#71836);
#14054=VERTEX_POINT('',#71838);
#14055=VERTEX_POINT('',#71842);
#14056=VERTEX_POINT('',#71844);
#14057=VERTEX_POINT('',#71848);
#14058=VERTEX_POINT('',#71850);
#14059=VERTEX_POINT('',#71854);
#14060=VERTEX_POINT('',#71856);
#14061=VERTEX_POINT('',#71860);
#14062=VERTEX_POINT('',#71862);
#14063=VERTEX_POINT('',#71866);
#14064=VERTEX_POINT('',#71868);
#14065=VERTEX_POINT('',#71872);
#14066=VERTEX_POINT('',#71874);
#14067=VERTEX_POINT('',#71878);
#14068=VERTEX_POINT('',#71880);
#14069=VERTEX_POINT('',#71884);
#14070=VERTEX_POINT('',#71886);
#14071=VERTEX_POINT('',#71890);
#14072=VERTEX_POINT('',#71892);
#14073=VERTEX_POINT('',#71896);
#14074=VERTEX_POINT('',#71898);
#14075=VERTEX_POINT('',#71902);
#14076=VERTEX_POINT('',#71904);
#14077=VERTEX_POINT('',#71908);
#14078=VERTEX_POINT('',#71910);
#14079=VERTEX_POINT('',#71914);
#14080=VERTEX_POINT('',#71916);
#14081=VERTEX_POINT('',#71920);
#14082=VERTEX_POINT('',#71922);
#14083=VERTEX_POINT('',#71926);
#14084=VERTEX_POINT('',#71928);
#14085=VERTEX_POINT('',#71932);
#14086=VERTEX_POINT('',#71934);
#14087=VERTEX_POINT('',#71938);
#14088=VERTEX_POINT('',#71940);
#14089=VERTEX_POINT('',#71944);
#14090=VERTEX_POINT('',#71946);
#14091=VERTEX_POINT('',#71950);
#14092=VERTEX_POINT('',#71952);
#14093=VERTEX_POINT('',#71956);
#14094=VERTEX_POINT('',#71958);
#14095=VERTEX_POINT('',#71962);
#14096=VERTEX_POINT('',#71964);
#14097=VERTEX_POINT('',#71968);
#14098=VERTEX_POINT('',#71970);
#14099=VERTEX_POINT('',#71974);
#14100=VERTEX_POINT('',#71979);
#14101=VERTEX_POINT('',#71983);
#14102=VERTEX_POINT('',#71988);
#14103=VERTEX_POINT('',#71992);
#14104=VERTEX_POINT('',#71997);
#14105=VERTEX_POINT('',#72001);
#14106=VERTEX_POINT('',#72006);
#14107=VERTEX_POINT('',#72010);
#14108=VERTEX_POINT('',#72015);
#14109=VERTEX_POINT('',#72019);
#14110=VERTEX_POINT('',#72024);
#14111=VERTEX_POINT('',#72028);
#14112=VERTEX_POINT('',#72033);
#14113=VERTEX_POINT('',#72037);
#14114=VERTEX_POINT('',#72042);
#14115=VERTEX_POINT('',#72046);
#14116=VERTEX_POINT('',#72051);
#14117=VERTEX_POINT('',#72055);
#14118=VERTEX_POINT('',#72060);
#14119=VERTEX_POINT('',#72064);
#14120=VERTEX_POINT('',#72069);
#14121=VERTEX_POINT('',#72073);
#14122=VERTEX_POINT('',#72078);
#14123=VERTEX_POINT('',#72082);
#14124=VERTEX_POINT('',#72087);
#14125=VERTEX_POINT('',#72091);
#14126=VERTEX_POINT('',#72096);
#14127=VERTEX_POINT('',#72100);
#14128=VERTEX_POINT('',#72105);
#14129=VERTEX_POINT('',#72109);
#14130=VERTEX_POINT('',#72111);
#14131=VERTEX_POINT('',#72115);
#14132=VERTEX_POINT('',#72117);
#14133=VERTEX_POINT('',#72121);
#14134=VERTEX_POINT('',#72123);
#14135=VERTEX_POINT('',#72127);
#14136=VERTEX_POINT('',#72129);
#14137=VERTEX_POINT('',#72133);
#14138=VERTEX_POINT('',#72135);
#14139=VERTEX_POINT('',#72139);
#14140=VERTEX_POINT('',#72141);
#14141=VERTEX_POINT('',#72145);
#14142=VERTEX_POINT('',#72147);
#14143=VERTEX_POINT('',#72151);
#14144=VERTEX_POINT('',#72153);
#14145=VERTEX_POINT('',#72157);
#14146=VERTEX_POINT('',#72159);
#14147=VERTEX_POINT('',#72163);
#14148=VERTEX_POINT('',#72165);
#14149=VERTEX_POINT('',#72169);
#14150=VERTEX_POINT('',#72171);
#14151=VERTEX_POINT('',#72183);
#14152=VERTEX_POINT('',#72185);
#14153=VERTEX_POINT('',#72189);
#14154=VERTEX_POINT('',#72193);
#14155=VERTEX_POINT('',#72197);
#14156=VERTEX_POINT('',#72201);
#14157=VERTEX_POINT('',#72205);
#14158=VERTEX_POINT('',#72207);
#14159=VERTEX_POINT('',#72211);
#14160=VERTEX_POINT('',#72213);
#14161=VERTEX_POINT('',#72217);
#14162=VERTEX_POINT('',#72219);
#14163=VERTEX_POINT('',#72223);
#14164=VERTEX_POINT('',#72225);
#14165=VERTEX_POINT('',#72229);
#14166=VERTEX_POINT('',#72231);
#14167=VERTEX_POINT('',#72235);
#14168=VERTEX_POINT('',#72237);
#14169=VERTEX_POINT('',#72241);
#14170=VERTEX_POINT('',#72243);
#14171=VERTEX_POINT('',#72247);
#14172=VERTEX_POINT('',#72249);
#14173=VERTEX_POINT('',#72253);
#14174=VERTEX_POINT('',#72255);
#14175=VERTEX_POINT('',#72259);
#14176=VERTEX_POINT('',#72261);
#14177=VERTEX_POINT('',#72265);
#14178=VERTEX_POINT('',#72267);
#14179=VERTEX_POINT('',#72271);
#14180=VERTEX_POINT('',#72273);
#14181=VERTEX_POINT('',#72277);
#14182=VERTEX_POINT('',#72279);
#14183=VERTEX_POINT('',#72283);
#14184=VERTEX_POINT('',#72285);
#14185=VERTEX_POINT('',#72289);
#14186=VERTEX_POINT('',#72291);
#14187=VERTEX_POINT('',#72295);
#14188=VERTEX_POINT('',#72297);
#14189=VERTEX_POINT('',#72301);
#14190=VERTEX_POINT('',#72303);
#14191=VERTEX_POINT('',#72307);
#14192=VERTEX_POINT('',#72309);
#14193=VERTEX_POINT('',#72313);
#14194=VERTEX_POINT('',#72315);
#14195=VERTEX_POINT('',#72319);
#14196=VERTEX_POINT('',#72321);
#14197=VERTEX_POINT('',#72325);
#14198=VERTEX_POINT('',#72327);
#14199=VERTEX_POINT('',#72331);
#14200=VERTEX_POINT('',#72333);
#14201=VERTEX_POINT('',#72337);
#14202=VERTEX_POINT('',#72339);
#14203=VERTEX_POINT('',#72343);
#14204=VERTEX_POINT('',#72345);
#14205=VERTEX_POINT('',#72349);
#14206=VERTEX_POINT('',#72351);
#14207=VERTEX_POINT('',#72355);
#14208=VERTEX_POINT('',#72357);
#14209=VERTEX_POINT('',#72361);
#14210=VERTEX_POINT('',#72363);
#14211=VERTEX_POINT('',#72367);
#14212=VERTEX_POINT('',#72369);
#14213=VERTEX_POINT('',#72373);
#14214=VERTEX_POINT('',#72375);
#14215=VERTEX_POINT('',#72379);
#14216=VERTEX_POINT('',#72381);
#14217=VERTEX_POINT('',#72385);
#14218=VERTEX_POINT('',#72387);
#14219=VERTEX_POINT('',#72391);
#14220=VERTEX_POINT('',#72393);
#14221=VERTEX_POINT('',#72397);
#14222=VERTEX_POINT('',#72399);
#14223=VERTEX_POINT('',#72403);
#14224=VERTEX_POINT('',#72405);
#14225=VERTEX_POINT('',#72409);
#14226=VERTEX_POINT('',#72411);
#14227=VERTEX_POINT('',#72415);
#14228=VERTEX_POINT('',#72417);
#14229=VERTEX_POINT('',#72421);
#14230=VERTEX_POINT('',#72423);
#14231=VERTEX_POINT('',#72427);
#14232=VERTEX_POINT('',#72429);
#14233=VERTEX_POINT('',#72433);
#14234=VERTEX_POINT('',#72435);
#14235=VERTEX_POINT('',#72439);
#14236=VERTEX_POINT('',#72441);
#14237=VERTEX_POINT('',#72445);
#14238=VERTEX_POINT('',#72447);
#14239=VERTEX_POINT('',#72451);
#14240=VERTEX_POINT('',#72453);
#14241=VERTEX_POINT('',#72457);
#14242=VERTEX_POINT('',#72459);
#14243=VERTEX_POINT('',#72463);
#14244=VERTEX_POINT('',#72465);
#14245=VERTEX_POINT('',#72469);
#14246=VERTEX_POINT('',#72471);
#14247=VERTEX_POINT('',#72475);
#14248=VERTEX_POINT('',#72477);
#14249=VERTEX_POINT('',#72481);
#14250=VERTEX_POINT('',#72483);
#14251=VERTEX_POINT('',#72487);
#14252=VERTEX_POINT('',#72489);
#14253=VERTEX_POINT('',#72493);
#14254=VERTEX_POINT('',#72495);
#14255=VERTEX_POINT('',#72499);
#14256=VERTEX_POINT('',#72501);
#14257=VERTEX_POINT('',#72505);
#14258=VERTEX_POINT('',#72507);
#14259=VERTEX_POINT('',#72511);
#14260=VERTEX_POINT('',#72513);
#14261=VERTEX_POINT('',#72517);
#14262=VERTEX_POINT('',#72519);
#14263=VERTEX_POINT('',#72523);
#14264=VERTEX_POINT('',#72525);
#14265=VERTEX_POINT('',#72529);
#14266=VERTEX_POINT('',#72531);
#14267=VERTEX_POINT('',#72535);
#14268=VERTEX_POINT('',#72537);
#14269=VERTEX_POINT('',#72541);
#14270=VERTEX_POINT('',#72543);
#14271=VERTEX_POINT('',#72547);
#14272=VERTEX_POINT('',#72549);
#14273=VERTEX_POINT('',#72553);
#14274=VERTEX_POINT('',#72555);
#14275=VERTEX_POINT('',#72559);
#14276=VERTEX_POINT('',#72561);
#14277=VERTEX_POINT('',#72565);
#14278=VERTEX_POINT('',#72567);
#14279=VERTEX_POINT('',#72571);
#14280=VERTEX_POINT('',#72573);
#14281=VERTEX_POINT('',#72577);
#14282=VERTEX_POINT('',#72579);
#14283=VERTEX_POINT('',#72583);
#14284=VERTEX_POINT('',#72585);
#14285=VERTEX_POINT('',#72589);
#14286=VERTEX_POINT('',#72591);
#14287=VERTEX_POINT('',#72595);
#14288=VERTEX_POINT('',#72597);
#14289=VERTEX_POINT('',#72601);
#14290=VERTEX_POINT('',#72603);
#14291=VERTEX_POINT('',#72607);
#14292=VERTEX_POINT('',#72609);
#14293=VERTEX_POINT('',#72613);
#14294=VERTEX_POINT('',#72615);
#14295=VERTEX_POINT('',#72619);
#14296=VERTEX_POINT('',#72621);
#14297=VERTEX_POINT('',#72625);
#14298=VERTEX_POINT('',#72627);
#14299=VERTEX_POINT('',#72631);
#14300=VERTEX_POINT('',#72633);
#14301=VERTEX_POINT('',#72637);
#14302=VERTEX_POINT('',#72639);
#14303=VERTEX_POINT('',#72643);
#14304=VERTEX_POINT('',#72645);
#14305=VERTEX_POINT('',#72649);
#14306=VERTEX_POINT('',#72651);
#14307=VERTEX_POINT('',#72655);
#14308=VERTEX_POINT('',#72657);
#14309=VERTEX_POINT('',#72661);
#14310=VERTEX_POINT('',#72663);
#14311=VERTEX_POINT('',#72667);
#14312=VERTEX_POINT('',#72669);
#14313=VERTEX_POINT('',#72673);
#14314=VERTEX_POINT('',#72675);
#14315=VERTEX_POINT('',#72679);
#14316=VERTEX_POINT('',#72681);
#14317=VERTEX_POINT('',#72685);
#14318=VERTEX_POINT('',#72687);
#14319=VERTEX_POINT('',#72691);
#14320=VERTEX_POINT('',#72693);
#14321=VERTEX_POINT('',#72697);
#14322=VERTEX_POINT('',#72699);
#14323=VERTEX_POINT('',#72703);
#14324=VERTEX_POINT('',#72705);
#14325=VERTEX_POINT('',#72709);
#14326=VERTEX_POINT('',#72711);
#14327=VERTEX_POINT('',#72715);
#14328=VERTEX_POINT('',#72717);
#14329=VERTEX_POINT('',#72721);
#14330=VERTEX_POINT('',#72723);
#14331=VERTEX_POINT('',#72727);
#14332=VERTEX_POINT('',#72729);
#14333=VERTEX_POINT('',#72733);
#14334=VERTEX_POINT('',#72735);
#14335=VERTEX_POINT('',#72739);
#14336=VERTEX_POINT('',#72741);
#14337=VERTEX_POINT('',#72745);
#14338=VERTEX_POINT('',#72747);
#14339=VERTEX_POINT('',#72751);
#14340=VERTEX_POINT('',#72753);
#14341=VERTEX_POINT('',#72757);
#14342=VERTEX_POINT('',#72759);
#14343=VERTEX_POINT('',#72763);
#14344=VERTEX_POINT('',#72765);
#14345=VERTEX_POINT('',#72769);
#14346=VERTEX_POINT('',#72771);
#14347=VERTEX_POINT('',#72775);
#14348=VERTEX_POINT('',#72777);
#14349=VERTEX_POINT('',#72781);
#14350=VERTEX_POINT('',#72783);
#14351=VERTEX_POINT('',#72787);
#14352=VERTEX_POINT('',#72789);
#14353=VERTEX_POINT('',#72793);
#14354=VERTEX_POINT('',#72795);
#14355=VERTEX_POINT('',#72799);
#14356=VERTEX_POINT('',#72801);
#14357=VERTEX_POINT('',#72805);
#14358=VERTEX_POINT('',#72807);
#14359=VERTEX_POINT('',#72811);
#14360=VERTEX_POINT('',#72813);
#14361=VERTEX_POINT('',#72817);
#14362=VERTEX_POINT('',#72819);
#14363=VERTEX_POINT('',#72823);
#14364=VERTEX_POINT('',#72825);
#14365=VERTEX_POINT('',#72829);
#14366=VERTEX_POINT('',#72831);
#14367=VERTEX_POINT('',#72835);
#14368=VERTEX_POINT('',#72837);
#14369=VERTEX_POINT('',#72841);
#14370=VERTEX_POINT('',#72843);
#14371=VERTEX_POINT('',#72847);
#14372=VERTEX_POINT('',#72849);
#14373=VERTEX_POINT('',#72853);
#14374=VERTEX_POINT('',#72855);
#14375=VERTEX_POINT('',#72859);
#14376=VERTEX_POINT('',#72861);
#14377=VERTEX_POINT('',#72865);
#14378=VERTEX_POINT('',#72867);
#14379=VERTEX_POINT('',#72871);
#14380=VERTEX_POINT('',#72873);
#14381=VERTEX_POINT('',#72877);
#14382=VERTEX_POINT('',#72879);
#14383=VERTEX_POINT('',#72883);
#14384=VERTEX_POINT('',#72885);
#14385=VERTEX_POINT('',#72889);
#14386=VERTEX_POINT('',#72891);
#14387=VERTEX_POINT('',#72895);
#14388=VERTEX_POINT('',#72897);
#14389=VERTEX_POINT('',#72901);
#14390=VERTEX_POINT('',#72903);
#14391=VERTEX_POINT('',#72907);
#14392=VERTEX_POINT('',#72909);
#14393=VERTEX_POINT('',#72913);
#14394=VERTEX_POINT('',#72915);
#14395=VERTEX_POINT('',#72919);
#14396=VERTEX_POINT('',#72921);
#14397=VERTEX_POINT('',#72925);
#14398=VERTEX_POINT('',#72927);
#14399=VERTEX_POINT('',#72931);
#14400=VERTEX_POINT('',#72933);
#14401=VERTEX_POINT('',#72937);
#14402=VERTEX_POINT('',#72939);
#14403=VERTEX_POINT('',#72943);
#14404=VERTEX_POINT('',#72945);
#14405=VERTEX_POINT('',#72949);
#14406=VERTEX_POINT('',#72951);
#14407=VERTEX_POINT('',#72955);
#14408=VERTEX_POINT('',#72957);
#14409=VERTEX_POINT('',#72961);
#14410=VERTEX_POINT('',#72963);
#14411=VERTEX_POINT('',#72967);
#14412=VERTEX_POINT('',#72969);
#14413=VERTEX_POINT('',#72973);
#14414=VERTEX_POINT('',#72975);
#14415=VERTEX_POINT('',#72979);
#14416=VERTEX_POINT('',#72981);
#14417=VERTEX_POINT('',#72985);
#14418=VERTEX_POINT('',#72987);
#14419=VERTEX_POINT('',#72991);
#14420=VERTEX_POINT('',#72993);
#14421=VERTEX_POINT('',#72997);
#14422=VERTEX_POINT('',#72999);
#14423=VERTEX_POINT('',#73003);
#14424=VERTEX_POINT('',#73005);
#14425=VERTEX_POINT('',#73009);
#14426=VERTEX_POINT('',#73011);
#14427=VERTEX_POINT('',#73015);
#14428=VERTEX_POINT('',#73017);
#14429=VERTEX_POINT('',#73021);
#14430=VERTEX_POINT('',#73023);
#14431=VERTEX_POINT('',#73027);
#14432=VERTEX_POINT('',#73029);
#14433=VERTEX_POINT('',#73033);
#14434=VERTEX_POINT('',#73035);
#14435=VERTEX_POINT('',#73039);
#14436=VERTEX_POINT('',#73041);
#14437=VERTEX_POINT('',#73045);
#14438=VERTEX_POINT('',#73047);
#14439=VERTEX_POINT('',#73051);
#14440=VERTEX_POINT('',#73053);
#14441=VERTEX_POINT('',#73057);
#14442=VERTEX_POINT('',#73059);
#14443=VERTEX_POINT('',#73063);
#14444=VERTEX_POINT('',#73065);
#14445=VERTEX_POINT('',#73069);
#14446=VERTEX_POINT('',#73071);
#14447=VERTEX_POINT('',#73075);
#14448=VERTEX_POINT('',#73077);
#14449=VERTEX_POINT('',#73081);
#14450=VERTEX_POINT('',#73083);
#14451=VERTEX_POINT('',#73087);
#14452=VERTEX_POINT('',#73089);
#14453=VERTEX_POINT('',#73093);
#14454=VERTEX_POINT('',#73095);
#14455=VERTEX_POINT('',#73099);
#14456=VERTEX_POINT('',#73101);
#14457=VERTEX_POINT('',#73105);
#14458=VERTEX_POINT('',#73107);
#14459=VERTEX_POINT('',#73111);
#14460=VERTEX_POINT('',#73113);
#14461=VERTEX_POINT('',#73117);
#14462=VERTEX_POINT('',#73119);
#14463=VERTEX_POINT('',#73123);
#14464=VERTEX_POINT('',#73125);
#14465=VERTEX_POINT('',#73129);
#14466=VERTEX_POINT('',#73131);
#14467=VERTEX_POINT('',#73135);
#14468=VERTEX_POINT('',#73137);
#14469=VERTEX_POINT('',#73141);
#14470=VERTEX_POINT('',#73143);
#14471=VERTEX_POINT('',#73147);
#14472=VERTEX_POINT('',#73149);
#14473=VERTEX_POINT('',#73392);
#14474=VERTEX_POINT('',#73394);
#14475=VERTEX_POINT('',#73398);
#14476=VERTEX_POINT('',#73400);
#14477=VERTEX_POINT('',#73408);
#14478=VERTEX_POINT('',#73409);
#14479=VERTEX_POINT('',#73411);
#14480=VERTEX_POINT('',#73413);
#14481=VERTEX_POINT('',#73415);
#14482=VERTEX_POINT('',#73417);
#14483=EDGE_CURVE('',#11093,#11094,#8601,.T.);
#14484=EDGE_CURVE('',#11095,#11093,#8602,.T.);
#14485=EDGE_CURVE('',#11095,#11096,#8603,.T.);
#14486=EDGE_CURVE('',#11094,#11096,#8604,.T.);
#14487=EDGE_CURVE('',#11094,#11097,#8605,.T.);
#14488=EDGE_CURVE('',#11098,#11097,#8606,.T.);
#14489=EDGE_CURVE('',#11098,#11099,#8607,.T.);
#14490=EDGE_CURVE('',#11094,#11099,#8608,.T.);
#14491=EDGE_CURVE('',#11094,#11100,#8609,.T.);
#14492=EDGE_CURVE('',#11099,#11101,#8610,.T.);
#14493=EDGE_CURVE('',#11100,#11101,#8611,.T.);
#14494=EDGE_CURVE('',#11101,#11098,#8612,.T.);
#14495=EDGE_CURVE('',#11096,#11102,#8613,.T.);
#14496=EDGE_CURVE('',#11097,#11102,#8614,.T.);
#14497=EDGE_CURVE('',#11102,#11095,#8615,.T.);
#14498=EDGE_CURVE('',#11094,#11103,#8616,.T.);
#14499=EDGE_CURVE('',#11103,#11104,#8617,.T.);
#14500=EDGE_CURVE('',#11093,#11104,#8618,.T.);
#14501=EDGE_CURVE('',#11105,#11100,#8619,.T.);
#14502=EDGE_CURVE('',#11105,#11103,#8620,.T.);
#14503=EDGE_CURVE('',#11104,#11105,#8621,.T.);
#14504=EDGE_CURVE('',#11106,#11106,#3400,.T.);
#14505=EDGE_CURVE('',#11106,#11107,#8622,.T.);
#14506=EDGE_CURVE('',#11107,#11107,#3401,.T.);
#14507=EDGE_CURVE('',#11108,#11109,#3402,.T.);
#14508=EDGE_CURVE('',#11110,#11111,#3403,.T.);
#14509=EDGE_CURVE('',#11112,#11113,#3404,.T.);
#14510=EDGE_CURVE('',#11114,#11114,#3405,.T.);
#14511=EDGE_CURVE('',#11114,#11115,#8623,.T.);
#14512=EDGE_CURVE('',#11115,#11115,#3406,.T.);
#14513=EDGE_CURVE('',#11116,#11116,#3407,.T.);
#14514=EDGE_CURVE('',#11116,#11117,#8624,.T.);
#14515=EDGE_CURVE('',#11117,#11117,#3408,.T.);
#14516=EDGE_CURVE('',#11118,#11118,#3409,.T.);
#14517=EDGE_CURVE('',#11118,#11119,#8625,.T.);
#14518=EDGE_CURVE('',#11119,#11119,#3410,.T.);
#14519=EDGE_CURVE('',#11120,#11121,#3411,.T.);
#14520=EDGE_CURVE('',#11121,#11122,#8626,.T.);
#14521=EDGE_CURVE('',#11122,#11123,#3412,.T.);
#14522=EDGE_CURVE('',#11123,#11120,#8627,.T.);
#14523=EDGE_CURVE('',#11121,#11124,#8628,.T.);
#14524=EDGE_CURVE('',#11125,#11124,#8629,.T.);
#14525=EDGE_CURVE('',#11122,#11125,#8630,.T.);
#14526=EDGE_CURVE('',#11126,#11127,#3413,.T.);
#14527=EDGE_CURVE('',#11127,#11128,#8631,.T.);
#14528=EDGE_CURVE('',#11128,#11129,#3414,.T.);
#14529=EDGE_CURVE('',#11129,#11126,#8632,.T.);
#14530=EDGE_CURVE('',#11127,#11130,#8633,.T.);
#14531=EDGE_CURVE('',#11131,#11130,#8634,.T.);
#14532=EDGE_CURVE('',#11128,#11131,#8635,.T.);
#14533=EDGE_CURVE('',#11132,#11133,#3415,.T.);
#14534=EDGE_CURVE('',#11133,#11134,#8636,.T.);
#14535=EDGE_CURVE('',#11134,#11135,#3416,.T.);
#14536=EDGE_CURVE('',#11135,#11132,#8637,.T.);
#14537=EDGE_CURVE('',#11133,#11136,#8638,.T.);
#14538=EDGE_CURVE('',#11137,#11136,#8639,.T.);
#14539=EDGE_CURVE('',#11134,#11137,#8640,.T.);
#14540=EDGE_CURVE('',#11138,#11139,#3417,.T.);
#14541=EDGE_CURVE('',#11139,#11140,#8641,.T.);
#14542=EDGE_CURVE('',#11140,#11141,#3418,.T.);
#14543=EDGE_CURVE('',#11141,#11138,#8642,.T.);
#14544=EDGE_CURVE('',#11142,#11139,#3419,.T.);
#14545=EDGE_CURVE('',#11143,#11142,#8643,.T.);
#14546=EDGE_CURVE('',#11143,#11140,#3420,.T.);
#14547=EDGE_CURVE('',#11138,#11129,#8644,.T.);
#14548=EDGE_CURVE('',#11144,#11131,#3421,.T.);
#14549=EDGE_CURVE('',#11144,#11145,#3422,.T.);
#14550=EDGE_CURVE('',#11146,#11145,#3423,.T.);
#14551=EDGE_CURVE('',#11146,#11123,#8645,.T.);
#14552=EDGE_CURVE('',#11147,#11125,#3424,.T.);
#14553=EDGE_CURVE('',#11147,#11148,#3425,.T.);
#14554=EDGE_CURVE('',#11149,#11148,#3426,.T.);
#14555=EDGE_CURVE('',#11149,#11135,#8646,.T.);
#14556=EDGE_CURVE('',#11142,#11137,#3427,.T.);
#14557=EDGE_CURVE('',#11130,#11150,#3428,.T.);
#14558=EDGE_CURVE('',#11150,#11144,#8647,.T.);
#14559=EDGE_CURVE('',#11150,#11151,#3429,.T.);
#14560=EDGE_CURVE('',#11145,#11151,#8648,.T.);
#14561=EDGE_CURVE('',#11151,#11152,#3430,.T.);
#14562=EDGE_CURVE('',#11152,#11146,#8649,.T.);
#14563=EDGE_CURVE('',#11124,#11153,#3431,.T.);
#14564=EDGE_CURVE('',#11153,#11147,#8650,.T.);
#14565=EDGE_CURVE('',#11136,#11143,#3432,.T.);
#14566=EDGE_CURVE('',#11148,#11154,#8651,.T.);
#14567=EDGE_CURVE('',#11154,#11155,#3433,.T.);
#14568=EDGE_CURVE('',#11155,#11149,#8652,.T.);
#14569=EDGE_CURVE('',#11155,#11132,#8653,.T.);
#14570=EDGE_CURVE('',#11153,#11154,#3434,.T.);
#14571=EDGE_CURVE('',#11152,#11120,#8654,.T.);
#14572=EDGE_CURVE('',#11141,#11126,#8655,.T.);
#14573=EDGE_CURVE('',#11156,#11157,#8656,.T.);
#14574=EDGE_CURVE('',#11158,#11156,#2974,.F.);
#14575=EDGE_CURVE('',#11158,#11159,#8657,.T.);
#14576=EDGE_CURVE('',#11159,#11159,#3435,.T.);
#14577=EDGE_CURVE('',#11160,#11158,#3436,.T.);
#14578=EDGE_CURVE('',#11157,#11160,#2975,.F.);
#14579=EDGE_CURVE('',#11161,#11162,#8658,.T.);
#14580=EDGE_CURVE('',#11156,#11161,#2976,.F.);
#14581=EDGE_CURVE('',#11162,#11157,#2977,.F.);
#14582=EDGE_CURVE('',#11163,#11164,#8659,.T.);
#14583=EDGE_CURVE('',#11161,#11163,#2978,.F.);
#14584=EDGE_CURVE('',#11164,#11162,#2979,.F.);
#14585=EDGE_CURVE('',#11165,#11166,#8660,.T.);
#14586=EDGE_CURVE('',#11163,#11165,#2980,.F.);
#14587=EDGE_CURVE('',#11166,#11164,#2981,.F.);
#14588=EDGE_CURVE('',#11167,#11168,#8661,.T.);
#14589=EDGE_CURVE('',#11165,#11167,#2982,.F.);
#14590=EDGE_CURVE('',#11168,#11166,#2983,.F.);
#14591=EDGE_CURVE('',#11169,#11170,#8662,.T.);
#14592=EDGE_CURVE('',#11167,#11169,#2984,.F.);
#14593=EDGE_CURVE('',#11170,#11168,#2985,.F.);
#14594=EDGE_CURVE('',#11171,#11172,#8663,.T.);
#14595=EDGE_CURVE('',#11169,#11171,#2986,.F.);
#14596=EDGE_CURVE('',#11172,#11170,#2987,.F.);
#14597=EDGE_CURVE('',#11173,#11174,#8664,.T.);
#14598=EDGE_CURVE('',#11171,#11173,#2988,.F.);
#14599=EDGE_CURVE('',#11174,#11172,#2989,.F.);
#14600=EDGE_CURVE('',#11175,#11176,#8665,.T.);
#14601=EDGE_CURVE('',#11173,#11175,#2990,.F.);
#14602=EDGE_CURVE('',#11176,#11174,#2991,.F.);
#14603=EDGE_CURVE('',#11177,#11178,#8666,.T.);
#14604=EDGE_CURVE('',#11175,#11177,#2992,.F.);
#14605=EDGE_CURVE('',#11178,#11176,#2993,.F.);
#14606=EDGE_CURVE('',#11179,#11180,#8667,.T.);
#14607=EDGE_CURVE('',#11177,#11179,#2994,.F.);
#14608=EDGE_CURVE('',#11180,#11178,#2995,.F.);
#14609=EDGE_CURVE('',#11181,#11182,#8668,.T.);
#14610=EDGE_CURVE('',#11179,#11181,#2996,.F.);
#14611=EDGE_CURVE('',#11182,#11180,#2997,.F.);
#14612=EDGE_CURVE('',#11183,#11184,#8669,.T.);
#14613=EDGE_CURVE('',#11181,#11183,#2998,.F.);
#14614=EDGE_CURVE('',#11184,#11182,#2999,.F.);
#14615=EDGE_CURVE('',#11185,#11186,#8670,.T.);
#14616=EDGE_CURVE('',#11183,#11185,#3000,.F.);
#14617=EDGE_CURVE('',#11186,#11184,#3001,.F.);
#14618=EDGE_CURVE('',#11187,#11188,#8671,.T.);
#14619=EDGE_CURVE('',#11185,#11187,#3002,.F.);
#14620=EDGE_CURVE('',#11188,#11186,#3003,.F.);
#14621=EDGE_CURVE('',#11189,#11190,#8672,.T.);
#14622=EDGE_CURVE('',#11187,#11189,#3004,.F.);
#14623=EDGE_CURVE('',#11190,#11188,#3005,.F.);
#14624=EDGE_CURVE('',#11191,#11192,#8673,.T.);
#14625=EDGE_CURVE('',#11189,#11191,#3006,.F.);
#14626=EDGE_CURVE('',#11192,#11190,#3007,.F.);
#14627=EDGE_CURVE('',#11193,#11194,#8674,.T.);
#14628=EDGE_CURVE('',#11191,#11193,#3008,.F.);
#14629=EDGE_CURVE('',#11194,#11192,#3009,.F.);
#14630=EDGE_CURVE('',#11195,#11196,#8675,.T.);
#14631=EDGE_CURVE('',#11193,#11195,#3010,.F.);
#14632=EDGE_CURVE('',#11196,#11194,#3011,.F.);
#14633=EDGE_CURVE('',#11197,#11198,#8676,.T.);
#14634=EDGE_CURVE('',#11195,#11197,#3012,.F.);
#14635=EDGE_CURVE('',#11198,#11196,#3013,.F.);
#14636=EDGE_CURVE('',#11199,#11200,#8677,.T.);
#14637=EDGE_CURVE('',#11197,#11199,#3014,.F.);
#14638=EDGE_CURVE('',#11200,#11198,#3015,.F.);
#14639=EDGE_CURVE('',#11201,#11202,#8678,.T.);
#14640=EDGE_CURVE('',#11199,#11201,#3016,.F.);
#14641=EDGE_CURVE('',#11202,#11200,#3017,.F.);
#14642=EDGE_CURVE('',#11203,#11204,#8679,.T.);
#14643=EDGE_CURVE('',#11201,#11203,#3018,.F.);
#14644=EDGE_CURVE('',#11204,#11202,#3019,.F.);
#14645=EDGE_CURVE('',#11205,#11206,#8680,.T.);
#14646=EDGE_CURVE('',#11203,#11205,#3020,.F.);
#14647=EDGE_CURVE('',#11206,#11204,#3021,.F.);
#14648=EDGE_CURVE('',#11207,#11208,#8681,.T.);
#14649=EDGE_CURVE('',#11205,#11207,#3022,.F.);
#14650=EDGE_CURVE('',#11208,#11206,#3023,.F.);
#14651=EDGE_CURVE('',#11209,#11210,#8682,.T.);
#14652=EDGE_CURVE('',#11207,#11209,#3024,.F.);
#14653=EDGE_CURVE('',#11210,#11208,#3025,.F.);
#14654=EDGE_CURVE('',#11211,#11212,#8683,.T.);
#14655=EDGE_CURVE('',#11209,#11211,#3026,.F.);
#14656=EDGE_CURVE('',#11212,#11210,#3027,.F.);
#14657=EDGE_CURVE('',#11213,#11214,#8684,.T.);
#14658=EDGE_CURVE('',#11211,#11213,#3028,.F.);
#14659=EDGE_CURVE('',#11214,#11212,#3029,.F.);
#14660=EDGE_CURVE('',#11215,#11216,#8685,.T.);
#14661=EDGE_CURVE('',#11215,#11217,#3030,.F.);
#14662=EDGE_CURVE('',#11216,#11217,#3437,.T.);
#14663=EDGE_CURVE('',#11218,#11217,#8686,.T.);
#14664=EDGE_CURVE('',#11219,#11218,#3031,.F.);
#14665=EDGE_CURVE('',#11217,#11219,#3438,.T.);
#14666=EDGE_CURVE('',#11220,#11221,#8687,.T.);
#14667=EDGE_CURVE('',#11218,#11220,#3032,.F.);
#14668=EDGE_CURVE('',#11217,#11221,#3033,.T.);
#14669=EDGE_CURVE('',#11222,#11223,#8688,.T.);
#14670=EDGE_CURVE('',#11220,#11222,#3034,.F.);
#14671=EDGE_CURVE('',#11221,#11223,#3035,.T.);
#14672=EDGE_CURVE('',#11224,#11225,#8689,.T.);
#14673=EDGE_CURVE('',#11222,#11224,#3036,.F.);
#14674=EDGE_CURVE('',#11223,#11225,#3037,.T.);
#14675=EDGE_CURVE('',#11226,#11227,#8690,.T.);
#14676=EDGE_CURVE('',#11224,#11226,#3038,.F.);
#14677=EDGE_CURVE('',#11225,#11227,#3039,.T.);
#14678=EDGE_CURVE('',#11228,#11229,#8691,.T.);
#14679=EDGE_CURVE('',#11226,#11228,#3040,.F.);
#14680=EDGE_CURVE('',#11227,#11229,#3041,.T.);
#14681=EDGE_CURVE('',#11230,#11231,#8692,.T.);
#14682=EDGE_CURVE('',#11228,#11230,#3042,.F.);
#14683=EDGE_CURVE('',#11229,#11231,#3043,.T.);
#14684=EDGE_CURVE('',#11232,#11233,#8693,.T.);
#14685=EDGE_CURVE('',#11230,#11232,#3044,.F.);
#14686=EDGE_CURVE('',#11231,#11233,#3045,.T.);
#14687=EDGE_CURVE('',#11234,#11235,#8694,.T.);
#14688=EDGE_CURVE('',#11232,#11234,#3046,.F.);
#14689=EDGE_CURVE('',#11233,#11235,#3047,.T.);
#14690=EDGE_CURVE('',#11236,#11237,#8695,.T.);
#14691=EDGE_CURVE('',#11234,#11236,#3048,.F.);
#14692=EDGE_CURVE('',#11235,#11237,#3049,.T.);
#14693=EDGE_CURVE('',#11238,#11239,#8696,.T.);
#14694=EDGE_CURVE('',#11236,#11238,#3050,.F.);
#14695=EDGE_CURVE('',#11237,#11239,#3051,.T.);
#14696=EDGE_CURVE('',#11240,#11241,#8697,.T.);
#14697=EDGE_CURVE('',#11238,#11240,#3052,.F.);
#14698=EDGE_CURVE('',#11239,#11241,#3053,.T.);
#14699=EDGE_CURVE('',#11242,#11243,#8698,.T.);
#14700=EDGE_CURVE('',#11240,#11242,#3054,.F.);
#14701=EDGE_CURVE('',#11241,#11243,#3055,.T.);
#14702=EDGE_CURVE('',#11244,#11245,#8699,.T.);
#14703=EDGE_CURVE('',#11242,#11244,#3056,.F.);
#14704=EDGE_CURVE('',#11243,#11245,#3057,.T.);
#14705=EDGE_CURVE('',#11246,#11247,#8700,.T.);
#14706=EDGE_CURVE('',#11244,#11246,#3058,.F.);
#14707=EDGE_CURVE('',#11245,#11247,#3059,.T.);
#14708=EDGE_CURVE('',#11248,#11249,#8701,.T.);
#14709=EDGE_CURVE('',#11246,#11248,#3060,.F.);
#14710=EDGE_CURVE('',#11247,#11249,#3061,.T.);
#14711=EDGE_CURVE('',#11250,#11251,#8702,.T.);
#14712=EDGE_CURVE('',#11248,#11250,#3062,.F.);
#14713=EDGE_CURVE('',#11249,#11251,#3063,.T.);
#14714=EDGE_CURVE('',#11252,#11253,#8703,.T.);
#14715=EDGE_CURVE('',#11250,#11252,#3064,.F.);
#14716=EDGE_CURVE('',#11251,#11253,#3065,.T.);
#14717=EDGE_CURVE('',#11254,#11255,#8704,.T.);
#14718=EDGE_CURVE('',#11252,#11254,#3066,.F.);
#14719=EDGE_CURVE('',#11253,#11255,#3067,.T.);
#14720=EDGE_CURVE('',#11256,#11257,#8705,.T.);
#14721=EDGE_CURVE('',#11254,#11256,#3068,.F.);
#14722=EDGE_CURVE('',#11255,#11257,#3069,.T.);
#14723=EDGE_CURVE('',#11258,#11259,#8706,.T.);
#14724=EDGE_CURVE('',#11256,#11258,#3070,.F.);
#14725=EDGE_CURVE('',#11257,#11259,#3071,.T.);
#14726=EDGE_CURVE('',#11260,#11261,#8707,.T.);
#14727=EDGE_CURVE('',#11258,#11260,#3072,.F.);
#14728=EDGE_CURVE('',#11259,#11261,#3073,.T.);
#14729=EDGE_CURVE('',#11262,#11263,#8708,.T.);
#14730=EDGE_CURVE('',#11260,#11262,#3074,.F.);
#14731=EDGE_CURVE('',#11261,#11263,#3075,.T.);
#14732=EDGE_CURVE('',#11264,#11265,#8709,.T.);
#14733=EDGE_CURVE('',#11262,#11264,#3076,.F.);
#14734=EDGE_CURVE('',#11263,#11265,#3077,.T.);
#14735=EDGE_CURVE('',#11266,#11267,#8710,.T.);
#14736=EDGE_CURVE('',#11264,#11266,#3078,.F.);
#14737=EDGE_CURVE('',#11265,#11267,#3079,.T.);
#14738=EDGE_CURVE('',#11268,#11269,#8711,.T.);
#14739=EDGE_CURVE('',#11266,#11268,#3080,.F.);
#14740=EDGE_CURVE('',#11267,#11269,#3081,.T.);
#14741=EDGE_CURVE('',#11270,#11271,#8712,.T.);
#14742=EDGE_CURVE('',#11268,#11270,#3082,.F.);
#14743=EDGE_CURVE('',#11269,#11271,#3083,.T.);
#14744=EDGE_CURVE('',#11272,#11273,#8713,.T.);
#14745=EDGE_CURVE('',#11270,#11272,#3084,.F.);
#14746=EDGE_CURVE('',#11271,#11273,#3085,.T.);
#14747=EDGE_CURVE('',#11274,#11275,#8714,.T.);
#14748=EDGE_CURVE('',#11272,#11274,#3086,.F.);
#14749=EDGE_CURVE('',#11273,#11275,#3087,.T.);
#14750=EDGE_CURVE('',#11276,#11277,#8715,.T.);
#14751=EDGE_CURVE('',#11274,#11276,#3088,.F.);
#14752=EDGE_CURVE('',#11275,#11277,#3089,.T.);
#14753=EDGE_CURVE('',#11277,#11278,#3090,.T.);
#14754=EDGE_CURVE('',#11276,#11278,#3439,.T.);
#14755=EDGE_CURVE('',#11219,#11216,#3440,.T.);
#14756=EDGE_CURVE('',#11219,#11279,#3091,.T.);
#14757=EDGE_CURVE('',#11279,#11280,#3441,.T.);
#14758=EDGE_CURVE('',#11280,#11215,#3092,.F.);
#14759=EDGE_CURVE('',#11280,#11214,#3093,.F.);
#14760=EDGE_CURVE('',#11213,#11279,#3094,.F.);
#14761=EDGE_CURVE('',#11281,#11282,#1522,.T.);
#14762=EDGE_CURVE('',#11282,#11283,#8716,.T.);
#14763=EDGE_CURVE('',#11283,#11284,#1523,.T.);
#14764=EDGE_CURVE('',#11281,#11284,#8717,.T.);
#14765=EDGE_CURVE('',#11285,#11286,#1524,.T.);
#14766=EDGE_CURVE('',#11286,#11287,#8718,.T.);
#14767=EDGE_CURVE('',#11287,#11288,#1525,.T.);
#14768=EDGE_CURVE('',#11285,#11288,#8719,.T.);
#14769=EDGE_CURVE('',#11289,#11290,#1526,.T.);
#14770=EDGE_CURVE('',#11290,#11291,#8720,.T.);
#14771=EDGE_CURVE('',#11291,#11292,#1527,.T.);
#14772=EDGE_CURVE('',#11289,#11292,#8721,.T.);
#14773=EDGE_CURVE('',#11293,#11294,#1528,.T.);
#14774=EDGE_CURVE('',#11294,#11295,#8722,.T.);
#14775=EDGE_CURVE('',#11295,#11296,#1529,.T.);
#14776=EDGE_CURVE('',#11293,#11296,#8723,.T.);
#14777=EDGE_CURVE('',#11297,#11298,#1530,.T.);
#14778=EDGE_CURVE('',#11298,#11299,#8724,.T.);
#14779=EDGE_CURVE('',#11299,#11300,#1531,.T.);
#14780=EDGE_CURVE('',#11297,#11300,#8725,.T.);
#14781=EDGE_CURVE('',#11301,#11302,#1532,.T.);
#14782=EDGE_CURVE('',#11302,#11303,#8726,.T.);
#14783=EDGE_CURVE('',#11303,#11304,#1533,.T.);
#14784=EDGE_CURVE('',#11301,#11304,#8727,.T.);
#14785=EDGE_CURVE('',#11305,#11306,#1534,.T.);
#14786=EDGE_CURVE('',#11306,#11307,#8728,.T.);
#14787=EDGE_CURVE('',#11307,#11308,#1535,.T.);
#14788=EDGE_CURVE('',#11305,#11308,#8729,.T.);
#14789=EDGE_CURVE('',#11309,#11310,#1536,.T.);
#14790=EDGE_CURVE('',#11310,#11311,#8730,.T.);
#14791=EDGE_CURVE('',#11311,#11312,#1537,.T.);
#14792=EDGE_CURVE('',#11309,#11312,#8731,.T.);
#14793=EDGE_CURVE('',#11313,#11314,#1538,.T.);
#14794=EDGE_CURVE('',#11314,#11315,#8732,.T.);
#14795=EDGE_CURVE('',#11315,#11316,#1539,.T.);
#14796=EDGE_CURVE('',#11313,#11316,#8733,.T.);
#14797=EDGE_CURVE('',#11317,#11318,#1540,.T.);
#14798=EDGE_CURVE('',#11318,#11319,#8734,.T.);
#14799=EDGE_CURVE('',#11319,#11320,#1541,.T.);
#14800=EDGE_CURVE('',#11317,#11320,#8735,.T.);
#14801=EDGE_CURVE('',#11321,#11322,#1542,.T.);
#14802=EDGE_CURVE('',#11322,#11323,#8736,.T.);
#14803=EDGE_CURVE('',#11323,#11324,#1543,.T.);
#14804=EDGE_CURVE('',#11321,#11324,#8737,.T.);
#14805=EDGE_CURVE('',#11325,#11326,#1544,.T.);
#14806=EDGE_CURVE('',#11326,#11327,#8738,.T.);
#14807=EDGE_CURVE('',#11327,#11328,#1545,.T.);
#14808=EDGE_CURVE('',#11325,#11328,#8739,.T.);
#14809=EDGE_CURVE('',#11329,#11330,#1546,.T.);
#14810=EDGE_CURVE('',#11330,#11331,#8740,.T.);
#14811=EDGE_CURVE('',#11331,#11332,#1547,.T.);
#14812=EDGE_CURVE('',#11329,#11332,#8741,.T.);
#14813=EDGE_CURVE('',#11333,#11334,#1548,.T.);
#14814=EDGE_CURVE('',#11334,#11335,#8742,.T.);
#14815=EDGE_CURVE('',#11335,#11336,#1549,.T.);
#14816=EDGE_CURVE('',#11333,#11336,#8743,.T.);
#14817=EDGE_CURVE('',#11337,#11338,#1550,.T.);
#14818=EDGE_CURVE('',#11338,#11339,#8744,.T.);
#14819=EDGE_CURVE('',#11339,#11340,#1551,.T.);
#14820=EDGE_CURVE('',#11337,#11340,#8745,.T.);
#14821=EDGE_CURVE('',#11341,#11342,#541,.T.);
#14822=EDGE_CURVE('',#11343,#11341,#542,.T.);
#14823=EDGE_CURVE('',#11344,#11343,#543,.T.);
#14824=EDGE_CURVE('',#11345,#11344,#544,.T.);
#14825=EDGE_CURVE('',#11346,#11345,#545,.T.);
#14826=EDGE_CURVE('',#11347,#11346,#546,.T.);
#14827=EDGE_CURVE('',#11342,#11347,#547,.T.);
#14828=EDGE_CURVE('',#11342,#11348,#8746,.T.);
#14829=EDGE_CURVE('',#11348,#11348,#3442,.T.);
#14830=EDGE_CURVE('',#11349,#11349,#3443,.T.);
#14831=EDGE_CURVE('',#11349,#11350,#3444,.T.);
#14832=EDGE_CURVE('',#11350,#11350,#3445,.T.);
#14833=EDGE_CURVE('',#11351,#11352,#3095,.T.);
#14834=EDGE_CURVE('',#11353,#11351,#548,.T.);
#14835=EDGE_CURVE('',#11354,#11353,#3446,.T.);
#14836=EDGE_CURVE('',#11355,#11354,#549,.T.);
#14837=EDGE_CURVE('',#11356,#11355,#1552,.T.);
#14838=EDGE_CURVE('',#11357,#11356,#550,.T.);
#14839=EDGE_CURVE('',#11358,#11357,#3447,.T.);
#14840=EDGE_CURVE('',#11359,#11358,#551,.T.);
#14841=EDGE_CURVE('',#11360,#11359,#1553,.T.);
#14842=EDGE_CURVE('',#11361,#11360,#552,.T.);
#14843=EDGE_CURVE('',#11362,#11361,#3448,.T.);
#14844=EDGE_CURVE('',#11363,#11362,#553,.T.);
#14845=EDGE_CURVE('',#11364,#11363,#1554,.T.);
#14846=EDGE_CURVE('',#11365,#11364,#554,.T.);
#14847=EDGE_CURVE('',#11366,#11365,#3449,.T.);
#14848=EDGE_CURVE('',#11367,#11366,#555,.T.);
#14849=EDGE_CURVE('',#11368,#11367,#1555,.T.);
#14850=EDGE_CURVE('',#11369,#11368,#556,.T.);
#14851=EDGE_CURVE('',#11370,#11369,#3450,.T.);
#14852=EDGE_CURVE('',#11371,#11370,#557,.T.);
#14853=EDGE_CURVE('',#11372,#11371,#1556,.T.);
#14854=EDGE_CURVE('',#11373,#11372,#558,.T.);
#14855=EDGE_CURVE('',#11374,#11373,#3451,.T.);
#14856=EDGE_CURVE('',#11375,#11374,#559,.T.);
#14857=EDGE_CURVE('',#11376,#11375,#1557,.T.);
#14858=EDGE_CURVE('',#11377,#11376,#560,.T.);
#14859=EDGE_CURVE('',#11378,#11377,#3452,.T.);
#14860=EDGE_CURVE('',#11379,#11378,#561,.T.);
#14861=EDGE_CURVE('',#11380,#11379,#1558,.T.);
#14862=EDGE_CURVE('',#11381,#11380,#562,.T.);
#14863=EDGE_CURVE('',#11382,#11381,#3453,.T.);
#14864=EDGE_CURVE('',#11383,#11382,#563,.T.);
#14865=EDGE_CURVE('',#11384,#11383,#1559,.T.);
#14866=EDGE_CURVE('',#11385,#11384,#564,.T.);
#14867=EDGE_CURVE('',#11386,#11385,#3454,.T.);
#14868=EDGE_CURVE('',#11387,#11386,#565,.T.);
#14869=EDGE_CURVE('',#11388,#11387,#1560,.T.);
#14870=EDGE_CURVE('',#11389,#11388,#566,.T.);
#14871=EDGE_CURVE('',#11390,#11389,#3455,.T.);
#14872=EDGE_CURVE('',#11391,#11390,#567,.T.);
#14873=EDGE_CURVE('',#11392,#11391,#1561,.T.);
#14874=EDGE_CURVE('',#11393,#11392,#568,.T.);
#14875=EDGE_CURVE('',#11394,#11393,#3456,.T.);
#14876=EDGE_CURVE('',#11395,#11394,#569,.T.);
#14877=EDGE_CURVE('',#11396,#11395,#1562,.T.);
#14878=EDGE_CURVE('',#11397,#11396,#570,.T.);
#14879=EDGE_CURVE('',#11398,#11397,#3457,.T.);
#14880=EDGE_CURVE('',#11399,#11398,#571,.T.);
#14881=EDGE_CURVE('',#11400,#11399,#1563,.T.);
#14882=EDGE_CURVE('',#11401,#11400,#572,.T.);
#14883=EDGE_CURVE('',#11402,#11401,#3458,.T.);
#14884=EDGE_CURVE('',#11403,#11402,#573,.T.);
#14885=EDGE_CURVE('',#11404,#11403,#1564,.T.);
#14886=EDGE_CURVE('',#11405,#11404,#574,.T.);
#14887=EDGE_CURVE('',#11406,#11405,#3459,.T.);
#14888=EDGE_CURVE('',#11407,#11406,#575,.T.);
#14889=EDGE_CURVE('',#11408,#11407,#1565,.T.);
#14890=EDGE_CURVE('',#11409,#11408,#576,.T.);
#14891=EDGE_CURVE('',#11410,#11409,#3460,.T.);
#14892=EDGE_CURVE('',#11411,#11410,#577,.T.);
#14893=EDGE_CURVE('',#11412,#11411,#1566,.T.);
#14894=EDGE_CURVE('',#11413,#11412,#578,.T.);
#14895=EDGE_CURVE('',#11414,#11413,#3461,.T.);
#14896=EDGE_CURVE('',#11415,#11414,#579,.T.);
#14897=EDGE_CURVE('',#11416,#11415,#1567,.T.);
#14898=EDGE_CURVE('',#11417,#11416,#580,.T.);
#14899=EDGE_CURVE('',#11418,#11417,#3462,.T.);
#14900=EDGE_CURVE('',#11419,#11418,#581,.T.);
#14901=EDGE_CURVE('',#11420,#11419,#1568,.T.);
#14902=EDGE_CURVE('',#11421,#11420,#582,.T.);
#14903=EDGE_CURVE('',#11422,#11421,#3463,.T.);
#14904=EDGE_CURVE('',#11423,#11422,#583,.T.);
#14905=EDGE_CURVE('',#11424,#11423,#1569,.T.);
#14906=EDGE_CURVE('',#11425,#11424,#584,.T.);
#14907=EDGE_CURVE('',#11426,#11425,#3464,.T.);
#14908=EDGE_CURVE('',#11427,#11426,#585,.T.);
#14909=EDGE_CURVE('',#11428,#11427,#1570,.T.);
#14910=EDGE_CURVE('',#11429,#11428,#586,.T.);
#14911=EDGE_CURVE('',#11430,#11429,#3465,.T.);
#14912=EDGE_CURVE('',#11431,#11430,#587,.T.);
#14913=EDGE_CURVE('',#11432,#11431,#1571,.T.);
#14914=EDGE_CURVE('',#11433,#11432,#588,.T.);
#14915=EDGE_CURVE('',#11434,#11433,#3466,.T.);
#14916=EDGE_CURVE('',#11435,#11434,#589,.T.);
#14917=EDGE_CURVE('',#11436,#11435,#1572,.T.);
#14918=EDGE_CURVE('',#11437,#11436,#590,.T.);
#14919=EDGE_CURVE('',#11438,#11437,#3467,.T.);
#14920=EDGE_CURVE('',#11439,#11438,#591,.T.);
#14921=EDGE_CURVE('',#11440,#11439,#1573,.T.);
#14922=EDGE_CURVE('',#11441,#11440,#592,.T.);
#14923=EDGE_CURVE('',#11442,#11441,#3468,.T.);
#14924=EDGE_CURVE('',#11443,#11442,#593,.T.);
#14925=EDGE_CURVE('',#11444,#11443,#1574,.T.);
#14926=EDGE_CURVE('',#11445,#11444,#594,.T.);
#14927=EDGE_CURVE('',#11446,#11445,#3469,.T.);
#14928=EDGE_CURVE('',#11447,#11446,#595,.T.);
#14929=EDGE_CURVE('',#11448,#11447,#1575,.T.);
#14930=EDGE_CURVE('',#11449,#11448,#596,.T.);
#14931=EDGE_CURVE('',#11450,#11449,#3470,.T.);
#14932=EDGE_CURVE('',#11451,#11450,#597,.T.);
#14933=EDGE_CURVE('',#11452,#11451,#1576,.T.);
#14934=EDGE_CURVE('',#11453,#11452,#598,.T.);
#14935=EDGE_CURVE('',#11454,#11453,#3471,.T.);
#14936=EDGE_CURVE('',#11455,#11454,#599,.T.);
#14937=EDGE_CURVE('',#11456,#11455,#1577,.T.);
#14938=EDGE_CURVE('',#11457,#11456,#600,.T.);
#14939=EDGE_CURVE('',#11458,#11457,#3472,.T.);
#14940=EDGE_CURVE('',#11459,#11458,#601,.T.);
#14941=EDGE_CURVE('',#11460,#11459,#1578,.T.);
#14942=EDGE_CURVE('',#11461,#11460,#602,.T.);
#14943=EDGE_CURVE('',#11462,#11461,#3473,.T.);
#14944=EDGE_CURVE('',#11463,#11462,#603,.T.);
#14945=EDGE_CURVE('',#11464,#11463,#1579,.T.);
#14946=EDGE_CURVE('',#11465,#11464,#604,.T.);
#14947=EDGE_CURVE('',#11466,#11465,#3474,.T.);
#14948=EDGE_CURVE('',#11467,#11466,#605,.T.);
#14949=EDGE_CURVE('',#11468,#11467,#1580,.T.);
#14950=EDGE_CURVE('',#11469,#11468,#606,.T.);
#14951=EDGE_CURVE('',#11470,#11469,#3475,.T.);
#14952=EDGE_CURVE('',#11471,#11470,#607,.T.);
#14953=EDGE_CURVE('',#11472,#11471,#1581,.T.);
#14954=EDGE_CURVE('',#11473,#11472,#608,.T.);
#14955=EDGE_CURVE('',#11474,#11473,#3476,.T.);
#14956=EDGE_CURVE('',#11475,#11474,#609,.T.);
#14957=EDGE_CURVE('',#11476,#11475,#1582,.T.);
#14958=EDGE_CURVE('',#11477,#11476,#610,.T.);
#14959=EDGE_CURVE('',#11478,#11477,#3477,.T.);
#14960=EDGE_CURVE('',#11479,#11478,#611,.T.);
#14961=EDGE_CURVE('',#11480,#11479,#1583,.T.);
#14962=EDGE_CURVE('',#11481,#11480,#612,.T.);
#14963=EDGE_CURVE('',#11482,#11481,#3478,.T.);
#14964=EDGE_CURVE('',#11483,#11482,#613,.T.);
#14965=EDGE_CURVE('',#11484,#11483,#1584,.T.);
#14966=EDGE_CURVE('',#11485,#11484,#614,.T.);
#14967=EDGE_CURVE('',#11486,#11485,#3479,.T.);
#14968=EDGE_CURVE('',#11487,#11486,#615,.T.);
#14969=EDGE_CURVE('',#11488,#11487,#1585,.T.);
#14970=EDGE_CURVE('',#11489,#11488,#616,.T.);
#14971=EDGE_CURVE('',#11490,#11489,#3480,.T.);
#14972=EDGE_CURVE('',#11491,#11490,#617,.T.);
#14973=EDGE_CURVE('',#11492,#11491,#1586,.T.);
#14974=EDGE_CURVE('',#11493,#11492,#618,.T.);
#14975=EDGE_CURVE('',#11494,#11493,#3481,.T.);
#14976=EDGE_CURVE('',#11495,#11494,#619,.T.);
#14977=EDGE_CURVE('',#11496,#11495,#1587,.T.);
#14978=EDGE_CURVE('',#11497,#11496,#620,.T.);
#14979=EDGE_CURVE('',#11498,#11497,#3482,.T.);
#14980=EDGE_CURVE('',#11499,#11498,#621,.T.);
#14981=EDGE_CURVE('',#11500,#11499,#1588,.T.);
#14982=EDGE_CURVE('',#11501,#11500,#622,.T.);
#14983=EDGE_CURVE('',#11502,#11501,#3483,.T.);
#14984=EDGE_CURVE('',#11503,#11502,#623,.T.);
#14985=EDGE_CURVE('',#11504,#11503,#1589,.T.);
#14986=EDGE_CURVE('',#11505,#11504,#624,.T.);
#14987=EDGE_CURVE('',#11506,#11505,#3484,.T.);
#14988=EDGE_CURVE('',#11507,#11506,#625,.T.);
#14989=EDGE_CURVE('',#11508,#11507,#1590,.T.);
#14990=EDGE_CURVE('',#11509,#11508,#626,.T.);
#14991=EDGE_CURVE('',#11510,#11509,#3485,.T.);
#14992=EDGE_CURVE('',#11511,#11510,#627,.T.);
#14993=EDGE_CURVE('',#11512,#11511,#1591,.T.);
#14994=EDGE_CURVE('',#11513,#11512,#628,.T.);
#14995=EDGE_CURVE('',#11514,#11513,#3486,.T.);
#14996=EDGE_CURVE('',#11515,#11514,#629,.T.);
#14997=EDGE_CURVE('',#11516,#11515,#1592,.T.);
#14998=EDGE_CURVE('',#11517,#11516,#630,.T.);
#14999=EDGE_CURVE('',#11518,#11517,#3487,.T.);
#15000=EDGE_CURVE('',#11519,#11518,#631,.T.);
#15001=EDGE_CURVE('',#11520,#11519,#1593,.T.);
#15002=EDGE_CURVE('',#11521,#11520,#632,.T.);
#15003=EDGE_CURVE('',#11522,#11521,#3488,.T.);
#15004=EDGE_CURVE('',#11523,#11522,#633,.T.);
#15005=EDGE_CURVE('',#11524,#11523,#1594,.T.);
#15006=EDGE_CURVE('',#11525,#11524,#634,.T.);
#15007=EDGE_CURVE('',#11526,#11525,#3489,.T.);
#15008=EDGE_CURVE('',#11527,#11526,#635,.T.);
#15009=EDGE_CURVE('',#11528,#11527,#1595,.T.);
#15010=EDGE_CURVE('',#11529,#11528,#636,.T.);
#15011=EDGE_CURVE('',#11530,#11529,#3490,.T.);
#15012=EDGE_CURVE('',#11531,#11530,#637,.T.);
#15013=EDGE_CURVE('',#11532,#11531,#1596,.T.);
#15014=EDGE_CURVE('',#11533,#11532,#638,.T.);
#15015=EDGE_CURVE('',#11534,#11533,#3491,.T.);
#15016=EDGE_CURVE('',#11340,#11534,#639,.T.);
#15017=EDGE_CURVE('',#11535,#11339,#640,.T.);
#15018=EDGE_CURVE('',#11536,#11535,#3492,.T.);
#15019=EDGE_CURVE('',#11336,#11536,#641,.T.);
#15020=EDGE_CURVE('',#11537,#11335,#642,.T.);
#15021=EDGE_CURVE('',#11538,#11537,#3493,.T.);
#15022=EDGE_CURVE('',#11332,#11538,#643,.T.);
#15023=EDGE_CURVE('',#11539,#11331,#644,.T.);
#15024=EDGE_CURVE('',#11540,#11539,#3494,.T.);
#15025=EDGE_CURVE('',#11328,#11540,#645,.T.);
#15026=EDGE_CURVE('',#11541,#11327,#646,.T.);
#15027=EDGE_CURVE('',#11542,#11541,#3495,.T.);
#15028=EDGE_CURVE('',#11324,#11542,#647,.T.);
#15029=EDGE_CURVE('',#11543,#11323,#648,.T.);
#15030=EDGE_CURVE('',#11544,#11543,#3496,.T.);
#15031=EDGE_CURVE('',#11320,#11544,#649,.T.);
#15032=EDGE_CURVE('',#11545,#11319,#650,.T.);
#15033=EDGE_CURVE('',#11546,#11545,#3497,.T.);
#15034=EDGE_CURVE('',#11316,#11546,#651,.T.);
#15035=EDGE_CURVE('',#11547,#11315,#652,.T.);
#15036=EDGE_CURVE('',#11548,#11547,#3498,.T.);
#15037=EDGE_CURVE('',#11312,#11548,#653,.T.);
#15038=EDGE_CURVE('',#11549,#11311,#654,.T.);
#15039=EDGE_CURVE('',#11550,#11549,#3499,.T.);
#15040=EDGE_CURVE('',#11308,#11550,#655,.T.);
#15041=EDGE_CURVE('',#11551,#11307,#656,.T.);
#15042=EDGE_CURVE('',#11552,#11551,#3500,.T.);
#15043=EDGE_CURVE('',#11284,#11552,#657,.T.);
#15044=EDGE_CURVE('',#11553,#11283,#658,.T.);
#15045=EDGE_CURVE('',#11554,#11553,#3501,.T.);
#15046=EDGE_CURVE('',#11288,#11554,#659,.T.);
#15047=EDGE_CURVE('',#11555,#11287,#660,.T.);
#15048=EDGE_CURVE('',#11556,#11555,#3502,.T.);
#15049=EDGE_CURVE('',#11292,#11556,#661,.T.);
#15050=EDGE_CURVE('',#11557,#11291,#662,.T.);
#15051=EDGE_CURVE('',#11558,#11557,#3503,.T.);
#15052=EDGE_CURVE('',#11296,#11558,#663,.T.);
#15053=EDGE_CURVE('',#11559,#11295,#664,.T.);
#15054=EDGE_CURVE('',#11560,#11559,#3504,.T.);
#15055=EDGE_CURVE('',#11300,#11560,#665,.T.);
#15056=EDGE_CURVE('',#11561,#11299,#666,.T.);
#15057=EDGE_CURVE('',#11562,#11561,#3505,.T.);
#15058=EDGE_CURVE('',#11304,#11562,#667,.T.);
#15059=EDGE_CURVE('',#11563,#11303,#668,.T.);
#15060=EDGE_CURVE('',#11564,#11563,#3506,.T.);
#15061=EDGE_CURVE('',#11565,#11564,#669,.T.);
#15062=EDGE_CURVE('',#11566,#11565,#1597,.T.);
#15063=EDGE_CURVE('',#11567,#11566,#670,.T.);
#15064=EDGE_CURVE('',#11568,#11567,#3507,.T.);
#15065=EDGE_CURVE('',#11569,#11568,#671,.T.);
#15066=EDGE_CURVE('',#11570,#11569,#1598,.T.);
#15067=EDGE_CURVE('',#11571,#11570,#672,.T.);
#15068=EDGE_CURVE('',#11572,#11571,#3508,.T.);
#15069=EDGE_CURVE('',#11573,#11572,#673,.T.);
#15070=EDGE_CURVE('',#11574,#11573,#1599,.T.);
#15071=EDGE_CURVE('',#11575,#11574,#674,.T.);
#15072=EDGE_CURVE('',#11576,#11575,#3509,.T.);
#15073=EDGE_CURVE('',#11577,#11576,#675,.T.);
#15074=EDGE_CURVE('',#11578,#11577,#1600,.T.);
#15075=EDGE_CURVE('',#11579,#11578,#676,.T.);
#15076=EDGE_CURVE('',#11580,#11579,#3510,.T.);
#15077=EDGE_CURVE('',#11581,#11580,#677,.T.);
#15078=EDGE_CURVE('',#11582,#11581,#1601,.T.);
#15079=EDGE_CURVE('',#11583,#11582,#678,.T.);
#15080=EDGE_CURVE('',#11584,#11583,#3511,.T.);
#15081=EDGE_CURVE('',#11585,#11584,#679,.T.);
#15082=EDGE_CURVE('',#11586,#11585,#1602,.T.);
#15083=EDGE_CURVE('',#11587,#11586,#680,.T.);
#15084=EDGE_CURVE('',#11588,#11587,#3512,.T.);
#15085=EDGE_CURVE('',#11589,#11588,#681,.T.);
#15086=EDGE_CURVE('',#11590,#11589,#1603,.T.);
#15087=EDGE_CURVE('',#11591,#11590,#682,.T.);
#15088=EDGE_CURVE('',#11592,#11591,#3513,.T.);
#15089=EDGE_CURVE('',#11593,#11592,#683,.T.);
#15090=EDGE_CURVE('',#11594,#11593,#1604,.T.);
#15091=EDGE_CURVE('',#11595,#11594,#684,.T.);
#15092=EDGE_CURVE('',#11596,#11595,#3514,.T.);
#15093=EDGE_CURVE('',#11597,#11596,#685,.T.);
#15094=EDGE_CURVE('',#11598,#11597,#1605,.T.);
#15095=EDGE_CURVE('',#11599,#11598,#686,.T.);
#15096=EDGE_CURVE('',#11600,#11599,#3515,.T.);
#15097=EDGE_CURVE('',#11601,#11600,#687,.T.);
#15098=EDGE_CURVE('',#11602,#11601,#1606,.T.);
#15099=EDGE_CURVE('',#11603,#11602,#688,.T.);
#15100=EDGE_CURVE('',#11604,#11603,#3516,.T.);
#15101=EDGE_CURVE('',#11605,#11604,#689,.T.);
#15102=EDGE_CURVE('',#11606,#11605,#1607,.T.);
#15103=EDGE_CURVE('',#11607,#11606,#690,.T.);
#15104=EDGE_CURVE('',#11608,#11607,#3517,.T.);
#15105=EDGE_CURVE('',#11609,#11608,#691,.T.);
#15106=EDGE_CURVE('',#11610,#11609,#1608,.T.);
#15107=EDGE_CURVE('',#11611,#11610,#692,.T.);
#15108=EDGE_CURVE('',#11612,#11611,#3518,.T.);
#15109=EDGE_CURVE('',#11613,#11612,#693,.T.);
#15110=EDGE_CURVE('',#11614,#11613,#1609,.T.);
#15111=EDGE_CURVE('',#11615,#11614,#694,.T.);
#15112=EDGE_CURVE('',#11616,#11615,#3519,.T.);
#15113=EDGE_CURVE('',#11617,#11616,#695,.T.);
#15114=EDGE_CURVE('',#11618,#11617,#1610,.T.);
#15115=EDGE_CURVE('',#11619,#11618,#696,.T.);
#15116=EDGE_CURVE('',#11620,#11619,#3520,.T.);
#15117=EDGE_CURVE('',#11621,#11620,#697,.T.);
#15118=EDGE_CURVE('',#11622,#11621,#1611,.T.);
#15119=EDGE_CURVE('',#11623,#11622,#698,.T.);
#15120=EDGE_CURVE('',#11624,#11623,#3521,.T.);
#15121=EDGE_CURVE('',#11625,#11624,#699,.T.);
#15122=EDGE_CURVE('',#11626,#11625,#1612,.T.);
#15123=EDGE_CURVE('',#11627,#11626,#700,.T.);
#15124=EDGE_CURVE('',#11628,#11627,#3522,.T.);
#15125=EDGE_CURVE('',#11629,#11628,#701,.T.);
#15126=EDGE_CURVE('',#11630,#11629,#1613,.T.);
#15127=EDGE_CURVE('',#11631,#11630,#702,.T.);
#15128=EDGE_CURVE('',#11632,#11631,#3523,.T.);
#15129=EDGE_CURVE('',#11633,#11632,#703,.T.);
#15130=EDGE_CURVE('',#11634,#11633,#1614,.T.);
#15131=EDGE_CURVE('',#11635,#11634,#704,.T.);
#15132=EDGE_CURVE('',#11636,#11635,#3524,.T.);
#15133=EDGE_CURVE('',#11637,#11636,#705,.T.);
#15134=EDGE_CURVE('',#11638,#11637,#1615,.T.);
#15135=EDGE_CURVE('',#11639,#11638,#706,.T.);
#15136=EDGE_CURVE('',#11640,#11639,#3525,.T.);
#15137=EDGE_CURVE('',#11641,#11640,#707,.T.);
#15138=EDGE_CURVE('',#11352,#11641,#3096,.T.);
#15139=EDGE_CURVE('',#11352,#11349,#8747,.T.);
#15140=EDGE_CURVE('',#11642,#11643,#3097,.T.);
#15141=EDGE_CURVE('',#11644,#11642,#708,.T.);
#15142=EDGE_CURVE('',#11644,#11645,#3526,.T.);
#15143=EDGE_CURVE('',#11646,#11645,#709,.T.);
#15144=EDGE_CURVE('',#11647,#11646,#1616,.T.);
#15145=EDGE_CURVE('',#11648,#11647,#710,.T.);
#15146=EDGE_CURVE('',#11648,#11649,#3527,.T.);
#15147=EDGE_CURVE('',#11650,#11649,#711,.T.);
#15148=EDGE_CURVE('',#11651,#11650,#1617,.T.);
#15149=EDGE_CURVE('',#11652,#11651,#712,.T.);
#15150=EDGE_CURVE('',#11652,#11653,#3528,.T.);
#15151=EDGE_CURVE('',#11654,#11653,#713,.T.);
#15152=EDGE_CURVE('',#11655,#11654,#1618,.T.);
#15153=EDGE_CURVE('',#11656,#11655,#714,.T.);
#15154=EDGE_CURVE('',#11656,#11657,#3529,.T.);
#15155=EDGE_CURVE('',#11658,#11657,#715,.T.);
#15156=EDGE_CURVE('',#11659,#11658,#1619,.T.);
#15157=EDGE_CURVE('',#11660,#11659,#716,.T.);
#15158=EDGE_CURVE('',#11660,#11661,#3530,.T.);
#15159=EDGE_CURVE('',#11662,#11661,#717,.T.);
#15160=EDGE_CURVE('',#11663,#11662,#1620,.T.);
#15161=EDGE_CURVE('',#11664,#11663,#718,.T.);
#15162=EDGE_CURVE('',#11664,#11665,#3531,.T.);
#15163=EDGE_CURVE('',#11666,#11665,#719,.T.);
#15164=EDGE_CURVE('',#11667,#11666,#1621,.T.);
#15165=EDGE_CURVE('',#11668,#11667,#720,.T.);
#15166=EDGE_CURVE('',#11668,#11669,#3532,.T.);
#15167=EDGE_CURVE('',#11670,#11669,#721,.T.);
#15168=EDGE_CURVE('',#11671,#11670,#1622,.T.);
#15169=EDGE_CURVE('',#11672,#11671,#722,.T.);
#15170=EDGE_CURVE('',#11672,#11673,#3533,.T.);
#15171=EDGE_CURVE('',#11674,#11673,#723,.T.);
#15172=EDGE_CURVE('',#11675,#11674,#1623,.T.);
#15173=EDGE_CURVE('',#11676,#11675,#724,.T.);
#15174=EDGE_CURVE('',#11676,#11677,#3534,.T.);
#15175=EDGE_CURVE('',#11678,#11677,#725,.T.);
#15176=EDGE_CURVE('',#11679,#11678,#1624,.T.);
#15177=EDGE_CURVE('',#11680,#11679,#726,.T.);
#15178=EDGE_CURVE('',#11680,#11681,#3535,.T.);
#15179=EDGE_CURVE('',#11682,#11681,#727,.T.);
#15180=EDGE_CURVE('',#11683,#11682,#1625,.T.);
#15181=EDGE_CURVE('',#11684,#11683,#728,.T.);
#15182=EDGE_CURVE('',#11684,#11685,#3536,.T.);
#15183=EDGE_CURVE('',#11686,#11685,#729,.T.);
#15184=EDGE_CURVE('',#11687,#11686,#1626,.T.);
#15185=EDGE_CURVE('',#11688,#11687,#730,.T.);
#15186=EDGE_CURVE('',#11688,#11689,#3537,.T.);
#15187=EDGE_CURVE('',#11690,#11689,#731,.T.);
#15188=EDGE_CURVE('',#11691,#11690,#1627,.T.);
#15189=EDGE_CURVE('',#11692,#11691,#732,.T.);
#15190=EDGE_CURVE('',#11692,#11693,#3538,.T.);
#15191=EDGE_CURVE('',#11694,#11693,#733,.T.);
#15192=EDGE_CURVE('',#11695,#11694,#1628,.T.);
#15193=EDGE_CURVE('',#11696,#11695,#734,.T.);
#15194=EDGE_CURVE('',#11696,#11697,#3539,.T.);
#15195=EDGE_CURVE('',#11698,#11697,#735,.T.);
#15196=EDGE_CURVE('',#11699,#11698,#1629,.T.);
#15197=EDGE_CURVE('',#11700,#11699,#736,.T.);
#15198=EDGE_CURVE('',#11700,#11701,#3540,.T.);
#15199=EDGE_CURVE('',#11702,#11701,#737,.T.);
#15200=EDGE_CURVE('',#11703,#11702,#1630,.T.);
#15201=EDGE_CURVE('',#11704,#11703,#738,.T.);
#15202=EDGE_CURVE('',#11704,#11705,#3541,.T.);
#15203=EDGE_CURVE('',#11706,#11705,#739,.T.);
#15204=EDGE_CURVE('',#11707,#11706,#1631,.T.);
#15205=EDGE_CURVE('',#11708,#11707,#740,.T.);
#15206=EDGE_CURVE('',#11708,#11709,#3542,.T.);
#15207=EDGE_CURVE('',#11710,#11709,#741,.T.);
#15208=EDGE_CURVE('',#11711,#11710,#1632,.T.);
#15209=EDGE_CURVE('',#11712,#11711,#742,.T.);
#15210=EDGE_CURVE('',#11712,#11713,#3543,.T.);
#15211=EDGE_CURVE('',#11714,#11713,#743,.T.);
#15212=EDGE_CURVE('',#11715,#11714,#1633,.T.);
#15213=EDGE_CURVE('',#11716,#11715,#744,.T.);
#15214=EDGE_CURVE('',#11716,#11717,#3544,.T.);
#15215=EDGE_CURVE('',#11718,#11717,#745,.T.);
#15216=EDGE_CURVE('',#11719,#11718,#1634,.T.);
#15217=EDGE_CURVE('',#11720,#11719,#746,.T.);
#15218=EDGE_CURVE('',#11720,#11721,#3545,.T.);
#15219=EDGE_CURVE('',#11722,#11721,#747,.T.);
#15220=EDGE_CURVE('',#11723,#11722,#1635,.T.);
#15221=EDGE_CURVE('',#11724,#11723,#748,.T.);
#15222=EDGE_CURVE('',#11724,#11725,#3546,.T.);
#15223=EDGE_CURVE('',#11726,#11725,#749,.T.);
#15224=EDGE_CURVE('',#11727,#11726,#1636,.T.);
#15225=EDGE_CURVE('',#11728,#11727,#750,.T.);
#15226=EDGE_CURVE('',#11728,#11729,#3547,.T.);
#15227=EDGE_CURVE('',#11730,#11729,#751,.T.);
#15228=EDGE_CURVE('',#11731,#11730,#1637,.T.);
#15229=EDGE_CURVE('',#11732,#11731,#752,.T.);
#15230=EDGE_CURVE('',#11732,#11733,#3548,.T.);
#15231=EDGE_CURVE('',#11734,#11733,#753,.T.);
#15232=EDGE_CURVE('',#11735,#11734,#1638,.T.);
#15233=EDGE_CURVE('',#11736,#11735,#754,.T.);
#15234=EDGE_CURVE('',#11736,#11737,#3549,.T.);
#15235=EDGE_CURVE('',#11738,#11737,#755,.T.);
#15236=EDGE_CURVE('',#11739,#11738,#1639,.T.);
#15237=EDGE_CURVE('',#11740,#11739,#756,.T.);
#15238=EDGE_CURVE('',#11740,#11741,#3550,.T.);
#15239=EDGE_CURVE('',#11742,#11741,#757,.T.);
#15240=EDGE_CURVE('',#11743,#11742,#1640,.T.);
#15241=EDGE_CURVE('',#11744,#11743,#758,.T.);
#15242=EDGE_CURVE('',#11744,#11745,#3551,.T.);
#15243=EDGE_CURVE('',#11746,#11745,#759,.T.);
#15244=EDGE_CURVE('',#11747,#11746,#1641,.T.);
#15245=EDGE_CURVE('',#11748,#11747,#760,.T.);
#15246=EDGE_CURVE('',#11748,#11749,#3552,.T.);
#15247=EDGE_CURVE('',#11750,#11749,#761,.T.);
#15248=EDGE_CURVE('',#11751,#11750,#1642,.T.);
#15249=EDGE_CURVE('',#11752,#11751,#762,.T.);
#15250=EDGE_CURVE('',#11752,#11753,#3553,.T.);
#15251=EDGE_CURVE('',#11754,#11753,#763,.T.);
#15252=EDGE_CURVE('',#11755,#11754,#1643,.T.);
#15253=EDGE_CURVE('',#11756,#11755,#764,.T.);
#15254=EDGE_CURVE('',#11756,#11757,#3554,.T.);
#15255=EDGE_CURVE('',#11758,#11757,#765,.T.);
#15256=EDGE_CURVE('',#11759,#11758,#1644,.T.);
#15257=EDGE_CURVE('',#11760,#11759,#766,.T.);
#15258=EDGE_CURVE('',#11760,#11761,#3555,.T.);
#15259=EDGE_CURVE('',#11762,#11761,#767,.T.);
#15260=EDGE_CURVE('',#11763,#11762,#1645,.T.);
#15261=EDGE_CURVE('',#11764,#11763,#768,.T.);
#15262=EDGE_CURVE('',#11764,#11765,#3556,.T.);
#15263=EDGE_CURVE('',#11766,#11765,#769,.T.);
#15264=EDGE_CURVE('',#11767,#11766,#1646,.T.);
#15265=EDGE_CURVE('',#11768,#11767,#770,.T.);
#15266=EDGE_CURVE('',#11768,#11769,#3557,.T.);
#15267=EDGE_CURVE('',#11770,#11769,#771,.T.);
#15268=EDGE_CURVE('',#11771,#11770,#1647,.T.);
#15269=EDGE_CURVE('',#11772,#11771,#772,.T.);
#15270=EDGE_CURVE('',#11772,#11773,#3558,.T.);
#15271=EDGE_CURVE('',#11774,#11773,#773,.T.);
#15272=EDGE_CURVE('',#11775,#11774,#1648,.T.);
#15273=EDGE_CURVE('',#11776,#11775,#774,.T.);
#15274=EDGE_CURVE('',#11776,#11777,#3559,.T.);
#15275=EDGE_CURVE('',#11778,#11777,#775,.T.);
#15276=EDGE_CURVE('',#11779,#11778,#1649,.T.);
#15277=EDGE_CURVE('',#11780,#11779,#776,.T.);
#15278=EDGE_CURVE('',#11780,#11781,#3560,.T.);
#15279=EDGE_CURVE('',#11782,#11781,#777,.T.);
#15280=EDGE_CURVE('',#11783,#11782,#1650,.T.);
#15281=EDGE_CURVE('',#11784,#11783,#778,.T.);
#15282=EDGE_CURVE('',#11784,#11785,#3561,.T.);
#15283=EDGE_CURVE('',#11786,#11785,#779,.T.);
#15284=EDGE_CURVE('',#11787,#11786,#1651,.T.);
#15285=EDGE_CURVE('',#11788,#11787,#780,.T.);
#15286=EDGE_CURVE('',#11788,#11789,#3562,.T.);
#15287=EDGE_CURVE('',#11790,#11789,#781,.T.);
#15288=EDGE_CURVE('',#11791,#11790,#1652,.T.);
#15289=EDGE_CURVE('',#11792,#11791,#782,.T.);
#15290=EDGE_CURVE('',#11792,#11793,#3563,.T.);
#15291=EDGE_CURVE('',#11794,#11793,#783,.T.);
#15292=EDGE_CURVE('',#11795,#11794,#1653,.T.);
#15293=EDGE_CURVE('',#11796,#11795,#784,.T.);
#15294=EDGE_CURVE('',#11796,#11797,#3564,.T.);
#15295=EDGE_CURVE('',#11798,#11797,#785,.T.);
#15296=EDGE_CURVE('',#11799,#11798,#1654,.T.);
#15297=EDGE_CURVE('',#11800,#11799,#786,.T.);
#15298=EDGE_CURVE('',#11800,#11801,#3565,.T.);
#15299=EDGE_CURVE('',#11802,#11801,#787,.T.);
#15300=EDGE_CURVE('',#11803,#11802,#1655,.T.);
#15301=EDGE_CURVE('',#11804,#11803,#788,.T.);
#15302=EDGE_CURVE('',#11804,#11805,#3566,.T.);
#15303=EDGE_CURVE('',#11806,#11805,#789,.T.);
#15304=EDGE_CURVE('',#11807,#11806,#1656,.T.);
#15305=EDGE_CURVE('',#11808,#11807,#790,.T.);
#15306=EDGE_CURVE('',#11808,#11809,#3567,.T.);
#15307=EDGE_CURVE('',#11810,#11809,#791,.T.);
#15308=EDGE_CURVE('',#11811,#11810,#1657,.T.);
#15309=EDGE_CURVE('',#11812,#11811,#792,.T.);
#15310=EDGE_CURVE('',#11812,#11813,#3568,.T.);
#15311=EDGE_CURVE('',#11814,#11813,#793,.T.);
#15312=EDGE_CURVE('',#11815,#11814,#1658,.T.);
#15313=EDGE_CURVE('',#11816,#11815,#794,.T.);
#15314=EDGE_CURVE('',#11816,#11817,#3569,.T.);
#15315=EDGE_CURVE('',#11818,#11817,#795,.T.);
#15316=EDGE_CURVE('',#11819,#11818,#1659,.T.);
#15317=EDGE_CURVE('',#11820,#11819,#796,.T.);
#15318=EDGE_CURVE('',#11820,#11821,#3570,.T.);
#15319=EDGE_CURVE('',#11822,#11821,#797,.T.);
#15320=EDGE_CURVE('',#11823,#11822,#1660,.T.);
#15321=EDGE_CURVE('',#11824,#11823,#798,.T.);
#15322=EDGE_CURVE('',#11824,#11825,#3571,.T.);
#15323=EDGE_CURVE('',#11826,#11825,#799,.T.);
#15324=EDGE_CURVE('',#11827,#11826,#1661,.T.);
#15325=EDGE_CURVE('',#11828,#11827,#800,.T.);
#15326=EDGE_CURVE('',#11828,#11829,#3572,.T.);
#15327=EDGE_CURVE('',#11830,#11829,#801,.T.);
#15328=EDGE_CURVE('',#11831,#11830,#1662,.T.);
#15329=EDGE_CURVE('',#11832,#11831,#802,.T.);
#15330=EDGE_CURVE('',#11832,#11833,#3573,.T.);
#15331=EDGE_CURVE('',#11834,#11833,#803,.T.);
#15332=EDGE_CURVE('',#11835,#11834,#1663,.T.);
#15333=EDGE_CURVE('',#11836,#11835,#804,.T.);
#15334=EDGE_CURVE('',#11836,#11837,#3574,.T.);
#15335=EDGE_CURVE('',#11838,#11837,#805,.T.);
#15336=EDGE_CURVE('',#11839,#11838,#1664,.T.);
#15337=EDGE_CURVE('',#11840,#11839,#806,.T.);
#15338=EDGE_CURVE('',#11840,#11841,#3575,.T.);
#15339=EDGE_CURVE('',#11842,#11841,#807,.T.);
#15340=EDGE_CURVE('',#11843,#11842,#1665,.T.);
#15341=EDGE_CURVE('',#11844,#11843,#808,.T.);
#15342=EDGE_CURVE('',#11844,#11845,#3576,.T.);
#15343=EDGE_CURVE('',#11846,#11845,#809,.T.);
#15344=EDGE_CURVE('',#11847,#11846,#1666,.T.);
#15345=EDGE_CURVE('',#11848,#11847,#810,.T.);
#15346=EDGE_CURVE('',#11848,#11849,#3577,.T.);
#15347=EDGE_CURVE('',#11850,#11849,#811,.T.);
#15348=EDGE_CURVE('',#11851,#11850,#1667,.T.);
#15349=EDGE_CURVE('',#11852,#11851,#812,.T.);
#15350=EDGE_CURVE('',#11852,#11853,#3578,.T.);
#15351=EDGE_CURVE('',#11854,#11853,#813,.T.);
#15352=EDGE_CURVE('',#11855,#11854,#1668,.T.);
#15353=EDGE_CURVE('',#11856,#11855,#814,.T.);
#15354=EDGE_CURVE('',#11856,#11857,#3579,.T.);
#15355=EDGE_CURVE('',#11858,#11857,#815,.T.);
#15356=EDGE_CURVE('',#11859,#11858,#1669,.T.);
#15357=EDGE_CURVE('',#11860,#11859,#816,.T.);
#15358=EDGE_CURVE('',#11860,#11861,#3580,.T.);
#15359=EDGE_CURVE('',#11862,#11861,#817,.T.);
#15360=EDGE_CURVE('',#11863,#11862,#1670,.T.);
#15361=EDGE_CURVE('',#11864,#11863,#818,.T.);
#15362=EDGE_CURVE('',#11864,#11865,#3581,.T.);
#15363=EDGE_CURVE('',#11866,#11865,#819,.T.);
#15364=EDGE_CURVE('',#11867,#11866,#1671,.T.);
#15365=EDGE_CURVE('',#11868,#11867,#820,.T.);
#15366=EDGE_CURVE('',#11868,#11869,#3582,.T.);
#15367=EDGE_CURVE('',#11870,#11869,#821,.T.);
#15368=EDGE_CURVE('',#11871,#11870,#1672,.T.);
#15369=EDGE_CURVE('',#11872,#11871,#822,.T.);
#15370=EDGE_CURVE('',#11872,#11873,#3583,.T.);
#15371=EDGE_CURVE('',#11874,#11873,#823,.T.);
#15372=EDGE_CURVE('',#11875,#11874,#1673,.T.);
#15373=EDGE_CURVE('',#11876,#11875,#824,.T.);
#15374=EDGE_CURVE('',#11876,#11877,#3584,.T.);
#15375=EDGE_CURVE('',#11878,#11877,#825,.T.);
#15376=EDGE_CURVE('',#11879,#11878,#1674,.T.);
#15377=EDGE_CURVE('',#11880,#11879,#826,.T.);
#15378=EDGE_CURVE('',#11880,#11881,#3585,.T.);
#15379=EDGE_CURVE('',#11302,#11881,#827,.T.);
#15380=EDGE_CURVE('',#11882,#11301,#828,.T.);
#15381=EDGE_CURVE('',#11882,#11883,#3586,.T.);
#15382=EDGE_CURVE('',#11298,#11883,#829,.T.);
#15383=EDGE_CURVE('',#11884,#11297,#830,.T.);
#15384=EDGE_CURVE('',#11884,#11885,#3587,.T.);
#15385=EDGE_CURVE('',#11294,#11885,#831,.T.);
#15386=EDGE_CURVE('',#11886,#11293,#832,.T.);
#15387=EDGE_CURVE('',#11886,#11887,#3588,.T.);
#15388=EDGE_CURVE('',#11290,#11887,#833,.T.);
#15389=EDGE_CURVE('',#11888,#11289,#834,.T.);
#15390=EDGE_CURVE('',#11888,#11889,#3589,.T.);
#15391=EDGE_CURVE('',#11286,#11889,#835,.T.);
#15392=EDGE_CURVE('',#11890,#11285,#836,.T.);
#15393=EDGE_CURVE('',#11890,#11891,#3590,.T.);
#15394=EDGE_CURVE('',#11282,#11891,#837,.T.);
#15395=EDGE_CURVE('',#11892,#11281,#838,.T.);
#15396=EDGE_CURVE('',#11892,#11893,#3591,.T.);
#15397=EDGE_CURVE('',#11306,#11893,#839,.T.);
#15398=EDGE_CURVE('',#11894,#11305,#840,.T.);
#15399=EDGE_CURVE('',#11894,#11895,#3592,.T.);
#15400=EDGE_CURVE('',#11310,#11895,#841,.T.);
#15401=EDGE_CURVE('',#11896,#11309,#842,.T.);
#15402=EDGE_CURVE('',#11896,#11897,#3593,.T.);
#15403=EDGE_CURVE('',#11314,#11897,#843,.T.);
#15404=EDGE_CURVE('',#11898,#11313,#844,.T.);
#15405=EDGE_CURVE('',#11898,#11899,#3594,.T.);
#15406=EDGE_CURVE('',#11318,#11899,#845,.T.);
#15407=EDGE_CURVE('',#11900,#11317,#846,.T.);
#15408=EDGE_CURVE('',#11900,#11901,#3595,.T.);
#15409=EDGE_CURVE('',#11322,#11901,#847,.T.);
#15410=EDGE_CURVE('',#11902,#11321,#848,.T.);
#15411=EDGE_CURVE('',#11902,#11903,#3596,.T.);
#15412=EDGE_CURVE('',#11326,#11903,#849,.T.);
#15413=EDGE_CURVE('',#11904,#11325,#850,.T.);
#15414=EDGE_CURVE('',#11904,#11905,#3597,.T.);
#15415=EDGE_CURVE('',#11330,#11905,#851,.T.);
#15416=EDGE_CURVE('',#11906,#11329,#852,.T.);
#15417=EDGE_CURVE('',#11906,#11907,#3598,.T.);
#15418=EDGE_CURVE('',#11334,#11907,#853,.T.);
#15419=EDGE_CURVE('',#11908,#11333,#854,.T.);
#15420=EDGE_CURVE('',#11908,#11909,#3599,.T.);
#15421=EDGE_CURVE('',#11338,#11909,#855,.T.);
#15422=EDGE_CURVE('',#11910,#11337,#856,.T.);
#15423=EDGE_CURVE('',#11910,#11911,#3600,.T.);
#15424=EDGE_CURVE('',#11912,#11911,#857,.T.);
#15425=EDGE_CURVE('',#11913,#11912,#1675,.T.);
#15426=EDGE_CURVE('',#11914,#11913,#858,.T.);
#15427=EDGE_CURVE('',#11914,#11915,#3601,.T.);
#15428=EDGE_CURVE('',#11916,#11915,#859,.T.);
#15429=EDGE_CURVE('',#11917,#11916,#1676,.T.);
#15430=EDGE_CURVE('',#11918,#11917,#860,.T.);
#15431=EDGE_CURVE('',#11918,#11919,#3602,.T.);
#15432=EDGE_CURVE('',#11920,#11919,#861,.T.);
#15433=EDGE_CURVE('',#11921,#11920,#1677,.T.);
#15434=EDGE_CURVE('',#11922,#11921,#862,.T.);
#15435=EDGE_CURVE('',#11922,#11923,#3603,.T.);
#15436=EDGE_CURVE('',#11924,#11923,#863,.T.);
#15437=EDGE_CURVE('',#11925,#11924,#1678,.T.);
#15438=EDGE_CURVE('',#11926,#11925,#864,.T.);
#15439=EDGE_CURVE('',#11926,#11927,#3604,.T.);
#15440=EDGE_CURVE('',#11928,#11927,#865,.T.);
#15441=EDGE_CURVE('',#11929,#11928,#1679,.T.);
#15442=EDGE_CURVE('',#11930,#11929,#866,.T.);
#15443=EDGE_CURVE('',#11930,#11931,#3605,.T.);
#15444=EDGE_CURVE('',#11932,#11931,#867,.T.);
#15445=EDGE_CURVE('',#11643,#11932,#3098,.T.);
#15446=EDGE_CURVE('',#11643,#11933,#8748,.T.);
#15447=EDGE_CURVE('',#11934,#11933,#3606,.T.);
#15448=EDGE_CURVE('',#11933,#11934,#3607,.T.);
#15449=EDGE_CURVE('',#11935,#11935,#3608,.T.);
#15450=EDGE_CURVE('',#11935,#11934,#3609,.T.);
#15451=EDGE_CURVE('',#11936,#11936,#3610,.T.);
#15452=EDGE_CURVE('',#11936,#11935,#8749,.T.);
#15453=EDGE_CURVE('',#11937,#11937,#3611,.T.);
#15454=EDGE_CURVE('',#11937,#11936,#3612,.T.);
#15455=EDGE_CURVE('',#11159,#11938,#3613,.T.);
#15456=EDGE_CURVE('',#11938,#11938,#3614,.T.);
#15457=EDGE_CURVE('',#11939,#11892,#1680,.T.);
#15458=EDGE_CURVE('',#11939,#11940,#3615,.T.);
#15459=EDGE_CURVE('',#11893,#11940,#1681,.T.);
#15460=EDGE_CURVE('',#11891,#11941,#1682,.T.);
#15461=EDGE_CURVE('',#11942,#11890,#1683,.T.);
#15462=EDGE_CURVE('',#11942,#11941,#3616,.T.);
#15463=EDGE_CURVE('',#11889,#11943,#1684,.T.);
#15464=EDGE_CURVE('',#11944,#11888,#1685,.T.);
#15465=EDGE_CURVE('',#11944,#11943,#3617,.T.);
#15466=EDGE_CURVE('',#11887,#11945,#1686,.T.);
#15467=EDGE_CURVE('',#11946,#11886,#1687,.T.);
#15468=EDGE_CURVE('',#11946,#11945,#3618,.T.);
#15469=EDGE_CURVE('',#11885,#11947,#1688,.T.);
#15470=EDGE_CURVE('',#11948,#11884,#1689,.T.);
#15471=EDGE_CURVE('',#11948,#11947,#3619,.T.);
#15472=EDGE_CURVE('',#11883,#11949,#1690,.T.);
#15473=EDGE_CURVE('',#11950,#11882,#1691,.T.);
#15474=EDGE_CURVE('',#11950,#11949,#3620,.T.);
#15475=EDGE_CURVE('',#11881,#11951,#1692,.T.);
#15476=EDGE_CURVE('',#11952,#11880,#1693,.T.);
#15477=EDGE_CURVE('',#11952,#11951,#3621,.T.);
#15478=EDGE_CURVE('',#11877,#11953,#1694,.T.);
#15479=EDGE_CURVE('',#11954,#11876,#1695,.T.);
#15480=EDGE_CURVE('',#11954,#11953,#3622,.T.);
#15481=EDGE_CURVE('',#11873,#11955,#1696,.T.);
#15482=EDGE_CURVE('',#11956,#11872,#1697,.T.);
#15483=EDGE_CURVE('',#11956,#11955,#3623,.T.);
#15484=EDGE_CURVE('',#11869,#11957,#1698,.T.);
#15485=EDGE_CURVE('',#11958,#11868,#1699,.T.);
#15486=EDGE_CURVE('',#11958,#11957,#3624,.T.);
#15487=EDGE_CURVE('',#11865,#11959,#1700,.T.);
#15488=EDGE_CURVE('',#11960,#11864,#1701,.T.);
#15489=EDGE_CURVE('',#11960,#11959,#3625,.T.);
#15490=EDGE_CURVE('',#11861,#11961,#1702,.T.);
#15491=EDGE_CURVE('',#11962,#11860,#1703,.T.);
#15492=EDGE_CURVE('',#11962,#11961,#3626,.T.);
#15493=EDGE_CURVE('',#11857,#11963,#1704,.T.);
#15494=EDGE_CURVE('',#11964,#11856,#1705,.T.);
#15495=EDGE_CURVE('',#11964,#11963,#3627,.T.);
#15496=EDGE_CURVE('',#11853,#11965,#1706,.T.);
#15497=EDGE_CURVE('',#11966,#11852,#1707,.T.);
#15498=EDGE_CURVE('',#11966,#11965,#3628,.T.);
#15499=EDGE_CURVE('',#11849,#11967,#1708,.T.);
#15500=EDGE_CURVE('',#11968,#11848,#1709,.T.);
#15501=EDGE_CURVE('',#11968,#11967,#3629,.T.);
#15502=EDGE_CURVE('',#11845,#11969,#1710,.T.);
#15503=EDGE_CURVE('',#11970,#11844,#1711,.T.);
#15504=EDGE_CURVE('',#11970,#11969,#3630,.T.);
#15505=EDGE_CURVE('',#11841,#11971,#1712,.T.);
#15506=EDGE_CURVE('',#11972,#11840,#1713,.T.);
#15507=EDGE_CURVE('',#11972,#11971,#3631,.T.);
#15508=EDGE_CURVE('',#11837,#11973,#1714,.T.);
#15509=EDGE_CURVE('',#11974,#11836,#1715,.T.);
#15510=EDGE_CURVE('',#11974,#11973,#3632,.T.);
#15511=EDGE_CURVE('',#11833,#11975,#1716,.T.);
#15512=EDGE_CURVE('',#11976,#11832,#1717,.T.);
#15513=EDGE_CURVE('',#11976,#11975,#3633,.T.);
#15514=EDGE_CURVE('',#11829,#11977,#1718,.T.);
#15515=EDGE_CURVE('',#11978,#11828,#1719,.T.);
#15516=EDGE_CURVE('',#11978,#11977,#3634,.T.);
#15517=EDGE_CURVE('',#11825,#11979,#1720,.T.);
#15518=EDGE_CURVE('',#11980,#11824,#1721,.T.);
#15519=EDGE_CURVE('',#11980,#11979,#3635,.T.);
#15520=EDGE_CURVE('',#11821,#11981,#1722,.T.);
#15521=EDGE_CURVE('',#11982,#11820,#1723,.T.);
#15522=EDGE_CURVE('',#11982,#11981,#3636,.T.);
#15523=EDGE_CURVE('',#11817,#11983,#1724,.T.);
#15524=EDGE_CURVE('',#11984,#11816,#1725,.T.);
#15525=EDGE_CURVE('',#11984,#11983,#3637,.T.);
#15526=EDGE_CURVE('',#11813,#11985,#1726,.T.);
#15527=EDGE_CURVE('',#11986,#11812,#1727,.T.);
#15528=EDGE_CURVE('',#11986,#11985,#3638,.T.);
#15529=EDGE_CURVE('',#11809,#11987,#1728,.T.);
#15530=EDGE_CURVE('',#11988,#11808,#1729,.T.);
#15531=EDGE_CURVE('',#11988,#11987,#3639,.T.);
#15532=EDGE_CURVE('',#11805,#11989,#1730,.T.);
#15533=EDGE_CURVE('',#11990,#11804,#1731,.T.);
#15534=EDGE_CURVE('',#11990,#11989,#3640,.T.);
#15535=EDGE_CURVE('',#11801,#11991,#1732,.T.);
#15536=EDGE_CURVE('',#11992,#11800,#1733,.T.);
#15537=EDGE_CURVE('',#11992,#11991,#3641,.T.);
#15538=EDGE_CURVE('',#11797,#11993,#1734,.T.);
#15539=EDGE_CURVE('',#11994,#11796,#1735,.T.);
#15540=EDGE_CURVE('',#11994,#11993,#3642,.T.);
#15541=EDGE_CURVE('',#11793,#11995,#1736,.T.);
#15542=EDGE_CURVE('',#11996,#11792,#1737,.T.);
#15543=EDGE_CURVE('',#11996,#11995,#3643,.T.);
#15544=EDGE_CURVE('',#11789,#11997,#1738,.T.);
#15545=EDGE_CURVE('',#11998,#11788,#1739,.T.);
#15546=EDGE_CURVE('',#11998,#11997,#3644,.T.);
#15547=EDGE_CURVE('',#11785,#11999,#1740,.T.);
#15548=EDGE_CURVE('',#12000,#11784,#1741,.T.);
#15549=EDGE_CURVE('',#12000,#11999,#3645,.T.);
#15550=EDGE_CURVE('',#11781,#12001,#1742,.T.);
#15551=EDGE_CURVE('',#12002,#11780,#1743,.T.);
#15552=EDGE_CURVE('',#12002,#12001,#3646,.T.);
#15553=EDGE_CURVE('',#11777,#12003,#1744,.T.);
#15554=EDGE_CURVE('',#12004,#11776,#1745,.T.);
#15555=EDGE_CURVE('',#12004,#12003,#3647,.T.);
#15556=EDGE_CURVE('',#11773,#12005,#1746,.T.);
#15557=EDGE_CURVE('',#12006,#11772,#1747,.T.);
#15558=EDGE_CURVE('',#12006,#12005,#3648,.T.);
#15559=EDGE_CURVE('',#11769,#12007,#1748,.T.);
#15560=EDGE_CURVE('',#12008,#11768,#1749,.T.);
#15561=EDGE_CURVE('',#12008,#12007,#3649,.T.);
#15562=EDGE_CURVE('',#11765,#12009,#1750,.T.);
#15563=EDGE_CURVE('',#12010,#11764,#1751,.T.);
#15564=EDGE_CURVE('',#12010,#12009,#3650,.T.);
#15565=EDGE_CURVE('',#11761,#12011,#1752,.T.);
#15566=EDGE_CURVE('',#12012,#11760,#1753,.T.);
#15567=EDGE_CURVE('',#12012,#12011,#3651,.T.);
#15568=EDGE_CURVE('',#11757,#12013,#1754,.T.);
#15569=EDGE_CURVE('',#12014,#11756,#1755,.T.);
#15570=EDGE_CURVE('',#12014,#12013,#3652,.T.);
#15571=EDGE_CURVE('',#11753,#12015,#1756,.T.);
#15572=EDGE_CURVE('',#12016,#11752,#1757,.T.);
#15573=EDGE_CURVE('',#12016,#12015,#3653,.T.);
#15574=EDGE_CURVE('',#11749,#12017,#1758,.T.);
#15575=EDGE_CURVE('',#12018,#11748,#1759,.T.);
#15576=EDGE_CURVE('',#12018,#12017,#3654,.T.);
#15577=EDGE_CURVE('',#11745,#12019,#1760,.T.);
#15578=EDGE_CURVE('',#12020,#11744,#1761,.T.);
#15579=EDGE_CURVE('',#12020,#12019,#3655,.T.);
#15580=EDGE_CURVE('',#11741,#12021,#1762,.T.);
#15581=EDGE_CURVE('',#12022,#11740,#1763,.T.);
#15582=EDGE_CURVE('',#12022,#12021,#3656,.T.);
#15583=EDGE_CURVE('',#11737,#12023,#1764,.T.);
#15584=EDGE_CURVE('',#12024,#11736,#1765,.T.);
#15585=EDGE_CURVE('',#12024,#12023,#3657,.T.);
#15586=EDGE_CURVE('',#11733,#12025,#1766,.T.);
#15587=EDGE_CURVE('',#12026,#11732,#1767,.T.);
#15588=EDGE_CURVE('',#12026,#12025,#3658,.T.);
#15589=EDGE_CURVE('',#11729,#12027,#1768,.T.);
#15590=EDGE_CURVE('',#12028,#11728,#1769,.T.);
#15591=EDGE_CURVE('',#12028,#12027,#3659,.T.);
#15592=EDGE_CURVE('',#11725,#12029,#1770,.T.);
#15593=EDGE_CURVE('',#12030,#11724,#1771,.T.);
#15594=EDGE_CURVE('',#12030,#12029,#3660,.T.);
#15595=EDGE_CURVE('',#11721,#12031,#1772,.T.);
#15596=EDGE_CURVE('',#12032,#11720,#1773,.T.);
#15597=EDGE_CURVE('',#12032,#12031,#3661,.T.);
#15598=EDGE_CURVE('',#11717,#12033,#1774,.T.);
#15599=EDGE_CURVE('',#12034,#11716,#1775,.T.);
#15600=EDGE_CURVE('',#12034,#12033,#3662,.T.);
#15601=EDGE_CURVE('',#11713,#12035,#1776,.T.);
#15602=EDGE_CURVE('',#12036,#11712,#1777,.T.);
#15603=EDGE_CURVE('',#12036,#12035,#3663,.T.);
#15604=EDGE_CURVE('',#11709,#12037,#1778,.T.);
#15605=EDGE_CURVE('',#12038,#11708,#1779,.T.);
#15606=EDGE_CURVE('',#12038,#12037,#3664,.T.);
#15607=EDGE_CURVE('',#11705,#12039,#1780,.T.);
#15608=EDGE_CURVE('',#12040,#11704,#1781,.T.);
#15609=EDGE_CURVE('',#12040,#12039,#3665,.T.);
#15610=EDGE_CURVE('',#11701,#12041,#1782,.T.);
#15611=EDGE_CURVE('',#12042,#11700,#1783,.T.);
#15612=EDGE_CURVE('',#12042,#12041,#3666,.T.);
#15613=EDGE_CURVE('',#11697,#12043,#1784,.T.);
#15614=EDGE_CURVE('',#12044,#11696,#1785,.T.);
#15615=EDGE_CURVE('',#12044,#12043,#3667,.T.);
#15616=EDGE_CURVE('',#11693,#12045,#1786,.T.);
#15617=EDGE_CURVE('',#12046,#11692,#1787,.T.);
#15618=EDGE_CURVE('',#12046,#12045,#3668,.T.);
#15619=EDGE_CURVE('',#11689,#12047,#1788,.T.);
#15620=EDGE_CURVE('',#12048,#11688,#1789,.T.);
#15621=EDGE_CURVE('',#12048,#12047,#3669,.T.);
#15622=EDGE_CURVE('',#11685,#12049,#1790,.T.);
#15623=EDGE_CURVE('',#12050,#11684,#1791,.T.);
#15624=EDGE_CURVE('',#12050,#12049,#3670,.T.);
#15625=EDGE_CURVE('',#11681,#12051,#1792,.T.);
#15626=EDGE_CURVE('',#12052,#11680,#1793,.T.);
#15627=EDGE_CURVE('',#12052,#12051,#3671,.T.);
#15628=EDGE_CURVE('',#11677,#12053,#1794,.T.);
#15629=EDGE_CURVE('',#12054,#11676,#1795,.T.);
#15630=EDGE_CURVE('',#12054,#12053,#3672,.T.);
#15631=EDGE_CURVE('',#11673,#12055,#1796,.T.);
#15632=EDGE_CURVE('',#12056,#11672,#1797,.T.);
#15633=EDGE_CURVE('',#12056,#12055,#3673,.T.);
#15634=EDGE_CURVE('',#11669,#12057,#1798,.T.);
#15635=EDGE_CURVE('',#12058,#11668,#1799,.T.);
#15636=EDGE_CURVE('',#12058,#12057,#3674,.T.);
#15637=EDGE_CURVE('',#11665,#12059,#1800,.T.);
#15638=EDGE_CURVE('',#12060,#11664,#1801,.T.);
#15639=EDGE_CURVE('',#12060,#12059,#3675,.T.);
#15640=EDGE_CURVE('',#11661,#12061,#1802,.T.);
#15641=EDGE_CURVE('',#12062,#11660,#1803,.T.);
#15642=EDGE_CURVE('',#12062,#12061,#3676,.T.);
#15643=EDGE_CURVE('',#11657,#12063,#1804,.T.);
#15644=EDGE_CURVE('',#12064,#11656,#1805,.T.);
#15645=EDGE_CURVE('',#12064,#12063,#3677,.T.);
#15646=EDGE_CURVE('',#11653,#12065,#1806,.T.);
#15647=EDGE_CURVE('',#12066,#11652,#1807,.T.);
#15648=EDGE_CURVE('',#12066,#12065,#3678,.T.);
#15649=EDGE_CURVE('',#12067,#11894,#1808,.T.);
#15650=EDGE_CURVE('',#12067,#12068,#3679,.T.);
#15651=EDGE_CURVE('',#11895,#12068,#1809,.T.);
#15652=EDGE_CURVE('',#12069,#11896,#1810,.T.);
#15653=EDGE_CURVE('',#12069,#12070,#3680,.T.);
#15654=EDGE_CURVE('',#11897,#12070,#1811,.T.);
#15655=EDGE_CURVE('',#12071,#11898,#1812,.T.);
#15656=EDGE_CURVE('',#12071,#12072,#3681,.T.);
#15657=EDGE_CURVE('',#11899,#12072,#1813,.T.);
#15658=EDGE_CURVE('',#12073,#11900,#1814,.T.);
#15659=EDGE_CURVE('',#12073,#12074,#3682,.T.);
#15660=EDGE_CURVE('',#11901,#12074,#1815,.T.);
#15661=EDGE_CURVE('',#12075,#11902,#1816,.T.);
#15662=EDGE_CURVE('',#12075,#12076,#3683,.T.);
#15663=EDGE_CURVE('',#11903,#12076,#1817,.T.);
#15664=EDGE_CURVE('',#12077,#11904,#1818,.T.);
#15665=EDGE_CURVE('',#12077,#12078,#3684,.T.);
#15666=EDGE_CURVE('',#11905,#12078,#1819,.T.);
#15667=EDGE_CURVE('',#12079,#11906,#1820,.T.);
#15668=EDGE_CURVE('',#12079,#12080,#3685,.T.);
#15669=EDGE_CURVE('',#11907,#12080,#1821,.T.);
#15670=EDGE_CURVE('',#12081,#11908,#1822,.T.);
#15671=EDGE_CURVE('',#12081,#12082,#3686,.T.);
#15672=EDGE_CURVE('',#11909,#12082,#1823,.T.);
#15673=EDGE_CURVE('',#12083,#11910,#1824,.T.);
#15674=EDGE_CURVE('',#12083,#12084,#3687,.T.);
#15675=EDGE_CURVE('',#11911,#12084,#1825,.T.);
#15676=EDGE_CURVE('',#12085,#11914,#1826,.T.);
#15677=EDGE_CURVE('',#12085,#12086,#3688,.T.);
#15678=EDGE_CURVE('',#11915,#12086,#1827,.T.);
#15679=EDGE_CURVE('',#12087,#11918,#1828,.T.);
#15680=EDGE_CURVE('',#12087,#12088,#3689,.T.);
#15681=EDGE_CURVE('',#11919,#12088,#1829,.T.);
#15682=EDGE_CURVE('',#12089,#11922,#1830,.T.);
#15683=EDGE_CURVE('',#12089,#12090,#3690,.T.);
#15684=EDGE_CURVE('',#11923,#12090,#1831,.T.);
#15685=EDGE_CURVE('',#12091,#11926,#1832,.T.);
#15686=EDGE_CURVE('',#12091,#12092,#3691,.T.);
#15687=EDGE_CURVE('',#11927,#12092,#1833,.T.);
#15688=EDGE_CURVE('',#12093,#11930,#1834,.T.);
#15689=EDGE_CURVE('',#12093,#12094,#3692,.T.);
#15690=EDGE_CURVE('',#11931,#12094,#1835,.T.);
#15691=EDGE_CURVE('',#11649,#12095,#1836,.T.);
#15692=EDGE_CURVE('',#12096,#11648,#1837,.T.);
#15693=EDGE_CURVE('',#12096,#12095,#3693,.T.);
#15694=EDGE_CURVE('',#12097,#11939,#8750,.T.);
#15695=EDGE_CURVE('',#12097,#12098,#3694,.T.);
#15696=EDGE_CURVE('',#11940,#12098,#8751,.T.);
#15697=EDGE_CURVE('',#11941,#12099,#8752,.T.);
#15698=EDGE_CURVE('',#12100,#11942,#8753,.T.);
#15699=EDGE_CURVE('',#12100,#12099,#3695,.T.);
#15700=EDGE_CURVE('',#11943,#12101,#8754,.T.);
#15701=EDGE_CURVE('',#12102,#11944,#8755,.T.);
#15702=EDGE_CURVE('',#12102,#12101,#3696,.T.);
#15703=EDGE_CURVE('',#11945,#12103,#8756,.T.);
#15704=EDGE_CURVE('',#12104,#11946,#8757,.T.);
#15705=EDGE_CURVE('',#12104,#12103,#3697,.T.);
#15706=EDGE_CURVE('',#11947,#12105,#8758,.T.);
#15707=EDGE_CURVE('',#12106,#11948,#8759,.T.);
#15708=EDGE_CURVE('',#12106,#12105,#3698,.T.);
#15709=EDGE_CURVE('',#11949,#12107,#8760,.T.);
#15710=EDGE_CURVE('',#12108,#11950,#8761,.T.);
#15711=EDGE_CURVE('',#12108,#12107,#3699,.T.);
#15712=EDGE_CURVE('',#11951,#12109,#8762,.T.);
#15713=EDGE_CURVE('',#12110,#11952,#8763,.T.);
#15714=EDGE_CURVE('',#12110,#12109,#3700,.T.);
#15715=EDGE_CURVE('',#11953,#12111,#8764,.T.);
#15716=EDGE_CURVE('',#12112,#11954,#8765,.T.);
#15717=EDGE_CURVE('',#12112,#12111,#3701,.T.);
#15718=EDGE_CURVE('',#11955,#12113,#8766,.T.);
#15719=EDGE_CURVE('',#12114,#11956,#8767,.T.);
#15720=EDGE_CURVE('',#12114,#12113,#3702,.T.);
#15721=EDGE_CURVE('',#11957,#12115,#8768,.T.);
#15722=EDGE_CURVE('',#12116,#11958,#8769,.T.);
#15723=EDGE_CURVE('',#12116,#12115,#3703,.T.);
#15724=EDGE_CURVE('',#11959,#12117,#8770,.T.);
#15725=EDGE_CURVE('',#12118,#11960,#8771,.T.);
#15726=EDGE_CURVE('',#12118,#12117,#3704,.T.);
#15727=EDGE_CURVE('',#11961,#12119,#8772,.T.);
#15728=EDGE_CURVE('',#12120,#11962,#8773,.T.);
#15729=EDGE_CURVE('',#12120,#12119,#3705,.T.);
#15730=EDGE_CURVE('',#11963,#12121,#8774,.T.);
#15731=EDGE_CURVE('',#12122,#11964,#8775,.T.);
#15732=EDGE_CURVE('',#12122,#12121,#3706,.T.);
#15733=EDGE_CURVE('',#11965,#12123,#8776,.T.);
#15734=EDGE_CURVE('',#12124,#11966,#8777,.T.);
#15735=EDGE_CURVE('',#12124,#12123,#3707,.T.);
#15736=EDGE_CURVE('',#11967,#12125,#8778,.T.);
#15737=EDGE_CURVE('',#12126,#11968,#8779,.T.);
#15738=EDGE_CURVE('',#12126,#12125,#3708,.T.);
#15739=EDGE_CURVE('',#11969,#12127,#8780,.T.);
#15740=EDGE_CURVE('',#12128,#11970,#8781,.T.);
#15741=EDGE_CURVE('',#12128,#12127,#3709,.T.);
#15742=EDGE_CURVE('',#11971,#12129,#8782,.T.);
#15743=EDGE_CURVE('',#12130,#11972,#8783,.T.);
#15744=EDGE_CURVE('',#12130,#12129,#3710,.T.);
#15745=EDGE_CURVE('',#11973,#12131,#8784,.T.);
#15746=EDGE_CURVE('',#12132,#11974,#8785,.T.);
#15747=EDGE_CURVE('',#12132,#12131,#3711,.T.);
#15748=EDGE_CURVE('',#11975,#12133,#8786,.T.);
#15749=EDGE_CURVE('',#12134,#11976,#8787,.T.);
#15750=EDGE_CURVE('',#12134,#12133,#3712,.T.);
#15751=EDGE_CURVE('',#11977,#12135,#8788,.T.);
#15752=EDGE_CURVE('',#12136,#11978,#8789,.T.);
#15753=EDGE_CURVE('',#12136,#12135,#3713,.T.);
#15754=EDGE_CURVE('',#11979,#12137,#8790,.T.);
#15755=EDGE_CURVE('',#12138,#11980,#8791,.T.);
#15756=EDGE_CURVE('',#12138,#12137,#3714,.T.);
#15757=EDGE_CURVE('',#11981,#12139,#8792,.T.);
#15758=EDGE_CURVE('',#12140,#11982,#8793,.T.);
#15759=EDGE_CURVE('',#12140,#12139,#3715,.T.);
#15760=EDGE_CURVE('',#11983,#12141,#8794,.T.);
#15761=EDGE_CURVE('',#12142,#11984,#8795,.T.);
#15762=EDGE_CURVE('',#12142,#12141,#3716,.T.);
#15763=EDGE_CURVE('',#11985,#12143,#8796,.T.);
#15764=EDGE_CURVE('',#12144,#11986,#8797,.T.);
#15765=EDGE_CURVE('',#12144,#12143,#3717,.T.);
#15766=EDGE_CURVE('',#11987,#12145,#8798,.T.);
#15767=EDGE_CURVE('',#12146,#11988,#8799,.T.);
#15768=EDGE_CURVE('',#12146,#12145,#3718,.T.);
#15769=EDGE_CURVE('',#11989,#12147,#8800,.T.);
#15770=EDGE_CURVE('',#12148,#11990,#8801,.T.);
#15771=EDGE_CURVE('',#12148,#12147,#3719,.T.);
#15772=EDGE_CURVE('',#11991,#12149,#8802,.T.);
#15773=EDGE_CURVE('',#12150,#11992,#8803,.T.);
#15774=EDGE_CURVE('',#12150,#12149,#3720,.T.);
#15775=EDGE_CURVE('',#11993,#12151,#8804,.T.);
#15776=EDGE_CURVE('',#12152,#11994,#8805,.T.);
#15777=EDGE_CURVE('',#12152,#12151,#3721,.T.);
#15778=EDGE_CURVE('',#11995,#12153,#8806,.T.);
#15779=EDGE_CURVE('',#12154,#11996,#8807,.T.);
#15780=EDGE_CURVE('',#12154,#12153,#3722,.T.);
#15781=EDGE_CURVE('',#11997,#12155,#8808,.T.);
#15782=EDGE_CURVE('',#12156,#11998,#8809,.T.);
#15783=EDGE_CURVE('',#12156,#12155,#3723,.T.);
#15784=EDGE_CURVE('',#11999,#12157,#8810,.T.);
#15785=EDGE_CURVE('',#12158,#12000,#8811,.T.);
#15786=EDGE_CURVE('',#12158,#12157,#3724,.T.);
#15787=EDGE_CURVE('',#12001,#12159,#8812,.T.);
#15788=EDGE_CURVE('',#12160,#12002,#8813,.T.);
#15789=EDGE_CURVE('',#12160,#12159,#3725,.T.);
#15790=EDGE_CURVE('',#12003,#12161,#8814,.T.);
#15791=EDGE_CURVE('',#12162,#12004,#8815,.T.);
#15792=EDGE_CURVE('',#12162,#12161,#3726,.T.);
#15793=EDGE_CURVE('',#12005,#12163,#8816,.T.);
#15794=EDGE_CURVE('',#12164,#12006,#8817,.T.);
#15795=EDGE_CURVE('',#12164,#12163,#3727,.T.);
#15796=EDGE_CURVE('',#12007,#12165,#8818,.T.);
#15797=EDGE_CURVE('',#12166,#12008,#8819,.T.);
#15798=EDGE_CURVE('',#12166,#12165,#3728,.T.);
#15799=EDGE_CURVE('',#12009,#12167,#8820,.T.);
#15800=EDGE_CURVE('',#12168,#12010,#8821,.T.);
#15801=EDGE_CURVE('',#12168,#12167,#3729,.T.);
#15802=EDGE_CURVE('',#12011,#12169,#8822,.T.);
#15803=EDGE_CURVE('',#12170,#12012,#8823,.T.);
#15804=EDGE_CURVE('',#12170,#12169,#3730,.T.);
#15805=EDGE_CURVE('',#12013,#12171,#8824,.T.);
#15806=EDGE_CURVE('',#12172,#12014,#8825,.T.);
#15807=EDGE_CURVE('',#12172,#12171,#3731,.T.);
#15808=EDGE_CURVE('',#12015,#12173,#8826,.T.);
#15809=EDGE_CURVE('',#12174,#12016,#8827,.T.);
#15810=EDGE_CURVE('',#12174,#12173,#3732,.T.);
#15811=EDGE_CURVE('',#12017,#12175,#8828,.T.);
#15812=EDGE_CURVE('',#12176,#12018,#8829,.T.);
#15813=EDGE_CURVE('',#12176,#12175,#3733,.T.);
#15814=EDGE_CURVE('',#12019,#12177,#8830,.T.);
#15815=EDGE_CURVE('',#12178,#12020,#8831,.T.);
#15816=EDGE_CURVE('',#12178,#12177,#3734,.T.);
#15817=EDGE_CURVE('',#12021,#12179,#8832,.T.);
#15818=EDGE_CURVE('',#12180,#12022,#8833,.T.);
#15819=EDGE_CURVE('',#12180,#12179,#3735,.T.);
#15820=EDGE_CURVE('',#12023,#12181,#8834,.T.);
#15821=EDGE_CURVE('',#12182,#12024,#8835,.T.);
#15822=EDGE_CURVE('',#12182,#12181,#3736,.T.);
#15823=EDGE_CURVE('',#12025,#12183,#8836,.T.);
#15824=EDGE_CURVE('',#12184,#12026,#8837,.T.);
#15825=EDGE_CURVE('',#12184,#12183,#3737,.T.);
#15826=EDGE_CURVE('',#12027,#12185,#8838,.T.);
#15827=EDGE_CURVE('',#12186,#12028,#8839,.T.);
#15828=EDGE_CURVE('',#12186,#12185,#3738,.T.);
#15829=EDGE_CURVE('',#12029,#12187,#8840,.T.);
#15830=EDGE_CURVE('',#12188,#12030,#8841,.T.);
#15831=EDGE_CURVE('',#12188,#12187,#3739,.T.);
#15832=EDGE_CURVE('',#12031,#12189,#8842,.T.);
#15833=EDGE_CURVE('',#12190,#12032,#8843,.T.);
#15834=EDGE_CURVE('',#12190,#12189,#3740,.T.);
#15835=EDGE_CURVE('',#12033,#12191,#8844,.T.);
#15836=EDGE_CURVE('',#12192,#12034,#8845,.T.);
#15837=EDGE_CURVE('',#12192,#12191,#3741,.T.);
#15838=EDGE_CURVE('',#12035,#12193,#8846,.T.);
#15839=EDGE_CURVE('',#12194,#12036,#8847,.T.);
#15840=EDGE_CURVE('',#12194,#12193,#3742,.T.);
#15841=EDGE_CURVE('',#12037,#12195,#8848,.T.);
#15842=EDGE_CURVE('',#12196,#12038,#8849,.T.);
#15843=EDGE_CURVE('',#12196,#12195,#3743,.T.);
#15844=EDGE_CURVE('',#12039,#12197,#8850,.T.);
#15845=EDGE_CURVE('',#12198,#12040,#8851,.T.);
#15846=EDGE_CURVE('',#12198,#12197,#3744,.T.);
#15847=EDGE_CURVE('',#12041,#12199,#8852,.T.);
#15848=EDGE_CURVE('',#12200,#12042,#8853,.T.);
#15849=EDGE_CURVE('',#12200,#12199,#3745,.T.);
#15850=EDGE_CURVE('',#12043,#12201,#8854,.T.);
#15851=EDGE_CURVE('',#12202,#12044,#8855,.T.);
#15852=EDGE_CURVE('',#12202,#12201,#3746,.T.);
#15853=EDGE_CURVE('',#12045,#12203,#8856,.T.);
#15854=EDGE_CURVE('',#12204,#12046,#8857,.T.);
#15855=EDGE_CURVE('',#12204,#12203,#3747,.T.);
#15856=EDGE_CURVE('',#12047,#12205,#8858,.T.);
#15857=EDGE_CURVE('',#12206,#12048,#8859,.T.);
#15858=EDGE_CURVE('',#12206,#12205,#3748,.T.);
#15859=EDGE_CURVE('',#12049,#12207,#8860,.T.);
#15860=EDGE_CURVE('',#12208,#12050,#8861,.T.);
#15861=EDGE_CURVE('',#12208,#12207,#3749,.T.);
#15862=EDGE_CURVE('',#12051,#12209,#8862,.T.);
#15863=EDGE_CURVE('',#12210,#12052,#8863,.T.);
#15864=EDGE_CURVE('',#12210,#12209,#3750,.T.);
#15865=EDGE_CURVE('',#12053,#12211,#8864,.T.);
#15866=EDGE_CURVE('',#12212,#12054,#8865,.T.);
#15867=EDGE_CURVE('',#12212,#12211,#3751,.T.);
#15868=EDGE_CURVE('',#12055,#12213,#8866,.T.);
#15869=EDGE_CURVE('',#12214,#12056,#8867,.T.);
#15870=EDGE_CURVE('',#12214,#12213,#3752,.T.);
#15871=EDGE_CURVE('',#12057,#12215,#8868,.T.);
#15872=EDGE_CURVE('',#12216,#12058,#8869,.T.);
#15873=EDGE_CURVE('',#12216,#12215,#3753,.T.);
#15874=EDGE_CURVE('',#12059,#12217,#8870,.T.);
#15875=EDGE_CURVE('',#12218,#12060,#8871,.T.);
#15876=EDGE_CURVE('',#12218,#12217,#3754,.T.);
#15877=EDGE_CURVE('',#12061,#12219,#8872,.T.);
#15878=EDGE_CURVE('',#12220,#12062,#8873,.T.);
#15879=EDGE_CURVE('',#12220,#12219,#3755,.T.);
#15880=EDGE_CURVE('',#12063,#12221,#8874,.T.);
#15881=EDGE_CURVE('',#12222,#12064,#8875,.T.);
#15882=EDGE_CURVE('',#12222,#12221,#3756,.T.);
#15883=EDGE_CURVE('',#12065,#12223,#8876,.T.);
#15884=EDGE_CURVE('',#12224,#12066,#8877,.T.);
#15885=EDGE_CURVE('',#12224,#12223,#3757,.T.);
#15886=EDGE_CURVE('',#12225,#12067,#8878,.T.);
#15887=EDGE_CURVE('',#12225,#12226,#3758,.T.);
#15888=EDGE_CURVE('',#12068,#12226,#8879,.T.);
#15889=EDGE_CURVE('',#12227,#12069,#8880,.T.);
#15890=EDGE_CURVE('',#12227,#12228,#3759,.T.);
#15891=EDGE_CURVE('',#12070,#12228,#8881,.T.);
#15892=EDGE_CURVE('',#12229,#12071,#8882,.T.);
#15893=EDGE_CURVE('',#12229,#12230,#3760,.T.);
#15894=EDGE_CURVE('',#12072,#12230,#8883,.T.);
#15895=EDGE_CURVE('',#12231,#12073,#8884,.T.);
#15896=EDGE_CURVE('',#12231,#12232,#3761,.T.);
#15897=EDGE_CURVE('',#12074,#12232,#8885,.T.);
#15898=EDGE_CURVE('',#12233,#12075,#8886,.T.);
#15899=EDGE_CURVE('',#12233,#12234,#3762,.T.);
#15900=EDGE_CURVE('',#12076,#12234,#8887,.T.);
#15901=EDGE_CURVE('',#12235,#12077,#8888,.T.);
#15902=EDGE_CURVE('',#12235,#12236,#3763,.T.);
#15903=EDGE_CURVE('',#12078,#12236,#8889,.T.);
#15904=EDGE_CURVE('',#12237,#12079,#8890,.T.);
#15905=EDGE_CURVE('',#12237,#12238,#3764,.T.);
#15906=EDGE_CURVE('',#12080,#12238,#8891,.T.);
#15907=EDGE_CURVE('',#12239,#12081,#8892,.T.);
#15908=EDGE_CURVE('',#12239,#12240,#3765,.T.);
#15909=EDGE_CURVE('',#12082,#12240,#8893,.T.);
#15910=EDGE_CURVE('',#12241,#12083,#8894,.T.);
#15911=EDGE_CURVE('',#12241,#12242,#3766,.T.);
#15912=EDGE_CURVE('',#12084,#12242,#8895,.T.);
#15913=EDGE_CURVE('',#12243,#12085,#8896,.T.);
#15914=EDGE_CURVE('',#12243,#12244,#3767,.T.);
#15915=EDGE_CURVE('',#12086,#12244,#8897,.T.);
#15916=EDGE_CURVE('',#12245,#12087,#8898,.T.);
#15917=EDGE_CURVE('',#12245,#12246,#3768,.T.);
#15918=EDGE_CURVE('',#12088,#12246,#8899,.T.);
#15919=EDGE_CURVE('',#12247,#12089,#8900,.T.);
#15920=EDGE_CURVE('',#12247,#12248,#3769,.T.);
#15921=EDGE_CURVE('',#12090,#12248,#8901,.T.);
#15922=EDGE_CURVE('',#12249,#12091,#8902,.T.);
#15923=EDGE_CURVE('',#12249,#12250,#3770,.T.);
#15924=EDGE_CURVE('',#12092,#12250,#8903,.T.);
#15925=EDGE_CURVE('',#12251,#12093,#8904,.T.);
#15926=EDGE_CURVE('',#12251,#12252,#3771,.T.);
#15927=EDGE_CURVE('',#12094,#12252,#8905,.T.);
#15928=EDGE_CURVE('',#12095,#12253,#8906,.T.);
#15929=EDGE_CURVE('',#12254,#12096,#8907,.T.);
#15930=EDGE_CURVE('',#12254,#12253,#3772,.T.);
#15931=EDGE_CURVE('',#11552,#12097,#1838,.T.);
#15932=EDGE_CURVE('',#12098,#11551,#1839,.T.);
#15933=EDGE_CURVE('',#12099,#11553,#1840,.T.);
#15934=EDGE_CURVE('',#11554,#12100,#1841,.T.);
#15935=EDGE_CURVE('',#12101,#11555,#1842,.T.);
#15936=EDGE_CURVE('',#11556,#12102,#1843,.T.);
#15937=EDGE_CURVE('',#12103,#11557,#1844,.T.);
#15938=EDGE_CURVE('',#11558,#12104,#1845,.T.);
#15939=EDGE_CURVE('',#12105,#11559,#1846,.T.);
#15940=EDGE_CURVE('',#11560,#12106,#1847,.T.);
#15941=EDGE_CURVE('',#12107,#11561,#1848,.T.);
#15942=EDGE_CURVE('',#11562,#12108,#1849,.T.);
#15943=EDGE_CURVE('',#12109,#11563,#1850,.T.);
#15944=EDGE_CURVE('',#11564,#12110,#1851,.T.);
#15945=EDGE_CURVE('',#12111,#11567,#1852,.T.);
#15946=EDGE_CURVE('',#11568,#12112,#1853,.T.);
#15947=EDGE_CURVE('',#12113,#11571,#1854,.T.);
#15948=EDGE_CURVE('',#11572,#12114,#1855,.T.);
#15949=EDGE_CURVE('',#12115,#11575,#1856,.T.);
#15950=EDGE_CURVE('',#11576,#12116,#1857,.T.);
#15951=EDGE_CURVE('',#12117,#11579,#1858,.T.);
#15952=EDGE_CURVE('',#11580,#12118,#1859,.T.);
#15953=EDGE_CURVE('',#12119,#11583,#1860,.T.);
#15954=EDGE_CURVE('',#11584,#12120,#1861,.T.);
#15955=EDGE_CURVE('',#12121,#11587,#1862,.T.);
#15956=EDGE_CURVE('',#11588,#12122,#1863,.T.);
#15957=EDGE_CURVE('',#12123,#11591,#1864,.T.);
#15958=EDGE_CURVE('',#11592,#12124,#1865,.T.);
#15959=EDGE_CURVE('',#12125,#11595,#1866,.T.);
#15960=EDGE_CURVE('',#11596,#12126,#1867,.T.);
#15961=EDGE_CURVE('',#12127,#11599,#1868,.T.);
#15962=EDGE_CURVE('',#11600,#12128,#1869,.T.);
#15963=EDGE_CURVE('',#12129,#11603,#1870,.T.);
#15964=EDGE_CURVE('',#11604,#12130,#1871,.T.);
#15965=EDGE_CURVE('',#12131,#11607,#1872,.T.);
#15966=EDGE_CURVE('',#11608,#12132,#1873,.T.);
#15967=EDGE_CURVE('',#12133,#11611,#1874,.T.);
#15968=EDGE_CURVE('',#11612,#12134,#1875,.T.);
#15969=EDGE_CURVE('',#12135,#11615,#1876,.T.);
#15970=EDGE_CURVE('',#11616,#12136,#1877,.T.);
#15971=EDGE_CURVE('',#12137,#11619,#1878,.T.);
#15972=EDGE_CURVE('',#11620,#12138,#1879,.T.);
#15973=EDGE_CURVE('',#12139,#11623,#1880,.T.);
#15974=EDGE_CURVE('',#11624,#12140,#1881,.T.);
#15975=EDGE_CURVE('',#12141,#11627,#1882,.T.);
#15976=EDGE_CURVE('',#11628,#12142,#1883,.T.);
#15977=EDGE_CURVE('',#12143,#11631,#1884,.T.);
#15978=EDGE_CURVE('',#11632,#12144,#1885,.T.);
#15979=EDGE_CURVE('',#12145,#11635,#1886,.T.);
#15980=EDGE_CURVE('',#11636,#12146,#1887,.T.);
#15981=EDGE_CURVE('',#12147,#11639,#1888,.T.);
#15982=EDGE_CURVE('',#11640,#12148,#1889,.T.);
#15983=EDGE_CURVE('',#12149,#11353,#1890,.T.);
#15984=EDGE_CURVE('',#11354,#12150,#1891,.T.);
#15985=EDGE_CURVE('',#12151,#11357,#1892,.T.);
#15986=EDGE_CURVE('',#11358,#12152,#1893,.T.);
#15987=EDGE_CURVE('',#12153,#11361,#1894,.T.);
#15988=EDGE_CURVE('',#11362,#12154,#1895,.T.);
#15989=EDGE_CURVE('',#12155,#11365,#1896,.T.);
#15990=EDGE_CURVE('',#11366,#12156,#1897,.T.);
#15991=EDGE_CURVE('',#12157,#11369,#1898,.T.);
#15992=EDGE_CURVE('',#11370,#12158,#1899,.T.);
#15993=EDGE_CURVE('',#12159,#11373,#1900,.T.);
#15994=EDGE_CURVE('',#11374,#12160,#1901,.T.);
#15995=EDGE_CURVE('',#12161,#11377,#1902,.T.);
#15996=EDGE_CURVE('',#11378,#12162,#1903,.T.);
#15997=EDGE_CURVE('',#12163,#11381,#1904,.T.);
#15998=EDGE_CURVE('',#11382,#12164,#1905,.T.);
#15999=EDGE_CURVE('',#12165,#11385,#1906,.T.);
#16000=EDGE_CURVE('',#11386,#12166,#1907,.T.);
#16001=EDGE_CURVE('',#12167,#11389,#1908,.T.);
#16002=EDGE_CURVE('',#11390,#12168,#1909,.T.);
#16003=EDGE_CURVE('',#12169,#11393,#1910,.T.);
#16004=EDGE_CURVE('',#11394,#12170,#1911,.T.);
#16005=EDGE_CURVE('',#12171,#11397,#1912,.T.);
#16006=EDGE_CURVE('',#11398,#12172,#1913,.T.);
#16007=EDGE_CURVE('',#12173,#11401,#1914,.T.);
#16008=EDGE_CURVE('',#11402,#12174,#1915,.T.);
#16009=EDGE_CURVE('',#12175,#11405,#1916,.T.);
#16010=EDGE_CURVE('',#11406,#12176,#1917,.T.);
#16011=EDGE_CURVE('',#12177,#11409,#1918,.T.);
#16012=EDGE_CURVE('',#11410,#12178,#1919,.T.);
#16013=EDGE_CURVE('',#12179,#11413,#1920,.T.);
#16014=EDGE_CURVE('',#11414,#12180,#1921,.T.);
#16015=EDGE_CURVE('',#12181,#11417,#1922,.T.);
#16016=EDGE_CURVE('',#11418,#12182,#1923,.T.);
#16017=EDGE_CURVE('',#12183,#11421,#1924,.T.);
#16018=EDGE_CURVE('',#11422,#12184,#1925,.T.);
#16019=EDGE_CURVE('',#12185,#11425,#1926,.T.);
#16020=EDGE_CURVE('',#11426,#12186,#1927,.T.);
#16021=EDGE_CURVE('',#12187,#11429,#1928,.T.);
#16022=EDGE_CURVE('',#11430,#12188,#1929,.T.);
#16023=EDGE_CURVE('',#12189,#11433,#1930,.T.);
#16024=EDGE_CURVE('',#11434,#12190,#1931,.T.);
#16025=EDGE_CURVE('',#12191,#11437,#1932,.T.);
#16026=EDGE_CURVE('',#11438,#12192,#1933,.T.);
#16027=EDGE_CURVE('',#12193,#11441,#1934,.T.);
#16028=EDGE_CURVE('',#11442,#12194,#1935,.T.);
#16029=EDGE_CURVE('',#12195,#11445,#1936,.T.);
#16030=EDGE_CURVE('',#11446,#12196,#1937,.T.);
#16031=EDGE_CURVE('',#12197,#11449,#1938,.T.);
#16032=EDGE_CURVE('',#11450,#12198,#1939,.T.);
#16033=EDGE_CURVE('',#12199,#11453,#1940,.T.);
#16034=EDGE_CURVE('',#11454,#12200,#1941,.T.);
#16035=EDGE_CURVE('',#12201,#11457,#1942,.T.);
#16036=EDGE_CURVE('',#11458,#12202,#1943,.T.);
#16037=EDGE_CURVE('',#12203,#11461,#1944,.T.);
#16038=EDGE_CURVE('',#11462,#12204,#1945,.T.);
#16039=EDGE_CURVE('',#12205,#11465,#1946,.T.);
#16040=EDGE_CURVE('',#11466,#12206,#1947,.T.);
#16041=EDGE_CURVE('',#12207,#11469,#1948,.T.);
#16042=EDGE_CURVE('',#11470,#12208,#1949,.T.);
#16043=EDGE_CURVE('',#12209,#11473,#1950,.T.);
#16044=EDGE_CURVE('',#11474,#12210,#1951,.T.);
#16045=EDGE_CURVE('',#12211,#11477,#1952,.T.);
#16046=EDGE_CURVE('',#11478,#12212,#1953,.T.);
#16047=EDGE_CURVE('',#12213,#11481,#1954,.T.);
#16048=EDGE_CURVE('',#11482,#12214,#1955,.T.);
#16049=EDGE_CURVE('',#12215,#11485,#1956,.T.);
#16050=EDGE_CURVE('',#11486,#12216,#1957,.T.);
#16051=EDGE_CURVE('',#12217,#11489,#1958,.T.);
#16052=EDGE_CURVE('',#11490,#12218,#1959,.T.);
#16053=EDGE_CURVE('',#12219,#11493,#1960,.T.);
#16054=EDGE_CURVE('',#11494,#12220,#1961,.T.);
#16055=EDGE_CURVE('',#12221,#11497,#1962,.T.);
#16056=EDGE_CURVE('',#11498,#12222,#1963,.T.);
#16057=EDGE_CURVE('',#12223,#11501,#1964,.T.);
#16058=EDGE_CURVE('',#11502,#12224,#1965,.T.);
#16059=EDGE_CURVE('',#11550,#12225,#1966,.T.);
#16060=EDGE_CURVE('',#12226,#11549,#1967,.T.);
#16061=EDGE_CURVE('',#11548,#12227,#1968,.T.);
#16062=EDGE_CURVE('',#12228,#11547,#1969,.T.);
#16063=EDGE_CURVE('',#11546,#12229,#1970,.T.);
#16064=EDGE_CURVE('',#12230,#11545,#1971,.T.);
#16065=EDGE_CURVE('',#11544,#12231,#1972,.T.);
#16066=EDGE_CURVE('',#12232,#11543,#1973,.T.);
#16067=EDGE_CURVE('',#11542,#12233,#1974,.T.);
#16068=EDGE_CURVE('',#12234,#11541,#1975,.T.);
#16069=EDGE_CURVE('',#11540,#12235,#1976,.T.);
#16070=EDGE_CURVE('',#12236,#11539,#1977,.T.);
#16071=EDGE_CURVE('',#11538,#12237,#1978,.T.);
#16072=EDGE_CURVE('',#12238,#11537,#1979,.T.);
#16073=EDGE_CURVE('',#11536,#12239,#1980,.T.);
#16074=EDGE_CURVE('',#12240,#11535,#1981,.T.);
#16075=EDGE_CURVE('',#11534,#12241,#1982,.T.);
#16076=EDGE_CURVE('',#12242,#11533,#1983,.T.);
#16077=EDGE_CURVE('',#11530,#12243,#1984,.T.);
#16078=EDGE_CURVE('',#12244,#11529,#1985,.T.);
#16079=EDGE_CURVE('',#11526,#12245,#1986,.T.);
#16080=EDGE_CURVE('',#12246,#11525,#1987,.T.);
#16081=EDGE_CURVE('',#11522,#12247,#1988,.T.);
#16082=EDGE_CURVE('',#12248,#11521,#1989,.T.);
#16083=EDGE_CURVE('',#11518,#12249,#1990,.T.);
#16084=EDGE_CURVE('',#12250,#11517,#1991,.T.);
#16085=EDGE_CURVE('',#11514,#12251,#1992,.T.);
#16086=EDGE_CURVE('',#12252,#11513,#1993,.T.);
#16087=EDGE_CURVE('',#12253,#11505,#1994,.T.);
#16088=EDGE_CURVE('',#11506,#12254,#1995,.T.);
#16089=EDGE_CURVE('',#11645,#12255,#1996,.T.);
#16090=EDGE_CURVE('',#12256,#11644,#1997,.T.);
#16091=EDGE_CURVE('',#12256,#12255,#3773,.T.);
#16092=EDGE_CURVE('',#12255,#12257,#8908,.T.);
#16093=EDGE_CURVE('',#12258,#12256,#8909,.T.);
#16094=EDGE_CURVE('',#12258,#12257,#3774,.T.);
#16095=EDGE_CURVE('',#12257,#11509,#1998,.T.);
#16096=EDGE_CURVE('',#11510,#12258,#1999,.T.);
#16097=EDGE_CURVE('',#12259,#12260,#8910,.T.);
#16098=EDGE_CURVE('',#12260,#12261,#8911,.T.);
#16099=EDGE_CURVE('',#12261,#12262,#8912,.T.);
#16100=EDGE_CURVE('',#12262,#12263,#8913,.T.);
#16101=EDGE_CURVE('',#12263,#12264,#8914,.T.);
#16102=EDGE_CURVE('',#12264,#12259,#8915,.T.);
#16103=EDGE_CURVE('',#12260,#11345,#8916,.T.);
#16104=EDGE_CURVE('',#12261,#11344,#8917,.T.);
#16105=EDGE_CURVE('',#12262,#11343,#8918,.T.);
#16106=EDGE_CURVE('',#12263,#11341,#8919,.T.);
#16107=EDGE_CURVE('',#12264,#11347,#8920,.T.);
#16108=EDGE_CURVE('',#12259,#11346,#8921,.T.);
#16109=EDGE_CURVE('',#11278,#11160,#3099,.T.);
#16110=EDGE_CURVE('',#11158,#11276,#8922,.T.);
#16111=EDGE_CURVE('',#11642,#11511,#8923,.T.);
#16112=EDGE_CURVE('',#11932,#11512,#8924,.T.);
#16113=EDGE_CURVE('',#11647,#11507,#8925,.T.);
#16114=EDGE_CURVE('',#11646,#11508,#8926,.T.);
#16115=EDGE_CURVE('',#11929,#11515,#8927,.T.);
#16116=EDGE_CURVE('',#11928,#11516,#8928,.T.);
#16117=EDGE_CURVE('',#11925,#11519,#8929,.T.);
#16118=EDGE_CURVE('',#11924,#11520,#8930,.T.);
#16119=EDGE_CURVE('',#11921,#11523,#8931,.T.);
#16120=EDGE_CURVE('',#11920,#11524,#8932,.T.);
#16121=EDGE_CURVE('',#11917,#11527,#8933,.T.);
#16122=EDGE_CURVE('',#11916,#11528,#8934,.T.);
#16123=EDGE_CURVE('',#11913,#11531,#8935,.T.);
#16124=EDGE_CURVE('',#11912,#11532,#8936,.T.);
#16125=EDGE_CURVE('',#11651,#11503,#8937,.T.);
#16126=EDGE_CURVE('',#11650,#11504,#8938,.T.);
#16127=EDGE_CURVE('',#11655,#11499,#8939,.T.);
#16128=EDGE_CURVE('',#11654,#11500,#8940,.T.);
#16129=EDGE_CURVE('',#11659,#11495,#8941,.T.);
#16130=EDGE_CURVE('',#11658,#11496,#8942,.T.);
#16131=EDGE_CURVE('',#11663,#11491,#8943,.T.);
#16132=EDGE_CURVE('',#11662,#11492,#8944,.T.);
#16133=EDGE_CURVE('',#11667,#11487,#8945,.T.);
#16134=EDGE_CURVE('',#11666,#11488,#8946,.T.);
#16135=EDGE_CURVE('',#11671,#11483,#8947,.T.);
#16136=EDGE_CURVE('',#11670,#11484,#8948,.T.);
#16137=EDGE_CURVE('',#11675,#11479,#8949,.T.);
#16138=EDGE_CURVE('',#11674,#11480,#8950,.T.);
#16139=EDGE_CURVE('',#11679,#11475,#8951,.T.);
#16140=EDGE_CURVE('',#11678,#11476,#8952,.T.);
#16141=EDGE_CURVE('',#11683,#11471,#8953,.T.);
#16142=EDGE_CURVE('',#11682,#11472,#8954,.T.);
#16143=EDGE_CURVE('',#11687,#11467,#8955,.T.);
#16144=EDGE_CURVE('',#11686,#11468,#8956,.T.);
#16145=EDGE_CURVE('',#11691,#11463,#8957,.T.);
#16146=EDGE_CURVE('',#11690,#11464,#8958,.T.);
#16147=EDGE_CURVE('',#11695,#11459,#8959,.T.);
#16148=EDGE_CURVE('',#11694,#11460,#8960,.T.);
#16149=EDGE_CURVE('',#11699,#11455,#8961,.T.);
#16150=EDGE_CURVE('',#11698,#11456,#8962,.T.);
#16151=EDGE_CURVE('',#11703,#11451,#8963,.T.);
#16152=EDGE_CURVE('',#11702,#11452,#8964,.T.);
#16153=EDGE_CURVE('',#11707,#11447,#8965,.T.);
#16154=EDGE_CURVE('',#11706,#11448,#8966,.T.);
#16155=EDGE_CURVE('',#11711,#11443,#8967,.T.);
#16156=EDGE_CURVE('',#11710,#11444,#8968,.T.);
#16157=EDGE_CURVE('',#11715,#11439,#8969,.T.);
#16158=EDGE_CURVE('',#11714,#11440,#8970,.T.);
#16159=EDGE_CURVE('',#11719,#11435,#8971,.T.);
#16160=EDGE_CURVE('',#11718,#11436,#8972,.T.);
#16161=EDGE_CURVE('',#11723,#11431,#8973,.T.);
#16162=EDGE_CURVE('',#11722,#11432,#8974,.T.);
#16163=EDGE_CURVE('',#11727,#11427,#8975,.T.);
#16164=EDGE_CURVE('',#11726,#11428,#8976,.T.);
#16165=EDGE_CURVE('',#11731,#11423,#8977,.T.);
#16166=EDGE_CURVE('',#11730,#11424,#8978,.T.);
#16167=EDGE_CURVE('',#11735,#11419,#8979,.T.);
#16168=EDGE_CURVE('',#11734,#11420,#8980,.T.);
#16169=EDGE_CURVE('',#11739,#11415,#8981,.T.);
#16170=EDGE_CURVE('',#11738,#11416,#8982,.T.);
#16171=EDGE_CURVE('',#11743,#11411,#8983,.T.);
#16172=EDGE_CURVE('',#11742,#11412,#8984,.T.);
#16173=EDGE_CURVE('',#11747,#11407,#8985,.T.);
#16174=EDGE_CURVE('',#11746,#11408,#8986,.T.);
#16175=EDGE_CURVE('',#11751,#11403,#8987,.T.);
#16176=EDGE_CURVE('',#11750,#11404,#8988,.T.);
#16177=EDGE_CURVE('',#11755,#11399,#8989,.T.);
#16178=EDGE_CURVE('',#11754,#11400,#8990,.T.);
#16179=EDGE_CURVE('',#11759,#11395,#8991,.T.);
#16180=EDGE_CURVE('',#11758,#11396,#8992,.T.);
#16181=EDGE_CURVE('',#11763,#11391,#8993,.T.);
#16182=EDGE_CURVE('',#11762,#11392,#8994,.T.);
#16183=EDGE_CURVE('',#11767,#11387,#8995,.T.);
#16184=EDGE_CURVE('',#11766,#11388,#8996,.T.);
#16185=EDGE_CURVE('',#11771,#11383,#8997,.T.);
#16186=EDGE_CURVE('',#11770,#11384,#8998,.T.);
#16187=EDGE_CURVE('',#11775,#11379,#8999,.T.);
#16188=EDGE_CURVE('',#11774,#11380,#9000,.T.);
#16189=EDGE_CURVE('',#11779,#11375,#9001,.T.);
#16190=EDGE_CURVE('',#11778,#11376,#9002,.T.);
#16191=EDGE_CURVE('',#11783,#11371,#9003,.T.);
#16192=EDGE_CURVE('',#11782,#11372,#9004,.T.);
#16193=EDGE_CURVE('',#11787,#11367,#9005,.T.);
#16194=EDGE_CURVE('',#11786,#11368,#9006,.T.);
#16195=EDGE_CURVE('',#11791,#11363,#9007,.T.);
#16196=EDGE_CURVE('',#11790,#11364,#9008,.T.);
#16197=EDGE_CURVE('',#11795,#11359,#9009,.T.);
#16198=EDGE_CURVE('',#11794,#11360,#9010,.T.);
#16199=EDGE_CURVE('',#11799,#11355,#9011,.T.);
#16200=EDGE_CURVE('',#11798,#11356,#9012,.T.);
#16201=EDGE_CURVE('',#11803,#11641,#9013,.T.);
#16202=EDGE_CURVE('',#11802,#11351,#9014,.T.);
#16203=EDGE_CURVE('',#11807,#11637,#9015,.T.);
#16204=EDGE_CURVE('',#11806,#11638,#9016,.T.);
#16205=EDGE_CURVE('',#11811,#11633,#9017,.T.);
#16206=EDGE_CURVE('',#11810,#11634,#9018,.T.);
#16207=EDGE_CURVE('',#11815,#11629,#9019,.T.);
#16208=EDGE_CURVE('',#11814,#11630,#9020,.T.);
#16209=EDGE_CURVE('',#11819,#11625,#9021,.T.);
#16210=EDGE_CURVE('',#11818,#11626,#9022,.T.);
#16211=EDGE_CURVE('',#11823,#11621,#9023,.T.);
#16212=EDGE_CURVE('',#11822,#11622,#9024,.T.);
#16213=EDGE_CURVE('',#11827,#11617,#9025,.T.);
#16214=EDGE_CURVE('',#11826,#11618,#9026,.T.);
#16215=EDGE_CURVE('',#11831,#11613,#9027,.T.);
#16216=EDGE_CURVE('',#11830,#11614,#9028,.T.);
#16217=EDGE_CURVE('',#11835,#11609,#9029,.T.);
#16218=EDGE_CURVE('',#11834,#11610,#9030,.T.);
#16219=EDGE_CURVE('',#11839,#11605,#9031,.T.);
#16220=EDGE_CURVE('',#11838,#11606,#9032,.T.);
#16221=EDGE_CURVE('',#11843,#11601,#9033,.T.);
#16222=EDGE_CURVE('',#11842,#11602,#9034,.T.);
#16223=EDGE_CURVE('',#11847,#11597,#9035,.T.);
#16224=EDGE_CURVE('',#11846,#11598,#9036,.T.);
#16225=EDGE_CURVE('',#11851,#11593,#9037,.T.);
#16226=EDGE_CURVE('',#11850,#11594,#9038,.T.);
#16227=EDGE_CURVE('',#11855,#11589,#9039,.T.);
#16228=EDGE_CURVE('',#11854,#11590,#9040,.T.);
#16229=EDGE_CURVE('',#11859,#11585,#9041,.T.);
#16230=EDGE_CURVE('',#11858,#11586,#9042,.T.);
#16231=EDGE_CURVE('',#11863,#11581,#9043,.T.);
#16232=EDGE_CURVE('',#11862,#11582,#9044,.T.);
#16233=EDGE_CURVE('',#11867,#11577,#9045,.T.);
#16234=EDGE_CURVE('',#11866,#11578,#9046,.T.);
#16235=EDGE_CURVE('',#11871,#11573,#9047,.T.);
#16236=EDGE_CURVE('',#11870,#11574,#9048,.T.);
#16237=EDGE_CURVE('',#11875,#11569,#9049,.T.);
#16238=EDGE_CURVE('',#11874,#11570,#9050,.T.);
#16239=EDGE_CURVE('',#11879,#11565,#9051,.T.);
#16240=EDGE_CURVE('',#11878,#11566,#9052,.T.);
#16241=EDGE_CURVE('',#12265,#12266,#9053,.T.);
#16242=EDGE_CURVE('',#12267,#12265,#3100,.F.);
#16243=EDGE_CURVE('',#12267,#12268,#9054,.T.);
#16244=EDGE_CURVE('',#12268,#12268,#3775,.T.);
#16245=EDGE_CURVE('',#12269,#12267,#3776,.T.);
#16246=EDGE_CURVE('',#12266,#12269,#3101,.F.);
#16247=EDGE_CURVE('',#12270,#12271,#9055,.T.);
#16248=EDGE_CURVE('',#12265,#12270,#3102,.F.);
#16249=EDGE_CURVE('',#12271,#12266,#3103,.F.);
#16250=EDGE_CURVE('',#12272,#12273,#9056,.T.);
#16251=EDGE_CURVE('',#12270,#12272,#3104,.F.);
#16252=EDGE_CURVE('',#12273,#12271,#3105,.F.);
#16253=EDGE_CURVE('',#12274,#12275,#9057,.T.);
#16254=EDGE_CURVE('',#12272,#12274,#3106,.F.);
#16255=EDGE_CURVE('',#12275,#12273,#3107,.F.);
#16256=EDGE_CURVE('',#12276,#12277,#9058,.T.);
#16257=EDGE_CURVE('',#12274,#12276,#3108,.F.);
#16258=EDGE_CURVE('',#12277,#12275,#3109,.F.);
#16259=EDGE_CURVE('',#12278,#12279,#9059,.T.);
#16260=EDGE_CURVE('',#12276,#12278,#3110,.F.);
#16261=EDGE_CURVE('',#12279,#12277,#3111,.F.);
#16262=EDGE_CURVE('',#12280,#12281,#9060,.T.);
#16263=EDGE_CURVE('',#12278,#12280,#3112,.F.);
#16264=EDGE_CURVE('',#12281,#12279,#3113,.F.);
#16265=EDGE_CURVE('',#12282,#12283,#9061,.T.);
#16266=EDGE_CURVE('',#12280,#12282,#3114,.F.);
#16267=EDGE_CURVE('',#12283,#12281,#3115,.F.);
#16268=EDGE_CURVE('',#12284,#12285,#9062,.T.);
#16269=EDGE_CURVE('',#12282,#12284,#3116,.F.);
#16270=EDGE_CURVE('',#12285,#12283,#3117,.F.);
#16271=EDGE_CURVE('',#12286,#12287,#9063,.T.);
#16272=EDGE_CURVE('',#12284,#12286,#3118,.F.);
#16273=EDGE_CURVE('',#12287,#12285,#3119,.F.);
#16274=EDGE_CURVE('',#12288,#12289,#9064,.T.);
#16275=EDGE_CURVE('',#12286,#12288,#3120,.F.);
#16276=EDGE_CURVE('',#12289,#12287,#3121,.F.);
#16277=EDGE_CURVE('',#12290,#12291,#9065,.T.);
#16278=EDGE_CURVE('',#12288,#12290,#3122,.F.);
#16279=EDGE_CURVE('',#12291,#12289,#3123,.F.);
#16280=EDGE_CURVE('',#12292,#12293,#9066,.T.);
#16281=EDGE_CURVE('',#12290,#12292,#3124,.F.);
#16282=EDGE_CURVE('',#12293,#12291,#3125,.F.);
#16283=EDGE_CURVE('',#12294,#12295,#9067,.T.);
#16284=EDGE_CURVE('',#12292,#12294,#3126,.F.);
#16285=EDGE_CURVE('',#12295,#12293,#3127,.F.);
#16286=EDGE_CURVE('',#12296,#12297,#9068,.T.);
#16287=EDGE_CURVE('',#12294,#12296,#3128,.F.);
#16288=EDGE_CURVE('',#12297,#12295,#3129,.F.);
#16289=EDGE_CURVE('',#12298,#12299,#9069,.T.);
#16290=EDGE_CURVE('',#12296,#12298,#3130,.F.);
#16291=EDGE_CURVE('',#12299,#12297,#3131,.F.);
#16292=EDGE_CURVE('',#12300,#12301,#9070,.T.);
#16293=EDGE_CURVE('',#12298,#12300,#3132,.F.);
#16294=EDGE_CURVE('',#12301,#12299,#3133,.F.);
#16295=EDGE_CURVE('',#12302,#12303,#9071,.T.);
#16296=EDGE_CURVE('',#12300,#12302,#3134,.F.);
#16297=EDGE_CURVE('',#12303,#12301,#3135,.F.);
#16298=EDGE_CURVE('',#12304,#12305,#9072,.T.);
#16299=EDGE_CURVE('',#12302,#12304,#3136,.F.);
#16300=EDGE_CURVE('',#12305,#12303,#3137,.F.);
#16301=EDGE_CURVE('',#12306,#12307,#9073,.T.);
#16302=EDGE_CURVE('',#12304,#12306,#3138,.F.);
#16303=EDGE_CURVE('',#12307,#12305,#3139,.F.);
#16304=EDGE_CURVE('',#12308,#12309,#9074,.T.);
#16305=EDGE_CURVE('',#12306,#12308,#3140,.F.);
#16306=EDGE_CURVE('',#12309,#12307,#3141,.F.);
#16307=EDGE_CURVE('',#12310,#12311,#9075,.T.);
#16308=EDGE_CURVE('',#12308,#12310,#3142,.F.);
#16309=EDGE_CURVE('',#12311,#12309,#3143,.F.);
#16310=EDGE_CURVE('',#12312,#12313,#9076,.T.);
#16311=EDGE_CURVE('',#12310,#12312,#3144,.F.);
#16312=EDGE_CURVE('',#12313,#12311,#3145,.F.);
#16313=EDGE_CURVE('',#12314,#12315,#9077,.T.);
#16314=EDGE_CURVE('',#12312,#12314,#3146,.F.);
#16315=EDGE_CURVE('',#12315,#12313,#3147,.F.);
#16316=EDGE_CURVE('',#12316,#12317,#9078,.T.);
#16317=EDGE_CURVE('',#12314,#12316,#3148,.F.);
#16318=EDGE_CURVE('',#12317,#12315,#3149,.F.);
#16319=EDGE_CURVE('',#12318,#12319,#9079,.T.);
#16320=EDGE_CURVE('',#12316,#12318,#3150,.F.);
#16321=EDGE_CURVE('',#12319,#12317,#3151,.F.);
#16322=EDGE_CURVE('',#12320,#12321,#9080,.T.);
#16323=EDGE_CURVE('',#12318,#12320,#3152,.F.);
#16324=EDGE_CURVE('',#12321,#12319,#3153,.F.);
#16325=EDGE_CURVE('',#12322,#12323,#9081,.T.);
#16326=EDGE_CURVE('',#12320,#12322,#3154,.F.);
#16327=EDGE_CURVE('',#12323,#12321,#3155,.F.);
#16328=EDGE_CURVE('',#12324,#12325,#9082,.T.);
#16329=EDGE_CURVE('',#12324,#12326,#3156,.F.);
#16330=EDGE_CURVE('',#12325,#12326,#3777,.T.);
#16331=EDGE_CURVE('',#12327,#12326,#9083,.T.);
#16332=EDGE_CURVE('',#12328,#12327,#3157,.F.);
#16333=EDGE_CURVE('',#12326,#12328,#3778,.T.);
#16334=EDGE_CURVE('',#12329,#12330,#9084,.T.);
#16335=EDGE_CURVE('',#12327,#12329,#3158,.F.);
#16336=EDGE_CURVE('',#12326,#12330,#3159,.T.);
#16337=EDGE_CURVE('',#12331,#12332,#9085,.T.);
#16338=EDGE_CURVE('',#12329,#12331,#3160,.F.);
#16339=EDGE_CURVE('',#12330,#12332,#3161,.T.);
#16340=EDGE_CURVE('',#12333,#12334,#9086,.T.);
#16341=EDGE_CURVE('',#12331,#12333,#3162,.F.);
#16342=EDGE_CURVE('',#12332,#12334,#3163,.T.);
#16343=EDGE_CURVE('',#12335,#12336,#9087,.T.);
#16344=EDGE_CURVE('',#12333,#12335,#3164,.F.);
#16345=EDGE_CURVE('',#12334,#12336,#3165,.T.);
#16346=EDGE_CURVE('',#12337,#12338,#9088,.T.);
#16347=EDGE_CURVE('',#12335,#12337,#3166,.F.);
#16348=EDGE_CURVE('',#12336,#12338,#3167,.T.);
#16349=EDGE_CURVE('',#12339,#12340,#9089,.T.);
#16350=EDGE_CURVE('',#12337,#12339,#3168,.F.);
#16351=EDGE_CURVE('',#12338,#12340,#3169,.T.);
#16352=EDGE_CURVE('',#12341,#12342,#9090,.T.);
#16353=EDGE_CURVE('',#12339,#12341,#3170,.F.);
#16354=EDGE_CURVE('',#12340,#12342,#3171,.T.);
#16355=EDGE_CURVE('',#12343,#12344,#9091,.T.);
#16356=EDGE_CURVE('',#12341,#12343,#3172,.F.);
#16357=EDGE_CURVE('',#12342,#12344,#3173,.T.);
#16358=EDGE_CURVE('',#12345,#12346,#9092,.T.);
#16359=EDGE_CURVE('',#12343,#12345,#3174,.F.);
#16360=EDGE_CURVE('',#12344,#12346,#3175,.T.);
#16361=EDGE_CURVE('',#12347,#12348,#9093,.T.);
#16362=EDGE_CURVE('',#12345,#12347,#3176,.F.);
#16363=EDGE_CURVE('',#12346,#12348,#3177,.T.);
#16364=EDGE_CURVE('',#12349,#12350,#9094,.T.);
#16365=EDGE_CURVE('',#12347,#12349,#3178,.F.);
#16366=EDGE_CURVE('',#12348,#12350,#3179,.T.);
#16367=EDGE_CURVE('',#12351,#12352,#9095,.T.);
#16368=EDGE_CURVE('',#12349,#12351,#3180,.F.);
#16369=EDGE_CURVE('',#12350,#12352,#3181,.T.);
#16370=EDGE_CURVE('',#12353,#12354,#9096,.T.);
#16371=EDGE_CURVE('',#12351,#12353,#3182,.F.);
#16372=EDGE_CURVE('',#12352,#12354,#3183,.T.);
#16373=EDGE_CURVE('',#12355,#12356,#9097,.T.);
#16374=EDGE_CURVE('',#12353,#12355,#3184,.F.);
#16375=EDGE_CURVE('',#12354,#12356,#3185,.T.);
#16376=EDGE_CURVE('',#12357,#12358,#9098,.T.);
#16377=EDGE_CURVE('',#12355,#12357,#3186,.F.);
#16378=EDGE_CURVE('',#12356,#12358,#3187,.T.);
#16379=EDGE_CURVE('',#12359,#12360,#9099,.T.);
#16380=EDGE_CURVE('',#12357,#12359,#3188,.F.);
#16381=EDGE_CURVE('',#12358,#12360,#3189,.T.);
#16382=EDGE_CURVE('',#12361,#12362,#9100,.T.);
#16383=EDGE_CURVE('',#12359,#12361,#3190,.F.);
#16384=EDGE_CURVE('',#12360,#12362,#3191,.T.);
#16385=EDGE_CURVE('',#12363,#12364,#9101,.T.);
#16386=EDGE_CURVE('',#12361,#12363,#3192,.F.);
#16387=EDGE_CURVE('',#12362,#12364,#3193,.T.);
#16388=EDGE_CURVE('',#12365,#12366,#9102,.T.);
#16389=EDGE_CURVE('',#12363,#12365,#3194,.F.);
#16390=EDGE_CURVE('',#12364,#12366,#3195,.T.);
#16391=EDGE_CURVE('',#12367,#12368,#9103,.T.);
#16392=EDGE_CURVE('',#12365,#12367,#3196,.F.);
#16393=EDGE_CURVE('',#12366,#12368,#3197,.T.);
#16394=EDGE_CURVE('',#12369,#12370,#9104,.T.);
#16395=EDGE_CURVE('',#12367,#12369,#3198,.F.);
#16396=EDGE_CURVE('',#12368,#12370,#3199,.T.);
#16397=EDGE_CURVE('',#12371,#12372,#9105,.T.);
#16398=EDGE_CURVE('',#12369,#12371,#3200,.F.);
#16399=EDGE_CURVE('',#12370,#12372,#3201,.T.);
#16400=EDGE_CURVE('',#12373,#12374,#9106,.T.);
#16401=EDGE_CURVE('',#12371,#12373,#3202,.F.);
#16402=EDGE_CURVE('',#12372,#12374,#3203,.T.);
#16403=EDGE_CURVE('',#12375,#12376,#9107,.T.);
#16404=EDGE_CURVE('',#12373,#12375,#3204,.F.);
#16405=EDGE_CURVE('',#12374,#12376,#3205,.T.);
#16406=EDGE_CURVE('',#12377,#12378,#9108,.T.);
#16407=EDGE_CURVE('',#12375,#12377,#3206,.F.);
#16408=EDGE_CURVE('',#12376,#12378,#3207,.T.);
#16409=EDGE_CURVE('',#12379,#12380,#9109,.T.);
#16410=EDGE_CURVE('',#12377,#12379,#3208,.F.);
#16411=EDGE_CURVE('',#12378,#12380,#3209,.T.);
#16412=EDGE_CURVE('',#12381,#12382,#9110,.T.);
#16413=EDGE_CURVE('',#12379,#12381,#3210,.F.);
#16414=EDGE_CURVE('',#12380,#12382,#3211,.T.);
#16415=EDGE_CURVE('',#12383,#12384,#9111,.T.);
#16416=EDGE_CURVE('',#12381,#12383,#3212,.F.);
#16417=EDGE_CURVE('',#12382,#12384,#3213,.T.);
#16418=EDGE_CURVE('',#12385,#12386,#9112,.T.);
#16419=EDGE_CURVE('',#12383,#12385,#3214,.F.);
#16420=EDGE_CURVE('',#12384,#12386,#3215,.T.);
#16421=EDGE_CURVE('',#12386,#12387,#3216,.T.);
#16422=EDGE_CURVE('',#12385,#12387,#3779,.T.);
#16423=EDGE_CURVE('',#12328,#12325,#3780,.T.);
#16424=EDGE_CURVE('',#12328,#12388,#3217,.T.);
#16425=EDGE_CURVE('',#12388,#12389,#3781,.T.);
#16426=EDGE_CURVE('',#12389,#12324,#3218,.F.);
#16427=EDGE_CURVE('',#12389,#12323,#3219,.F.);
#16428=EDGE_CURVE('',#12322,#12388,#3220,.F.);
#16429=EDGE_CURVE('',#12390,#12391,#2000,.T.);
#16430=EDGE_CURVE('',#12391,#12392,#9113,.T.);
#16431=EDGE_CURVE('',#12392,#12393,#2001,.T.);
#16432=EDGE_CURVE('',#12390,#12393,#9114,.T.);
#16433=EDGE_CURVE('',#12394,#12395,#2002,.T.);
#16434=EDGE_CURVE('',#12395,#12396,#9115,.T.);
#16435=EDGE_CURVE('',#12396,#12397,#2003,.T.);
#16436=EDGE_CURVE('',#12394,#12397,#9116,.T.);
#16437=EDGE_CURVE('',#12398,#12399,#2004,.T.);
#16438=EDGE_CURVE('',#12399,#12400,#9117,.T.);
#16439=EDGE_CURVE('',#12400,#12401,#2005,.T.);
#16440=EDGE_CURVE('',#12398,#12401,#9118,.T.);
#16441=EDGE_CURVE('',#12402,#12403,#2006,.T.);
#16442=EDGE_CURVE('',#12403,#12404,#9119,.T.);
#16443=EDGE_CURVE('',#12404,#12405,#2007,.T.);
#16444=EDGE_CURVE('',#12402,#12405,#9120,.T.);
#16445=EDGE_CURVE('',#12406,#12407,#2008,.T.);
#16446=EDGE_CURVE('',#12407,#12408,#9121,.T.);
#16447=EDGE_CURVE('',#12408,#12409,#2009,.T.);
#16448=EDGE_CURVE('',#12406,#12409,#9122,.T.);
#16449=EDGE_CURVE('',#12410,#12411,#2010,.T.);
#16450=EDGE_CURVE('',#12411,#12412,#9123,.T.);
#16451=EDGE_CURVE('',#12412,#12413,#2011,.T.);
#16452=EDGE_CURVE('',#12410,#12413,#9124,.T.);
#16453=EDGE_CURVE('',#12414,#12415,#2012,.T.);
#16454=EDGE_CURVE('',#12415,#12416,#9125,.T.);
#16455=EDGE_CURVE('',#12416,#12417,#2013,.T.);
#16456=EDGE_CURVE('',#12414,#12417,#9126,.T.);
#16457=EDGE_CURVE('',#12418,#12419,#2014,.T.);
#16458=EDGE_CURVE('',#12419,#12420,#9127,.T.);
#16459=EDGE_CURVE('',#12420,#12421,#2015,.T.);
#16460=EDGE_CURVE('',#12418,#12421,#9128,.T.);
#16461=EDGE_CURVE('',#12422,#12423,#2016,.T.);
#16462=EDGE_CURVE('',#12423,#12424,#9129,.T.);
#16463=EDGE_CURVE('',#12424,#12425,#2017,.T.);
#16464=EDGE_CURVE('',#12422,#12425,#9130,.T.);
#16465=EDGE_CURVE('',#12426,#12427,#2018,.T.);
#16466=EDGE_CURVE('',#12427,#12428,#9131,.T.);
#16467=EDGE_CURVE('',#12428,#12429,#2019,.T.);
#16468=EDGE_CURVE('',#12426,#12429,#9132,.T.);
#16469=EDGE_CURVE('',#12430,#12431,#2020,.T.);
#16470=EDGE_CURVE('',#12431,#12432,#9133,.T.);
#16471=EDGE_CURVE('',#12432,#12433,#2021,.T.);
#16472=EDGE_CURVE('',#12430,#12433,#9134,.T.);
#16473=EDGE_CURVE('',#12434,#12435,#2022,.T.);
#16474=EDGE_CURVE('',#12435,#12436,#9135,.T.);
#16475=EDGE_CURVE('',#12436,#12437,#2023,.T.);
#16476=EDGE_CURVE('',#12434,#12437,#9136,.T.);
#16477=EDGE_CURVE('',#12438,#12439,#2024,.T.);
#16478=EDGE_CURVE('',#12439,#12440,#9137,.T.);
#16479=EDGE_CURVE('',#12440,#12441,#2025,.T.);
#16480=EDGE_CURVE('',#12438,#12441,#9138,.T.);
#16481=EDGE_CURVE('',#12442,#12443,#2026,.T.);
#16482=EDGE_CURVE('',#12443,#12444,#9139,.T.);
#16483=EDGE_CURVE('',#12444,#12445,#2027,.T.);
#16484=EDGE_CURVE('',#12442,#12445,#9140,.T.);
#16485=EDGE_CURVE('',#12446,#12447,#2028,.T.);
#16486=EDGE_CURVE('',#12447,#12448,#9141,.T.);
#16487=EDGE_CURVE('',#12448,#12449,#2029,.T.);
#16488=EDGE_CURVE('',#12446,#12449,#9142,.T.);
#16489=EDGE_CURVE('',#12450,#12451,#868,.T.);
#16490=EDGE_CURVE('',#12452,#12450,#869,.T.);
#16491=EDGE_CURVE('',#12453,#12452,#870,.T.);
#16492=EDGE_CURVE('',#12454,#12453,#871,.T.);
#16493=EDGE_CURVE('',#12455,#12454,#872,.T.);
#16494=EDGE_CURVE('',#12456,#12455,#873,.T.);
#16495=EDGE_CURVE('',#12451,#12456,#874,.T.);
#16496=EDGE_CURVE('',#12451,#12457,#9143,.T.);
#16497=EDGE_CURVE('',#12457,#12457,#3782,.T.);
#16498=EDGE_CURVE('',#12458,#12458,#3783,.T.);
#16499=EDGE_CURVE('',#12458,#12459,#3784,.T.);
#16500=EDGE_CURVE('',#12459,#12459,#3785,.T.);
#16501=EDGE_CURVE('',#12460,#12461,#3221,.T.);
#16502=EDGE_CURVE('',#12462,#12460,#875,.T.);
#16503=EDGE_CURVE('',#12463,#12462,#3786,.T.);
#16504=EDGE_CURVE('',#12464,#12463,#876,.T.);
#16505=EDGE_CURVE('',#12465,#12464,#2030,.T.);
#16506=EDGE_CURVE('',#12466,#12465,#877,.T.);
#16507=EDGE_CURVE('',#12467,#12466,#3787,.T.);
#16508=EDGE_CURVE('',#12468,#12467,#878,.T.);
#16509=EDGE_CURVE('',#12469,#12468,#2031,.T.);
#16510=EDGE_CURVE('',#12470,#12469,#879,.T.);
#16511=EDGE_CURVE('',#12471,#12470,#3788,.T.);
#16512=EDGE_CURVE('',#12472,#12471,#880,.T.);
#16513=EDGE_CURVE('',#12473,#12472,#2032,.T.);
#16514=EDGE_CURVE('',#12474,#12473,#881,.T.);
#16515=EDGE_CURVE('',#12475,#12474,#3789,.T.);
#16516=EDGE_CURVE('',#12476,#12475,#882,.T.);
#16517=EDGE_CURVE('',#12477,#12476,#2033,.T.);
#16518=EDGE_CURVE('',#12478,#12477,#883,.T.);
#16519=EDGE_CURVE('',#12479,#12478,#3790,.T.);
#16520=EDGE_CURVE('',#12480,#12479,#884,.T.);
#16521=EDGE_CURVE('',#12481,#12480,#2034,.T.);
#16522=EDGE_CURVE('',#12482,#12481,#885,.T.);
#16523=EDGE_CURVE('',#12483,#12482,#3791,.T.);
#16524=EDGE_CURVE('',#12484,#12483,#886,.T.);
#16525=EDGE_CURVE('',#12485,#12484,#2035,.T.);
#16526=EDGE_CURVE('',#12486,#12485,#887,.T.);
#16527=EDGE_CURVE('',#12487,#12486,#3792,.T.);
#16528=EDGE_CURVE('',#12488,#12487,#888,.T.);
#16529=EDGE_CURVE('',#12489,#12488,#2036,.T.);
#16530=EDGE_CURVE('',#12490,#12489,#889,.T.);
#16531=EDGE_CURVE('',#12491,#12490,#3793,.T.);
#16532=EDGE_CURVE('',#12492,#12491,#890,.T.);
#16533=EDGE_CURVE('',#12493,#12492,#2037,.T.);
#16534=EDGE_CURVE('',#12494,#12493,#891,.T.);
#16535=EDGE_CURVE('',#12495,#12494,#3794,.T.);
#16536=EDGE_CURVE('',#12496,#12495,#892,.T.);
#16537=EDGE_CURVE('',#12497,#12496,#2038,.T.);
#16538=EDGE_CURVE('',#12498,#12497,#893,.T.);
#16539=EDGE_CURVE('',#12499,#12498,#3795,.T.);
#16540=EDGE_CURVE('',#12500,#12499,#894,.T.);
#16541=EDGE_CURVE('',#12501,#12500,#2039,.T.);
#16542=EDGE_CURVE('',#12502,#12501,#895,.T.);
#16543=EDGE_CURVE('',#12503,#12502,#3796,.T.);
#16544=EDGE_CURVE('',#12504,#12503,#896,.T.);
#16545=EDGE_CURVE('',#12505,#12504,#2040,.T.);
#16546=EDGE_CURVE('',#12506,#12505,#897,.T.);
#16547=EDGE_CURVE('',#12507,#12506,#3797,.T.);
#16548=EDGE_CURVE('',#12508,#12507,#898,.T.);
#16549=EDGE_CURVE('',#12509,#12508,#2041,.T.);
#16550=EDGE_CURVE('',#12510,#12509,#899,.T.);
#16551=EDGE_CURVE('',#12511,#12510,#3798,.T.);
#16552=EDGE_CURVE('',#12512,#12511,#900,.T.);
#16553=EDGE_CURVE('',#12513,#12512,#2042,.T.);
#16554=EDGE_CURVE('',#12514,#12513,#901,.T.);
#16555=EDGE_CURVE('',#12515,#12514,#3799,.T.);
#16556=EDGE_CURVE('',#12516,#12515,#902,.T.);
#16557=EDGE_CURVE('',#12517,#12516,#2043,.T.);
#16558=EDGE_CURVE('',#12518,#12517,#903,.T.);
#16559=EDGE_CURVE('',#12519,#12518,#3800,.T.);
#16560=EDGE_CURVE('',#12520,#12519,#904,.T.);
#16561=EDGE_CURVE('',#12521,#12520,#2044,.T.);
#16562=EDGE_CURVE('',#12522,#12521,#905,.T.);
#16563=EDGE_CURVE('',#12523,#12522,#3801,.T.);
#16564=EDGE_CURVE('',#12524,#12523,#906,.T.);
#16565=EDGE_CURVE('',#12525,#12524,#2045,.T.);
#16566=EDGE_CURVE('',#12526,#12525,#907,.T.);
#16567=EDGE_CURVE('',#12527,#12526,#3802,.T.);
#16568=EDGE_CURVE('',#12528,#12527,#908,.T.);
#16569=EDGE_CURVE('',#12529,#12528,#2046,.T.);
#16570=EDGE_CURVE('',#12530,#12529,#909,.T.);
#16571=EDGE_CURVE('',#12531,#12530,#3803,.T.);
#16572=EDGE_CURVE('',#12532,#12531,#910,.T.);
#16573=EDGE_CURVE('',#12533,#12532,#2047,.T.);
#16574=EDGE_CURVE('',#12534,#12533,#911,.T.);
#16575=EDGE_CURVE('',#12535,#12534,#3804,.T.);
#16576=EDGE_CURVE('',#12536,#12535,#912,.T.);
#16577=EDGE_CURVE('',#12537,#12536,#2048,.T.);
#16578=EDGE_CURVE('',#12538,#12537,#913,.T.);
#16579=EDGE_CURVE('',#12539,#12538,#3805,.T.);
#16580=EDGE_CURVE('',#12540,#12539,#914,.T.);
#16581=EDGE_CURVE('',#12541,#12540,#2049,.T.);
#16582=EDGE_CURVE('',#12542,#12541,#915,.T.);
#16583=EDGE_CURVE('',#12543,#12542,#3806,.T.);
#16584=EDGE_CURVE('',#12544,#12543,#916,.T.);
#16585=EDGE_CURVE('',#12545,#12544,#2050,.T.);
#16586=EDGE_CURVE('',#12546,#12545,#917,.T.);
#16587=EDGE_CURVE('',#12547,#12546,#3807,.T.);
#16588=EDGE_CURVE('',#12548,#12547,#918,.T.);
#16589=EDGE_CURVE('',#12549,#12548,#2051,.T.);
#16590=EDGE_CURVE('',#12550,#12549,#919,.T.);
#16591=EDGE_CURVE('',#12551,#12550,#3808,.T.);
#16592=EDGE_CURVE('',#12552,#12551,#920,.T.);
#16593=EDGE_CURVE('',#12553,#12552,#2052,.T.);
#16594=EDGE_CURVE('',#12554,#12553,#921,.T.);
#16595=EDGE_CURVE('',#12555,#12554,#3809,.T.);
#16596=EDGE_CURVE('',#12556,#12555,#922,.T.);
#16597=EDGE_CURVE('',#12557,#12556,#2053,.T.);
#16598=EDGE_CURVE('',#12558,#12557,#923,.T.);
#16599=EDGE_CURVE('',#12559,#12558,#3810,.T.);
#16600=EDGE_CURVE('',#12560,#12559,#924,.T.);
#16601=EDGE_CURVE('',#12561,#12560,#2054,.T.);
#16602=EDGE_CURVE('',#12562,#12561,#925,.T.);
#16603=EDGE_CURVE('',#12563,#12562,#3811,.T.);
#16604=EDGE_CURVE('',#12564,#12563,#926,.T.);
#16605=EDGE_CURVE('',#12565,#12564,#2055,.T.);
#16606=EDGE_CURVE('',#12566,#12565,#927,.T.);
#16607=EDGE_CURVE('',#12567,#12566,#3812,.T.);
#16608=EDGE_CURVE('',#12568,#12567,#928,.T.);
#16609=EDGE_CURVE('',#12569,#12568,#2056,.T.);
#16610=EDGE_CURVE('',#12570,#12569,#929,.T.);
#16611=EDGE_CURVE('',#12571,#12570,#3813,.T.);
#16612=EDGE_CURVE('',#12572,#12571,#930,.T.);
#16613=EDGE_CURVE('',#12573,#12572,#2057,.T.);
#16614=EDGE_CURVE('',#12574,#12573,#931,.T.);
#16615=EDGE_CURVE('',#12575,#12574,#3814,.T.);
#16616=EDGE_CURVE('',#12576,#12575,#932,.T.);
#16617=EDGE_CURVE('',#12577,#12576,#2058,.T.);
#16618=EDGE_CURVE('',#12578,#12577,#933,.T.);
#16619=EDGE_CURVE('',#12579,#12578,#3815,.T.);
#16620=EDGE_CURVE('',#12580,#12579,#934,.T.);
#16621=EDGE_CURVE('',#12581,#12580,#2059,.T.);
#16622=EDGE_CURVE('',#12582,#12581,#935,.T.);
#16623=EDGE_CURVE('',#12583,#12582,#3816,.T.);
#16624=EDGE_CURVE('',#12584,#12583,#936,.T.);
#16625=EDGE_CURVE('',#12585,#12584,#2060,.T.);
#16626=EDGE_CURVE('',#12586,#12585,#937,.T.);
#16627=EDGE_CURVE('',#12587,#12586,#3817,.T.);
#16628=EDGE_CURVE('',#12588,#12587,#938,.T.);
#16629=EDGE_CURVE('',#12589,#12588,#2061,.T.);
#16630=EDGE_CURVE('',#12590,#12589,#939,.T.);
#16631=EDGE_CURVE('',#12591,#12590,#3818,.T.);
#16632=EDGE_CURVE('',#12592,#12591,#940,.T.);
#16633=EDGE_CURVE('',#12593,#12592,#2062,.T.);
#16634=EDGE_CURVE('',#12594,#12593,#941,.T.);
#16635=EDGE_CURVE('',#12595,#12594,#3819,.T.);
#16636=EDGE_CURVE('',#12596,#12595,#942,.T.);
#16637=EDGE_CURVE('',#12597,#12596,#2063,.T.);
#16638=EDGE_CURVE('',#12598,#12597,#943,.T.);
#16639=EDGE_CURVE('',#12599,#12598,#3820,.T.);
#16640=EDGE_CURVE('',#12600,#12599,#944,.T.);
#16641=EDGE_CURVE('',#12601,#12600,#2064,.T.);
#16642=EDGE_CURVE('',#12602,#12601,#945,.T.);
#16643=EDGE_CURVE('',#12603,#12602,#3821,.T.);
#16644=EDGE_CURVE('',#12604,#12603,#946,.T.);
#16645=EDGE_CURVE('',#12605,#12604,#2065,.T.);
#16646=EDGE_CURVE('',#12606,#12605,#947,.T.);
#16647=EDGE_CURVE('',#12607,#12606,#3822,.T.);
#16648=EDGE_CURVE('',#12608,#12607,#948,.T.);
#16649=EDGE_CURVE('',#12609,#12608,#2066,.T.);
#16650=EDGE_CURVE('',#12610,#12609,#949,.T.);
#16651=EDGE_CURVE('',#12611,#12610,#3823,.T.);
#16652=EDGE_CURVE('',#12612,#12611,#950,.T.);
#16653=EDGE_CURVE('',#12613,#12612,#2067,.T.);
#16654=EDGE_CURVE('',#12614,#12613,#951,.T.);
#16655=EDGE_CURVE('',#12615,#12614,#3824,.T.);
#16656=EDGE_CURVE('',#12616,#12615,#952,.T.);
#16657=EDGE_CURVE('',#12617,#12616,#2068,.T.);
#16658=EDGE_CURVE('',#12618,#12617,#953,.T.);
#16659=EDGE_CURVE('',#12619,#12618,#3825,.T.);
#16660=EDGE_CURVE('',#12620,#12619,#954,.T.);
#16661=EDGE_CURVE('',#12621,#12620,#2069,.T.);
#16662=EDGE_CURVE('',#12622,#12621,#955,.T.);
#16663=EDGE_CURVE('',#12623,#12622,#3826,.T.);
#16664=EDGE_CURVE('',#12624,#12623,#956,.T.);
#16665=EDGE_CURVE('',#12625,#12624,#2070,.T.);
#16666=EDGE_CURVE('',#12626,#12625,#957,.T.);
#16667=EDGE_CURVE('',#12627,#12626,#3827,.T.);
#16668=EDGE_CURVE('',#12628,#12627,#958,.T.);
#16669=EDGE_CURVE('',#12629,#12628,#2071,.T.);
#16670=EDGE_CURVE('',#12630,#12629,#959,.T.);
#16671=EDGE_CURVE('',#12631,#12630,#3828,.T.);
#16672=EDGE_CURVE('',#12632,#12631,#960,.T.);
#16673=EDGE_CURVE('',#12633,#12632,#2072,.T.);
#16674=EDGE_CURVE('',#12634,#12633,#961,.T.);
#16675=EDGE_CURVE('',#12635,#12634,#3829,.T.);
#16676=EDGE_CURVE('',#12636,#12635,#962,.T.);
#16677=EDGE_CURVE('',#12637,#12636,#2073,.T.);
#16678=EDGE_CURVE('',#12638,#12637,#963,.T.);
#16679=EDGE_CURVE('',#12639,#12638,#3830,.T.);
#16680=EDGE_CURVE('',#12640,#12639,#964,.T.);
#16681=EDGE_CURVE('',#12641,#12640,#2074,.T.);
#16682=EDGE_CURVE('',#12642,#12641,#965,.T.);
#16683=EDGE_CURVE('',#12643,#12642,#3831,.T.);
#16684=EDGE_CURVE('',#12449,#12643,#966,.T.);
#16685=EDGE_CURVE('',#12644,#12448,#967,.T.);
#16686=EDGE_CURVE('',#12645,#12644,#3832,.T.);
#16687=EDGE_CURVE('',#12445,#12645,#968,.T.);
#16688=EDGE_CURVE('',#12646,#12444,#969,.T.);
#16689=EDGE_CURVE('',#12647,#12646,#3833,.T.);
#16690=EDGE_CURVE('',#12441,#12647,#970,.T.);
#16691=EDGE_CURVE('',#12648,#12440,#971,.T.);
#16692=EDGE_CURVE('',#12649,#12648,#3834,.T.);
#16693=EDGE_CURVE('',#12437,#12649,#972,.T.);
#16694=EDGE_CURVE('',#12650,#12436,#973,.T.);
#16695=EDGE_CURVE('',#12651,#12650,#3835,.T.);
#16696=EDGE_CURVE('',#12433,#12651,#974,.T.);
#16697=EDGE_CURVE('',#12652,#12432,#975,.T.);
#16698=EDGE_CURVE('',#12653,#12652,#3836,.T.);
#16699=EDGE_CURVE('',#12429,#12653,#976,.T.);
#16700=EDGE_CURVE('',#12654,#12428,#977,.T.);
#16701=EDGE_CURVE('',#12655,#12654,#3837,.T.);
#16702=EDGE_CURVE('',#12425,#12655,#978,.T.);
#16703=EDGE_CURVE('',#12656,#12424,#979,.T.);
#16704=EDGE_CURVE('',#12657,#12656,#3838,.T.);
#16705=EDGE_CURVE('',#12421,#12657,#980,.T.);
#16706=EDGE_CURVE('',#12658,#12420,#981,.T.);
#16707=EDGE_CURVE('',#12659,#12658,#3839,.T.);
#16708=EDGE_CURVE('',#12417,#12659,#982,.T.);
#16709=EDGE_CURVE('',#12660,#12416,#983,.T.);
#16710=EDGE_CURVE('',#12661,#12660,#3840,.T.);
#16711=EDGE_CURVE('',#12393,#12661,#984,.T.);
#16712=EDGE_CURVE('',#12662,#12392,#985,.T.);
#16713=EDGE_CURVE('',#12663,#12662,#3841,.T.);
#16714=EDGE_CURVE('',#12397,#12663,#986,.T.);
#16715=EDGE_CURVE('',#12664,#12396,#987,.T.);
#16716=EDGE_CURVE('',#12665,#12664,#3842,.T.);
#16717=EDGE_CURVE('',#12401,#12665,#988,.T.);
#16718=EDGE_CURVE('',#12666,#12400,#989,.T.);
#16719=EDGE_CURVE('',#12667,#12666,#3843,.T.);
#16720=EDGE_CURVE('',#12405,#12667,#990,.T.);
#16721=EDGE_CURVE('',#12668,#12404,#991,.T.);
#16722=EDGE_CURVE('',#12669,#12668,#3844,.T.);
#16723=EDGE_CURVE('',#12409,#12669,#992,.T.);
#16724=EDGE_CURVE('',#12670,#12408,#993,.T.);
#16725=EDGE_CURVE('',#12671,#12670,#3845,.T.);
#16726=EDGE_CURVE('',#12413,#12671,#994,.T.);
#16727=EDGE_CURVE('',#12672,#12412,#995,.T.);
#16728=EDGE_CURVE('',#12673,#12672,#3846,.T.);
#16729=EDGE_CURVE('',#12674,#12673,#996,.T.);
#16730=EDGE_CURVE('',#12675,#12674,#2075,.T.);
#16731=EDGE_CURVE('',#12676,#12675,#997,.T.);
#16732=EDGE_CURVE('',#12677,#12676,#3847,.T.);
#16733=EDGE_CURVE('',#12678,#12677,#998,.T.);
#16734=EDGE_CURVE('',#12679,#12678,#2076,.T.);
#16735=EDGE_CURVE('',#12680,#12679,#999,.T.);
#16736=EDGE_CURVE('',#12681,#12680,#3848,.T.);
#16737=EDGE_CURVE('',#12682,#12681,#1000,.T.);
#16738=EDGE_CURVE('',#12683,#12682,#2077,.T.);
#16739=EDGE_CURVE('',#12684,#12683,#1001,.T.);
#16740=EDGE_CURVE('',#12685,#12684,#3849,.T.);
#16741=EDGE_CURVE('',#12686,#12685,#1002,.T.);
#16742=EDGE_CURVE('',#12687,#12686,#2078,.T.);
#16743=EDGE_CURVE('',#12688,#12687,#1003,.T.);
#16744=EDGE_CURVE('',#12689,#12688,#3850,.T.);
#16745=EDGE_CURVE('',#12690,#12689,#1004,.T.);
#16746=EDGE_CURVE('',#12691,#12690,#2079,.T.);
#16747=EDGE_CURVE('',#12692,#12691,#1005,.T.);
#16748=EDGE_CURVE('',#12693,#12692,#3851,.T.);
#16749=EDGE_CURVE('',#12694,#12693,#1006,.T.);
#16750=EDGE_CURVE('',#12695,#12694,#2080,.T.);
#16751=EDGE_CURVE('',#12696,#12695,#1007,.T.);
#16752=EDGE_CURVE('',#12697,#12696,#3852,.T.);
#16753=EDGE_CURVE('',#12698,#12697,#1008,.T.);
#16754=EDGE_CURVE('',#12699,#12698,#2081,.T.);
#16755=EDGE_CURVE('',#12700,#12699,#1009,.T.);
#16756=EDGE_CURVE('',#12701,#12700,#3853,.T.);
#16757=EDGE_CURVE('',#12702,#12701,#1010,.T.);
#16758=EDGE_CURVE('',#12703,#12702,#2082,.T.);
#16759=EDGE_CURVE('',#12704,#12703,#1011,.T.);
#16760=EDGE_CURVE('',#12705,#12704,#3854,.T.);
#16761=EDGE_CURVE('',#12706,#12705,#1012,.T.);
#16762=EDGE_CURVE('',#12707,#12706,#2083,.T.);
#16763=EDGE_CURVE('',#12708,#12707,#1013,.T.);
#16764=EDGE_CURVE('',#12709,#12708,#3855,.T.);
#16765=EDGE_CURVE('',#12710,#12709,#1014,.T.);
#16766=EDGE_CURVE('',#12711,#12710,#2084,.T.);
#16767=EDGE_CURVE('',#12712,#12711,#1015,.T.);
#16768=EDGE_CURVE('',#12713,#12712,#3856,.T.);
#16769=EDGE_CURVE('',#12714,#12713,#1016,.T.);
#16770=EDGE_CURVE('',#12715,#12714,#2085,.T.);
#16771=EDGE_CURVE('',#12716,#12715,#1017,.T.);
#16772=EDGE_CURVE('',#12717,#12716,#3857,.T.);
#16773=EDGE_CURVE('',#12718,#12717,#1018,.T.);
#16774=EDGE_CURVE('',#12719,#12718,#2086,.T.);
#16775=EDGE_CURVE('',#12720,#12719,#1019,.T.);
#16776=EDGE_CURVE('',#12721,#12720,#3858,.T.);
#16777=EDGE_CURVE('',#12722,#12721,#1020,.T.);
#16778=EDGE_CURVE('',#12723,#12722,#2087,.T.);
#16779=EDGE_CURVE('',#12724,#12723,#1021,.T.);
#16780=EDGE_CURVE('',#12725,#12724,#3859,.T.);
#16781=EDGE_CURVE('',#12726,#12725,#1022,.T.);
#16782=EDGE_CURVE('',#12727,#12726,#2088,.T.);
#16783=EDGE_CURVE('',#12728,#12727,#1023,.T.);
#16784=EDGE_CURVE('',#12729,#12728,#3860,.T.);
#16785=EDGE_CURVE('',#12730,#12729,#1024,.T.);
#16786=EDGE_CURVE('',#12731,#12730,#2089,.T.);
#16787=EDGE_CURVE('',#12732,#12731,#1025,.T.);
#16788=EDGE_CURVE('',#12733,#12732,#3861,.T.);
#16789=EDGE_CURVE('',#12734,#12733,#1026,.T.);
#16790=EDGE_CURVE('',#12735,#12734,#2090,.T.);
#16791=EDGE_CURVE('',#12736,#12735,#1027,.T.);
#16792=EDGE_CURVE('',#12737,#12736,#3862,.T.);
#16793=EDGE_CURVE('',#12738,#12737,#1028,.T.);
#16794=EDGE_CURVE('',#12739,#12738,#2091,.T.);
#16795=EDGE_CURVE('',#12740,#12739,#1029,.T.);
#16796=EDGE_CURVE('',#12741,#12740,#3863,.T.);
#16797=EDGE_CURVE('',#12742,#12741,#1030,.T.);
#16798=EDGE_CURVE('',#12743,#12742,#2092,.T.);
#16799=EDGE_CURVE('',#12744,#12743,#1031,.T.);
#16800=EDGE_CURVE('',#12745,#12744,#3864,.T.);
#16801=EDGE_CURVE('',#12746,#12745,#1032,.T.);
#16802=EDGE_CURVE('',#12747,#12746,#2093,.T.);
#16803=EDGE_CURVE('',#12748,#12747,#1033,.T.);
#16804=EDGE_CURVE('',#12749,#12748,#3865,.T.);
#16805=EDGE_CURVE('',#12750,#12749,#1034,.T.);
#16806=EDGE_CURVE('',#12461,#12750,#3222,.T.);
#16807=EDGE_CURVE('',#12461,#12458,#9144,.T.);
#16808=EDGE_CURVE('',#12751,#12752,#3223,.T.);
#16809=EDGE_CURVE('',#12753,#12751,#1035,.T.);
#16810=EDGE_CURVE('',#12753,#12754,#3866,.T.);
#16811=EDGE_CURVE('',#12755,#12754,#1036,.T.);
#16812=EDGE_CURVE('',#12756,#12755,#2094,.T.);
#16813=EDGE_CURVE('',#12757,#12756,#1037,.T.);
#16814=EDGE_CURVE('',#12757,#12758,#3867,.T.);
#16815=EDGE_CURVE('',#12759,#12758,#1038,.T.);
#16816=EDGE_CURVE('',#12760,#12759,#2095,.T.);
#16817=EDGE_CURVE('',#12761,#12760,#1039,.T.);
#16818=EDGE_CURVE('',#12761,#12762,#3868,.T.);
#16819=EDGE_CURVE('',#12763,#12762,#1040,.T.);
#16820=EDGE_CURVE('',#12764,#12763,#2096,.T.);
#16821=EDGE_CURVE('',#12765,#12764,#1041,.T.);
#16822=EDGE_CURVE('',#12765,#12766,#3869,.T.);
#16823=EDGE_CURVE('',#12767,#12766,#1042,.T.);
#16824=EDGE_CURVE('',#12768,#12767,#2097,.T.);
#16825=EDGE_CURVE('',#12769,#12768,#1043,.T.);
#16826=EDGE_CURVE('',#12769,#12770,#3870,.T.);
#16827=EDGE_CURVE('',#12771,#12770,#1044,.T.);
#16828=EDGE_CURVE('',#12772,#12771,#2098,.T.);
#16829=EDGE_CURVE('',#12773,#12772,#1045,.T.);
#16830=EDGE_CURVE('',#12773,#12774,#3871,.T.);
#16831=EDGE_CURVE('',#12775,#12774,#1046,.T.);
#16832=EDGE_CURVE('',#12776,#12775,#2099,.T.);
#16833=EDGE_CURVE('',#12777,#12776,#1047,.T.);
#16834=EDGE_CURVE('',#12777,#12778,#3872,.T.);
#16835=EDGE_CURVE('',#12779,#12778,#1048,.T.);
#16836=EDGE_CURVE('',#12780,#12779,#2100,.T.);
#16837=EDGE_CURVE('',#12781,#12780,#1049,.T.);
#16838=EDGE_CURVE('',#12781,#12782,#3873,.T.);
#16839=EDGE_CURVE('',#12783,#12782,#1050,.T.);
#16840=EDGE_CURVE('',#12784,#12783,#2101,.T.);
#16841=EDGE_CURVE('',#12785,#12784,#1051,.T.);
#16842=EDGE_CURVE('',#12785,#12786,#3874,.T.);
#16843=EDGE_CURVE('',#12787,#12786,#1052,.T.);
#16844=EDGE_CURVE('',#12788,#12787,#2102,.T.);
#16845=EDGE_CURVE('',#12789,#12788,#1053,.T.);
#16846=EDGE_CURVE('',#12789,#12790,#3875,.T.);
#16847=EDGE_CURVE('',#12791,#12790,#1054,.T.);
#16848=EDGE_CURVE('',#12792,#12791,#2103,.T.);
#16849=EDGE_CURVE('',#12793,#12792,#1055,.T.);
#16850=EDGE_CURVE('',#12793,#12794,#3876,.T.);
#16851=EDGE_CURVE('',#12795,#12794,#1056,.T.);
#16852=EDGE_CURVE('',#12796,#12795,#2104,.T.);
#16853=EDGE_CURVE('',#12797,#12796,#1057,.T.);
#16854=EDGE_CURVE('',#12797,#12798,#3877,.T.);
#16855=EDGE_CURVE('',#12799,#12798,#1058,.T.);
#16856=EDGE_CURVE('',#12800,#12799,#2105,.T.);
#16857=EDGE_CURVE('',#12801,#12800,#1059,.T.);
#16858=EDGE_CURVE('',#12801,#12802,#3878,.T.);
#16859=EDGE_CURVE('',#12803,#12802,#1060,.T.);
#16860=EDGE_CURVE('',#12804,#12803,#2106,.T.);
#16861=EDGE_CURVE('',#12805,#12804,#1061,.T.);
#16862=EDGE_CURVE('',#12805,#12806,#3879,.T.);
#16863=EDGE_CURVE('',#12807,#12806,#1062,.T.);
#16864=EDGE_CURVE('',#12808,#12807,#2107,.T.);
#16865=EDGE_CURVE('',#12809,#12808,#1063,.T.);
#16866=EDGE_CURVE('',#12809,#12810,#3880,.T.);
#16867=EDGE_CURVE('',#12811,#12810,#1064,.T.);
#16868=EDGE_CURVE('',#12812,#12811,#2108,.T.);
#16869=EDGE_CURVE('',#12813,#12812,#1065,.T.);
#16870=EDGE_CURVE('',#12813,#12814,#3881,.T.);
#16871=EDGE_CURVE('',#12815,#12814,#1066,.T.);
#16872=EDGE_CURVE('',#12816,#12815,#2109,.T.);
#16873=EDGE_CURVE('',#12817,#12816,#1067,.T.);
#16874=EDGE_CURVE('',#12817,#12818,#3882,.T.);
#16875=EDGE_CURVE('',#12819,#12818,#1068,.T.);
#16876=EDGE_CURVE('',#12820,#12819,#2110,.T.);
#16877=EDGE_CURVE('',#12821,#12820,#1069,.T.);
#16878=EDGE_CURVE('',#12821,#12822,#3883,.T.);
#16879=EDGE_CURVE('',#12823,#12822,#1070,.T.);
#16880=EDGE_CURVE('',#12824,#12823,#2111,.T.);
#16881=EDGE_CURVE('',#12825,#12824,#1071,.T.);
#16882=EDGE_CURVE('',#12825,#12826,#3884,.T.);
#16883=EDGE_CURVE('',#12827,#12826,#1072,.T.);
#16884=EDGE_CURVE('',#12828,#12827,#2112,.T.);
#16885=EDGE_CURVE('',#12829,#12828,#1073,.T.);
#16886=EDGE_CURVE('',#12829,#12830,#3885,.T.);
#16887=EDGE_CURVE('',#12831,#12830,#1074,.T.);
#16888=EDGE_CURVE('',#12832,#12831,#2113,.T.);
#16889=EDGE_CURVE('',#12833,#12832,#1075,.T.);
#16890=EDGE_CURVE('',#12833,#12834,#3886,.T.);
#16891=EDGE_CURVE('',#12835,#12834,#1076,.T.);
#16892=EDGE_CURVE('',#12836,#12835,#2114,.T.);
#16893=EDGE_CURVE('',#12837,#12836,#1077,.T.);
#16894=EDGE_CURVE('',#12837,#12838,#3887,.T.);
#16895=EDGE_CURVE('',#12839,#12838,#1078,.T.);
#16896=EDGE_CURVE('',#12840,#12839,#2115,.T.);
#16897=EDGE_CURVE('',#12841,#12840,#1079,.T.);
#16898=EDGE_CURVE('',#12841,#12842,#3888,.T.);
#16899=EDGE_CURVE('',#12843,#12842,#1080,.T.);
#16900=EDGE_CURVE('',#12844,#12843,#2116,.T.);
#16901=EDGE_CURVE('',#12845,#12844,#1081,.T.);
#16902=EDGE_CURVE('',#12845,#12846,#3889,.T.);
#16903=EDGE_CURVE('',#12847,#12846,#1082,.T.);
#16904=EDGE_CURVE('',#12848,#12847,#2117,.T.);
#16905=EDGE_CURVE('',#12849,#12848,#1083,.T.);
#16906=EDGE_CURVE('',#12849,#12850,#3890,.T.);
#16907=EDGE_CURVE('',#12851,#12850,#1084,.T.);
#16908=EDGE_CURVE('',#12852,#12851,#2118,.T.);
#16909=EDGE_CURVE('',#12853,#12852,#1085,.T.);
#16910=EDGE_CURVE('',#12853,#12854,#3891,.T.);
#16911=EDGE_CURVE('',#12855,#12854,#1086,.T.);
#16912=EDGE_CURVE('',#12856,#12855,#2119,.T.);
#16913=EDGE_CURVE('',#12857,#12856,#1087,.T.);
#16914=EDGE_CURVE('',#12857,#12858,#3892,.T.);
#16915=EDGE_CURVE('',#12859,#12858,#1088,.T.);
#16916=EDGE_CURVE('',#12860,#12859,#2120,.T.);
#16917=EDGE_CURVE('',#12861,#12860,#1089,.T.);
#16918=EDGE_CURVE('',#12861,#12862,#3893,.T.);
#16919=EDGE_CURVE('',#12863,#12862,#1090,.T.);
#16920=EDGE_CURVE('',#12864,#12863,#2121,.T.);
#16921=EDGE_CURVE('',#12865,#12864,#1091,.T.);
#16922=EDGE_CURVE('',#12865,#12866,#3894,.T.);
#16923=EDGE_CURVE('',#12867,#12866,#1092,.T.);
#16924=EDGE_CURVE('',#12868,#12867,#2122,.T.);
#16925=EDGE_CURVE('',#12869,#12868,#1093,.T.);
#16926=EDGE_CURVE('',#12869,#12870,#3895,.T.);
#16927=EDGE_CURVE('',#12871,#12870,#1094,.T.);
#16928=EDGE_CURVE('',#12872,#12871,#2123,.T.);
#16929=EDGE_CURVE('',#12873,#12872,#1095,.T.);
#16930=EDGE_CURVE('',#12873,#12874,#3896,.T.);
#16931=EDGE_CURVE('',#12875,#12874,#1096,.T.);
#16932=EDGE_CURVE('',#12876,#12875,#2124,.T.);
#16933=EDGE_CURVE('',#12877,#12876,#1097,.T.);
#16934=EDGE_CURVE('',#12877,#12878,#3897,.T.);
#16935=EDGE_CURVE('',#12879,#12878,#1098,.T.);
#16936=EDGE_CURVE('',#12880,#12879,#2125,.T.);
#16937=EDGE_CURVE('',#12881,#12880,#1099,.T.);
#16938=EDGE_CURVE('',#12881,#12882,#3898,.T.);
#16939=EDGE_CURVE('',#12883,#12882,#1100,.T.);
#16940=EDGE_CURVE('',#12884,#12883,#2126,.T.);
#16941=EDGE_CURVE('',#12885,#12884,#1101,.T.);
#16942=EDGE_CURVE('',#12885,#12886,#3899,.T.);
#16943=EDGE_CURVE('',#12887,#12886,#1102,.T.);
#16944=EDGE_CURVE('',#12888,#12887,#2127,.T.);
#16945=EDGE_CURVE('',#12889,#12888,#1103,.T.);
#16946=EDGE_CURVE('',#12889,#12890,#3900,.T.);
#16947=EDGE_CURVE('',#12891,#12890,#1104,.T.);
#16948=EDGE_CURVE('',#12892,#12891,#2128,.T.);
#16949=EDGE_CURVE('',#12893,#12892,#1105,.T.);
#16950=EDGE_CURVE('',#12893,#12894,#3901,.T.);
#16951=EDGE_CURVE('',#12895,#12894,#1106,.T.);
#16952=EDGE_CURVE('',#12896,#12895,#2129,.T.);
#16953=EDGE_CURVE('',#12897,#12896,#1107,.T.);
#16954=EDGE_CURVE('',#12897,#12898,#3902,.T.);
#16955=EDGE_CURVE('',#12899,#12898,#1108,.T.);
#16956=EDGE_CURVE('',#12900,#12899,#2130,.T.);
#16957=EDGE_CURVE('',#12901,#12900,#1109,.T.);
#16958=EDGE_CURVE('',#12901,#12902,#3903,.T.);
#16959=EDGE_CURVE('',#12903,#12902,#1110,.T.);
#16960=EDGE_CURVE('',#12904,#12903,#2131,.T.);
#16961=EDGE_CURVE('',#12905,#12904,#1111,.T.);
#16962=EDGE_CURVE('',#12905,#12906,#3904,.T.);
#16963=EDGE_CURVE('',#12907,#12906,#1112,.T.);
#16964=EDGE_CURVE('',#12908,#12907,#2132,.T.);
#16965=EDGE_CURVE('',#12909,#12908,#1113,.T.);
#16966=EDGE_CURVE('',#12909,#12910,#3905,.T.);
#16967=EDGE_CURVE('',#12911,#12910,#1114,.T.);
#16968=EDGE_CURVE('',#12912,#12911,#2133,.T.);
#16969=EDGE_CURVE('',#12913,#12912,#1115,.T.);
#16970=EDGE_CURVE('',#12913,#12914,#3906,.T.);
#16971=EDGE_CURVE('',#12915,#12914,#1116,.T.);
#16972=EDGE_CURVE('',#12916,#12915,#2134,.T.);
#16973=EDGE_CURVE('',#12917,#12916,#1117,.T.);
#16974=EDGE_CURVE('',#12917,#12918,#3907,.T.);
#16975=EDGE_CURVE('',#12919,#12918,#1118,.T.);
#16976=EDGE_CURVE('',#12920,#12919,#2135,.T.);
#16977=EDGE_CURVE('',#12921,#12920,#1119,.T.);
#16978=EDGE_CURVE('',#12921,#12922,#3908,.T.);
#16979=EDGE_CURVE('',#12923,#12922,#1120,.T.);
#16980=EDGE_CURVE('',#12924,#12923,#2136,.T.);
#16981=EDGE_CURVE('',#12925,#12924,#1121,.T.);
#16982=EDGE_CURVE('',#12925,#12926,#3909,.T.);
#16983=EDGE_CURVE('',#12927,#12926,#1122,.T.);
#16984=EDGE_CURVE('',#12928,#12927,#2137,.T.);
#16985=EDGE_CURVE('',#12929,#12928,#1123,.T.);
#16986=EDGE_CURVE('',#12929,#12930,#3910,.T.);
#16987=EDGE_CURVE('',#12931,#12930,#1124,.T.);
#16988=EDGE_CURVE('',#12932,#12931,#2138,.T.);
#16989=EDGE_CURVE('',#12933,#12932,#1125,.T.);
#16990=EDGE_CURVE('',#12933,#12934,#3911,.T.);
#16991=EDGE_CURVE('',#12935,#12934,#1126,.T.);
#16992=EDGE_CURVE('',#12936,#12935,#2139,.T.);
#16993=EDGE_CURVE('',#12937,#12936,#1127,.T.);
#16994=EDGE_CURVE('',#12937,#12938,#3912,.T.);
#16995=EDGE_CURVE('',#12939,#12938,#1128,.T.);
#16996=EDGE_CURVE('',#12940,#12939,#2140,.T.);
#16997=EDGE_CURVE('',#12941,#12940,#1129,.T.);
#16998=EDGE_CURVE('',#12941,#12942,#3913,.T.);
#16999=EDGE_CURVE('',#12943,#12942,#1130,.T.);
#17000=EDGE_CURVE('',#12944,#12943,#2141,.T.);
#17001=EDGE_CURVE('',#12945,#12944,#1131,.T.);
#17002=EDGE_CURVE('',#12945,#12946,#3914,.T.);
#17003=EDGE_CURVE('',#12947,#12946,#1132,.T.);
#17004=EDGE_CURVE('',#12948,#12947,#2142,.T.);
#17005=EDGE_CURVE('',#12949,#12948,#1133,.T.);
#17006=EDGE_CURVE('',#12949,#12950,#3915,.T.);
#17007=EDGE_CURVE('',#12951,#12950,#1134,.T.);
#17008=EDGE_CURVE('',#12952,#12951,#2143,.T.);
#17009=EDGE_CURVE('',#12953,#12952,#1135,.T.);
#17010=EDGE_CURVE('',#12953,#12954,#3916,.T.);
#17011=EDGE_CURVE('',#12955,#12954,#1136,.T.);
#17012=EDGE_CURVE('',#12956,#12955,#2144,.T.);
#17013=EDGE_CURVE('',#12957,#12956,#1137,.T.);
#17014=EDGE_CURVE('',#12957,#12958,#3917,.T.);
#17015=EDGE_CURVE('',#12959,#12958,#1138,.T.);
#17016=EDGE_CURVE('',#12960,#12959,#2145,.T.);
#17017=EDGE_CURVE('',#12961,#12960,#1139,.T.);
#17018=EDGE_CURVE('',#12961,#12962,#3918,.T.);
#17019=EDGE_CURVE('',#12963,#12962,#1140,.T.);
#17020=EDGE_CURVE('',#12964,#12963,#2146,.T.);
#17021=EDGE_CURVE('',#12965,#12964,#1141,.T.);
#17022=EDGE_CURVE('',#12965,#12966,#3919,.T.);
#17023=EDGE_CURVE('',#12967,#12966,#1142,.T.);
#17024=EDGE_CURVE('',#12968,#12967,#2147,.T.);
#17025=EDGE_CURVE('',#12969,#12968,#1143,.T.);
#17026=EDGE_CURVE('',#12969,#12970,#3920,.T.);
#17027=EDGE_CURVE('',#12971,#12970,#1144,.T.);
#17028=EDGE_CURVE('',#12972,#12971,#2148,.T.);
#17029=EDGE_CURVE('',#12973,#12972,#1145,.T.);
#17030=EDGE_CURVE('',#12973,#12974,#3921,.T.);
#17031=EDGE_CURVE('',#12975,#12974,#1146,.T.);
#17032=EDGE_CURVE('',#12976,#12975,#2149,.T.);
#17033=EDGE_CURVE('',#12977,#12976,#1147,.T.);
#17034=EDGE_CURVE('',#12977,#12978,#3922,.T.);
#17035=EDGE_CURVE('',#12979,#12978,#1148,.T.);
#17036=EDGE_CURVE('',#12980,#12979,#2150,.T.);
#17037=EDGE_CURVE('',#12981,#12980,#1149,.T.);
#17038=EDGE_CURVE('',#12981,#12982,#3923,.T.);
#17039=EDGE_CURVE('',#12983,#12982,#1150,.T.);
#17040=EDGE_CURVE('',#12984,#12983,#2151,.T.);
#17041=EDGE_CURVE('',#12985,#12984,#1151,.T.);
#17042=EDGE_CURVE('',#12985,#12986,#3924,.T.);
#17043=EDGE_CURVE('',#12987,#12986,#1152,.T.);
#17044=EDGE_CURVE('',#12988,#12987,#2152,.T.);
#17045=EDGE_CURVE('',#12989,#12988,#1153,.T.);
#17046=EDGE_CURVE('',#12989,#12990,#3925,.T.);
#17047=EDGE_CURVE('',#12411,#12990,#1154,.T.);
#17048=EDGE_CURVE('',#12991,#12410,#1155,.T.);
#17049=EDGE_CURVE('',#12991,#12992,#3926,.T.);
#17050=EDGE_CURVE('',#12407,#12992,#1156,.T.);
#17051=EDGE_CURVE('',#12993,#12406,#1157,.T.);
#17052=EDGE_CURVE('',#12993,#12994,#3927,.T.);
#17053=EDGE_CURVE('',#12403,#12994,#1158,.T.);
#17054=EDGE_CURVE('',#12995,#12402,#1159,.T.);
#17055=EDGE_CURVE('',#12995,#12996,#3928,.T.);
#17056=EDGE_CURVE('',#12399,#12996,#1160,.T.);
#17057=EDGE_CURVE('',#12997,#12398,#1161,.T.);
#17058=EDGE_CURVE('',#12997,#12998,#3929,.T.);
#17059=EDGE_CURVE('',#12395,#12998,#1162,.T.);
#17060=EDGE_CURVE('',#12999,#12394,#1163,.T.);
#17061=EDGE_CURVE('',#12999,#13000,#3930,.T.);
#17062=EDGE_CURVE('',#12391,#13000,#1164,.T.);
#17063=EDGE_CURVE('',#13001,#12390,#1165,.T.);
#17064=EDGE_CURVE('',#13001,#13002,#3931,.T.);
#17065=EDGE_CURVE('',#12415,#13002,#1166,.T.);
#17066=EDGE_CURVE('',#13003,#12414,#1167,.T.);
#17067=EDGE_CURVE('',#13003,#13004,#3932,.T.);
#17068=EDGE_CURVE('',#12419,#13004,#1168,.T.);
#17069=EDGE_CURVE('',#13005,#12418,#1169,.T.);
#17070=EDGE_CURVE('',#13005,#13006,#3933,.T.);
#17071=EDGE_CURVE('',#12423,#13006,#1170,.T.);
#17072=EDGE_CURVE('',#13007,#12422,#1171,.T.);
#17073=EDGE_CURVE('',#13007,#13008,#3934,.T.);
#17074=EDGE_CURVE('',#12427,#13008,#1172,.T.);
#17075=EDGE_CURVE('',#13009,#12426,#1173,.T.);
#17076=EDGE_CURVE('',#13009,#13010,#3935,.T.);
#17077=EDGE_CURVE('',#12431,#13010,#1174,.T.);
#17078=EDGE_CURVE('',#13011,#12430,#1175,.T.);
#17079=EDGE_CURVE('',#13011,#13012,#3936,.T.);
#17080=EDGE_CURVE('',#12435,#13012,#1176,.T.);
#17081=EDGE_CURVE('',#13013,#12434,#1177,.T.);
#17082=EDGE_CURVE('',#13013,#13014,#3937,.T.);
#17083=EDGE_CURVE('',#12439,#13014,#1178,.T.);
#17084=EDGE_CURVE('',#13015,#12438,#1179,.T.);
#17085=EDGE_CURVE('',#13015,#13016,#3938,.T.);
#17086=EDGE_CURVE('',#12443,#13016,#1180,.T.);
#17087=EDGE_CURVE('',#13017,#12442,#1181,.T.);
#17088=EDGE_CURVE('',#13017,#13018,#3939,.T.);
#17089=EDGE_CURVE('',#12447,#13018,#1182,.T.);
#17090=EDGE_CURVE('',#13019,#12446,#1183,.T.);
#17091=EDGE_CURVE('',#13019,#13020,#3940,.T.);
#17092=EDGE_CURVE('',#13021,#13020,#1184,.T.);
#17093=EDGE_CURVE('',#13022,#13021,#2153,.T.);
#17094=EDGE_CURVE('',#13023,#13022,#1185,.T.);
#17095=EDGE_CURVE('',#13023,#13024,#3941,.T.);
#17096=EDGE_CURVE('',#13025,#13024,#1186,.T.);
#17097=EDGE_CURVE('',#13026,#13025,#2154,.T.);
#17098=EDGE_CURVE('',#13027,#13026,#1187,.T.);
#17099=EDGE_CURVE('',#13027,#13028,#3942,.T.);
#17100=EDGE_CURVE('',#13029,#13028,#1188,.T.);
#17101=EDGE_CURVE('',#13030,#13029,#2155,.T.);
#17102=EDGE_CURVE('',#13031,#13030,#1189,.T.);
#17103=EDGE_CURVE('',#13031,#13032,#3943,.T.);
#17104=EDGE_CURVE('',#13033,#13032,#1190,.T.);
#17105=EDGE_CURVE('',#13034,#13033,#2156,.T.);
#17106=EDGE_CURVE('',#13035,#13034,#1191,.T.);
#17107=EDGE_CURVE('',#13035,#13036,#3944,.T.);
#17108=EDGE_CURVE('',#13037,#13036,#1192,.T.);
#17109=EDGE_CURVE('',#13038,#13037,#2157,.T.);
#17110=EDGE_CURVE('',#13039,#13038,#1193,.T.);
#17111=EDGE_CURVE('',#13039,#13040,#3945,.T.);
#17112=EDGE_CURVE('',#13041,#13040,#1194,.T.);
#17113=EDGE_CURVE('',#12752,#13041,#3224,.T.);
#17114=EDGE_CURVE('',#12752,#13042,#9145,.T.);
#17115=EDGE_CURVE('',#13043,#13042,#3946,.T.);
#17116=EDGE_CURVE('',#13042,#13043,#3947,.T.);
#17117=EDGE_CURVE('',#13044,#13044,#3948,.T.);
#17118=EDGE_CURVE('',#13044,#13043,#3949,.T.);
#17119=EDGE_CURVE('',#13045,#13045,#3950,.T.);
#17120=EDGE_CURVE('',#13045,#13044,#9146,.T.);
#17121=EDGE_CURVE('',#13046,#13046,#3951,.T.);
#17122=EDGE_CURVE('',#13046,#13045,#3952,.T.);
#17123=EDGE_CURVE('',#12268,#13047,#3953,.T.);
#17124=EDGE_CURVE('',#13047,#13047,#3954,.T.);
#17125=EDGE_CURVE('',#13048,#13001,#2158,.T.);
#17126=EDGE_CURVE('',#13048,#13049,#3955,.T.);
#17127=EDGE_CURVE('',#13002,#13049,#2159,.T.);
#17128=EDGE_CURVE('',#13000,#13050,#2160,.T.);
#17129=EDGE_CURVE('',#13051,#12999,#2161,.T.);
#17130=EDGE_CURVE('',#13051,#13050,#3956,.T.);
#17131=EDGE_CURVE('',#12998,#13052,#2162,.T.);
#17132=EDGE_CURVE('',#13053,#12997,#2163,.T.);
#17133=EDGE_CURVE('',#13053,#13052,#3957,.T.);
#17134=EDGE_CURVE('',#12996,#13054,#2164,.T.);
#17135=EDGE_CURVE('',#13055,#12995,#2165,.T.);
#17136=EDGE_CURVE('',#13055,#13054,#3958,.T.);
#17137=EDGE_CURVE('',#12994,#13056,#2166,.T.);
#17138=EDGE_CURVE('',#13057,#12993,#2167,.T.);
#17139=EDGE_CURVE('',#13057,#13056,#3959,.T.);
#17140=EDGE_CURVE('',#12992,#13058,#2168,.T.);
#17141=EDGE_CURVE('',#13059,#12991,#2169,.T.);
#17142=EDGE_CURVE('',#13059,#13058,#3960,.T.);
#17143=EDGE_CURVE('',#12990,#13060,#2170,.T.);
#17144=EDGE_CURVE('',#13061,#12989,#2171,.T.);
#17145=EDGE_CURVE('',#13061,#13060,#3961,.T.);
#17146=EDGE_CURVE('',#12986,#13062,#2172,.T.);
#17147=EDGE_CURVE('',#13063,#12985,#2173,.T.);
#17148=EDGE_CURVE('',#13063,#13062,#3962,.T.);
#17149=EDGE_CURVE('',#12982,#13064,#2174,.T.);
#17150=EDGE_CURVE('',#13065,#12981,#2175,.T.);
#17151=EDGE_CURVE('',#13065,#13064,#3963,.T.);
#17152=EDGE_CURVE('',#12978,#13066,#2176,.T.);
#17153=EDGE_CURVE('',#13067,#12977,#2177,.T.);
#17154=EDGE_CURVE('',#13067,#13066,#3964,.T.);
#17155=EDGE_CURVE('',#12974,#13068,#2178,.T.);
#17156=EDGE_CURVE('',#13069,#12973,#2179,.T.);
#17157=EDGE_CURVE('',#13069,#13068,#3965,.T.);
#17158=EDGE_CURVE('',#12970,#13070,#2180,.T.);
#17159=EDGE_CURVE('',#13071,#12969,#2181,.T.);
#17160=EDGE_CURVE('',#13071,#13070,#3966,.T.);
#17161=EDGE_CURVE('',#12966,#13072,#2182,.T.);
#17162=EDGE_CURVE('',#13073,#12965,#2183,.T.);
#17163=EDGE_CURVE('',#13073,#13072,#3967,.T.);
#17164=EDGE_CURVE('',#12962,#13074,#2184,.T.);
#17165=EDGE_CURVE('',#13075,#12961,#2185,.T.);
#17166=EDGE_CURVE('',#13075,#13074,#3968,.T.);
#17167=EDGE_CURVE('',#12958,#13076,#2186,.T.);
#17168=EDGE_CURVE('',#13077,#12957,#2187,.T.);
#17169=EDGE_CURVE('',#13077,#13076,#3969,.T.);
#17170=EDGE_CURVE('',#12954,#13078,#2188,.T.);
#17171=EDGE_CURVE('',#13079,#12953,#2189,.T.);
#17172=EDGE_CURVE('',#13079,#13078,#3970,.T.);
#17173=EDGE_CURVE('',#12950,#13080,#2190,.T.);
#17174=EDGE_CURVE('',#13081,#12949,#2191,.T.);
#17175=EDGE_CURVE('',#13081,#13080,#3971,.T.);
#17176=EDGE_CURVE('',#12946,#13082,#2192,.T.);
#17177=EDGE_CURVE('',#13083,#12945,#2193,.T.);
#17178=EDGE_CURVE('',#13083,#13082,#3972,.T.);
#17179=EDGE_CURVE('',#12942,#13084,#2194,.T.);
#17180=EDGE_CURVE('',#13085,#12941,#2195,.T.);
#17181=EDGE_CURVE('',#13085,#13084,#3973,.T.);
#17182=EDGE_CURVE('',#12938,#13086,#2196,.T.);
#17183=EDGE_CURVE('',#13087,#12937,#2197,.T.);
#17184=EDGE_CURVE('',#13087,#13086,#3974,.T.);
#17185=EDGE_CURVE('',#12934,#13088,#2198,.T.);
#17186=EDGE_CURVE('',#13089,#12933,#2199,.T.);
#17187=EDGE_CURVE('',#13089,#13088,#3975,.T.);
#17188=EDGE_CURVE('',#12930,#13090,#2200,.T.);
#17189=EDGE_CURVE('',#13091,#12929,#2201,.T.);
#17190=EDGE_CURVE('',#13091,#13090,#3976,.T.);
#17191=EDGE_CURVE('',#12926,#13092,#2202,.T.);
#17192=EDGE_CURVE('',#13093,#12925,#2203,.T.);
#17193=EDGE_CURVE('',#13093,#13092,#3977,.T.);
#17194=EDGE_CURVE('',#12922,#13094,#2204,.T.);
#17195=EDGE_CURVE('',#13095,#12921,#2205,.T.);
#17196=EDGE_CURVE('',#13095,#13094,#3978,.T.);
#17197=EDGE_CURVE('',#12918,#13096,#2206,.T.);
#17198=EDGE_CURVE('',#13097,#12917,#2207,.T.);
#17199=EDGE_CURVE('',#13097,#13096,#3979,.T.);
#17200=EDGE_CURVE('',#12914,#13098,#2208,.T.);
#17201=EDGE_CURVE('',#13099,#12913,#2209,.T.);
#17202=EDGE_CURVE('',#13099,#13098,#3980,.T.);
#17203=EDGE_CURVE('',#12910,#13100,#2210,.T.);
#17204=EDGE_CURVE('',#13101,#12909,#2211,.T.);
#17205=EDGE_CURVE('',#13101,#13100,#3981,.T.);
#17206=EDGE_CURVE('',#12906,#13102,#2212,.T.);
#17207=EDGE_CURVE('',#13103,#12905,#2213,.T.);
#17208=EDGE_CURVE('',#13103,#13102,#3982,.T.);
#17209=EDGE_CURVE('',#12902,#13104,#2214,.T.);
#17210=EDGE_CURVE('',#13105,#12901,#2215,.T.);
#17211=EDGE_CURVE('',#13105,#13104,#3983,.T.);
#17212=EDGE_CURVE('',#12898,#13106,#2216,.T.);
#17213=EDGE_CURVE('',#13107,#12897,#2217,.T.);
#17214=EDGE_CURVE('',#13107,#13106,#3984,.T.);
#17215=EDGE_CURVE('',#12894,#13108,#2218,.T.);
#17216=EDGE_CURVE('',#13109,#12893,#2219,.T.);
#17217=EDGE_CURVE('',#13109,#13108,#3985,.T.);
#17218=EDGE_CURVE('',#12890,#13110,#2220,.T.);
#17219=EDGE_CURVE('',#13111,#12889,#2221,.T.);
#17220=EDGE_CURVE('',#13111,#13110,#3986,.T.);
#17221=EDGE_CURVE('',#12886,#13112,#2222,.T.);
#17222=EDGE_CURVE('',#13113,#12885,#2223,.T.);
#17223=EDGE_CURVE('',#13113,#13112,#3987,.T.);
#17224=EDGE_CURVE('',#12882,#13114,#2224,.T.);
#17225=EDGE_CURVE('',#13115,#12881,#2225,.T.);
#17226=EDGE_CURVE('',#13115,#13114,#3988,.T.);
#17227=EDGE_CURVE('',#12878,#13116,#2226,.T.);
#17228=EDGE_CURVE('',#13117,#12877,#2227,.T.);
#17229=EDGE_CURVE('',#13117,#13116,#3989,.T.);
#17230=EDGE_CURVE('',#12874,#13118,#2228,.T.);
#17231=EDGE_CURVE('',#13119,#12873,#2229,.T.);
#17232=EDGE_CURVE('',#13119,#13118,#3990,.T.);
#17233=EDGE_CURVE('',#12870,#13120,#2230,.T.);
#17234=EDGE_CURVE('',#13121,#12869,#2231,.T.);
#17235=EDGE_CURVE('',#13121,#13120,#3991,.T.);
#17236=EDGE_CURVE('',#12866,#13122,#2232,.T.);
#17237=EDGE_CURVE('',#13123,#12865,#2233,.T.);
#17238=EDGE_CURVE('',#13123,#13122,#3992,.T.);
#17239=EDGE_CURVE('',#12862,#13124,#2234,.T.);
#17240=EDGE_CURVE('',#13125,#12861,#2235,.T.);
#17241=EDGE_CURVE('',#13125,#13124,#3993,.T.);
#17242=EDGE_CURVE('',#12858,#13126,#2236,.T.);
#17243=EDGE_CURVE('',#13127,#12857,#2237,.T.);
#17244=EDGE_CURVE('',#13127,#13126,#3994,.T.);
#17245=EDGE_CURVE('',#12854,#13128,#2238,.T.);
#17246=EDGE_CURVE('',#13129,#12853,#2239,.T.);
#17247=EDGE_CURVE('',#13129,#13128,#3995,.T.);
#17248=EDGE_CURVE('',#12850,#13130,#2240,.T.);
#17249=EDGE_CURVE('',#13131,#12849,#2241,.T.);
#17250=EDGE_CURVE('',#13131,#13130,#3996,.T.);
#17251=EDGE_CURVE('',#12846,#13132,#2242,.T.);
#17252=EDGE_CURVE('',#13133,#12845,#2243,.T.);
#17253=EDGE_CURVE('',#13133,#13132,#3997,.T.);
#17254=EDGE_CURVE('',#12842,#13134,#2244,.T.);
#17255=EDGE_CURVE('',#13135,#12841,#2245,.T.);
#17256=EDGE_CURVE('',#13135,#13134,#3998,.T.);
#17257=EDGE_CURVE('',#12838,#13136,#2246,.T.);
#17258=EDGE_CURVE('',#13137,#12837,#2247,.T.);
#17259=EDGE_CURVE('',#13137,#13136,#3999,.T.);
#17260=EDGE_CURVE('',#12834,#13138,#2248,.T.);
#17261=EDGE_CURVE('',#13139,#12833,#2249,.T.);
#17262=EDGE_CURVE('',#13139,#13138,#4000,.T.);
#17263=EDGE_CURVE('',#12830,#13140,#2250,.T.);
#17264=EDGE_CURVE('',#13141,#12829,#2251,.T.);
#17265=EDGE_CURVE('',#13141,#13140,#4001,.T.);
#17266=EDGE_CURVE('',#12826,#13142,#2252,.T.);
#17267=EDGE_CURVE('',#13143,#12825,#2253,.T.);
#17268=EDGE_CURVE('',#13143,#13142,#4002,.T.);
#17269=EDGE_CURVE('',#12822,#13144,#2254,.T.);
#17270=EDGE_CURVE('',#13145,#12821,#2255,.T.);
#17271=EDGE_CURVE('',#13145,#13144,#4003,.T.);
#17272=EDGE_CURVE('',#12818,#13146,#2256,.T.);
#17273=EDGE_CURVE('',#13147,#12817,#2257,.T.);
#17274=EDGE_CURVE('',#13147,#13146,#4004,.T.);
#17275=EDGE_CURVE('',#12814,#13148,#2258,.T.);
#17276=EDGE_CURVE('',#13149,#12813,#2259,.T.);
#17277=EDGE_CURVE('',#13149,#13148,#4005,.T.);
#17278=EDGE_CURVE('',#12810,#13150,#2260,.T.);
#17279=EDGE_CURVE('',#13151,#12809,#2261,.T.);
#17280=EDGE_CURVE('',#13151,#13150,#4006,.T.);
#17281=EDGE_CURVE('',#12806,#13152,#2262,.T.);
#17282=EDGE_CURVE('',#13153,#12805,#2263,.T.);
#17283=EDGE_CURVE('',#13153,#13152,#4007,.T.);
#17284=EDGE_CURVE('',#12802,#13154,#2264,.T.);
#17285=EDGE_CURVE('',#13155,#12801,#2265,.T.);
#17286=EDGE_CURVE('',#13155,#13154,#4008,.T.);
#17287=EDGE_CURVE('',#12798,#13156,#2266,.T.);
#17288=EDGE_CURVE('',#13157,#12797,#2267,.T.);
#17289=EDGE_CURVE('',#13157,#13156,#4009,.T.);
#17290=EDGE_CURVE('',#12794,#13158,#2268,.T.);
#17291=EDGE_CURVE('',#13159,#12793,#2269,.T.);
#17292=EDGE_CURVE('',#13159,#13158,#4010,.T.);
#17293=EDGE_CURVE('',#12790,#13160,#2270,.T.);
#17294=EDGE_CURVE('',#13161,#12789,#2271,.T.);
#17295=EDGE_CURVE('',#13161,#13160,#4011,.T.);
#17296=EDGE_CURVE('',#12786,#13162,#2272,.T.);
#17297=EDGE_CURVE('',#13163,#12785,#2273,.T.);
#17298=EDGE_CURVE('',#13163,#13162,#4012,.T.);
#17299=EDGE_CURVE('',#12782,#13164,#2274,.T.);
#17300=EDGE_CURVE('',#13165,#12781,#2275,.T.);
#17301=EDGE_CURVE('',#13165,#13164,#4013,.T.);
#17302=EDGE_CURVE('',#12778,#13166,#2276,.T.);
#17303=EDGE_CURVE('',#13167,#12777,#2277,.T.);
#17304=EDGE_CURVE('',#13167,#13166,#4014,.T.);
#17305=EDGE_CURVE('',#12774,#13168,#2278,.T.);
#17306=EDGE_CURVE('',#13169,#12773,#2279,.T.);
#17307=EDGE_CURVE('',#13169,#13168,#4015,.T.);
#17308=EDGE_CURVE('',#12770,#13170,#2280,.T.);
#17309=EDGE_CURVE('',#13171,#12769,#2281,.T.);
#17310=EDGE_CURVE('',#13171,#13170,#4016,.T.);
#17311=EDGE_CURVE('',#12766,#13172,#2282,.T.);
#17312=EDGE_CURVE('',#13173,#12765,#2283,.T.);
#17313=EDGE_CURVE('',#13173,#13172,#4017,.T.);
#17314=EDGE_CURVE('',#12762,#13174,#2284,.T.);
#17315=EDGE_CURVE('',#13175,#12761,#2285,.T.);
#17316=EDGE_CURVE('',#13175,#13174,#4018,.T.);
#17317=EDGE_CURVE('',#13176,#13003,#2286,.T.);
#17318=EDGE_CURVE('',#13176,#13177,#4019,.T.);
#17319=EDGE_CURVE('',#13004,#13177,#2287,.T.);
#17320=EDGE_CURVE('',#13178,#13005,#2288,.T.);
#17321=EDGE_CURVE('',#13178,#13179,#4020,.T.);
#17322=EDGE_CURVE('',#13006,#13179,#2289,.T.);
#17323=EDGE_CURVE('',#13180,#13007,#2290,.T.);
#17324=EDGE_CURVE('',#13180,#13181,#4021,.T.);
#17325=EDGE_CURVE('',#13008,#13181,#2291,.T.);
#17326=EDGE_CURVE('',#13182,#13009,#2292,.T.);
#17327=EDGE_CURVE('',#13182,#13183,#4022,.T.);
#17328=EDGE_CURVE('',#13010,#13183,#2293,.T.);
#17329=EDGE_CURVE('',#13184,#13011,#2294,.T.);
#17330=EDGE_CURVE('',#13184,#13185,#4023,.T.);
#17331=EDGE_CURVE('',#13012,#13185,#2295,.T.);
#17332=EDGE_CURVE('',#13186,#13013,#2296,.T.);
#17333=EDGE_CURVE('',#13186,#13187,#4024,.T.);
#17334=EDGE_CURVE('',#13014,#13187,#2297,.T.);
#17335=EDGE_CURVE('',#13188,#13015,#2298,.T.);
#17336=EDGE_CURVE('',#13188,#13189,#4025,.T.);
#17337=EDGE_CURVE('',#13016,#13189,#2299,.T.);
#17338=EDGE_CURVE('',#13190,#13017,#2300,.T.);
#17339=EDGE_CURVE('',#13190,#13191,#4026,.T.);
#17340=EDGE_CURVE('',#13018,#13191,#2301,.T.);
#17341=EDGE_CURVE('',#13192,#13019,#2302,.T.);
#17342=EDGE_CURVE('',#13192,#13193,#4027,.T.);
#17343=EDGE_CURVE('',#13020,#13193,#2303,.T.);
#17344=EDGE_CURVE('',#13194,#13023,#2304,.T.);
#17345=EDGE_CURVE('',#13194,#13195,#4028,.T.);
#17346=EDGE_CURVE('',#13024,#13195,#2305,.T.);
#17347=EDGE_CURVE('',#13196,#13027,#2306,.T.);
#17348=EDGE_CURVE('',#13196,#13197,#4029,.T.);
#17349=EDGE_CURVE('',#13028,#13197,#2307,.T.);
#17350=EDGE_CURVE('',#13198,#13031,#2308,.T.);
#17351=EDGE_CURVE('',#13198,#13199,#4030,.T.);
#17352=EDGE_CURVE('',#13032,#13199,#2309,.T.);
#17353=EDGE_CURVE('',#13200,#13035,#2310,.T.);
#17354=EDGE_CURVE('',#13200,#13201,#4031,.T.);
#17355=EDGE_CURVE('',#13036,#13201,#2311,.T.);
#17356=EDGE_CURVE('',#13202,#13039,#2312,.T.);
#17357=EDGE_CURVE('',#13202,#13203,#4032,.T.);
#17358=EDGE_CURVE('',#13040,#13203,#2313,.T.);
#17359=EDGE_CURVE('',#12758,#13204,#2314,.T.);
#17360=EDGE_CURVE('',#13205,#12757,#2315,.T.);
#17361=EDGE_CURVE('',#13205,#13204,#4033,.T.);
#17362=EDGE_CURVE('',#13206,#13048,#9147,.T.);
#17363=EDGE_CURVE('',#13206,#13207,#4034,.T.);
#17364=EDGE_CURVE('',#13049,#13207,#9148,.T.);
#17365=EDGE_CURVE('',#13050,#13208,#9149,.T.);
#17366=EDGE_CURVE('',#13209,#13051,#9150,.T.);
#17367=EDGE_CURVE('',#13209,#13208,#4035,.T.);
#17368=EDGE_CURVE('',#13052,#13210,#9151,.T.);
#17369=EDGE_CURVE('',#13211,#13053,#9152,.T.);
#17370=EDGE_CURVE('',#13211,#13210,#4036,.T.);
#17371=EDGE_CURVE('',#13054,#13212,#9153,.T.);
#17372=EDGE_CURVE('',#13213,#13055,#9154,.T.);
#17373=EDGE_CURVE('',#13213,#13212,#4037,.T.);
#17374=EDGE_CURVE('',#13056,#13214,#9155,.T.);
#17375=EDGE_CURVE('',#13215,#13057,#9156,.T.);
#17376=EDGE_CURVE('',#13215,#13214,#4038,.T.);
#17377=EDGE_CURVE('',#13058,#13216,#9157,.T.);
#17378=EDGE_CURVE('',#13217,#13059,#9158,.T.);
#17379=EDGE_CURVE('',#13217,#13216,#4039,.T.);
#17380=EDGE_CURVE('',#13060,#13218,#9159,.T.);
#17381=EDGE_CURVE('',#13219,#13061,#9160,.T.);
#17382=EDGE_CURVE('',#13219,#13218,#4040,.T.);
#17383=EDGE_CURVE('',#13062,#13220,#9161,.T.);
#17384=EDGE_CURVE('',#13221,#13063,#9162,.T.);
#17385=EDGE_CURVE('',#13221,#13220,#4041,.T.);
#17386=EDGE_CURVE('',#13064,#13222,#9163,.T.);
#17387=EDGE_CURVE('',#13223,#13065,#9164,.T.);
#17388=EDGE_CURVE('',#13223,#13222,#4042,.T.);
#17389=EDGE_CURVE('',#13066,#13224,#9165,.T.);
#17390=EDGE_CURVE('',#13225,#13067,#9166,.T.);
#17391=EDGE_CURVE('',#13225,#13224,#4043,.T.);
#17392=EDGE_CURVE('',#13068,#13226,#9167,.T.);
#17393=EDGE_CURVE('',#13227,#13069,#9168,.T.);
#17394=EDGE_CURVE('',#13227,#13226,#4044,.T.);
#17395=EDGE_CURVE('',#13070,#13228,#9169,.T.);
#17396=EDGE_CURVE('',#13229,#13071,#9170,.T.);
#17397=EDGE_CURVE('',#13229,#13228,#4045,.T.);
#17398=EDGE_CURVE('',#13072,#13230,#9171,.T.);
#17399=EDGE_CURVE('',#13231,#13073,#9172,.T.);
#17400=EDGE_CURVE('',#13231,#13230,#4046,.T.);
#17401=EDGE_CURVE('',#13074,#13232,#9173,.T.);
#17402=EDGE_CURVE('',#13233,#13075,#9174,.T.);
#17403=EDGE_CURVE('',#13233,#13232,#4047,.T.);
#17404=EDGE_CURVE('',#13076,#13234,#9175,.T.);
#17405=EDGE_CURVE('',#13235,#13077,#9176,.T.);
#17406=EDGE_CURVE('',#13235,#13234,#4048,.T.);
#17407=EDGE_CURVE('',#13078,#13236,#9177,.T.);
#17408=EDGE_CURVE('',#13237,#13079,#9178,.T.);
#17409=EDGE_CURVE('',#13237,#13236,#4049,.T.);
#17410=EDGE_CURVE('',#13080,#13238,#9179,.T.);
#17411=EDGE_CURVE('',#13239,#13081,#9180,.T.);
#17412=EDGE_CURVE('',#13239,#13238,#4050,.T.);
#17413=EDGE_CURVE('',#13082,#13240,#9181,.T.);
#17414=EDGE_CURVE('',#13241,#13083,#9182,.T.);
#17415=EDGE_CURVE('',#13241,#13240,#4051,.T.);
#17416=EDGE_CURVE('',#13084,#13242,#9183,.T.);
#17417=EDGE_CURVE('',#13243,#13085,#9184,.T.);
#17418=EDGE_CURVE('',#13243,#13242,#4052,.T.);
#17419=EDGE_CURVE('',#13086,#13244,#9185,.T.);
#17420=EDGE_CURVE('',#13245,#13087,#9186,.T.);
#17421=EDGE_CURVE('',#13245,#13244,#4053,.T.);
#17422=EDGE_CURVE('',#13088,#13246,#9187,.T.);
#17423=EDGE_CURVE('',#13247,#13089,#9188,.T.);
#17424=EDGE_CURVE('',#13247,#13246,#4054,.T.);
#17425=EDGE_CURVE('',#13090,#13248,#9189,.T.);
#17426=EDGE_CURVE('',#13249,#13091,#9190,.T.);
#17427=EDGE_CURVE('',#13249,#13248,#4055,.T.);
#17428=EDGE_CURVE('',#13092,#13250,#9191,.T.);
#17429=EDGE_CURVE('',#13251,#13093,#9192,.T.);
#17430=EDGE_CURVE('',#13251,#13250,#4056,.T.);
#17431=EDGE_CURVE('',#13094,#13252,#9193,.T.);
#17432=EDGE_CURVE('',#13253,#13095,#9194,.T.);
#17433=EDGE_CURVE('',#13253,#13252,#4057,.T.);
#17434=EDGE_CURVE('',#13096,#13254,#9195,.T.);
#17435=EDGE_CURVE('',#13255,#13097,#9196,.T.);
#17436=EDGE_CURVE('',#13255,#13254,#4058,.T.);
#17437=EDGE_CURVE('',#13098,#13256,#9197,.T.);
#17438=EDGE_CURVE('',#13257,#13099,#9198,.T.);
#17439=EDGE_CURVE('',#13257,#13256,#4059,.T.);
#17440=EDGE_CURVE('',#13100,#13258,#9199,.T.);
#17441=EDGE_CURVE('',#13259,#13101,#9200,.T.);
#17442=EDGE_CURVE('',#13259,#13258,#4060,.T.);
#17443=EDGE_CURVE('',#13102,#13260,#9201,.T.);
#17444=EDGE_CURVE('',#13261,#13103,#9202,.T.);
#17445=EDGE_CURVE('',#13261,#13260,#4061,.T.);
#17446=EDGE_CURVE('',#13104,#13262,#9203,.T.);
#17447=EDGE_CURVE('',#13263,#13105,#9204,.T.);
#17448=EDGE_CURVE('',#13263,#13262,#4062,.T.);
#17449=EDGE_CURVE('',#13106,#13264,#9205,.T.);
#17450=EDGE_CURVE('',#13265,#13107,#9206,.T.);
#17451=EDGE_CURVE('',#13265,#13264,#4063,.T.);
#17452=EDGE_CURVE('',#13108,#13266,#9207,.T.);
#17453=EDGE_CURVE('',#13267,#13109,#9208,.T.);
#17454=EDGE_CURVE('',#13267,#13266,#4064,.T.);
#17455=EDGE_CURVE('',#13110,#13268,#9209,.T.);
#17456=EDGE_CURVE('',#13269,#13111,#9210,.T.);
#17457=EDGE_CURVE('',#13269,#13268,#4065,.T.);
#17458=EDGE_CURVE('',#13112,#13270,#9211,.T.);
#17459=EDGE_CURVE('',#13271,#13113,#9212,.T.);
#17460=EDGE_CURVE('',#13271,#13270,#4066,.T.);
#17461=EDGE_CURVE('',#13114,#13272,#9213,.T.);
#17462=EDGE_CURVE('',#13273,#13115,#9214,.T.);
#17463=EDGE_CURVE('',#13273,#13272,#4067,.T.);
#17464=EDGE_CURVE('',#13116,#13274,#9215,.T.);
#17465=EDGE_CURVE('',#13275,#13117,#9216,.T.);
#17466=EDGE_CURVE('',#13275,#13274,#4068,.T.);
#17467=EDGE_CURVE('',#13118,#13276,#9217,.T.);
#17468=EDGE_CURVE('',#13277,#13119,#9218,.T.);
#17469=EDGE_CURVE('',#13277,#13276,#4069,.T.);
#17470=EDGE_CURVE('',#13120,#13278,#9219,.T.);
#17471=EDGE_CURVE('',#13279,#13121,#9220,.T.);
#17472=EDGE_CURVE('',#13279,#13278,#4070,.T.);
#17473=EDGE_CURVE('',#13122,#13280,#9221,.T.);
#17474=EDGE_CURVE('',#13281,#13123,#9222,.T.);
#17475=EDGE_CURVE('',#13281,#13280,#4071,.T.);
#17476=EDGE_CURVE('',#13124,#13282,#9223,.T.);
#17477=EDGE_CURVE('',#13283,#13125,#9224,.T.);
#17478=EDGE_CURVE('',#13283,#13282,#4072,.T.);
#17479=EDGE_CURVE('',#13126,#13284,#9225,.T.);
#17480=EDGE_CURVE('',#13285,#13127,#9226,.T.);
#17481=EDGE_CURVE('',#13285,#13284,#4073,.T.);
#17482=EDGE_CURVE('',#13128,#13286,#9227,.T.);
#17483=EDGE_CURVE('',#13287,#13129,#9228,.T.);
#17484=EDGE_CURVE('',#13287,#13286,#4074,.T.);
#17485=EDGE_CURVE('',#13130,#13288,#9229,.T.);
#17486=EDGE_CURVE('',#13289,#13131,#9230,.T.);
#17487=EDGE_CURVE('',#13289,#13288,#4075,.T.);
#17488=EDGE_CURVE('',#13132,#13290,#9231,.T.);
#17489=EDGE_CURVE('',#13291,#13133,#9232,.T.);
#17490=EDGE_CURVE('',#13291,#13290,#4076,.T.);
#17491=EDGE_CURVE('',#13134,#13292,#9233,.T.);
#17492=EDGE_CURVE('',#13293,#13135,#9234,.T.);
#17493=EDGE_CURVE('',#13293,#13292,#4077,.T.);
#17494=EDGE_CURVE('',#13136,#13294,#9235,.T.);
#17495=EDGE_CURVE('',#13295,#13137,#9236,.T.);
#17496=EDGE_CURVE('',#13295,#13294,#4078,.T.);
#17497=EDGE_CURVE('',#13138,#13296,#9237,.T.);
#17498=EDGE_CURVE('',#13297,#13139,#9238,.T.);
#17499=EDGE_CURVE('',#13297,#13296,#4079,.T.);
#17500=EDGE_CURVE('',#13140,#13298,#9239,.T.);
#17501=EDGE_CURVE('',#13299,#13141,#9240,.T.);
#17502=EDGE_CURVE('',#13299,#13298,#4080,.T.);
#17503=EDGE_CURVE('',#13142,#13300,#9241,.T.);
#17504=EDGE_CURVE('',#13301,#13143,#9242,.T.);
#17505=EDGE_CURVE('',#13301,#13300,#4081,.T.);
#17506=EDGE_CURVE('',#13144,#13302,#9243,.T.);
#17507=EDGE_CURVE('',#13303,#13145,#9244,.T.);
#17508=EDGE_CURVE('',#13303,#13302,#4082,.T.);
#17509=EDGE_CURVE('',#13146,#13304,#9245,.T.);
#17510=EDGE_CURVE('',#13305,#13147,#9246,.T.);
#17511=EDGE_CURVE('',#13305,#13304,#4083,.T.);
#17512=EDGE_CURVE('',#13148,#13306,#9247,.T.);
#17513=EDGE_CURVE('',#13307,#13149,#9248,.T.);
#17514=EDGE_CURVE('',#13307,#13306,#4084,.T.);
#17515=EDGE_CURVE('',#13150,#13308,#9249,.T.);
#17516=EDGE_CURVE('',#13309,#13151,#9250,.T.);
#17517=EDGE_CURVE('',#13309,#13308,#4085,.T.);
#17518=EDGE_CURVE('',#13152,#13310,#9251,.T.);
#17519=EDGE_CURVE('',#13311,#13153,#9252,.T.);
#17520=EDGE_CURVE('',#13311,#13310,#4086,.T.);
#17521=EDGE_CURVE('',#13154,#13312,#9253,.T.);
#17522=EDGE_CURVE('',#13313,#13155,#9254,.T.);
#17523=EDGE_CURVE('',#13313,#13312,#4087,.T.);
#17524=EDGE_CURVE('',#13156,#13314,#9255,.T.);
#17525=EDGE_CURVE('',#13315,#13157,#9256,.T.);
#17526=EDGE_CURVE('',#13315,#13314,#4088,.T.);
#17527=EDGE_CURVE('',#13158,#13316,#9257,.T.);
#17528=EDGE_CURVE('',#13317,#13159,#9258,.T.);
#17529=EDGE_CURVE('',#13317,#13316,#4089,.T.);
#17530=EDGE_CURVE('',#13160,#13318,#9259,.T.);
#17531=EDGE_CURVE('',#13319,#13161,#9260,.T.);
#17532=EDGE_CURVE('',#13319,#13318,#4090,.T.);
#17533=EDGE_CURVE('',#13162,#13320,#9261,.T.);
#17534=EDGE_CURVE('',#13321,#13163,#9262,.T.);
#17535=EDGE_CURVE('',#13321,#13320,#4091,.T.);
#17536=EDGE_CURVE('',#13164,#13322,#9263,.T.);
#17537=EDGE_CURVE('',#13323,#13165,#9264,.T.);
#17538=EDGE_CURVE('',#13323,#13322,#4092,.T.);
#17539=EDGE_CURVE('',#13166,#13324,#9265,.T.);
#17540=EDGE_CURVE('',#13325,#13167,#9266,.T.);
#17541=EDGE_CURVE('',#13325,#13324,#4093,.T.);
#17542=EDGE_CURVE('',#13168,#13326,#9267,.T.);
#17543=EDGE_CURVE('',#13327,#13169,#9268,.T.);
#17544=EDGE_CURVE('',#13327,#13326,#4094,.T.);
#17545=EDGE_CURVE('',#13170,#13328,#9269,.T.);
#17546=EDGE_CURVE('',#13329,#13171,#9270,.T.);
#17547=EDGE_CURVE('',#13329,#13328,#4095,.T.);
#17548=EDGE_CURVE('',#13172,#13330,#9271,.T.);
#17549=EDGE_CURVE('',#13331,#13173,#9272,.T.);
#17550=EDGE_CURVE('',#13331,#13330,#4096,.T.);
#17551=EDGE_CURVE('',#13174,#13332,#9273,.T.);
#17552=EDGE_CURVE('',#13333,#13175,#9274,.T.);
#17553=EDGE_CURVE('',#13333,#13332,#4097,.T.);
#17554=EDGE_CURVE('',#13334,#13176,#9275,.T.);
#17555=EDGE_CURVE('',#13334,#13335,#4098,.T.);
#17556=EDGE_CURVE('',#13177,#13335,#9276,.T.);
#17557=EDGE_CURVE('',#13336,#13178,#9277,.T.);
#17558=EDGE_CURVE('',#13336,#13337,#4099,.T.);
#17559=EDGE_CURVE('',#13179,#13337,#9278,.T.);
#17560=EDGE_CURVE('',#13338,#13180,#9279,.T.);
#17561=EDGE_CURVE('',#13338,#13339,#4100,.T.);
#17562=EDGE_CURVE('',#13181,#13339,#9280,.T.);
#17563=EDGE_CURVE('',#13340,#13182,#9281,.T.);
#17564=EDGE_CURVE('',#13340,#13341,#4101,.T.);
#17565=EDGE_CURVE('',#13183,#13341,#9282,.T.);
#17566=EDGE_CURVE('',#13342,#13184,#9283,.T.);
#17567=EDGE_CURVE('',#13342,#13343,#4102,.T.);
#17568=EDGE_CURVE('',#13185,#13343,#9284,.T.);
#17569=EDGE_CURVE('',#13344,#13186,#9285,.T.);
#17570=EDGE_CURVE('',#13344,#13345,#4103,.T.);
#17571=EDGE_CURVE('',#13187,#13345,#9286,.T.);
#17572=EDGE_CURVE('',#13346,#13188,#9287,.T.);
#17573=EDGE_CURVE('',#13346,#13347,#4104,.T.);
#17574=EDGE_CURVE('',#13189,#13347,#9288,.T.);
#17575=EDGE_CURVE('',#13348,#13190,#9289,.T.);
#17576=EDGE_CURVE('',#13348,#13349,#4105,.T.);
#17577=EDGE_CURVE('',#13191,#13349,#9290,.T.);
#17578=EDGE_CURVE('',#13350,#13192,#9291,.T.);
#17579=EDGE_CURVE('',#13350,#13351,#4106,.T.);
#17580=EDGE_CURVE('',#13193,#13351,#9292,.T.);
#17581=EDGE_CURVE('',#13352,#13194,#9293,.T.);
#17582=EDGE_CURVE('',#13352,#13353,#4107,.T.);
#17583=EDGE_CURVE('',#13195,#13353,#9294,.T.);
#17584=EDGE_CURVE('',#13354,#13196,#9295,.T.);
#17585=EDGE_CURVE('',#13354,#13355,#4108,.T.);
#17586=EDGE_CURVE('',#13197,#13355,#9296,.T.);
#17587=EDGE_CURVE('',#13356,#13198,#9297,.T.);
#17588=EDGE_CURVE('',#13356,#13357,#4109,.T.);
#17589=EDGE_CURVE('',#13199,#13357,#9298,.T.);
#17590=EDGE_CURVE('',#13358,#13200,#9299,.T.);
#17591=EDGE_CURVE('',#13358,#13359,#4110,.T.);
#17592=EDGE_CURVE('',#13201,#13359,#9300,.T.);
#17593=EDGE_CURVE('',#13360,#13202,#9301,.T.);
#17594=EDGE_CURVE('',#13360,#13361,#4111,.T.);
#17595=EDGE_CURVE('',#13203,#13361,#9302,.T.);
#17596=EDGE_CURVE('',#13204,#13362,#9303,.T.);
#17597=EDGE_CURVE('',#13363,#13205,#9304,.T.);
#17598=EDGE_CURVE('',#13363,#13362,#4112,.T.);
#17599=EDGE_CURVE('',#12661,#13206,#2316,.T.);
#17600=EDGE_CURVE('',#13207,#12660,#2317,.T.);
#17601=EDGE_CURVE('',#13208,#12662,#2318,.T.);
#17602=EDGE_CURVE('',#12663,#13209,#2319,.T.);
#17603=EDGE_CURVE('',#13210,#12664,#2320,.T.);
#17604=EDGE_CURVE('',#12665,#13211,#2321,.T.);
#17605=EDGE_CURVE('',#13212,#12666,#2322,.T.);
#17606=EDGE_CURVE('',#12667,#13213,#2323,.T.);
#17607=EDGE_CURVE('',#13214,#12668,#2324,.T.);
#17608=EDGE_CURVE('',#12669,#13215,#2325,.T.);
#17609=EDGE_CURVE('',#13216,#12670,#2326,.T.);
#17610=EDGE_CURVE('',#12671,#13217,#2327,.T.);
#17611=EDGE_CURVE('',#13218,#12672,#2328,.T.);
#17612=EDGE_CURVE('',#12673,#13219,#2329,.T.);
#17613=EDGE_CURVE('',#13220,#12676,#2330,.T.);
#17614=EDGE_CURVE('',#12677,#13221,#2331,.T.);
#17615=EDGE_CURVE('',#13222,#12680,#2332,.T.);
#17616=EDGE_CURVE('',#12681,#13223,#2333,.T.);
#17617=EDGE_CURVE('',#13224,#12684,#2334,.T.);
#17618=EDGE_CURVE('',#12685,#13225,#2335,.T.);
#17619=EDGE_CURVE('',#13226,#12688,#2336,.T.);
#17620=EDGE_CURVE('',#12689,#13227,#2337,.T.);
#17621=EDGE_CURVE('',#13228,#12692,#2338,.T.);
#17622=EDGE_CURVE('',#12693,#13229,#2339,.T.);
#17623=EDGE_CURVE('',#13230,#12696,#2340,.T.);
#17624=EDGE_CURVE('',#12697,#13231,#2341,.T.);
#17625=EDGE_CURVE('',#13232,#12700,#2342,.T.);
#17626=EDGE_CURVE('',#12701,#13233,#2343,.T.);
#17627=EDGE_CURVE('',#13234,#12704,#2344,.T.);
#17628=EDGE_CURVE('',#12705,#13235,#2345,.T.);
#17629=EDGE_CURVE('',#13236,#12708,#2346,.T.);
#17630=EDGE_CURVE('',#12709,#13237,#2347,.T.);
#17631=EDGE_CURVE('',#13238,#12712,#2348,.T.);
#17632=EDGE_CURVE('',#12713,#13239,#2349,.T.);
#17633=EDGE_CURVE('',#13240,#12716,#2350,.T.);
#17634=EDGE_CURVE('',#12717,#13241,#2351,.T.);
#17635=EDGE_CURVE('',#13242,#12720,#2352,.T.);
#17636=EDGE_CURVE('',#12721,#13243,#2353,.T.);
#17637=EDGE_CURVE('',#13244,#12724,#2354,.T.);
#17638=EDGE_CURVE('',#12725,#13245,#2355,.T.);
#17639=EDGE_CURVE('',#13246,#12728,#2356,.T.);
#17640=EDGE_CURVE('',#12729,#13247,#2357,.T.);
#17641=EDGE_CURVE('',#13248,#12732,#2358,.T.);
#17642=EDGE_CURVE('',#12733,#13249,#2359,.T.);
#17643=EDGE_CURVE('',#13250,#12736,#2360,.T.);
#17644=EDGE_CURVE('',#12737,#13251,#2361,.T.);
#17645=EDGE_CURVE('',#13252,#12740,#2362,.T.);
#17646=EDGE_CURVE('',#12741,#13253,#2363,.T.);
#17647=EDGE_CURVE('',#13254,#12744,#2364,.T.);
#17648=EDGE_CURVE('',#12745,#13255,#2365,.T.);
#17649=EDGE_CURVE('',#13256,#12748,#2366,.T.);
#17650=EDGE_CURVE('',#12749,#13257,#2367,.T.);
#17651=EDGE_CURVE('',#13258,#12462,#2368,.T.);
#17652=EDGE_CURVE('',#12463,#13259,#2369,.T.);
#17653=EDGE_CURVE('',#13260,#12466,#2370,.T.);
#17654=EDGE_CURVE('',#12467,#13261,#2371,.T.);
#17655=EDGE_CURVE('',#13262,#12470,#2372,.T.);
#17656=EDGE_CURVE('',#12471,#13263,#2373,.T.);
#17657=EDGE_CURVE('',#13264,#12474,#2374,.T.);
#17658=EDGE_CURVE('',#12475,#13265,#2375,.T.);
#17659=EDGE_CURVE('',#13266,#12478,#2376,.T.);
#17660=EDGE_CURVE('',#12479,#13267,#2377,.T.);
#17661=EDGE_CURVE('',#13268,#12482,#2378,.T.);
#17662=EDGE_CURVE('',#12483,#13269,#2379,.T.);
#17663=EDGE_CURVE('',#13270,#12486,#2380,.T.);
#17664=EDGE_CURVE('',#12487,#13271,#2381,.T.);
#17665=EDGE_CURVE('',#13272,#12490,#2382,.T.);
#17666=EDGE_CURVE('',#12491,#13273,#2383,.T.);
#17667=EDGE_CURVE('',#13274,#12494,#2384,.T.);
#17668=EDGE_CURVE('',#12495,#13275,#2385,.T.);
#17669=EDGE_CURVE('',#13276,#12498,#2386,.T.);
#17670=EDGE_CURVE('',#12499,#13277,#2387,.T.);
#17671=EDGE_CURVE('',#13278,#12502,#2388,.T.);
#17672=EDGE_CURVE('',#12503,#13279,#2389,.T.);
#17673=EDGE_CURVE('',#13280,#12506,#2390,.T.);
#17674=EDGE_CURVE('',#12507,#13281,#2391,.T.);
#17675=EDGE_CURVE('',#13282,#12510,#2392,.T.);
#17676=EDGE_CURVE('',#12511,#13283,#2393,.T.);
#17677=EDGE_CURVE('',#13284,#12514,#2394,.T.);
#17678=EDGE_CURVE('',#12515,#13285,#2395,.T.);
#17679=EDGE_CURVE('',#13286,#12518,#2396,.T.);
#17680=EDGE_CURVE('',#12519,#13287,#2397,.T.);
#17681=EDGE_CURVE('',#13288,#12522,#2398,.T.);
#17682=EDGE_CURVE('',#12523,#13289,#2399,.T.);
#17683=EDGE_CURVE('',#13290,#12526,#2400,.T.);
#17684=EDGE_CURVE('',#12527,#13291,#2401,.T.);
#17685=EDGE_CURVE('',#13292,#12530,#2402,.T.);
#17686=EDGE_CURVE('',#12531,#13293,#2403,.T.);
#17687=EDGE_CURVE('',#13294,#12534,#2404,.T.);
#17688=EDGE_CURVE('',#12535,#13295,#2405,.T.);
#17689=EDGE_CURVE('',#13296,#12538,#2406,.T.);
#17690=EDGE_CURVE('',#12539,#13297,#2407,.T.);
#17691=EDGE_CURVE('',#13298,#12542,#2408,.T.);
#17692=EDGE_CURVE('',#12543,#13299,#2409,.T.);
#17693=EDGE_CURVE('',#13300,#12546,#2410,.T.);
#17694=EDGE_CURVE('',#12547,#13301,#2411,.T.);
#17695=EDGE_CURVE('',#13302,#12550,#2412,.T.);
#17696=EDGE_CURVE('',#12551,#13303,#2413,.T.);
#17697=EDGE_CURVE('',#13304,#12554,#2414,.T.);
#17698=EDGE_CURVE('',#12555,#13305,#2415,.T.);
#17699=EDGE_CURVE('',#13306,#12558,#2416,.T.);
#17700=EDGE_CURVE('',#12559,#13307,#2417,.T.);
#17701=EDGE_CURVE('',#13308,#12562,#2418,.T.);
#17702=EDGE_CURVE('',#12563,#13309,#2419,.T.);
#17703=EDGE_CURVE('',#13310,#12566,#2420,.T.);
#17704=EDGE_CURVE('',#12567,#13311,#2421,.T.);
#17705=EDGE_CURVE('',#13312,#12570,#2422,.T.);
#17706=EDGE_CURVE('',#12571,#13313,#2423,.T.);
#17707=EDGE_CURVE('',#13314,#12574,#2424,.T.);
#17708=EDGE_CURVE('',#12575,#13315,#2425,.T.);
#17709=EDGE_CURVE('',#13316,#12578,#2426,.T.);
#17710=EDGE_CURVE('',#12579,#13317,#2427,.T.);
#17711=EDGE_CURVE('',#13318,#12582,#2428,.T.);
#17712=EDGE_CURVE('',#12583,#13319,#2429,.T.);
#17713=EDGE_CURVE('',#13320,#12586,#2430,.T.);
#17714=EDGE_CURVE('',#12587,#13321,#2431,.T.);
#17715=EDGE_CURVE('',#13322,#12590,#2432,.T.);
#17716=EDGE_CURVE('',#12591,#13323,#2433,.T.);
#17717=EDGE_CURVE('',#13324,#12594,#2434,.T.);
#17718=EDGE_CURVE('',#12595,#13325,#2435,.T.);
#17719=EDGE_CURVE('',#13326,#12598,#2436,.T.);
#17720=EDGE_CURVE('',#12599,#13327,#2437,.T.);
#17721=EDGE_CURVE('',#13328,#12602,#2438,.T.);
#17722=EDGE_CURVE('',#12603,#13329,#2439,.T.);
#17723=EDGE_CURVE('',#13330,#12606,#2440,.T.);
#17724=EDGE_CURVE('',#12607,#13331,#2441,.T.);
#17725=EDGE_CURVE('',#13332,#12610,#2442,.T.);
#17726=EDGE_CURVE('',#12611,#13333,#2443,.T.);
#17727=EDGE_CURVE('',#12659,#13334,#2444,.T.);
#17728=EDGE_CURVE('',#13335,#12658,#2445,.T.);
#17729=EDGE_CURVE('',#12657,#13336,#2446,.T.);
#17730=EDGE_CURVE('',#13337,#12656,#2447,.T.);
#17731=EDGE_CURVE('',#12655,#13338,#2448,.T.);
#17732=EDGE_CURVE('',#13339,#12654,#2449,.T.);
#17733=EDGE_CURVE('',#12653,#13340,#2450,.T.);
#17734=EDGE_CURVE('',#13341,#12652,#2451,.T.);
#17735=EDGE_CURVE('',#12651,#13342,#2452,.T.);
#17736=EDGE_CURVE('',#13343,#12650,#2453,.T.);
#17737=EDGE_CURVE('',#12649,#13344,#2454,.T.);
#17738=EDGE_CURVE('',#13345,#12648,#2455,.T.);
#17739=EDGE_CURVE('',#12647,#13346,#2456,.T.);
#17740=EDGE_CURVE('',#13347,#12646,#2457,.T.);
#17741=EDGE_CURVE('',#12645,#13348,#2458,.T.);
#17742=EDGE_CURVE('',#13349,#12644,#2459,.T.);
#17743=EDGE_CURVE('',#12643,#13350,#2460,.T.);
#17744=EDGE_CURVE('',#13351,#12642,#2461,.T.);
#17745=EDGE_CURVE('',#12639,#13352,#2462,.T.);
#17746=EDGE_CURVE('',#13353,#12638,#2463,.T.);
#17747=EDGE_CURVE('',#12635,#13354,#2464,.T.);
#17748=EDGE_CURVE('',#13355,#12634,#2465,.T.);
#17749=EDGE_CURVE('',#12631,#13356,#2466,.T.);
#17750=EDGE_CURVE('',#13357,#12630,#2467,.T.);
#17751=EDGE_CURVE('',#12627,#13358,#2468,.T.);
#17752=EDGE_CURVE('',#13359,#12626,#2469,.T.);
#17753=EDGE_CURVE('',#12623,#13360,#2470,.T.);
#17754=EDGE_CURVE('',#13361,#12622,#2471,.T.);
#17755=EDGE_CURVE('',#13362,#12614,#2472,.T.);
#17756=EDGE_CURVE('',#12615,#13363,#2473,.T.);
#17757=EDGE_CURVE('',#12754,#13364,#2474,.T.);
#17758=EDGE_CURVE('',#13365,#12753,#2475,.T.);
#17759=EDGE_CURVE('',#13365,#13364,#4113,.T.);
#17760=EDGE_CURVE('',#13364,#13366,#9305,.T.);
#17761=EDGE_CURVE('',#13367,#13365,#9306,.T.);
#17762=EDGE_CURVE('',#13367,#13366,#4114,.T.);
#17763=EDGE_CURVE('',#13366,#12618,#2476,.T.);
#17764=EDGE_CURVE('',#12619,#13367,#2477,.T.);
#17765=EDGE_CURVE('',#13368,#13369,#9307,.T.);
#17766=EDGE_CURVE('',#13369,#13370,#9308,.T.);
#17767=EDGE_CURVE('',#13370,#13371,#9309,.T.);
#17768=EDGE_CURVE('',#13371,#13372,#9310,.T.);
#17769=EDGE_CURVE('',#13372,#13373,#9311,.T.);
#17770=EDGE_CURVE('',#13373,#13368,#9312,.T.);
#17771=EDGE_CURVE('',#13369,#12454,#9313,.T.);
#17772=EDGE_CURVE('',#13370,#12453,#9314,.T.);
#17773=EDGE_CURVE('',#13371,#12452,#9315,.T.);
#17774=EDGE_CURVE('',#13372,#12450,#9316,.T.);
#17775=EDGE_CURVE('',#13373,#12456,#9317,.T.);
#17776=EDGE_CURVE('',#13368,#12455,#9318,.T.);
#17777=EDGE_CURVE('',#12387,#12269,#3225,.T.);
#17778=EDGE_CURVE('',#12267,#12385,#9319,.T.);
#17779=EDGE_CURVE('',#12751,#12620,#9320,.T.);
#17780=EDGE_CURVE('',#13041,#12621,#9321,.T.);
#17781=EDGE_CURVE('',#12756,#12616,#9322,.T.);
#17782=EDGE_CURVE('',#12755,#12617,#9323,.T.);
#17783=EDGE_CURVE('',#13038,#12624,#9324,.T.);
#17784=EDGE_CURVE('',#13037,#12625,#9325,.T.);
#17785=EDGE_CURVE('',#13034,#12628,#9326,.T.);
#17786=EDGE_CURVE('',#13033,#12629,#9327,.T.);
#17787=EDGE_CURVE('',#13030,#12632,#9328,.T.);
#17788=EDGE_CURVE('',#13029,#12633,#9329,.T.);
#17789=EDGE_CURVE('',#13026,#12636,#9330,.T.);
#17790=EDGE_CURVE('',#13025,#12637,#9331,.T.);
#17791=EDGE_CURVE('',#13022,#12640,#9332,.T.);
#17792=EDGE_CURVE('',#13021,#12641,#9333,.T.);
#17793=EDGE_CURVE('',#12760,#12612,#9334,.T.);
#17794=EDGE_CURVE('',#12759,#12613,#9335,.T.);
#17795=EDGE_CURVE('',#12764,#12608,#9336,.T.);
#17796=EDGE_CURVE('',#12763,#12609,#9337,.T.);
#17797=EDGE_CURVE('',#12768,#12604,#9338,.T.);
#17798=EDGE_CURVE('',#12767,#12605,#9339,.T.);
#17799=EDGE_CURVE('',#12772,#12600,#9340,.T.);
#17800=EDGE_CURVE('',#12771,#12601,#9341,.T.);
#17801=EDGE_CURVE('',#12776,#12596,#9342,.T.);
#17802=EDGE_CURVE('',#12775,#12597,#9343,.T.);
#17803=EDGE_CURVE('',#12780,#12592,#9344,.T.);
#17804=EDGE_CURVE('',#12779,#12593,#9345,.T.);
#17805=EDGE_CURVE('',#12784,#12588,#9346,.T.);
#17806=EDGE_CURVE('',#12783,#12589,#9347,.T.);
#17807=EDGE_CURVE('',#12788,#12584,#9348,.T.);
#17808=EDGE_CURVE('',#12787,#12585,#9349,.T.);
#17809=EDGE_CURVE('',#12792,#12580,#9350,.T.);
#17810=EDGE_CURVE('',#12791,#12581,#9351,.T.);
#17811=EDGE_CURVE('',#12796,#12576,#9352,.T.);
#17812=EDGE_CURVE('',#12795,#12577,#9353,.T.);
#17813=EDGE_CURVE('',#12800,#12572,#9354,.T.);
#17814=EDGE_CURVE('',#12799,#12573,#9355,.T.);
#17815=EDGE_CURVE('',#12804,#12568,#9356,.T.);
#17816=EDGE_CURVE('',#12803,#12569,#9357,.T.);
#17817=EDGE_CURVE('',#12808,#12564,#9358,.T.);
#17818=EDGE_CURVE('',#12807,#12565,#9359,.T.);
#17819=EDGE_CURVE('',#12812,#12560,#9360,.T.);
#17820=EDGE_CURVE('',#12811,#12561,#9361,.T.);
#17821=EDGE_CURVE('',#12816,#12556,#9362,.T.);
#17822=EDGE_CURVE('',#12815,#12557,#9363,.T.);
#17823=EDGE_CURVE('',#12820,#12552,#9364,.T.);
#17824=EDGE_CURVE('',#12819,#12553,#9365,.T.);
#17825=EDGE_CURVE('',#12824,#12548,#9366,.T.);
#17826=EDGE_CURVE('',#12823,#12549,#9367,.T.);
#17827=EDGE_CURVE('',#12828,#12544,#9368,.T.);
#17828=EDGE_CURVE('',#12827,#12545,#9369,.T.);
#17829=EDGE_CURVE('',#12832,#12540,#9370,.T.);
#17830=EDGE_CURVE('',#12831,#12541,#9371,.T.);
#17831=EDGE_CURVE('',#12836,#12536,#9372,.T.);
#17832=EDGE_CURVE('',#12835,#12537,#9373,.T.);
#17833=EDGE_CURVE('',#12840,#12532,#9374,.T.);
#17834=EDGE_CURVE('',#12839,#12533,#9375,.T.);
#17835=EDGE_CURVE('',#12844,#12528,#9376,.T.);
#17836=EDGE_CURVE('',#12843,#12529,#9377,.T.);
#17837=EDGE_CURVE('',#12848,#12524,#9378,.T.);
#17838=EDGE_CURVE('',#12847,#12525,#9379,.T.);
#17839=EDGE_CURVE('',#12852,#12520,#9380,.T.);
#17840=EDGE_CURVE('',#12851,#12521,#9381,.T.);
#17841=EDGE_CURVE('',#12856,#12516,#9382,.T.);
#17842=EDGE_CURVE('',#12855,#12517,#9383,.T.);
#17843=EDGE_CURVE('',#12860,#12512,#9384,.T.);
#17844=EDGE_CURVE('',#12859,#12513,#9385,.T.);
#17845=EDGE_CURVE('',#12864,#12508,#9386,.T.);
#17846=EDGE_CURVE('',#12863,#12509,#9387,.T.);
#17847=EDGE_CURVE('',#12868,#12504,#9388,.T.);
#17848=EDGE_CURVE('',#12867,#12505,#9389,.T.);
#17849=EDGE_CURVE('',#12872,#12500,#9390,.T.);
#17850=EDGE_CURVE('',#12871,#12501,#9391,.T.);
#17851=EDGE_CURVE('',#12876,#12496,#9392,.T.);
#17852=EDGE_CURVE('',#12875,#12497,#9393,.T.);
#17853=EDGE_CURVE('',#12880,#12492,#9394,.T.);
#17854=EDGE_CURVE('',#12879,#12493,#9395,.T.);
#17855=EDGE_CURVE('',#12884,#12488,#9396,.T.);
#17856=EDGE_CURVE('',#12883,#12489,#9397,.T.);
#17857=EDGE_CURVE('',#12888,#12484,#9398,.T.);
#17858=EDGE_CURVE('',#12887,#12485,#9399,.T.);
#17859=EDGE_CURVE('',#12892,#12480,#9400,.T.);
#17860=EDGE_CURVE('',#12891,#12481,#9401,.T.);
#17861=EDGE_CURVE('',#12896,#12476,#9402,.T.);
#17862=EDGE_CURVE('',#12895,#12477,#9403,.T.);
#17863=EDGE_CURVE('',#12900,#12472,#9404,.T.);
#17864=EDGE_CURVE('',#12899,#12473,#9405,.T.);
#17865=EDGE_CURVE('',#12904,#12468,#9406,.T.);
#17866=EDGE_CURVE('',#12903,#12469,#9407,.T.);
#17867=EDGE_CURVE('',#12908,#12464,#9408,.T.);
#17868=EDGE_CURVE('',#12907,#12465,#9409,.T.);
#17869=EDGE_CURVE('',#12912,#12750,#9410,.T.);
#17870=EDGE_CURVE('',#12911,#12460,#9411,.T.);
#17871=EDGE_CURVE('',#12916,#12746,#9412,.T.);
#17872=EDGE_CURVE('',#12915,#12747,#9413,.T.);
#17873=EDGE_CURVE('',#12920,#12742,#9414,.T.);
#17874=EDGE_CURVE('',#12919,#12743,#9415,.T.);
#17875=EDGE_CURVE('',#12924,#12738,#9416,.T.);
#17876=EDGE_CURVE('',#12923,#12739,#9417,.T.);
#17877=EDGE_CURVE('',#12928,#12734,#9418,.T.);
#17878=EDGE_CURVE('',#12927,#12735,#9419,.T.);
#17879=EDGE_CURVE('',#12932,#12730,#9420,.T.);
#17880=EDGE_CURVE('',#12931,#12731,#9421,.T.);
#17881=EDGE_CURVE('',#12936,#12726,#9422,.T.);
#17882=EDGE_CURVE('',#12935,#12727,#9423,.T.);
#17883=EDGE_CURVE('',#12940,#12722,#9424,.T.);
#17884=EDGE_CURVE('',#12939,#12723,#9425,.T.);
#17885=EDGE_CURVE('',#12944,#12718,#9426,.T.);
#17886=EDGE_CURVE('',#12943,#12719,#9427,.T.);
#17887=EDGE_CURVE('',#12948,#12714,#9428,.T.);
#17888=EDGE_CURVE('',#12947,#12715,#9429,.T.);
#17889=EDGE_CURVE('',#12952,#12710,#9430,.T.);
#17890=EDGE_CURVE('',#12951,#12711,#9431,.T.);
#17891=EDGE_CURVE('',#12956,#12706,#9432,.T.);
#17892=EDGE_CURVE('',#12955,#12707,#9433,.T.);
#17893=EDGE_CURVE('',#12960,#12702,#9434,.T.);
#17894=EDGE_CURVE('',#12959,#12703,#9435,.T.);
#17895=EDGE_CURVE('',#12964,#12698,#9436,.T.);
#17896=EDGE_CURVE('',#12963,#12699,#9437,.T.);
#17897=EDGE_CURVE('',#12968,#12694,#9438,.T.);
#17898=EDGE_CURVE('',#12967,#12695,#9439,.T.);
#17899=EDGE_CURVE('',#12972,#12690,#9440,.T.);
#17900=EDGE_CURVE('',#12971,#12691,#9441,.T.);
#17901=EDGE_CURVE('',#12976,#12686,#9442,.T.);
#17902=EDGE_CURVE('',#12975,#12687,#9443,.T.);
#17903=EDGE_CURVE('',#12980,#12682,#9444,.T.);
#17904=EDGE_CURVE('',#12979,#12683,#9445,.T.);
#17905=EDGE_CURVE('',#12984,#12678,#9446,.T.);
#17906=EDGE_CURVE('',#12983,#12679,#9447,.T.);
#17907=EDGE_CURVE('',#12988,#12674,#9448,.T.);
#17908=EDGE_CURVE('',#12987,#12675,#9449,.T.);
#17909=EDGE_CURVE('',#13374,#13375,#9450,.T.);
#17910=EDGE_CURVE('',#13376,#13374,#3226,.F.);
#17911=EDGE_CURVE('',#13376,#13377,#9451,.T.);
#17912=EDGE_CURVE('',#13377,#13377,#4115,.T.);
#17913=EDGE_CURVE('',#13378,#13376,#4116,.T.);
#17914=EDGE_CURVE('',#13375,#13378,#3227,.F.);
#17915=EDGE_CURVE('',#13379,#13380,#9452,.T.);
#17916=EDGE_CURVE('',#13374,#13379,#3228,.F.);
#17917=EDGE_CURVE('',#13380,#13375,#3229,.F.);
#17918=EDGE_CURVE('',#13381,#13382,#9453,.T.);
#17919=EDGE_CURVE('',#13379,#13381,#3230,.F.);
#17920=EDGE_CURVE('',#13382,#13380,#3231,.F.);
#17921=EDGE_CURVE('',#13383,#13384,#9454,.T.);
#17922=EDGE_CURVE('',#13381,#13383,#3232,.F.);
#17923=EDGE_CURVE('',#13384,#13382,#3233,.F.);
#17924=EDGE_CURVE('',#13385,#13386,#9455,.T.);
#17925=EDGE_CURVE('',#13383,#13385,#3234,.F.);
#17926=EDGE_CURVE('',#13386,#13384,#3235,.F.);
#17927=EDGE_CURVE('',#13387,#13388,#9456,.T.);
#17928=EDGE_CURVE('',#13385,#13387,#3236,.F.);
#17929=EDGE_CURVE('',#13388,#13386,#3237,.F.);
#17930=EDGE_CURVE('',#13389,#13390,#9457,.T.);
#17931=EDGE_CURVE('',#13387,#13389,#3238,.F.);
#17932=EDGE_CURVE('',#13390,#13388,#3239,.F.);
#17933=EDGE_CURVE('',#13391,#13392,#9458,.T.);
#17934=EDGE_CURVE('',#13389,#13391,#3240,.F.);
#17935=EDGE_CURVE('',#13392,#13390,#3241,.F.);
#17936=EDGE_CURVE('',#13393,#13394,#9459,.T.);
#17937=EDGE_CURVE('',#13391,#13393,#3242,.F.);
#17938=EDGE_CURVE('',#13394,#13392,#3243,.F.);
#17939=EDGE_CURVE('',#13395,#13396,#9460,.T.);
#17940=EDGE_CURVE('',#13393,#13395,#3244,.F.);
#17941=EDGE_CURVE('',#13396,#13394,#3245,.F.);
#17942=EDGE_CURVE('',#13397,#13398,#9461,.T.);
#17943=EDGE_CURVE('',#13395,#13397,#3246,.F.);
#17944=EDGE_CURVE('',#13398,#13396,#3247,.F.);
#17945=EDGE_CURVE('',#13399,#13400,#9462,.T.);
#17946=EDGE_CURVE('',#13397,#13399,#3248,.F.);
#17947=EDGE_CURVE('',#13400,#13398,#3249,.F.);
#17948=EDGE_CURVE('',#13401,#13402,#9463,.T.);
#17949=EDGE_CURVE('',#13399,#13401,#3250,.F.);
#17950=EDGE_CURVE('',#13402,#13400,#3251,.F.);
#17951=EDGE_CURVE('',#13403,#13404,#9464,.T.);
#17952=EDGE_CURVE('',#13401,#13403,#3252,.F.);
#17953=EDGE_CURVE('',#13404,#13402,#3253,.F.);
#17954=EDGE_CURVE('',#13405,#13406,#9465,.T.);
#17955=EDGE_CURVE('',#13403,#13405,#3254,.F.);
#17956=EDGE_CURVE('',#13406,#13404,#3255,.F.);
#17957=EDGE_CURVE('',#13407,#13408,#9466,.T.);
#17958=EDGE_CURVE('',#13405,#13407,#3256,.F.);
#17959=EDGE_CURVE('',#13408,#13406,#3257,.F.);
#17960=EDGE_CURVE('',#13409,#13410,#9467,.T.);
#17961=EDGE_CURVE('',#13407,#13409,#3258,.F.);
#17962=EDGE_CURVE('',#13410,#13408,#3259,.F.);
#17963=EDGE_CURVE('',#13411,#13412,#9468,.T.);
#17964=EDGE_CURVE('',#13409,#13411,#3260,.F.);
#17965=EDGE_CURVE('',#13412,#13410,#3261,.F.);
#17966=EDGE_CURVE('',#13413,#13414,#9469,.T.);
#17967=EDGE_CURVE('',#13411,#13413,#3262,.F.);
#17968=EDGE_CURVE('',#13414,#13412,#3263,.F.);
#17969=EDGE_CURVE('',#13415,#13416,#9470,.T.);
#17970=EDGE_CURVE('',#13413,#13415,#3264,.F.);
#17971=EDGE_CURVE('',#13416,#13414,#3265,.F.);
#17972=EDGE_CURVE('',#13417,#13418,#9471,.T.);
#17973=EDGE_CURVE('',#13415,#13417,#3266,.F.);
#17974=EDGE_CURVE('',#13418,#13416,#3267,.F.);
#17975=EDGE_CURVE('',#13419,#13420,#9472,.T.);
#17976=EDGE_CURVE('',#13417,#13419,#3268,.F.);
#17977=EDGE_CURVE('',#13420,#13418,#3269,.F.);
#17978=EDGE_CURVE('',#13421,#13422,#9473,.T.);
#17979=EDGE_CURVE('',#13419,#13421,#3270,.F.);
#17980=EDGE_CURVE('',#13422,#13420,#3271,.F.);
#17981=EDGE_CURVE('',#13423,#13424,#9474,.T.);
#17982=EDGE_CURVE('',#13421,#13423,#3272,.F.);
#17983=EDGE_CURVE('',#13424,#13422,#3273,.F.);
#17984=EDGE_CURVE('',#13425,#13426,#9475,.T.);
#17985=EDGE_CURVE('',#13423,#13425,#3274,.F.);
#17986=EDGE_CURVE('',#13426,#13424,#3275,.F.);
#17987=EDGE_CURVE('',#13427,#13428,#9476,.T.);
#17988=EDGE_CURVE('',#13425,#13427,#3276,.F.);
#17989=EDGE_CURVE('',#13428,#13426,#3277,.F.);
#17990=EDGE_CURVE('',#13429,#13430,#9477,.T.);
#17991=EDGE_CURVE('',#13427,#13429,#3278,.F.);
#17992=EDGE_CURVE('',#13430,#13428,#3279,.F.);
#17993=EDGE_CURVE('',#13431,#13432,#9478,.T.);
#17994=EDGE_CURVE('',#13429,#13431,#3280,.F.);
#17995=EDGE_CURVE('',#13432,#13430,#3281,.F.);
#17996=EDGE_CURVE('',#13433,#13434,#9479,.T.);
#17997=EDGE_CURVE('',#13433,#13435,#3282,.F.);
#17998=EDGE_CURVE('',#13434,#13435,#4117,.T.);
#17999=EDGE_CURVE('',#13436,#13435,#9480,.T.);
#18000=EDGE_CURVE('',#13437,#13436,#3283,.F.);
#18001=EDGE_CURVE('',#13435,#13437,#4118,.T.);
#18002=EDGE_CURVE('',#13438,#13439,#9481,.T.);
#18003=EDGE_CURVE('',#13436,#13438,#3284,.F.);
#18004=EDGE_CURVE('',#13435,#13439,#3285,.T.);
#18005=EDGE_CURVE('',#13440,#13441,#9482,.T.);
#18006=EDGE_CURVE('',#13438,#13440,#3286,.F.);
#18007=EDGE_CURVE('',#13439,#13441,#3287,.T.);
#18008=EDGE_CURVE('',#13442,#13443,#9483,.T.);
#18009=EDGE_CURVE('',#13440,#13442,#3288,.F.);
#18010=EDGE_CURVE('',#13441,#13443,#3289,.T.);
#18011=EDGE_CURVE('',#13444,#13445,#9484,.T.);
#18012=EDGE_CURVE('',#13442,#13444,#3290,.F.);
#18013=EDGE_CURVE('',#13443,#13445,#3291,.T.);
#18014=EDGE_CURVE('',#13446,#13447,#9485,.T.);
#18015=EDGE_CURVE('',#13444,#13446,#3292,.F.);
#18016=EDGE_CURVE('',#13445,#13447,#3293,.T.);
#18017=EDGE_CURVE('',#13448,#13449,#9486,.T.);
#18018=EDGE_CURVE('',#13446,#13448,#3294,.F.);
#18019=EDGE_CURVE('',#13447,#13449,#3295,.T.);
#18020=EDGE_CURVE('',#13450,#13451,#9487,.T.);
#18021=EDGE_CURVE('',#13448,#13450,#3296,.F.);
#18022=EDGE_CURVE('',#13449,#13451,#3297,.T.);
#18023=EDGE_CURVE('',#13452,#13453,#9488,.T.);
#18024=EDGE_CURVE('',#13450,#13452,#3298,.F.);
#18025=EDGE_CURVE('',#13451,#13453,#3299,.T.);
#18026=EDGE_CURVE('',#13454,#13455,#9489,.T.);
#18027=EDGE_CURVE('',#13452,#13454,#3300,.F.);
#18028=EDGE_CURVE('',#13453,#13455,#3301,.T.);
#18029=EDGE_CURVE('',#13456,#13457,#9490,.T.);
#18030=EDGE_CURVE('',#13454,#13456,#3302,.F.);
#18031=EDGE_CURVE('',#13455,#13457,#3303,.T.);
#18032=EDGE_CURVE('',#13458,#13459,#9491,.T.);
#18033=EDGE_CURVE('',#13456,#13458,#3304,.F.);
#18034=EDGE_CURVE('',#13457,#13459,#3305,.T.);
#18035=EDGE_CURVE('',#13460,#13461,#9492,.T.);
#18036=EDGE_CURVE('',#13458,#13460,#3306,.F.);
#18037=EDGE_CURVE('',#13459,#13461,#3307,.T.);
#18038=EDGE_CURVE('',#13462,#13463,#9493,.T.);
#18039=EDGE_CURVE('',#13460,#13462,#3308,.F.);
#18040=EDGE_CURVE('',#13461,#13463,#3309,.T.);
#18041=EDGE_CURVE('',#13464,#13465,#9494,.T.);
#18042=EDGE_CURVE('',#13462,#13464,#3310,.F.);
#18043=EDGE_CURVE('',#13463,#13465,#3311,.T.);
#18044=EDGE_CURVE('',#13466,#13467,#9495,.T.);
#18045=EDGE_CURVE('',#13464,#13466,#3312,.F.);
#18046=EDGE_CURVE('',#13465,#13467,#3313,.T.);
#18047=EDGE_CURVE('',#13468,#13469,#9496,.T.);
#18048=EDGE_CURVE('',#13466,#13468,#3314,.F.);
#18049=EDGE_CURVE('',#13467,#13469,#3315,.T.);
#18050=EDGE_CURVE('',#13470,#13471,#9497,.T.);
#18051=EDGE_CURVE('',#13468,#13470,#3316,.F.);
#18052=EDGE_CURVE('',#13469,#13471,#3317,.T.);
#18053=EDGE_CURVE('',#13472,#13473,#9498,.T.);
#18054=EDGE_CURVE('',#13470,#13472,#3318,.F.);
#18055=EDGE_CURVE('',#13471,#13473,#3319,.T.);
#18056=EDGE_CURVE('',#13474,#13475,#9499,.T.);
#18057=EDGE_CURVE('',#13472,#13474,#3320,.F.);
#18058=EDGE_CURVE('',#13473,#13475,#3321,.T.);
#18059=EDGE_CURVE('',#13476,#13477,#9500,.T.);
#18060=EDGE_CURVE('',#13474,#13476,#3322,.F.);
#18061=EDGE_CURVE('',#13475,#13477,#3323,.T.);
#18062=EDGE_CURVE('',#13478,#13479,#9501,.T.);
#18063=EDGE_CURVE('',#13476,#13478,#3324,.F.);
#18064=EDGE_CURVE('',#13477,#13479,#3325,.T.);
#18065=EDGE_CURVE('',#13480,#13481,#9502,.T.);
#18066=EDGE_CURVE('',#13478,#13480,#3326,.F.);
#18067=EDGE_CURVE('',#13479,#13481,#3327,.T.);
#18068=EDGE_CURVE('',#13482,#13483,#9503,.T.);
#18069=EDGE_CURVE('',#13480,#13482,#3328,.F.);
#18070=EDGE_CURVE('',#13481,#13483,#3329,.T.);
#18071=EDGE_CURVE('',#13484,#13485,#9504,.T.);
#18072=EDGE_CURVE('',#13482,#13484,#3330,.F.);
#18073=EDGE_CURVE('',#13483,#13485,#3331,.T.);
#18074=EDGE_CURVE('',#13486,#13487,#9505,.T.);
#18075=EDGE_CURVE('',#13484,#13486,#3332,.F.);
#18076=EDGE_CURVE('',#13485,#13487,#3333,.T.);
#18077=EDGE_CURVE('',#13488,#13489,#9506,.T.);
#18078=EDGE_CURVE('',#13486,#13488,#3334,.F.);
#18079=EDGE_CURVE('',#13487,#13489,#3335,.T.);
#18080=EDGE_CURVE('',#13490,#13491,#9507,.T.);
#18081=EDGE_CURVE('',#13488,#13490,#3336,.F.);
#18082=EDGE_CURVE('',#13489,#13491,#3337,.T.);
#18083=EDGE_CURVE('',#13492,#13493,#9508,.T.);
#18084=EDGE_CURVE('',#13490,#13492,#3338,.F.);
#18085=EDGE_CURVE('',#13491,#13493,#3339,.T.);
#18086=EDGE_CURVE('',#13494,#13495,#9509,.T.);
#18087=EDGE_CURVE('',#13492,#13494,#3340,.F.);
#18088=EDGE_CURVE('',#13493,#13495,#3341,.T.);
#18089=EDGE_CURVE('',#13495,#13496,#3342,.T.);
#18090=EDGE_CURVE('',#13494,#13496,#4119,.T.);
#18091=EDGE_CURVE('',#13437,#13434,#4120,.T.);
#18092=EDGE_CURVE('',#13437,#13497,#3343,.T.);
#18093=EDGE_CURVE('',#13497,#13498,#4121,.T.);
#18094=EDGE_CURVE('',#13498,#13433,#3344,.F.);
#18095=EDGE_CURVE('',#13498,#13432,#3345,.F.);
#18096=EDGE_CURVE('',#13431,#13497,#3346,.F.);
#18097=EDGE_CURVE('',#13499,#13500,#2478,.T.);
#18098=EDGE_CURVE('',#13500,#13501,#9510,.T.);
#18099=EDGE_CURVE('',#13501,#13502,#2479,.T.);
#18100=EDGE_CURVE('',#13499,#13502,#9511,.T.);
#18101=EDGE_CURVE('',#13503,#13504,#2480,.T.);
#18102=EDGE_CURVE('',#13504,#13505,#9512,.T.);
#18103=EDGE_CURVE('',#13505,#13506,#2481,.T.);
#18104=EDGE_CURVE('',#13503,#13506,#9513,.T.);
#18105=EDGE_CURVE('',#13507,#13508,#2482,.T.);
#18106=EDGE_CURVE('',#13508,#13509,#9514,.T.);
#18107=EDGE_CURVE('',#13509,#13510,#2483,.T.);
#18108=EDGE_CURVE('',#13507,#13510,#9515,.T.);
#18109=EDGE_CURVE('',#13511,#13512,#2484,.T.);
#18110=EDGE_CURVE('',#13512,#13513,#9516,.T.);
#18111=EDGE_CURVE('',#13513,#13514,#2485,.T.);
#18112=EDGE_CURVE('',#13511,#13514,#9517,.T.);
#18113=EDGE_CURVE('',#13515,#13516,#2486,.T.);
#18114=EDGE_CURVE('',#13516,#13517,#9518,.T.);
#18115=EDGE_CURVE('',#13517,#13518,#2487,.T.);
#18116=EDGE_CURVE('',#13515,#13518,#9519,.T.);
#18117=EDGE_CURVE('',#13519,#13520,#2488,.T.);
#18118=EDGE_CURVE('',#13520,#13521,#9520,.T.);
#18119=EDGE_CURVE('',#13521,#13522,#2489,.T.);
#18120=EDGE_CURVE('',#13519,#13522,#9521,.T.);
#18121=EDGE_CURVE('',#13523,#13524,#2490,.T.);
#18122=EDGE_CURVE('',#13524,#13525,#9522,.T.);
#18123=EDGE_CURVE('',#13525,#13526,#2491,.T.);
#18124=EDGE_CURVE('',#13523,#13526,#9523,.T.);
#18125=EDGE_CURVE('',#13527,#13528,#2492,.T.);
#18126=EDGE_CURVE('',#13528,#13529,#9524,.T.);
#18127=EDGE_CURVE('',#13529,#13530,#2493,.T.);
#18128=EDGE_CURVE('',#13527,#13530,#9525,.T.);
#18129=EDGE_CURVE('',#13531,#13532,#2494,.T.);
#18130=EDGE_CURVE('',#13532,#13533,#9526,.T.);
#18131=EDGE_CURVE('',#13533,#13534,#2495,.T.);
#18132=EDGE_CURVE('',#13531,#13534,#9527,.T.);
#18133=EDGE_CURVE('',#13535,#13536,#2496,.T.);
#18134=EDGE_CURVE('',#13536,#13537,#9528,.T.);
#18135=EDGE_CURVE('',#13537,#13538,#2497,.T.);
#18136=EDGE_CURVE('',#13535,#13538,#9529,.T.);
#18137=EDGE_CURVE('',#13539,#13540,#2498,.T.);
#18138=EDGE_CURVE('',#13540,#13541,#9530,.T.);
#18139=EDGE_CURVE('',#13541,#13542,#2499,.T.);
#18140=EDGE_CURVE('',#13539,#13542,#9531,.T.);
#18141=EDGE_CURVE('',#13543,#13544,#2500,.T.);
#18142=EDGE_CURVE('',#13544,#13545,#9532,.T.);
#18143=EDGE_CURVE('',#13545,#13546,#2501,.T.);
#18144=EDGE_CURVE('',#13543,#13546,#9533,.T.);
#18145=EDGE_CURVE('',#13547,#13548,#2502,.T.);
#18146=EDGE_CURVE('',#13548,#13549,#9534,.T.);
#18147=EDGE_CURVE('',#13549,#13550,#2503,.T.);
#18148=EDGE_CURVE('',#13547,#13550,#9535,.T.);
#18149=EDGE_CURVE('',#13551,#13552,#2504,.T.);
#18150=EDGE_CURVE('',#13552,#13553,#9536,.T.);
#18151=EDGE_CURVE('',#13553,#13554,#2505,.T.);
#18152=EDGE_CURVE('',#13551,#13554,#9537,.T.);
#18153=EDGE_CURVE('',#13555,#13556,#2506,.T.);
#18154=EDGE_CURVE('',#13556,#13557,#9538,.T.);
#18155=EDGE_CURVE('',#13557,#13558,#2507,.T.);
#18156=EDGE_CURVE('',#13555,#13558,#9539,.T.);
#18157=EDGE_CURVE('',#13559,#13560,#1195,.T.);
#18158=EDGE_CURVE('',#13561,#13559,#1196,.T.);
#18159=EDGE_CURVE('',#13562,#13561,#1197,.T.);
#18160=EDGE_CURVE('',#13563,#13562,#1198,.T.);
#18161=EDGE_CURVE('',#13564,#13563,#1199,.T.);
#18162=EDGE_CURVE('',#13565,#13564,#1200,.T.);
#18163=EDGE_CURVE('',#13560,#13565,#1201,.T.);
#18164=EDGE_CURVE('',#13560,#13566,#9540,.T.);
#18165=EDGE_CURVE('',#13566,#13566,#4122,.T.);
#18166=EDGE_CURVE('',#13567,#13567,#4123,.T.);
#18167=EDGE_CURVE('',#13567,#13568,#4124,.T.);
#18168=EDGE_CURVE('',#13568,#13568,#4125,.T.);
#18169=EDGE_CURVE('',#13569,#13570,#3347,.T.);
#18170=EDGE_CURVE('',#13571,#13569,#1202,.T.);
#18171=EDGE_CURVE('',#13572,#13571,#4126,.T.);
#18172=EDGE_CURVE('',#13573,#13572,#1203,.T.);
#18173=EDGE_CURVE('',#13574,#13573,#2508,.T.);
#18174=EDGE_CURVE('',#13575,#13574,#1204,.T.);
#18175=EDGE_CURVE('',#13576,#13575,#4127,.T.);
#18176=EDGE_CURVE('',#13577,#13576,#1205,.T.);
#18177=EDGE_CURVE('',#13578,#13577,#2509,.T.);
#18178=EDGE_CURVE('',#13579,#13578,#1206,.T.);
#18179=EDGE_CURVE('',#13580,#13579,#4128,.T.);
#18180=EDGE_CURVE('',#13581,#13580,#1207,.T.);
#18181=EDGE_CURVE('',#13582,#13581,#2510,.T.);
#18182=EDGE_CURVE('',#13583,#13582,#1208,.T.);
#18183=EDGE_CURVE('',#13584,#13583,#4129,.T.);
#18184=EDGE_CURVE('',#13585,#13584,#1209,.T.);
#18185=EDGE_CURVE('',#13586,#13585,#2511,.T.);
#18186=EDGE_CURVE('',#13587,#13586,#1210,.T.);
#18187=EDGE_CURVE('',#13588,#13587,#4130,.T.);
#18188=EDGE_CURVE('',#13589,#13588,#1211,.T.);
#18189=EDGE_CURVE('',#13590,#13589,#2512,.T.);
#18190=EDGE_CURVE('',#13591,#13590,#1212,.T.);
#18191=EDGE_CURVE('',#13592,#13591,#4131,.T.);
#18192=EDGE_CURVE('',#13593,#13592,#1213,.T.);
#18193=EDGE_CURVE('',#13594,#13593,#2513,.T.);
#18194=EDGE_CURVE('',#13595,#13594,#1214,.T.);
#18195=EDGE_CURVE('',#13596,#13595,#4132,.T.);
#18196=EDGE_CURVE('',#13597,#13596,#1215,.T.);
#18197=EDGE_CURVE('',#13598,#13597,#2514,.T.);
#18198=EDGE_CURVE('',#13599,#13598,#1216,.T.);
#18199=EDGE_CURVE('',#13600,#13599,#4133,.T.);
#18200=EDGE_CURVE('',#13601,#13600,#1217,.T.);
#18201=EDGE_CURVE('',#13602,#13601,#2515,.T.);
#18202=EDGE_CURVE('',#13603,#13602,#1218,.T.);
#18203=EDGE_CURVE('',#13604,#13603,#4134,.T.);
#18204=EDGE_CURVE('',#13605,#13604,#1219,.T.);
#18205=EDGE_CURVE('',#13606,#13605,#2516,.T.);
#18206=EDGE_CURVE('',#13607,#13606,#1220,.T.);
#18207=EDGE_CURVE('',#13608,#13607,#4135,.T.);
#18208=EDGE_CURVE('',#13609,#13608,#1221,.T.);
#18209=EDGE_CURVE('',#13610,#13609,#2517,.T.);
#18210=EDGE_CURVE('',#13611,#13610,#1222,.T.);
#18211=EDGE_CURVE('',#13612,#13611,#4136,.T.);
#18212=EDGE_CURVE('',#13613,#13612,#1223,.T.);
#18213=EDGE_CURVE('',#13614,#13613,#2518,.T.);
#18214=EDGE_CURVE('',#13615,#13614,#1224,.T.);
#18215=EDGE_CURVE('',#13616,#13615,#4137,.T.);
#18216=EDGE_CURVE('',#13617,#13616,#1225,.T.);
#18217=EDGE_CURVE('',#13618,#13617,#2519,.T.);
#18218=EDGE_CURVE('',#13619,#13618,#1226,.T.);
#18219=EDGE_CURVE('',#13620,#13619,#4138,.T.);
#18220=EDGE_CURVE('',#13621,#13620,#1227,.T.);
#18221=EDGE_CURVE('',#13622,#13621,#2520,.T.);
#18222=EDGE_CURVE('',#13623,#13622,#1228,.T.);
#18223=EDGE_CURVE('',#13624,#13623,#4139,.T.);
#18224=EDGE_CURVE('',#13625,#13624,#1229,.T.);
#18225=EDGE_CURVE('',#13626,#13625,#2521,.T.);
#18226=EDGE_CURVE('',#13627,#13626,#1230,.T.);
#18227=EDGE_CURVE('',#13628,#13627,#4140,.T.);
#18228=EDGE_CURVE('',#13629,#13628,#1231,.T.);
#18229=EDGE_CURVE('',#13630,#13629,#2522,.T.);
#18230=EDGE_CURVE('',#13631,#13630,#1232,.T.);
#18231=EDGE_CURVE('',#13632,#13631,#4141,.T.);
#18232=EDGE_CURVE('',#13633,#13632,#1233,.T.);
#18233=EDGE_CURVE('',#13634,#13633,#2523,.T.);
#18234=EDGE_CURVE('',#13635,#13634,#1234,.T.);
#18235=EDGE_CURVE('',#13636,#13635,#4142,.T.);
#18236=EDGE_CURVE('',#13637,#13636,#1235,.T.);
#18237=EDGE_CURVE('',#13638,#13637,#2524,.T.);
#18238=EDGE_CURVE('',#13639,#13638,#1236,.T.);
#18239=EDGE_CURVE('',#13640,#13639,#4143,.T.);
#18240=EDGE_CURVE('',#13641,#13640,#1237,.T.);
#18241=EDGE_CURVE('',#13642,#13641,#2525,.T.);
#18242=EDGE_CURVE('',#13643,#13642,#1238,.T.);
#18243=EDGE_CURVE('',#13644,#13643,#4144,.T.);
#18244=EDGE_CURVE('',#13645,#13644,#1239,.T.);
#18245=EDGE_CURVE('',#13646,#13645,#2526,.T.);
#18246=EDGE_CURVE('',#13647,#13646,#1240,.T.);
#18247=EDGE_CURVE('',#13648,#13647,#4145,.T.);
#18248=EDGE_CURVE('',#13649,#13648,#1241,.T.);
#18249=EDGE_CURVE('',#13650,#13649,#2527,.T.);
#18250=EDGE_CURVE('',#13651,#13650,#1242,.T.);
#18251=EDGE_CURVE('',#13652,#13651,#4146,.T.);
#18252=EDGE_CURVE('',#13653,#13652,#1243,.T.);
#18253=EDGE_CURVE('',#13654,#13653,#2528,.T.);
#18254=EDGE_CURVE('',#13655,#13654,#1244,.T.);
#18255=EDGE_CURVE('',#13656,#13655,#4147,.T.);
#18256=EDGE_CURVE('',#13657,#13656,#1245,.T.);
#18257=EDGE_CURVE('',#13658,#13657,#2529,.T.);
#18258=EDGE_CURVE('',#13659,#13658,#1246,.T.);
#18259=EDGE_CURVE('',#13660,#13659,#4148,.T.);
#18260=EDGE_CURVE('',#13661,#13660,#1247,.T.);
#18261=EDGE_CURVE('',#13662,#13661,#2530,.T.);
#18262=EDGE_CURVE('',#13663,#13662,#1248,.T.);
#18263=EDGE_CURVE('',#13664,#13663,#4149,.T.);
#18264=EDGE_CURVE('',#13665,#13664,#1249,.T.);
#18265=EDGE_CURVE('',#13666,#13665,#2531,.T.);
#18266=EDGE_CURVE('',#13667,#13666,#1250,.T.);
#18267=EDGE_CURVE('',#13668,#13667,#4150,.T.);
#18268=EDGE_CURVE('',#13669,#13668,#1251,.T.);
#18269=EDGE_CURVE('',#13670,#13669,#2532,.T.);
#18270=EDGE_CURVE('',#13671,#13670,#1252,.T.);
#18271=EDGE_CURVE('',#13672,#13671,#4151,.T.);
#18272=EDGE_CURVE('',#13673,#13672,#1253,.T.);
#18273=EDGE_CURVE('',#13674,#13673,#2533,.T.);
#18274=EDGE_CURVE('',#13675,#13674,#1254,.T.);
#18275=EDGE_CURVE('',#13676,#13675,#4152,.T.);
#18276=EDGE_CURVE('',#13677,#13676,#1255,.T.);
#18277=EDGE_CURVE('',#13678,#13677,#2534,.T.);
#18278=EDGE_CURVE('',#13679,#13678,#1256,.T.);
#18279=EDGE_CURVE('',#13680,#13679,#4153,.T.);
#18280=EDGE_CURVE('',#13681,#13680,#1257,.T.);
#18281=EDGE_CURVE('',#13682,#13681,#2535,.T.);
#18282=EDGE_CURVE('',#13683,#13682,#1258,.T.);
#18283=EDGE_CURVE('',#13684,#13683,#4154,.T.);
#18284=EDGE_CURVE('',#13685,#13684,#1259,.T.);
#18285=EDGE_CURVE('',#13686,#13685,#2536,.T.);
#18286=EDGE_CURVE('',#13687,#13686,#1260,.T.);
#18287=EDGE_CURVE('',#13688,#13687,#4155,.T.);
#18288=EDGE_CURVE('',#13689,#13688,#1261,.T.);
#18289=EDGE_CURVE('',#13690,#13689,#2537,.T.);
#18290=EDGE_CURVE('',#13691,#13690,#1262,.T.);
#18291=EDGE_CURVE('',#13692,#13691,#4156,.T.);
#18292=EDGE_CURVE('',#13693,#13692,#1263,.T.);
#18293=EDGE_CURVE('',#13694,#13693,#2538,.T.);
#18294=EDGE_CURVE('',#13695,#13694,#1264,.T.);
#18295=EDGE_CURVE('',#13696,#13695,#4157,.T.);
#18296=EDGE_CURVE('',#13697,#13696,#1265,.T.);
#18297=EDGE_CURVE('',#13698,#13697,#2539,.T.);
#18298=EDGE_CURVE('',#13699,#13698,#1266,.T.);
#18299=EDGE_CURVE('',#13700,#13699,#4158,.T.);
#18300=EDGE_CURVE('',#13701,#13700,#1267,.T.);
#18301=EDGE_CURVE('',#13702,#13701,#2540,.T.);
#18302=EDGE_CURVE('',#13703,#13702,#1268,.T.);
#18303=EDGE_CURVE('',#13704,#13703,#4159,.T.);
#18304=EDGE_CURVE('',#13705,#13704,#1269,.T.);
#18305=EDGE_CURVE('',#13706,#13705,#2541,.T.);
#18306=EDGE_CURVE('',#13707,#13706,#1270,.T.);
#18307=EDGE_CURVE('',#13708,#13707,#4160,.T.);
#18308=EDGE_CURVE('',#13709,#13708,#1271,.T.);
#18309=EDGE_CURVE('',#13710,#13709,#2542,.T.);
#18310=EDGE_CURVE('',#13711,#13710,#1272,.T.);
#18311=EDGE_CURVE('',#13712,#13711,#4161,.T.);
#18312=EDGE_CURVE('',#13713,#13712,#1273,.T.);
#18313=EDGE_CURVE('',#13714,#13713,#2543,.T.);
#18314=EDGE_CURVE('',#13715,#13714,#1274,.T.);
#18315=EDGE_CURVE('',#13716,#13715,#4162,.T.);
#18316=EDGE_CURVE('',#13717,#13716,#1275,.T.);
#18317=EDGE_CURVE('',#13718,#13717,#2544,.T.);
#18318=EDGE_CURVE('',#13719,#13718,#1276,.T.);
#18319=EDGE_CURVE('',#13720,#13719,#4163,.T.);
#18320=EDGE_CURVE('',#13721,#13720,#1277,.T.);
#18321=EDGE_CURVE('',#13722,#13721,#2545,.T.);
#18322=EDGE_CURVE('',#13723,#13722,#1278,.T.);
#18323=EDGE_CURVE('',#13724,#13723,#4164,.T.);
#18324=EDGE_CURVE('',#13725,#13724,#1279,.T.);
#18325=EDGE_CURVE('',#13726,#13725,#2546,.T.);
#18326=EDGE_CURVE('',#13727,#13726,#1280,.T.);
#18327=EDGE_CURVE('',#13728,#13727,#4165,.T.);
#18328=EDGE_CURVE('',#13729,#13728,#1281,.T.);
#18329=EDGE_CURVE('',#13730,#13729,#2547,.T.);
#18330=EDGE_CURVE('',#13731,#13730,#1282,.T.);
#18331=EDGE_CURVE('',#13732,#13731,#4166,.T.);
#18332=EDGE_CURVE('',#13733,#13732,#1283,.T.);
#18333=EDGE_CURVE('',#13734,#13733,#2548,.T.);
#18334=EDGE_CURVE('',#13735,#13734,#1284,.T.);
#18335=EDGE_CURVE('',#13736,#13735,#4167,.T.);
#18336=EDGE_CURVE('',#13737,#13736,#1285,.T.);
#18337=EDGE_CURVE('',#13738,#13737,#2549,.T.);
#18338=EDGE_CURVE('',#13739,#13738,#1286,.T.);
#18339=EDGE_CURVE('',#13740,#13739,#4168,.T.);
#18340=EDGE_CURVE('',#13741,#13740,#1287,.T.);
#18341=EDGE_CURVE('',#13742,#13741,#2550,.T.);
#18342=EDGE_CURVE('',#13743,#13742,#1288,.T.);
#18343=EDGE_CURVE('',#13744,#13743,#4169,.T.);
#18344=EDGE_CURVE('',#13745,#13744,#1289,.T.);
#18345=EDGE_CURVE('',#13746,#13745,#2551,.T.);
#18346=EDGE_CURVE('',#13747,#13746,#1290,.T.);
#18347=EDGE_CURVE('',#13748,#13747,#4170,.T.);
#18348=EDGE_CURVE('',#13749,#13748,#1291,.T.);
#18349=EDGE_CURVE('',#13750,#13749,#2552,.T.);
#18350=EDGE_CURVE('',#13751,#13750,#1292,.T.);
#18351=EDGE_CURVE('',#13752,#13751,#4171,.T.);
#18352=EDGE_CURVE('',#13558,#13752,#1293,.T.);
#18353=EDGE_CURVE('',#13753,#13557,#1294,.T.);
#18354=EDGE_CURVE('',#13754,#13753,#4172,.T.);
#18355=EDGE_CURVE('',#13554,#13754,#1295,.T.);
#18356=EDGE_CURVE('',#13755,#13553,#1296,.T.);
#18357=EDGE_CURVE('',#13756,#13755,#4173,.T.);
#18358=EDGE_CURVE('',#13550,#13756,#1297,.T.);
#18359=EDGE_CURVE('',#13757,#13549,#1298,.T.);
#18360=EDGE_CURVE('',#13758,#13757,#4174,.T.);
#18361=EDGE_CURVE('',#13546,#13758,#1299,.T.);
#18362=EDGE_CURVE('',#13759,#13545,#1300,.T.);
#18363=EDGE_CURVE('',#13760,#13759,#4175,.T.);
#18364=EDGE_CURVE('',#13542,#13760,#1301,.T.);
#18365=EDGE_CURVE('',#13761,#13541,#1302,.T.);
#18366=EDGE_CURVE('',#13762,#13761,#4176,.T.);
#18367=EDGE_CURVE('',#13538,#13762,#1303,.T.);
#18368=EDGE_CURVE('',#13763,#13537,#1304,.T.);
#18369=EDGE_CURVE('',#13764,#13763,#4177,.T.);
#18370=EDGE_CURVE('',#13534,#13764,#1305,.T.);
#18371=EDGE_CURVE('',#13765,#13533,#1306,.T.);
#18372=EDGE_CURVE('',#13766,#13765,#4178,.T.);
#18373=EDGE_CURVE('',#13530,#13766,#1307,.T.);
#18374=EDGE_CURVE('',#13767,#13529,#1308,.T.);
#18375=EDGE_CURVE('',#13768,#13767,#4179,.T.);
#18376=EDGE_CURVE('',#13526,#13768,#1309,.T.);
#18377=EDGE_CURVE('',#13769,#13525,#1310,.T.);
#18378=EDGE_CURVE('',#13770,#13769,#4180,.T.);
#18379=EDGE_CURVE('',#13502,#13770,#1311,.T.);
#18380=EDGE_CURVE('',#13771,#13501,#1312,.T.);
#18381=EDGE_CURVE('',#13772,#13771,#4181,.T.);
#18382=EDGE_CURVE('',#13506,#13772,#1313,.T.);
#18383=EDGE_CURVE('',#13773,#13505,#1314,.T.);
#18384=EDGE_CURVE('',#13774,#13773,#4182,.T.);
#18385=EDGE_CURVE('',#13510,#13774,#1315,.T.);
#18386=EDGE_CURVE('',#13775,#13509,#1316,.T.);
#18387=EDGE_CURVE('',#13776,#13775,#4183,.T.);
#18388=EDGE_CURVE('',#13514,#13776,#1317,.T.);
#18389=EDGE_CURVE('',#13777,#13513,#1318,.T.);
#18390=EDGE_CURVE('',#13778,#13777,#4184,.T.);
#18391=EDGE_CURVE('',#13518,#13778,#1319,.T.);
#18392=EDGE_CURVE('',#13779,#13517,#1320,.T.);
#18393=EDGE_CURVE('',#13780,#13779,#4185,.T.);
#18394=EDGE_CURVE('',#13522,#13780,#1321,.T.);
#18395=EDGE_CURVE('',#13781,#13521,#1322,.T.);
#18396=EDGE_CURVE('',#13782,#13781,#4186,.T.);
#18397=EDGE_CURVE('',#13783,#13782,#1323,.T.);
#18398=EDGE_CURVE('',#13784,#13783,#2553,.T.);
#18399=EDGE_CURVE('',#13785,#13784,#1324,.T.);
#18400=EDGE_CURVE('',#13786,#13785,#4187,.T.);
#18401=EDGE_CURVE('',#13787,#13786,#1325,.T.);
#18402=EDGE_CURVE('',#13788,#13787,#2554,.T.);
#18403=EDGE_CURVE('',#13789,#13788,#1326,.T.);
#18404=EDGE_CURVE('',#13790,#13789,#4188,.T.);
#18405=EDGE_CURVE('',#13791,#13790,#1327,.T.);
#18406=EDGE_CURVE('',#13792,#13791,#2555,.T.);
#18407=EDGE_CURVE('',#13793,#13792,#1328,.T.);
#18408=EDGE_CURVE('',#13794,#13793,#4189,.T.);
#18409=EDGE_CURVE('',#13795,#13794,#1329,.T.);
#18410=EDGE_CURVE('',#13796,#13795,#2556,.T.);
#18411=EDGE_CURVE('',#13797,#13796,#1330,.T.);
#18412=EDGE_CURVE('',#13798,#13797,#4190,.T.);
#18413=EDGE_CURVE('',#13799,#13798,#1331,.T.);
#18414=EDGE_CURVE('',#13800,#13799,#2557,.T.);
#18415=EDGE_CURVE('',#13801,#13800,#1332,.T.);
#18416=EDGE_CURVE('',#13802,#13801,#4191,.T.);
#18417=EDGE_CURVE('',#13803,#13802,#1333,.T.);
#18418=EDGE_CURVE('',#13804,#13803,#2558,.T.);
#18419=EDGE_CURVE('',#13805,#13804,#1334,.T.);
#18420=EDGE_CURVE('',#13806,#13805,#4192,.T.);
#18421=EDGE_CURVE('',#13807,#13806,#1335,.T.);
#18422=EDGE_CURVE('',#13808,#13807,#2559,.T.);
#18423=EDGE_CURVE('',#13809,#13808,#1336,.T.);
#18424=EDGE_CURVE('',#13810,#13809,#4193,.T.);
#18425=EDGE_CURVE('',#13811,#13810,#1337,.T.);
#18426=EDGE_CURVE('',#13812,#13811,#2560,.T.);
#18427=EDGE_CURVE('',#13813,#13812,#1338,.T.);
#18428=EDGE_CURVE('',#13814,#13813,#4194,.T.);
#18429=EDGE_CURVE('',#13815,#13814,#1339,.T.);
#18430=EDGE_CURVE('',#13816,#13815,#2561,.T.);
#18431=EDGE_CURVE('',#13817,#13816,#1340,.T.);
#18432=EDGE_CURVE('',#13818,#13817,#4195,.T.);
#18433=EDGE_CURVE('',#13819,#13818,#1341,.T.);
#18434=EDGE_CURVE('',#13820,#13819,#2562,.T.);
#18435=EDGE_CURVE('',#13821,#13820,#1342,.T.);
#18436=EDGE_CURVE('',#13822,#13821,#4196,.T.);
#18437=EDGE_CURVE('',#13823,#13822,#1343,.T.);
#18438=EDGE_CURVE('',#13824,#13823,#2563,.T.);
#18439=EDGE_CURVE('',#13825,#13824,#1344,.T.);
#18440=EDGE_CURVE('',#13826,#13825,#4197,.T.);
#18441=EDGE_CURVE('',#13827,#13826,#1345,.T.);
#18442=EDGE_CURVE('',#13828,#13827,#2564,.T.);
#18443=EDGE_CURVE('',#13829,#13828,#1346,.T.);
#18444=EDGE_CURVE('',#13830,#13829,#4198,.T.);
#18445=EDGE_CURVE('',#13831,#13830,#1347,.T.);
#18446=EDGE_CURVE('',#13832,#13831,#2565,.T.);
#18447=EDGE_CURVE('',#13833,#13832,#1348,.T.);
#18448=EDGE_CURVE('',#13834,#13833,#4199,.T.);
#18449=EDGE_CURVE('',#13835,#13834,#1349,.T.);
#18450=EDGE_CURVE('',#13836,#13835,#2566,.T.);
#18451=EDGE_CURVE('',#13837,#13836,#1350,.T.);
#18452=EDGE_CURVE('',#13838,#13837,#4200,.T.);
#18453=EDGE_CURVE('',#13839,#13838,#1351,.T.);
#18454=EDGE_CURVE('',#13840,#13839,#2567,.T.);
#18455=EDGE_CURVE('',#13841,#13840,#1352,.T.);
#18456=EDGE_CURVE('',#13842,#13841,#4201,.T.);
#18457=EDGE_CURVE('',#13843,#13842,#1353,.T.);
#18458=EDGE_CURVE('',#13844,#13843,#2568,.T.);
#18459=EDGE_CURVE('',#13845,#13844,#1354,.T.);
#18460=EDGE_CURVE('',#13846,#13845,#4202,.T.);
#18461=EDGE_CURVE('',#13847,#13846,#1355,.T.);
#18462=EDGE_CURVE('',#13848,#13847,#2569,.T.);
#18463=EDGE_CURVE('',#13849,#13848,#1356,.T.);
#18464=EDGE_CURVE('',#13850,#13849,#4203,.T.);
#18465=EDGE_CURVE('',#13851,#13850,#1357,.T.);
#18466=EDGE_CURVE('',#13852,#13851,#2570,.T.);
#18467=EDGE_CURVE('',#13853,#13852,#1358,.T.);
#18468=EDGE_CURVE('',#13854,#13853,#4204,.T.);
#18469=EDGE_CURVE('',#13855,#13854,#1359,.T.);
#18470=EDGE_CURVE('',#13856,#13855,#2571,.T.);
#18471=EDGE_CURVE('',#13857,#13856,#1360,.T.);
#18472=EDGE_CURVE('',#13858,#13857,#4205,.T.);
#18473=EDGE_CURVE('',#13859,#13858,#1361,.T.);
#18474=EDGE_CURVE('',#13570,#13859,#3348,.T.);
#18475=EDGE_CURVE('',#13570,#13567,#9541,.T.);
#18476=EDGE_CURVE('',#13860,#13861,#3349,.T.);
#18477=EDGE_CURVE('',#13862,#13860,#1362,.T.);
#18478=EDGE_CURVE('',#13862,#13863,#4206,.T.);
#18479=EDGE_CURVE('',#13864,#13863,#1363,.T.);
#18480=EDGE_CURVE('',#13865,#13864,#2572,.T.);
#18481=EDGE_CURVE('',#13866,#13865,#1364,.T.);
#18482=EDGE_CURVE('',#13866,#13867,#4207,.T.);
#18483=EDGE_CURVE('',#13868,#13867,#1365,.T.);
#18484=EDGE_CURVE('',#13869,#13868,#2573,.T.);
#18485=EDGE_CURVE('',#13870,#13869,#1366,.T.);
#18486=EDGE_CURVE('',#13870,#13871,#4208,.T.);
#18487=EDGE_CURVE('',#13872,#13871,#1367,.T.);
#18488=EDGE_CURVE('',#13873,#13872,#2574,.T.);
#18489=EDGE_CURVE('',#13874,#13873,#1368,.T.);
#18490=EDGE_CURVE('',#13874,#13875,#4209,.T.);
#18491=EDGE_CURVE('',#13876,#13875,#1369,.T.);
#18492=EDGE_CURVE('',#13877,#13876,#2575,.T.);
#18493=EDGE_CURVE('',#13878,#13877,#1370,.T.);
#18494=EDGE_CURVE('',#13878,#13879,#4210,.T.);
#18495=EDGE_CURVE('',#13880,#13879,#1371,.T.);
#18496=EDGE_CURVE('',#13881,#13880,#2576,.T.);
#18497=EDGE_CURVE('',#13882,#13881,#1372,.T.);
#18498=EDGE_CURVE('',#13882,#13883,#4211,.T.);
#18499=EDGE_CURVE('',#13884,#13883,#1373,.T.);
#18500=EDGE_CURVE('',#13885,#13884,#2577,.T.);
#18501=EDGE_CURVE('',#13886,#13885,#1374,.T.);
#18502=EDGE_CURVE('',#13886,#13887,#4212,.T.);
#18503=EDGE_CURVE('',#13888,#13887,#1375,.T.);
#18504=EDGE_CURVE('',#13889,#13888,#2578,.T.);
#18505=EDGE_CURVE('',#13890,#13889,#1376,.T.);
#18506=EDGE_CURVE('',#13890,#13891,#4213,.T.);
#18507=EDGE_CURVE('',#13892,#13891,#1377,.T.);
#18508=EDGE_CURVE('',#13893,#13892,#2579,.T.);
#18509=EDGE_CURVE('',#13894,#13893,#1378,.T.);
#18510=EDGE_CURVE('',#13894,#13895,#4214,.T.);
#18511=EDGE_CURVE('',#13896,#13895,#1379,.T.);
#18512=EDGE_CURVE('',#13897,#13896,#2580,.T.);
#18513=EDGE_CURVE('',#13898,#13897,#1380,.T.);
#18514=EDGE_CURVE('',#13898,#13899,#4215,.T.);
#18515=EDGE_CURVE('',#13900,#13899,#1381,.T.);
#18516=EDGE_CURVE('',#13901,#13900,#2581,.T.);
#18517=EDGE_CURVE('',#13902,#13901,#1382,.T.);
#18518=EDGE_CURVE('',#13902,#13903,#4216,.T.);
#18519=EDGE_CURVE('',#13904,#13903,#1383,.T.);
#18520=EDGE_CURVE('',#13905,#13904,#2582,.T.);
#18521=EDGE_CURVE('',#13906,#13905,#1384,.T.);
#18522=EDGE_CURVE('',#13906,#13907,#4217,.T.);
#18523=EDGE_CURVE('',#13908,#13907,#1385,.T.);
#18524=EDGE_CURVE('',#13909,#13908,#2583,.T.);
#18525=EDGE_CURVE('',#13910,#13909,#1386,.T.);
#18526=EDGE_CURVE('',#13910,#13911,#4218,.T.);
#18527=EDGE_CURVE('',#13912,#13911,#1387,.T.);
#18528=EDGE_CURVE('',#13913,#13912,#2584,.T.);
#18529=EDGE_CURVE('',#13914,#13913,#1388,.T.);
#18530=EDGE_CURVE('',#13914,#13915,#4219,.T.);
#18531=EDGE_CURVE('',#13916,#13915,#1389,.T.);
#18532=EDGE_CURVE('',#13917,#13916,#2585,.T.);
#18533=EDGE_CURVE('',#13918,#13917,#1390,.T.);
#18534=EDGE_CURVE('',#13918,#13919,#4220,.T.);
#18535=EDGE_CURVE('',#13920,#13919,#1391,.T.);
#18536=EDGE_CURVE('',#13921,#13920,#2586,.T.);
#18537=EDGE_CURVE('',#13922,#13921,#1392,.T.);
#18538=EDGE_CURVE('',#13922,#13923,#4221,.T.);
#18539=EDGE_CURVE('',#13924,#13923,#1393,.T.);
#18540=EDGE_CURVE('',#13925,#13924,#2587,.T.);
#18541=EDGE_CURVE('',#13926,#13925,#1394,.T.);
#18542=EDGE_CURVE('',#13926,#13927,#4222,.T.);
#18543=EDGE_CURVE('',#13928,#13927,#1395,.T.);
#18544=EDGE_CURVE('',#13929,#13928,#2588,.T.);
#18545=EDGE_CURVE('',#13930,#13929,#1396,.T.);
#18546=EDGE_CURVE('',#13930,#13931,#4223,.T.);
#18547=EDGE_CURVE('',#13932,#13931,#1397,.T.);
#18548=EDGE_CURVE('',#13933,#13932,#2589,.T.);
#18549=EDGE_CURVE('',#13934,#13933,#1398,.T.);
#18550=EDGE_CURVE('',#13934,#13935,#4224,.T.);
#18551=EDGE_CURVE('',#13936,#13935,#1399,.T.);
#18552=EDGE_CURVE('',#13937,#13936,#2590,.T.);
#18553=EDGE_CURVE('',#13938,#13937,#1400,.T.);
#18554=EDGE_CURVE('',#13938,#13939,#4225,.T.);
#18555=EDGE_CURVE('',#13940,#13939,#1401,.T.);
#18556=EDGE_CURVE('',#13941,#13940,#2591,.T.);
#18557=EDGE_CURVE('',#13942,#13941,#1402,.T.);
#18558=EDGE_CURVE('',#13942,#13943,#4226,.T.);
#18559=EDGE_CURVE('',#13944,#13943,#1403,.T.);
#18560=EDGE_CURVE('',#13945,#13944,#2592,.T.);
#18561=EDGE_CURVE('',#13946,#13945,#1404,.T.);
#18562=EDGE_CURVE('',#13946,#13947,#4227,.T.);
#18563=EDGE_CURVE('',#13948,#13947,#1405,.T.);
#18564=EDGE_CURVE('',#13949,#13948,#2593,.T.);
#18565=EDGE_CURVE('',#13950,#13949,#1406,.T.);
#18566=EDGE_CURVE('',#13950,#13951,#4228,.T.);
#18567=EDGE_CURVE('',#13952,#13951,#1407,.T.);
#18568=EDGE_CURVE('',#13953,#13952,#2594,.T.);
#18569=EDGE_CURVE('',#13954,#13953,#1408,.T.);
#18570=EDGE_CURVE('',#13954,#13955,#4229,.T.);
#18571=EDGE_CURVE('',#13956,#13955,#1409,.T.);
#18572=EDGE_CURVE('',#13957,#13956,#2595,.T.);
#18573=EDGE_CURVE('',#13958,#13957,#1410,.T.);
#18574=EDGE_CURVE('',#13958,#13959,#4230,.T.);
#18575=EDGE_CURVE('',#13960,#13959,#1411,.T.);
#18576=EDGE_CURVE('',#13961,#13960,#2596,.T.);
#18577=EDGE_CURVE('',#13962,#13961,#1412,.T.);
#18578=EDGE_CURVE('',#13962,#13963,#4231,.T.);
#18579=EDGE_CURVE('',#13964,#13963,#1413,.T.);
#18580=EDGE_CURVE('',#13965,#13964,#2597,.T.);
#18581=EDGE_CURVE('',#13966,#13965,#1414,.T.);
#18582=EDGE_CURVE('',#13966,#13967,#4232,.T.);
#18583=EDGE_CURVE('',#13968,#13967,#1415,.T.);
#18584=EDGE_CURVE('',#13969,#13968,#2598,.T.);
#18585=EDGE_CURVE('',#13970,#13969,#1416,.T.);
#18586=EDGE_CURVE('',#13970,#13971,#4233,.T.);
#18587=EDGE_CURVE('',#13972,#13971,#1417,.T.);
#18588=EDGE_CURVE('',#13973,#13972,#2599,.T.);
#18589=EDGE_CURVE('',#13974,#13973,#1418,.T.);
#18590=EDGE_CURVE('',#13974,#13975,#4234,.T.);
#18591=EDGE_CURVE('',#13976,#13975,#1419,.T.);
#18592=EDGE_CURVE('',#13977,#13976,#2600,.T.);
#18593=EDGE_CURVE('',#13978,#13977,#1420,.T.);
#18594=EDGE_CURVE('',#13978,#13979,#4235,.T.);
#18595=EDGE_CURVE('',#13980,#13979,#1421,.T.);
#18596=EDGE_CURVE('',#13981,#13980,#2601,.T.);
#18597=EDGE_CURVE('',#13982,#13981,#1422,.T.);
#18598=EDGE_CURVE('',#13982,#13983,#4236,.T.);
#18599=EDGE_CURVE('',#13984,#13983,#1423,.T.);
#18600=EDGE_CURVE('',#13985,#13984,#2602,.T.);
#18601=EDGE_CURVE('',#13986,#13985,#1424,.T.);
#18602=EDGE_CURVE('',#13986,#13987,#4237,.T.);
#18603=EDGE_CURVE('',#13988,#13987,#1425,.T.);
#18604=EDGE_CURVE('',#13989,#13988,#2603,.T.);
#18605=EDGE_CURVE('',#13990,#13989,#1426,.T.);
#18606=EDGE_CURVE('',#13990,#13991,#4238,.T.);
#18607=EDGE_CURVE('',#13992,#13991,#1427,.T.);
#18608=EDGE_CURVE('',#13993,#13992,#2604,.T.);
#18609=EDGE_CURVE('',#13994,#13993,#1428,.T.);
#18610=EDGE_CURVE('',#13994,#13995,#4239,.T.);
#18611=EDGE_CURVE('',#13996,#13995,#1429,.T.);
#18612=EDGE_CURVE('',#13997,#13996,#2605,.T.);
#18613=EDGE_CURVE('',#13998,#13997,#1430,.T.);
#18614=EDGE_CURVE('',#13998,#13999,#4240,.T.);
#18615=EDGE_CURVE('',#14000,#13999,#1431,.T.);
#18616=EDGE_CURVE('',#14001,#14000,#2606,.T.);
#18617=EDGE_CURVE('',#14002,#14001,#1432,.T.);
#18618=EDGE_CURVE('',#14002,#14003,#4241,.T.);
#18619=EDGE_CURVE('',#14004,#14003,#1433,.T.);
#18620=EDGE_CURVE('',#14005,#14004,#2607,.T.);
#18621=EDGE_CURVE('',#14006,#14005,#1434,.T.);
#18622=EDGE_CURVE('',#14006,#14007,#4242,.T.);
#18623=EDGE_CURVE('',#14008,#14007,#1435,.T.);
#18624=EDGE_CURVE('',#14009,#14008,#2608,.T.);
#18625=EDGE_CURVE('',#14010,#14009,#1436,.T.);
#18626=EDGE_CURVE('',#14010,#14011,#4243,.T.);
#18627=EDGE_CURVE('',#14012,#14011,#1437,.T.);
#18628=EDGE_CURVE('',#14013,#14012,#2609,.T.);
#18629=EDGE_CURVE('',#14014,#14013,#1438,.T.);
#18630=EDGE_CURVE('',#14014,#14015,#4244,.T.);
#18631=EDGE_CURVE('',#14016,#14015,#1439,.T.);
#18632=EDGE_CURVE('',#14017,#14016,#2610,.T.);
#18633=EDGE_CURVE('',#14018,#14017,#1440,.T.);
#18634=EDGE_CURVE('',#14018,#14019,#4245,.T.);
#18635=EDGE_CURVE('',#14020,#14019,#1441,.T.);
#18636=EDGE_CURVE('',#14021,#14020,#2611,.T.);
#18637=EDGE_CURVE('',#14022,#14021,#1442,.T.);
#18638=EDGE_CURVE('',#14022,#14023,#4246,.T.);
#18639=EDGE_CURVE('',#14024,#14023,#1443,.T.);
#18640=EDGE_CURVE('',#14025,#14024,#2612,.T.);
#18641=EDGE_CURVE('',#14026,#14025,#1444,.T.);
#18642=EDGE_CURVE('',#14026,#14027,#4247,.T.);
#18643=EDGE_CURVE('',#14028,#14027,#1445,.T.);
#18644=EDGE_CURVE('',#14029,#14028,#2613,.T.);
#18645=EDGE_CURVE('',#14030,#14029,#1446,.T.);
#18646=EDGE_CURVE('',#14030,#14031,#4248,.T.);
#18647=EDGE_CURVE('',#14032,#14031,#1447,.T.);
#18648=EDGE_CURVE('',#14033,#14032,#2614,.T.);
#18649=EDGE_CURVE('',#14034,#14033,#1448,.T.);
#18650=EDGE_CURVE('',#14034,#14035,#4249,.T.);
#18651=EDGE_CURVE('',#14036,#14035,#1449,.T.);
#18652=EDGE_CURVE('',#14037,#14036,#2615,.T.);
#18653=EDGE_CURVE('',#14038,#14037,#1450,.T.);
#18654=EDGE_CURVE('',#14038,#14039,#4250,.T.);
#18655=EDGE_CURVE('',#14040,#14039,#1451,.T.);
#18656=EDGE_CURVE('',#14041,#14040,#2616,.T.);
#18657=EDGE_CURVE('',#14042,#14041,#1452,.T.);
#18658=EDGE_CURVE('',#14042,#14043,#4251,.T.);
#18659=EDGE_CURVE('',#14044,#14043,#1453,.T.);
#18660=EDGE_CURVE('',#14045,#14044,#2617,.T.);
#18661=EDGE_CURVE('',#14046,#14045,#1454,.T.);
#18662=EDGE_CURVE('',#14046,#14047,#4252,.T.);
#18663=EDGE_CURVE('',#14048,#14047,#1455,.T.);
#18664=EDGE_CURVE('',#14049,#14048,#2618,.T.);
#18665=EDGE_CURVE('',#14050,#14049,#1456,.T.);
#18666=EDGE_CURVE('',#14050,#14051,#4253,.T.);
#18667=EDGE_CURVE('',#14052,#14051,#1457,.T.);
#18668=EDGE_CURVE('',#14053,#14052,#2619,.T.);
#18669=EDGE_CURVE('',#14054,#14053,#1458,.T.);
#18670=EDGE_CURVE('',#14054,#14055,#4254,.T.);
#18671=EDGE_CURVE('',#14056,#14055,#1459,.T.);
#18672=EDGE_CURVE('',#14057,#14056,#2620,.T.);
#18673=EDGE_CURVE('',#14058,#14057,#1460,.T.);
#18674=EDGE_CURVE('',#14058,#14059,#4255,.T.);
#18675=EDGE_CURVE('',#14060,#14059,#1461,.T.);
#18676=EDGE_CURVE('',#14061,#14060,#2621,.T.);
#18677=EDGE_CURVE('',#14062,#14061,#1462,.T.);
#18678=EDGE_CURVE('',#14062,#14063,#4256,.T.);
#18679=EDGE_CURVE('',#14064,#14063,#1463,.T.);
#18680=EDGE_CURVE('',#14065,#14064,#2622,.T.);
#18681=EDGE_CURVE('',#14066,#14065,#1464,.T.);
#18682=EDGE_CURVE('',#14066,#14067,#4257,.T.);
#18683=EDGE_CURVE('',#14068,#14067,#1465,.T.);
#18684=EDGE_CURVE('',#14069,#14068,#2623,.T.);
#18685=EDGE_CURVE('',#14070,#14069,#1466,.T.);
#18686=EDGE_CURVE('',#14070,#14071,#4258,.T.);
#18687=EDGE_CURVE('',#14072,#14071,#1467,.T.);
#18688=EDGE_CURVE('',#14073,#14072,#2624,.T.);
#18689=EDGE_CURVE('',#14074,#14073,#1468,.T.);
#18690=EDGE_CURVE('',#14074,#14075,#4259,.T.);
#18691=EDGE_CURVE('',#14076,#14075,#1469,.T.);
#18692=EDGE_CURVE('',#14077,#14076,#2625,.T.);
#18693=EDGE_CURVE('',#14078,#14077,#1470,.T.);
#18694=EDGE_CURVE('',#14078,#14079,#4260,.T.);
#18695=EDGE_CURVE('',#14080,#14079,#1471,.T.);
#18696=EDGE_CURVE('',#14081,#14080,#2626,.T.);
#18697=EDGE_CURVE('',#14082,#14081,#1472,.T.);
#18698=EDGE_CURVE('',#14082,#14083,#4261,.T.);
#18699=EDGE_CURVE('',#14084,#14083,#1473,.T.);
#18700=EDGE_CURVE('',#14085,#14084,#2627,.T.);
#18701=EDGE_CURVE('',#14086,#14085,#1474,.T.);
#18702=EDGE_CURVE('',#14086,#14087,#4262,.T.);
#18703=EDGE_CURVE('',#14088,#14087,#1475,.T.);
#18704=EDGE_CURVE('',#14089,#14088,#2628,.T.);
#18705=EDGE_CURVE('',#14090,#14089,#1476,.T.);
#18706=EDGE_CURVE('',#14090,#14091,#4263,.T.);
#18707=EDGE_CURVE('',#14092,#14091,#1477,.T.);
#18708=EDGE_CURVE('',#14093,#14092,#2629,.T.);
#18709=EDGE_CURVE('',#14094,#14093,#1478,.T.);
#18710=EDGE_CURVE('',#14094,#14095,#4264,.T.);
#18711=EDGE_CURVE('',#14096,#14095,#1479,.T.);
#18712=EDGE_CURVE('',#14097,#14096,#2630,.T.);
#18713=EDGE_CURVE('',#14098,#14097,#1480,.T.);
#18714=EDGE_CURVE('',#14098,#14099,#4265,.T.);
#18715=EDGE_CURVE('',#13520,#14099,#1481,.T.);
#18716=EDGE_CURVE('',#14100,#13519,#1482,.T.);
#18717=EDGE_CURVE('',#14100,#14101,#4266,.T.);
#18718=EDGE_CURVE('',#13516,#14101,#1483,.T.);
#18719=EDGE_CURVE('',#14102,#13515,#1484,.T.);
#18720=EDGE_CURVE('',#14102,#14103,#4267,.T.);
#18721=EDGE_CURVE('',#13512,#14103,#1485,.T.);
#18722=EDGE_CURVE('',#14104,#13511,#1486,.T.);
#18723=EDGE_CURVE('',#14104,#14105,#4268,.T.);
#18724=EDGE_CURVE('',#13508,#14105,#1487,.T.);
#18725=EDGE_CURVE('',#14106,#13507,#1488,.T.);
#18726=EDGE_CURVE('',#14106,#14107,#4269,.T.);
#18727=EDGE_CURVE('',#13504,#14107,#1489,.T.);
#18728=EDGE_CURVE('',#14108,#13503,#1490,.T.);
#18729=EDGE_CURVE('',#14108,#14109,#4270,.T.);
#18730=EDGE_CURVE('',#13500,#14109,#1491,.T.);
#18731=EDGE_CURVE('',#14110,#13499,#1492,.T.);
#18732=EDGE_CURVE('',#14110,#14111,#4271,.T.);
#18733=EDGE_CURVE('',#13524,#14111,#1493,.T.);
#18734=EDGE_CURVE('',#14112,#13523,#1494,.T.);
#18735=EDGE_CURVE('',#14112,#14113,#4272,.T.);
#18736=EDGE_CURVE('',#13528,#14113,#1495,.T.);
#18737=EDGE_CURVE('',#14114,#13527,#1496,.T.);
#18738=EDGE_CURVE('',#14114,#14115,#4273,.T.);
#18739=EDGE_CURVE('',#13532,#14115,#1497,.T.);
#18740=EDGE_CURVE('',#14116,#13531,#1498,.T.);
#18741=EDGE_CURVE('',#14116,#14117,#4274,.T.);
#18742=EDGE_CURVE('',#13536,#14117,#1499,.T.);
#18743=EDGE_CURVE('',#14118,#13535,#1500,.T.);
#18744=EDGE_CURVE('',#14118,#14119,#4275,.T.);
#18745=EDGE_CURVE('',#13540,#14119,#1501,.T.);
#18746=EDGE_CURVE('',#14120,#13539,#1502,.T.);
#18747=EDGE_CURVE('',#14120,#14121,#4276,.T.);
#18748=EDGE_CURVE('',#13544,#14121,#1503,.T.);
#18749=EDGE_CURVE('',#14122,#13543,#1504,.T.);
#18750=EDGE_CURVE('',#14122,#14123,#4277,.T.);
#18751=EDGE_CURVE('',#13548,#14123,#1505,.T.);
#18752=EDGE_CURVE('',#14124,#13547,#1506,.T.);
#18753=EDGE_CURVE('',#14124,#14125,#4278,.T.);
#18754=EDGE_CURVE('',#13552,#14125,#1507,.T.);
#18755=EDGE_CURVE('',#14126,#13551,#1508,.T.);
#18756=EDGE_CURVE('',#14126,#14127,#4279,.T.);
#18757=EDGE_CURVE('',#13556,#14127,#1509,.T.);
#18758=EDGE_CURVE('',#14128,#13555,#1510,.T.);
#18759=EDGE_CURVE('',#14128,#14129,#4280,.T.);
#18760=EDGE_CURVE('',#14130,#14129,#1511,.T.);
#18761=EDGE_CURVE('',#14131,#14130,#2631,.T.);
#18762=EDGE_CURVE('',#14132,#14131,#1512,.T.);
#18763=EDGE_CURVE('',#14132,#14133,#4281,.T.);
#18764=EDGE_CURVE('',#14134,#14133,#1513,.T.);
#18765=EDGE_CURVE('',#14135,#14134,#2632,.T.);
#18766=EDGE_CURVE('',#14136,#14135,#1514,.T.);
#18767=EDGE_CURVE('',#14136,#14137,#4282,.T.);
#18768=EDGE_CURVE('',#14138,#14137,#1515,.T.);
#18769=EDGE_CURVE('',#14139,#14138,#2633,.T.);
#18770=EDGE_CURVE('',#14140,#14139,#1516,.T.);
#18771=EDGE_CURVE('',#14140,#14141,#4283,.T.);
#18772=EDGE_CURVE('',#14142,#14141,#1517,.T.);
#18773=EDGE_CURVE('',#14143,#14142,#2634,.T.);
#18774=EDGE_CURVE('',#14144,#14143,#1518,.T.);
#18775=EDGE_CURVE('',#14144,#14145,#4284,.T.);
#18776=EDGE_CURVE('',#14146,#14145,#1519,.T.);
#18777=EDGE_CURVE('',#14147,#14146,#2635,.T.);
#18778=EDGE_CURVE('',#14148,#14147,#1520,.T.);
#18779=EDGE_CURVE('',#14148,#14149,#4285,.T.);
#18780=EDGE_CURVE('',#14150,#14149,#1521,.T.);
#18781=EDGE_CURVE('',#13861,#14150,#3350,.T.);
#18782=EDGE_CURVE('',#13861,#14151,#9542,.T.);
#18783=EDGE_CURVE('',#14152,#14151,#4286,.T.);
#18784=EDGE_CURVE('',#14151,#14152,#4287,.T.);
#18785=EDGE_CURVE('',#14153,#14153,#4288,.T.);
#18786=EDGE_CURVE('',#14153,#14152,#4289,.T.);
#18787=EDGE_CURVE('',#14154,#14154,#4290,.T.);
#18788=EDGE_CURVE('',#14154,#14153,#9543,.T.);
#18789=EDGE_CURVE('',#14155,#14155,#4291,.T.);
#18790=EDGE_CURVE('',#14155,#14154,#4292,.T.);
#18791=EDGE_CURVE('',#13377,#14156,#4293,.T.);
#18792=EDGE_CURVE('',#14156,#14156,#4294,.T.);
#18793=EDGE_CURVE('',#14157,#14110,#2636,.T.);
#18794=EDGE_CURVE('',#14157,#14158,#4295,.T.);
#18795=EDGE_CURVE('',#14111,#14158,#2637,.T.);
#18796=EDGE_CURVE('',#14109,#14159,#2638,.T.);
#18797=EDGE_CURVE('',#14160,#14108,#2639,.T.);
#18798=EDGE_CURVE('',#14160,#14159,#4296,.T.);
#18799=EDGE_CURVE('',#14107,#14161,#2640,.T.);
#18800=EDGE_CURVE('',#14162,#14106,#2641,.T.);
#18801=EDGE_CURVE('',#14162,#14161,#4297,.T.);
#18802=EDGE_CURVE('',#14105,#14163,#2642,.T.);
#18803=EDGE_CURVE('',#14164,#14104,#2643,.T.);
#18804=EDGE_CURVE('',#14164,#14163,#4298,.T.);
#18805=EDGE_CURVE('',#14103,#14165,#2644,.T.);
#18806=EDGE_CURVE('',#14166,#14102,#2645,.T.);
#18807=EDGE_CURVE('',#14166,#14165,#4299,.T.);
#18808=EDGE_CURVE('',#14101,#14167,#2646,.T.);
#18809=EDGE_CURVE('',#14168,#14100,#2647,.T.);
#18810=EDGE_CURVE('',#14168,#14167,#4300,.T.);
#18811=EDGE_CURVE('',#14099,#14169,#2648,.T.);
#18812=EDGE_CURVE('',#14170,#14098,#2649,.T.);
#18813=EDGE_CURVE('',#14170,#14169,#4301,.T.);
#18814=EDGE_CURVE('',#14095,#14171,#2650,.T.);
#18815=EDGE_CURVE('',#14172,#14094,#2651,.T.);
#18816=EDGE_CURVE('',#14172,#14171,#4302,.T.);
#18817=EDGE_CURVE('',#14091,#14173,#2652,.T.);
#18818=EDGE_CURVE('',#14174,#14090,#2653,.T.);
#18819=EDGE_CURVE('',#14174,#14173,#4303,.T.);
#18820=EDGE_CURVE('',#14087,#14175,#2654,.T.);
#18821=EDGE_CURVE('',#14176,#14086,#2655,.T.);
#18822=EDGE_CURVE('',#14176,#14175,#4304,.T.);
#18823=EDGE_CURVE('',#14083,#14177,#2656,.T.);
#18824=EDGE_CURVE('',#14178,#14082,#2657,.T.);
#18825=EDGE_CURVE('',#14178,#14177,#4305,.T.);
#18826=EDGE_CURVE('',#14079,#14179,#2658,.T.);
#18827=EDGE_CURVE('',#14180,#14078,#2659,.T.);
#18828=EDGE_CURVE('',#14180,#14179,#4306,.T.);
#18829=EDGE_CURVE('',#14075,#14181,#2660,.T.);
#18830=EDGE_CURVE('',#14182,#14074,#2661,.T.);
#18831=EDGE_CURVE('',#14182,#14181,#4307,.T.);
#18832=EDGE_CURVE('',#14071,#14183,#2662,.T.);
#18833=EDGE_CURVE('',#14184,#14070,#2663,.T.);
#18834=EDGE_CURVE('',#14184,#14183,#4308,.T.);
#18835=EDGE_CURVE('',#14067,#14185,#2664,.T.);
#18836=EDGE_CURVE('',#14186,#14066,#2665,.T.);
#18837=EDGE_CURVE('',#14186,#14185,#4309,.T.);
#18838=EDGE_CURVE('',#14063,#14187,#2666,.T.);
#18839=EDGE_CURVE('',#14188,#14062,#2667,.T.);
#18840=EDGE_CURVE('',#14188,#14187,#4310,.T.);
#18841=EDGE_CURVE('',#14059,#14189,#2668,.T.);
#18842=EDGE_CURVE('',#14190,#14058,#2669,.T.);
#18843=EDGE_CURVE('',#14190,#14189,#4311,.T.);
#18844=EDGE_CURVE('',#14055,#14191,#2670,.T.);
#18845=EDGE_CURVE('',#14192,#14054,#2671,.T.);
#18846=EDGE_CURVE('',#14192,#14191,#4312,.T.);
#18847=EDGE_CURVE('',#14051,#14193,#2672,.T.);
#18848=EDGE_CURVE('',#14194,#14050,#2673,.T.);
#18849=EDGE_CURVE('',#14194,#14193,#4313,.T.);
#18850=EDGE_CURVE('',#14047,#14195,#2674,.T.);
#18851=EDGE_CURVE('',#14196,#14046,#2675,.T.);
#18852=EDGE_CURVE('',#14196,#14195,#4314,.T.);
#18853=EDGE_CURVE('',#14043,#14197,#2676,.T.);
#18854=EDGE_CURVE('',#14198,#14042,#2677,.T.);
#18855=EDGE_CURVE('',#14198,#14197,#4315,.T.);
#18856=EDGE_CURVE('',#14039,#14199,#2678,.T.);
#18857=EDGE_CURVE('',#14200,#14038,#2679,.T.);
#18858=EDGE_CURVE('',#14200,#14199,#4316,.T.);
#18859=EDGE_CURVE('',#14035,#14201,#2680,.T.);
#18860=EDGE_CURVE('',#14202,#14034,#2681,.T.);
#18861=EDGE_CURVE('',#14202,#14201,#4317,.T.);
#18862=EDGE_CURVE('',#14031,#14203,#2682,.T.);
#18863=EDGE_CURVE('',#14204,#14030,#2683,.T.);
#18864=EDGE_CURVE('',#14204,#14203,#4318,.T.);
#18865=EDGE_CURVE('',#14027,#14205,#2684,.T.);
#18866=EDGE_CURVE('',#14206,#14026,#2685,.T.);
#18867=EDGE_CURVE('',#14206,#14205,#4319,.T.);
#18868=EDGE_CURVE('',#14023,#14207,#2686,.T.);
#18869=EDGE_CURVE('',#14208,#14022,#2687,.T.);
#18870=EDGE_CURVE('',#14208,#14207,#4320,.T.);
#18871=EDGE_CURVE('',#14019,#14209,#2688,.T.);
#18872=EDGE_CURVE('',#14210,#14018,#2689,.T.);
#18873=EDGE_CURVE('',#14210,#14209,#4321,.T.);
#18874=EDGE_CURVE('',#14015,#14211,#2690,.T.);
#18875=EDGE_CURVE('',#14212,#14014,#2691,.T.);
#18876=EDGE_CURVE('',#14212,#14211,#4322,.T.);
#18877=EDGE_CURVE('',#14011,#14213,#2692,.T.);
#18878=EDGE_CURVE('',#14214,#14010,#2693,.T.);
#18879=EDGE_CURVE('',#14214,#14213,#4323,.T.);
#18880=EDGE_CURVE('',#14007,#14215,#2694,.T.);
#18881=EDGE_CURVE('',#14216,#14006,#2695,.T.);
#18882=EDGE_CURVE('',#14216,#14215,#4324,.T.);
#18883=EDGE_CURVE('',#14003,#14217,#2696,.T.);
#18884=EDGE_CURVE('',#14218,#14002,#2697,.T.);
#18885=EDGE_CURVE('',#14218,#14217,#4325,.T.);
#18886=EDGE_CURVE('',#13999,#14219,#2698,.T.);
#18887=EDGE_CURVE('',#14220,#13998,#2699,.T.);
#18888=EDGE_CURVE('',#14220,#14219,#4326,.T.);
#18889=EDGE_CURVE('',#13995,#14221,#2700,.T.);
#18890=EDGE_CURVE('',#14222,#13994,#2701,.T.);
#18891=EDGE_CURVE('',#14222,#14221,#4327,.T.);
#18892=EDGE_CURVE('',#13991,#14223,#2702,.T.);
#18893=EDGE_CURVE('',#14224,#13990,#2703,.T.);
#18894=EDGE_CURVE('',#14224,#14223,#4328,.T.);
#18895=EDGE_CURVE('',#13987,#14225,#2704,.T.);
#18896=EDGE_CURVE('',#14226,#13986,#2705,.T.);
#18897=EDGE_CURVE('',#14226,#14225,#4329,.T.);
#18898=EDGE_CURVE('',#13983,#14227,#2706,.T.);
#18899=EDGE_CURVE('',#14228,#13982,#2707,.T.);
#18900=EDGE_CURVE('',#14228,#14227,#4330,.T.);
#18901=EDGE_CURVE('',#13979,#14229,#2708,.T.);
#18902=EDGE_CURVE('',#14230,#13978,#2709,.T.);
#18903=EDGE_CURVE('',#14230,#14229,#4331,.T.);
#18904=EDGE_CURVE('',#13975,#14231,#2710,.T.);
#18905=EDGE_CURVE('',#14232,#13974,#2711,.T.);
#18906=EDGE_CURVE('',#14232,#14231,#4332,.T.);
#18907=EDGE_CURVE('',#13971,#14233,#2712,.T.);
#18908=EDGE_CURVE('',#14234,#13970,#2713,.T.);
#18909=EDGE_CURVE('',#14234,#14233,#4333,.T.);
#18910=EDGE_CURVE('',#13967,#14235,#2714,.T.);
#18911=EDGE_CURVE('',#14236,#13966,#2715,.T.);
#18912=EDGE_CURVE('',#14236,#14235,#4334,.T.);
#18913=EDGE_CURVE('',#13963,#14237,#2716,.T.);
#18914=EDGE_CURVE('',#14238,#13962,#2717,.T.);
#18915=EDGE_CURVE('',#14238,#14237,#4335,.T.);
#18916=EDGE_CURVE('',#13959,#14239,#2718,.T.);
#18917=EDGE_CURVE('',#14240,#13958,#2719,.T.);
#18918=EDGE_CURVE('',#14240,#14239,#4336,.T.);
#18919=EDGE_CURVE('',#13955,#14241,#2720,.T.);
#18920=EDGE_CURVE('',#14242,#13954,#2721,.T.);
#18921=EDGE_CURVE('',#14242,#14241,#4337,.T.);
#18922=EDGE_CURVE('',#13951,#14243,#2722,.T.);
#18923=EDGE_CURVE('',#14244,#13950,#2723,.T.);
#18924=EDGE_CURVE('',#14244,#14243,#4338,.T.);
#18925=EDGE_CURVE('',#13947,#14245,#2724,.T.);
#18926=EDGE_CURVE('',#14246,#13946,#2725,.T.);
#18927=EDGE_CURVE('',#14246,#14245,#4339,.T.);
#18928=EDGE_CURVE('',#13943,#14247,#2726,.T.);
#18929=EDGE_CURVE('',#14248,#13942,#2727,.T.);
#18930=EDGE_CURVE('',#14248,#14247,#4340,.T.);
#18931=EDGE_CURVE('',#13939,#14249,#2728,.T.);
#18932=EDGE_CURVE('',#14250,#13938,#2729,.T.);
#18933=EDGE_CURVE('',#14250,#14249,#4341,.T.);
#18934=EDGE_CURVE('',#13935,#14251,#2730,.T.);
#18935=EDGE_CURVE('',#14252,#13934,#2731,.T.);
#18936=EDGE_CURVE('',#14252,#14251,#4342,.T.);
#18937=EDGE_CURVE('',#13931,#14253,#2732,.T.);
#18938=EDGE_CURVE('',#14254,#13930,#2733,.T.);
#18939=EDGE_CURVE('',#14254,#14253,#4343,.T.);
#18940=EDGE_CURVE('',#13927,#14255,#2734,.T.);
#18941=EDGE_CURVE('',#14256,#13926,#2735,.T.);
#18942=EDGE_CURVE('',#14256,#14255,#4344,.T.);
#18943=EDGE_CURVE('',#13923,#14257,#2736,.T.);
#18944=EDGE_CURVE('',#14258,#13922,#2737,.T.);
#18945=EDGE_CURVE('',#14258,#14257,#4345,.T.);
#18946=EDGE_CURVE('',#13919,#14259,#2738,.T.);
#18947=EDGE_CURVE('',#14260,#13918,#2739,.T.);
#18948=EDGE_CURVE('',#14260,#14259,#4346,.T.);
#18949=EDGE_CURVE('',#13915,#14261,#2740,.T.);
#18950=EDGE_CURVE('',#14262,#13914,#2741,.T.);
#18951=EDGE_CURVE('',#14262,#14261,#4347,.T.);
#18952=EDGE_CURVE('',#13911,#14263,#2742,.T.);
#18953=EDGE_CURVE('',#14264,#13910,#2743,.T.);
#18954=EDGE_CURVE('',#14264,#14263,#4348,.T.);
#18955=EDGE_CURVE('',#13907,#14265,#2744,.T.);
#18956=EDGE_CURVE('',#14266,#13906,#2745,.T.);
#18957=EDGE_CURVE('',#14266,#14265,#4349,.T.);
#18958=EDGE_CURVE('',#13903,#14267,#2746,.T.);
#18959=EDGE_CURVE('',#14268,#13902,#2747,.T.);
#18960=EDGE_CURVE('',#14268,#14267,#4350,.T.);
#18961=EDGE_CURVE('',#13899,#14269,#2748,.T.);
#18962=EDGE_CURVE('',#14270,#13898,#2749,.T.);
#18963=EDGE_CURVE('',#14270,#14269,#4351,.T.);
#18964=EDGE_CURVE('',#13895,#14271,#2750,.T.);
#18965=EDGE_CURVE('',#14272,#13894,#2751,.T.);
#18966=EDGE_CURVE('',#14272,#14271,#4352,.T.);
#18967=EDGE_CURVE('',#13891,#14273,#2752,.T.);
#18968=EDGE_CURVE('',#14274,#13890,#2753,.T.);
#18969=EDGE_CURVE('',#14274,#14273,#4353,.T.);
#18970=EDGE_CURVE('',#13887,#14275,#2754,.T.);
#18971=EDGE_CURVE('',#14276,#13886,#2755,.T.);
#18972=EDGE_CURVE('',#14276,#14275,#4354,.T.);
#18973=EDGE_CURVE('',#13883,#14277,#2756,.T.);
#18974=EDGE_CURVE('',#14278,#13882,#2757,.T.);
#18975=EDGE_CURVE('',#14278,#14277,#4355,.T.);
#18976=EDGE_CURVE('',#13879,#14279,#2758,.T.);
#18977=EDGE_CURVE('',#14280,#13878,#2759,.T.);
#18978=EDGE_CURVE('',#14280,#14279,#4356,.T.);
#18979=EDGE_CURVE('',#13875,#14281,#2760,.T.);
#18980=EDGE_CURVE('',#14282,#13874,#2761,.T.);
#18981=EDGE_CURVE('',#14282,#14281,#4357,.T.);
#18982=EDGE_CURVE('',#13871,#14283,#2762,.T.);
#18983=EDGE_CURVE('',#14284,#13870,#2763,.T.);
#18984=EDGE_CURVE('',#14284,#14283,#4358,.T.);
#18985=EDGE_CURVE('',#14285,#14112,#2764,.T.);
#18986=EDGE_CURVE('',#14285,#14286,#4359,.T.);
#18987=EDGE_CURVE('',#14113,#14286,#2765,.T.);
#18988=EDGE_CURVE('',#14287,#14114,#2766,.T.);
#18989=EDGE_CURVE('',#14287,#14288,#4360,.T.);
#18990=EDGE_CURVE('',#14115,#14288,#2767,.T.);
#18991=EDGE_CURVE('',#14289,#14116,#2768,.T.);
#18992=EDGE_CURVE('',#14289,#14290,#4361,.T.);
#18993=EDGE_CURVE('',#14117,#14290,#2769,.T.);
#18994=EDGE_CURVE('',#14291,#14118,#2770,.T.);
#18995=EDGE_CURVE('',#14291,#14292,#4362,.T.);
#18996=EDGE_CURVE('',#14119,#14292,#2771,.T.);
#18997=EDGE_CURVE('',#14293,#14120,#2772,.T.);
#18998=EDGE_CURVE('',#14293,#14294,#4363,.T.);
#18999=EDGE_CURVE('',#14121,#14294,#2773,.T.);
#19000=EDGE_CURVE('',#14295,#14122,#2774,.T.);
#19001=EDGE_CURVE('',#14295,#14296,#4364,.T.);
#19002=EDGE_CURVE('',#14123,#14296,#2775,.T.);
#19003=EDGE_CURVE('',#14297,#14124,#2776,.T.);
#19004=EDGE_CURVE('',#14297,#14298,#4365,.T.);
#19005=EDGE_CURVE('',#14125,#14298,#2777,.T.);
#19006=EDGE_CURVE('',#14299,#14126,#2778,.T.);
#19007=EDGE_CURVE('',#14299,#14300,#4366,.T.);
#19008=EDGE_CURVE('',#14127,#14300,#2779,.T.);
#19009=EDGE_CURVE('',#14301,#14128,#2780,.T.);
#19010=EDGE_CURVE('',#14301,#14302,#4367,.T.);
#19011=EDGE_CURVE('',#14129,#14302,#2781,.T.);
#19012=EDGE_CURVE('',#14303,#14132,#2782,.T.);
#19013=EDGE_CURVE('',#14303,#14304,#4368,.T.);
#19014=EDGE_CURVE('',#14133,#14304,#2783,.T.);
#19015=EDGE_CURVE('',#14305,#14136,#2784,.T.);
#19016=EDGE_CURVE('',#14305,#14306,#4369,.T.);
#19017=EDGE_CURVE('',#14137,#14306,#2785,.T.);
#19018=EDGE_CURVE('',#14307,#14140,#2786,.T.);
#19019=EDGE_CURVE('',#14307,#14308,#4370,.T.);
#19020=EDGE_CURVE('',#14141,#14308,#2787,.T.);
#19021=EDGE_CURVE('',#14309,#14144,#2788,.T.);
#19022=EDGE_CURVE('',#14309,#14310,#4371,.T.);
#19023=EDGE_CURVE('',#14145,#14310,#2789,.T.);
#19024=EDGE_CURVE('',#14311,#14148,#2790,.T.);
#19025=EDGE_CURVE('',#14311,#14312,#4372,.T.);
#19026=EDGE_CURVE('',#14149,#14312,#2791,.T.);
#19027=EDGE_CURVE('',#13867,#14313,#2792,.T.);
#19028=EDGE_CURVE('',#14314,#13866,#2793,.T.);
#19029=EDGE_CURVE('',#14314,#14313,#4373,.T.);
#19030=EDGE_CURVE('',#14315,#14157,#9544,.T.);
#19031=EDGE_CURVE('',#14315,#14316,#4374,.T.);
#19032=EDGE_CURVE('',#14158,#14316,#9545,.T.);
#19033=EDGE_CURVE('',#14159,#14317,#9546,.T.);
#19034=EDGE_CURVE('',#14318,#14160,#9547,.T.);
#19035=EDGE_CURVE('',#14318,#14317,#4375,.T.);
#19036=EDGE_CURVE('',#14161,#14319,#9548,.T.);
#19037=EDGE_CURVE('',#14320,#14162,#9549,.T.);
#19038=EDGE_CURVE('',#14320,#14319,#4376,.T.);
#19039=EDGE_CURVE('',#14163,#14321,#9550,.T.);
#19040=EDGE_CURVE('',#14322,#14164,#9551,.T.);
#19041=EDGE_CURVE('',#14322,#14321,#4377,.T.);
#19042=EDGE_CURVE('',#14165,#14323,#9552,.T.);
#19043=EDGE_CURVE('',#14324,#14166,#9553,.T.);
#19044=EDGE_CURVE('',#14324,#14323,#4378,.T.);
#19045=EDGE_CURVE('',#14167,#14325,#9554,.T.);
#19046=EDGE_CURVE('',#14326,#14168,#9555,.T.);
#19047=EDGE_CURVE('',#14326,#14325,#4379,.T.);
#19048=EDGE_CURVE('',#14169,#14327,#9556,.T.);
#19049=EDGE_CURVE('',#14328,#14170,#9557,.T.);
#19050=EDGE_CURVE('',#14328,#14327,#4380,.T.);
#19051=EDGE_CURVE('',#14171,#14329,#9558,.T.);
#19052=EDGE_CURVE('',#14330,#14172,#9559,.T.);
#19053=EDGE_CURVE('',#14330,#14329,#4381,.T.);
#19054=EDGE_CURVE('',#14173,#14331,#9560,.T.);
#19055=EDGE_CURVE('',#14332,#14174,#9561,.T.);
#19056=EDGE_CURVE('',#14332,#14331,#4382,.T.);
#19057=EDGE_CURVE('',#14175,#14333,#9562,.T.);
#19058=EDGE_CURVE('',#14334,#14176,#9563,.T.);
#19059=EDGE_CURVE('',#14334,#14333,#4383,.T.);
#19060=EDGE_CURVE('',#14177,#14335,#9564,.T.);
#19061=EDGE_CURVE('',#14336,#14178,#9565,.T.);
#19062=EDGE_CURVE('',#14336,#14335,#4384,.T.);
#19063=EDGE_CURVE('',#14179,#14337,#9566,.T.);
#19064=EDGE_CURVE('',#14338,#14180,#9567,.T.);
#19065=EDGE_CURVE('',#14338,#14337,#4385,.T.);
#19066=EDGE_CURVE('',#14181,#14339,#9568,.T.);
#19067=EDGE_CURVE('',#14340,#14182,#9569,.T.);
#19068=EDGE_CURVE('',#14340,#14339,#4386,.T.);
#19069=EDGE_CURVE('',#14183,#14341,#9570,.T.);
#19070=EDGE_CURVE('',#14342,#14184,#9571,.T.);
#19071=EDGE_CURVE('',#14342,#14341,#4387,.T.);
#19072=EDGE_CURVE('',#14185,#14343,#9572,.T.);
#19073=EDGE_CURVE('',#14344,#14186,#9573,.T.);
#19074=EDGE_CURVE('',#14344,#14343,#4388,.T.);
#19075=EDGE_CURVE('',#14187,#14345,#9574,.T.);
#19076=EDGE_CURVE('',#14346,#14188,#9575,.T.);
#19077=EDGE_CURVE('',#14346,#14345,#4389,.T.);
#19078=EDGE_CURVE('',#14189,#14347,#9576,.T.);
#19079=EDGE_CURVE('',#14348,#14190,#9577,.T.);
#19080=EDGE_CURVE('',#14348,#14347,#4390,.T.);
#19081=EDGE_CURVE('',#14191,#14349,#9578,.T.);
#19082=EDGE_CURVE('',#14350,#14192,#9579,.T.);
#19083=EDGE_CURVE('',#14350,#14349,#4391,.T.);
#19084=EDGE_CURVE('',#14193,#14351,#9580,.T.);
#19085=EDGE_CURVE('',#14352,#14194,#9581,.T.);
#19086=EDGE_CURVE('',#14352,#14351,#4392,.T.);
#19087=EDGE_CURVE('',#14195,#14353,#9582,.T.);
#19088=EDGE_CURVE('',#14354,#14196,#9583,.T.);
#19089=EDGE_CURVE('',#14354,#14353,#4393,.T.);
#19090=EDGE_CURVE('',#14197,#14355,#9584,.T.);
#19091=EDGE_CURVE('',#14356,#14198,#9585,.T.);
#19092=EDGE_CURVE('',#14356,#14355,#4394,.T.);
#19093=EDGE_CURVE('',#14199,#14357,#9586,.T.);
#19094=EDGE_CURVE('',#14358,#14200,#9587,.T.);
#19095=EDGE_CURVE('',#14358,#14357,#4395,.T.);
#19096=EDGE_CURVE('',#14201,#14359,#9588,.T.);
#19097=EDGE_CURVE('',#14360,#14202,#9589,.T.);
#19098=EDGE_CURVE('',#14360,#14359,#4396,.T.);
#19099=EDGE_CURVE('',#14203,#14361,#9590,.T.);
#19100=EDGE_CURVE('',#14362,#14204,#9591,.T.);
#19101=EDGE_CURVE('',#14362,#14361,#4397,.T.);
#19102=EDGE_CURVE('',#14205,#14363,#9592,.T.);
#19103=EDGE_CURVE('',#14364,#14206,#9593,.T.);
#19104=EDGE_CURVE('',#14364,#14363,#4398,.T.);
#19105=EDGE_CURVE('',#14207,#14365,#9594,.T.);
#19106=EDGE_CURVE('',#14366,#14208,#9595,.T.);
#19107=EDGE_CURVE('',#14366,#14365,#4399,.T.);
#19108=EDGE_CURVE('',#14209,#14367,#9596,.T.);
#19109=EDGE_CURVE('',#14368,#14210,#9597,.T.);
#19110=EDGE_CURVE('',#14368,#14367,#4400,.T.);
#19111=EDGE_CURVE('',#14211,#14369,#9598,.T.);
#19112=EDGE_CURVE('',#14370,#14212,#9599,.T.);
#19113=EDGE_CURVE('',#14370,#14369,#4401,.T.);
#19114=EDGE_CURVE('',#14213,#14371,#9600,.T.);
#19115=EDGE_CURVE('',#14372,#14214,#9601,.T.);
#19116=EDGE_CURVE('',#14372,#14371,#4402,.T.);
#19117=EDGE_CURVE('',#14215,#14373,#9602,.T.);
#19118=EDGE_CURVE('',#14374,#14216,#9603,.T.);
#19119=EDGE_CURVE('',#14374,#14373,#4403,.T.);
#19120=EDGE_CURVE('',#14217,#14375,#9604,.T.);
#19121=EDGE_CURVE('',#14376,#14218,#9605,.T.);
#19122=EDGE_CURVE('',#14376,#14375,#4404,.T.);
#19123=EDGE_CURVE('',#14219,#14377,#9606,.T.);
#19124=EDGE_CURVE('',#14378,#14220,#9607,.T.);
#19125=EDGE_CURVE('',#14378,#14377,#4405,.T.);
#19126=EDGE_CURVE('',#14221,#14379,#9608,.T.);
#19127=EDGE_CURVE('',#14380,#14222,#9609,.T.);
#19128=EDGE_CURVE('',#14380,#14379,#4406,.T.);
#19129=EDGE_CURVE('',#14223,#14381,#9610,.T.);
#19130=EDGE_CURVE('',#14382,#14224,#9611,.T.);
#19131=EDGE_CURVE('',#14382,#14381,#4407,.T.);
#19132=EDGE_CURVE('',#14225,#14383,#9612,.T.);
#19133=EDGE_CURVE('',#14384,#14226,#9613,.T.);
#19134=EDGE_CURVE('',#14384,#14383,#4408,.T.);
#19135=EDGE_CURVE('',#14227,#14385,#9614,.T.);
#19136=EDGE_CURVE('',#14386,#14228,#9615,.T.);
#19137=EDGE_CURVE('',#14386,#14385,#4409,.T.);
#19138=EDGE_CURVE('',#14229,#14387,#9616,.T.);
#19139=EDGE_CURVE('',#14388,#14230,#9617,.T.);
#19140=EDGE_CURVE('',#14388,#14387,#4410,.T.);
#19141=EDGE_CURVE('',#14231,#14389,#9618,.T.);
#19142=EDGE_CURVE('',#14390,#14232,#9619,.T.);
#19143=EDGE_CURVE('',#14390,#14389,#4411,.T.);
#19144=EDGE_CURVE('',#14233,#14391,#9620,.T.);
#19145=EDGE_CURVE('',#14392,#14234,#9621,.T.);
#19146=EDGE_CURVE('',#14392,#14391,#4412,.T.);
#19147=EDGE_CURVE('',#14235,#14393,#9622,.T.);
#19148=EDGE_CURVE('',#14394,#14236,#9623,.T.);
#19149=EDGE_CURVE('',#14394,#14393,#4413,.T.);
#19150=EDGE_CURVE('',#14237,#14395,#9624,.T.);
#19151=EDGE_CURVE('',#14396,#14238,#9625,.T.);
#19152=EDGE_CURVE('',#14396,#14395,#4414,.T.);
#19153=EDGE_CURVE('',#14239,#14397,#9626,.T.);
#19154=EDGE_CURVE('',#14398,#14240,#9627,.T.);
#19155=EDGE_CURVE('',#14398,#14397,#4415,.T.);
#19156=EDGE_CURVE('',#14241,#14399,#9628,.T.);
#19157=EDGE_CURVE('',#14400,#14242,#9629,.T.);
#19158=EDGE_CURVE('',#14400,#14399,#4416,.T.);
#19159=EDGE_CURVE('',#14243,#14401,#9630,.T.);
#19160=EDGE_CURVE('',#14402,#14244,#9631,.T.);
#19161=EDGE_CURVE('',#14402,#14401,#4417,.T.);
#19162=EDGE_CURVE('',#14245,#14403,#9632,.T.);
#19163=EDGE_CURVE('',#14404,#14246,#9633,.T.);
#19164=EDGE_CURVE('',#14404,#14403,#4418,.T.);
#19165=EDGE_CURVE('',#14247,#14405,#9634,.T.);
#19166=EDGE_CURVE('',#14406,#14248,#9635,.T.);
#19167=EDGE_CURVE('',#14406,#14405,#4419,.T.);
#19168=EDGE_CURVE('',#14249,#14407,#9636,.T.);
#19169=EDGE_CURVE('',#14408,#14250,#9637,.T.);
#19170=EDGE_CURVE('',#14408,#14407,#4420,.T.);
#19171=EDGE_CURVE('',#14251,#14409,#9638,.T.);
#19172=EDGE_CURVE('',#14410,#14252,#9639,.T.);
#19173=EDGE_CURVE('',#14410,#14409,#4421,.T.);
#19174=EDGE_CURVE('',#14253,#14411,#9640,.T.);
#19175=EDGE_CURVE('',#14412,#14254,#9641,.T.);
#19176=EDGE_CURVE('',#14412,#14411,#4422,.T.);
#19177=EDGE_CURVE('',#14255,#14413,#9642,.T.);
#19178=EDGE_CURVE('',#14414,#14256,#9643,.T.);
#19179=EDGE_CURVE('',#14414,#14413,#4423,.T.);
#19180=EDGE_CURVE('',#14257,#14415,#9644,.T.);
#19181=EDGE_CURVE('',#14416,#14258,#9645,.T.);
#19182=EDGE_CURVE('',#14416,#14415,#4424,.T.);
#19183=EDGE_CURVE('',#14259,#14417,#9646,.T.);
#19184=EDGE_CURVE('',#14418,#14260,#9647,.T.);
#19185=EDGE_CURVE('',#14418,#14417,#4425,.T.);
#19186=EDGE_CURVE('',#14261,#14419,#9648,.T.);
#19187=EDGE_CURVE('',#14420,#14262,#9649,.T.);
#19188=EDGE_CURVE('',#14420,#14419,#4426,.T.);
#19189=EDGE_CURVE('',#14263,#14421,#9650,.T.);
#19190=EDGE_CURVE('',#14422,#14264,#9651,.T.);
#19191=EDGE_CURVE('',#14422,#14421,#4427,.T.);
#19192=EDGE_CURVE('',#14265,#14423,#9652,.T.);
#19193=EDGE_CURVE('',#14424,#14266,#9653,.T.);
#19194=EDGE_CURVE('',#14424,#14423,#4428,.T.);
#19195=EDGE_CURVE('',#14267,#14425,#9654,.T.);
#19196=EDGE_CURVE('',#14426,#14268,#9655,.T.);
#19197=EDGE_CURVE('',#14426,#14425,#4429,.T.);
#19198=EDGE_CURVE('',#14269,#14427,#9656,.T.);
#19199=EDGE_CURVE('',#14428,#14270,#9657,.T.);
#19200=EDGE_CURVE('',#14428,#14427,#4430,.T.);
#19201=EDGE_CURVE('',#14271,#14429,#9658,.T.);
#19202=EDGE_CURVE('',#14430,#14272,#9659,.T.);
#19203=EDGE_CURVE('',#14430,#14429,#4431,.T.);
#19204=EDGE_CURVE('',#14273,#14431,#9660,.T.);
#19205=EDGE_CURVE('',#14432,#14274,#9661,.T.);
#19206=EDGE_CURVE('',#14432,#14431,#4432,.T.);
#19207=EDGE_CURVE('',#14275,#14433,#9662,.T.);
#19208=EDGE_CURVE('',#14434,#14276,#9663,.T.);
#19209=EDGE_CURVE('',#14434,#14433,#4433,.T.);
#19210=EDGE_CURVE('',#14277,#14435,#9664,.T.);
#19211=EDGE_CURVE('',#14436,#14278,#9665,.T.);
#19212=EDGE_CURVE('',#14436,#14435,#4434,.T.);
#19213=EDGE_CURVE('',#14279,#14437,#9666,.T.);
#19214=EDGE_CURVE('',#14438,#14280,#9667,.T.);
#19215=EDGE_CURVE('',#14438,#14437,#4435,.T.);
#19216=EDGE_CURVE('',#14281,#14439,#9668,.T.);
#19217=EDGE_CURVE('',#14440,#14282,#9669,.T.);
#19218=EDGE_CURVE('',#14440,#14439,#4436,.T.);
#19219=EDGE_CURVE('',#14283,#14441,#9670,.T.);
#19220=EDGE_CURVE('',#14442,#14284,#9671,.T.);
#19221=EDGE_CURVE('',#14442,#14441,#4437,.T.);
#19222=EDGE_CURVE('',#14443,#14285,#9672,.T.);
#19223=EDGE_CURVE('',#14443,#14444,#4438,.T.);
#19224=EDGE_CURVE('',#14286,#14444,#9673,.T.);
#19225=EDGE_CURVE('',#14445,#14287,#9674,.T.);
#19226=EDGE_CURVE('',#14445,#14446,#4439,.T.);
#19227=EDGE_CURVE('',#14288,#14446,#9675,.T.);
#19228=EDGE_CURVE('',#14447,#14289,#9676,.T.);
#19229=EDGE_CURVE('',#14447,#14448,#4440,.T.);
#19230=EDGE_CURVE('',#14290,#14448,#9677,.T.);
#19231=EDGE_CURVE('',#14449,#14291,#9678,.T.);
#19232=EDGE_CURVE('',#14449,#14450,#4441,.T.);
#19233=EDGE_CURVE('',#14292,#14450,#9679,.T.);
#19234=EDGE_CURVE('',#14451,#14293,#9680,.T.);
#19235=EDGE_CURVE('',#14451,#14452,#4442,.T.);
#19236=EDGE_CURVE('',#14294,#14452,#9681,.T.);
#19237=EDGE_CURVE('',#14453,#14295,#9682,.T.);
#19238=EDGE_CURVE('',#14453,#14454,#4443,.T.);
#19239=EDGE_CURVE('',#14296,#14454,#9683,.T.);
#19240=EDGE_CURVE('',#14455,#14297,#9684,.T.);
#19241=EDGE_CURVE('',#14455,#14456,#4444,.T.);
#19242=EDGE_CURVE('',#14298,#14456,#9685,.T.);
#19243=EDGE_CURVE('',#14457,#14299,#9686,.T.);
#19244=EDGE_CURVE('',#14457,#14458,#4445,.T.);
#19245=EDGE_CURVE('',#14300,#14458,#9687,.T.);
#19246=EDGE_CURVE('',#14459,#14301,#9688,.T.);
#19247=EDGE_CURVE('',#14459,#14460,#4446,.T.);
#19248=EDGE_CURVE('',#14302,#14460,#9689,.T.);
#19249=EDGE_CURVE('',#14461,#14303,#9690,.T.);
#19250=EDGE_CURVE('',#14461,#14462,#4447,.T.);
#19251=EDGE_CURVE('',#14304,#14462,#9691,.T.);
#19252=EDGE_CURVE('',#14463,#14305,#9692,.T.);
#19253=EDGE_CURVE('',#14463,#14464,#4448,.T.);
#19254=EDGE_CURVE('',#14306,#14464,#9693,.T.);
#19255=EDGE_CURVE('',#14465,#14307,#9694,.T.);
#19256=EDGE_CURVE('',#14465,#14466,#4449,.T.);
#19257=EDGE_CURVE('',#14308,#14466,#9695,.T.);
#19258=EDGE_CURVE('',#14467,#14309,#9696,.T.);
#19259=EDGE_CURVE('',#14467,#14468,#4450,.T.);
#19260=EDGE_CURVE('',#14310,#14468,#9697,.T.);
#19261=EDGE_CURVE('',#14469,#14311,#9698,.T.);
#19262=EDGE_CURVE('',#14469,#14470,#4451,.T.);
#19263=EDGE_CURVE('',#14312,#14470,#9699,.T.);
#19264=EDGE_CURVE('',#14313,#14471,#9700,.T.);
#19265=EDGE_CURVE('',#14472,#14314,#9701,.T.);
#19266=EDGE_CURVE('',#14472,#14471,#4452,.T.);
#19267=EDGE_CURVE('',#13770,#14315,#2794,.T.);
#19268=EDGE_CURVE('',#14316,#13769,#2795,.T.);
#19269=EDGE_CURVE('',#14317,#13771,#2796,.T.);
#19270=EDGE_CURVE('',#13772,#14318,#2797,.T.);
#19271=EDGE_CURVE('',#14319,#13773,#2798,.T.);
#19272=EDGE_CURVE('',#13774,#14320,#2799,.T.);
#19273=EDGE_CURVE('',#14321,#13775,#2800,.T.);
#19274=EDGE_CURVE('',#13776,#14322,#2801,.T.);
#19275=EDGE_CURVE('',#14323,#13777,#2802,.T.);
#19276=EDGE_CURVE('',#13778,#14324,#2803,.T.);
#19277=EDGE_CURVE('',#14325,#13779,#2804,.T.);
#19278=EDGE_CURVE('',#13780,#14326,#2805,.T.);
#19279=EDGE_CURVE('',#14327,#13781,#2806,.T.);
#19280=EDGE_CURVE('',#13782,#14328,#2807,.T.);
#19281=EDGE_CURVE('',#14329,#13785,#2808,.T.);
#19282=EDGE_CURVE('',#13786,#14330,#2809,.T.);
#19283=EDGE_CURVE('',#14331,#13789,#2810,.T.);
#19284=EDGE_CURVE('',#13790,#14332,#2811,.T.);
#19285=EDGE_CURVE('',#14333,#13793,#2812,.T.);
#19286=EDGE_CURVE('',#13794,#14334,#2813,.T.);
#19287=EDGE_CURVE('',#14335,#13797,#2814,.T.);
#19288=EDGE_CURVE('',#13798,#14336,#2815,.T.);
#19289=EDGE_CURVE('',#14337,#13801,#2816,.T.);
#19290=EDGE_CURVE('',#13802,#14338,#2817,.T.);
#19291=EDGE_CURVE('',#14339,#13805,#2818,.T.);
#19292=EDGE_CURVE('',#13806,#14340,#2819,.T.);
#19293=EDGE_CURVE('',#14341,#13809,#2820,.T.);
#19294=EDGE_CURVE('',#13810,#14342,#2821,.T.);
#19295=EDGE_CURVE('',#14343,#13813,#2822,.T.);
#19296=EDGE_CURVE('',#13814,#14344,#2823,.T.);
#19297=EDGE_CURVE('',#14345,#13817,#2824,.T.);
#19298=EDGE_CURVE('',#13818,#14346,#2825,.T.);
#19299=EDGE_CURVE('',#14347,#13821,#2826,.T.);
#19300=EDGE_CURVE('',#13822,#14348,#2827,.T.);
#19301=EDGE_CURVE('',#14349,#13825,#2828,.T.);
#19302=EDGE_CURVE('',#13826,#14350,#2829,.T.);
#19303=EDGE_CURVE('',#14351,#13829,#2830,.T.);
#19304=EDGE_CURVE('',#13830,#14352,#2831,.T.);
#19305=EDGE_CURVE('',#14353,#13833,#2832,.T.);
#19306=EDGE_CURVE('',#13834,#14354,#2833,.T.);
#19307=EDGE_CURVE('',#14355,#13837,#2834,.T.);
#19308=EDGE_CURVE('',#13838,#14356,#2835,.T.);
#19309=EDGE_CURVE('',#14357,#13841,#2836,.T.);
#19310=EDGE_CURVE('',#13842,#14358,#2837,.T.);
#19311=EDGE_CURVE('',#14359,#13845,#2838,.T.);
#19312=EDGE_CURVE('',#13846,#14360,#2839,.T.);
#19313=EDGE_CURVE('',#14361,#13849,#2840,.T.);
#19314=EDGE_CURVE('',#13850,#14362,#2841,.T.);
#19315=EDGE_CURVE('',#14363,#13853,#2842,.T.);
#19316=EDGE_CURVE('',#13854,#14364,#2843,.T.);
#19317=EDGE_CURVE('',#14365,#13857,#2844,.T.);
#19318=EDGE_CURVE('',#13858,#14366,#2845,.T.);
#19319=EDGE_CURVE('',#14367,#13571,#2846,.T.);
#19320=EDGE_CURVE('',#13572,#14368,#2847,.T.);
#19321=EDGE_CURVE('',#14369,#13575,#2848,.T.);
#19322=EDGE_CURVE('',#13576,#14370,#2849,.T.);
#19323=EDGE_CURVE('',#14371,#13579,#2850,.T.);
#19324=EDGE_CURVE('',#13580,#14372,#2851,.T.);
#19325=EDGE_CURVE('',#14373,#13583,#2852,.T.);
#19326=EDGE_CURVE('',#13584,#14374,#2853,.T.);
#19327=EDGE_CURVE('',#14375,#13587,#2854,.T.);
#19328=EDGE_CURVE('',#13588,#14376,#2855,.T.);
#19329=EDGE_CURVE('',#14377,#13591,#2856,.T.);
#19330=EDGE_CURVE('',#13592,#14378,#2857,.T.);
#19331=EDGE_CURVE('',#14379,#13595,#2858,.T.);
#19332=EDGE_CURVE('',#13596,#14380,#2859,.T.);
#19333=EDGE_CURVE('',#14381,#13599,#2860,.T.);
#19334=EDGE_CURVE('',#13600,#14382,#2861,.T.);
#19335=EDGE_CURVE('',#14383,#13603,#2862,.T.);
#19336=EDGE_CURVE('',#13604,#14384,#2863,.T.);
#19337=EDGE_CURVE('',#14385,#13607,#2864,.T.);
#19338=EDGE_CURVE('',#13608,#14386,#2865,.T.);
#19339=EDGE_CURVE('',#14387,#13611,#2866,.T.);
#19340=EDGE_CURVE('',#13612,#14388,#2867,.T.);
#19341=EDGE_CURVE('',#14389,#13615,#2868,.T.);
#19342=EDGE_CURVE('',#13616,#14390,#2869,.T.);
#19343=EDGE_CURVE('',#14391,#13619,#2870,.T.);
#19344=EDGE_CURVE('',#13620,#14392,#2871,.T.);
#19345=EDGE_CURVE('',#14393,#13623,#2872,.T.);
#19346=EDGE_CURVE('',#13624,#14394,#2873,.T.);
#19347=EDGE_CURVE('',#14395,#13627,#2874,.T.);
#19348=EDGE_CURVE('',#13628,#14396,#2875,.T.);
#19349=EDGE_CURVE('',#14397,#13631,#2876,.T.);
#19350=EDGE_CURVE('',#13632,#14398,#2877,.T.);
#19351=EDGE_CURVE('',#14399,#13635,#2878,.T.);
#19352=EDGE_CURVE('',#13636,#14400,#2879,.T.);
#19353=EDGE_CURVE('',#14401,#13639,#2880,.T.);
#19354=EDGE_CURVE('',#13640,#14402,#2881,.T.);
#19355=EDGE_CURVE('',#14403,#13643,#2882,.T.);
#19356=EDGE_CURVE('',#13644,#14404,#2883,.T.);
#19357=EDGE_CURVE('',#14405,#13647,#2884,.T.);
#19358=EDGE_CURVE('',#13648,#14406,#2885,.T.);
#19359=EDGE_CURVE('',#14407,#13651,#2886,.T.);
#19360=EDGE_CURVE('',#13652,#14408,#2887,.T.);
#19361=EDGE_CURVE('',#14409,#13655,#2888,.T.);
#19362=EDGE_CURVE('',#13656,#14410,#2889,.T.);
#19363=EDGE_CURVE('',#14411,#13659,#2890,.T.);
#19364=EDGE_CURVE('',#13660,#14412,#2891,.T.);
#19365=EDGE_CURVE('',#14413,#13663,#2892,.T.);
#19366=EDGE_CURVE('',#13664,#14414,#2893,.T.);
#19367=EDGE_CURVE('',#14415,#13667,#2894,.T.);
#19368=EDGE_CURVE('',#13668,#14416,#2895,.T.);
#19369=EDGE_CURVE('',#14417,#13671,#2896,.T.);
#19370=EDGE_CURVE('',#13672,#14418,#2897,.T.);
#19371=EDGE_CURVE('',#14419,#13675,#2898,.T.);
#19372=EDGE_CURVE('',#13676,#14420,#2899,.T.);
#19373=EDGE_CURVE('',#14421,#13679,#2900,.T.);
#19374=EDGE_CURVE('',#13680,#14422,#2901,.T.);
#19375=EDGE_CURVE('',#14423,#13683,#2902,.T.);
#19376=EDGE_CURVE('',#13684,#14424,#2903,.T.);
#19377=EDGE_CURVE('',#14425,#13687,#2904,.T.);
#19378=EDGE_CURVE('',#13688,#14426,#2905,.T.);
#19379=EDGE_CURVE('',#14427,#13691,#2906,.T.);
#19380=EDGE_CURVE('',#13692,#14428,#2907,.T.);
#19381=EDGE_CURVE('',#14429,#13695,#2908,.T.);
#19382=EDGE_CURVE('',#13696,#14430,#2909,.T.);
#19383=EDGE_CURVE('',#14431,#13699,#2910,.T.);
#19384=EDGE_CURVE('',#13700,#14432,#2911,.T.);
#19385=EDGE_CURVE('',#14433,#13703,#2912,.T.);
#19386=EDGE_CURVE('',#13704,#14434,#2913,.T.);
#19387=EDGE_CURVE('',#14435,#13707,#2914,.T.);
#19388=EDGE_CURVE('',#13708,#14436,#2915,.T.);
#19389=EDGE_CURVE('',#14437,#13711,#2916,.T.);
#19390=EDGE_CURVE('',#13712,#14438,#2917,.T.);
#19391=EDGE_CURVE('',#14439,#13715,#2918,.T.);
#19392=EDGE_CURVE('',#13716,#14440,#2919,.T.);
#19393=EDGE_CURVE('',#14441,#13719,#2920,.T.);
#19394=EDGE_CURVE('',#13720,#14442,#2921,.T.);
#19395=EDGE_CURVE('',#13768,#14443,#2922,.T.);
#19396=EDGE_CURVE('',#14444,#13767,#2923,.T.);
#19397=EDGE_CURVE('',#13766,#14445,#2924,.T.);
#19398=EDGE_CURVE('',#14446,#13765,#2925,.T.);
#19399=EDGE_CURVE('',#13764,#14447,#2926,.T.);
#19400=EDGE_CURVE('',#14448,#13763,#2927,.T.);
#19401=EDGE_CURVE('',#13762,#14449,#2928,.T.);
#19402=EDGE_CURVE('',#14450,#13761,#2929,.T.);
#19403=EDGE_CURVE('',#13760,#14451,#2930,.T.);
#19404=EDGE_CURVE('',#14452,#13759,#2931,.T.);
#19405=EDGE_CURVE('',#13758,#14453,#2932,.T.);
#19406=EDGE_CURVE('',#14454,#13757,#2933,.T.);
#19407=EDGE_CURVE('',#13756,#14455,#2934,.T.);
#19408=EDGE_CURVE('',#14456,#13755,#2935,.T.);
#19409=EDGE_CURVE('',#13754,#14457,#2936,.T.);
#19410=EDGE_CURVE('',#14458,#13753,#2937,.T.);
#19411=EDGE_CURVE('',#13752,#14459,#2938,.T.);
#19412=EDGE_CURVE('',#14460,#13751,#2939,.T.);
#19413=EDGE_CURVE('',#13748,#14461,#2940,.T.);
#19414=EDGE_CURVE('',#14462,#13747,#2941,.T.);
#19415=EDGE_CURVE('',#13744,#14463,#2942,.T.);
#19416=EDGE_CURVE('',#14464,#13743,#2943,.T.);
#19417=EDGE_CURVE('',#13740,#14465,#2944,.T.);
#19418=EDGE_CURVE('',#14466,#13739,#2945,.T.);
#19419=EDGE_CURVE('',#13736,#14467,#2946,.T.);
#19420=EDGE_CURVE('',#14468,#13735,#2947,.T.);
#19421=EDGE_CURVE('',#13732,#14469,#2948,.T.);
#19422=EDGE_CURVE('',#14470,#13731,#2949,.T.);
#19423=EDGE_CURVE('',#14471,#13723,#2950,.T.);
#19424=EDGE_CURVE('',#13724,#14472,#2951,.T.);
#19425=EDGE_CURVE('',#13863,#14473,#2952,.T.);
#19426=EDGE_CURVE('',#14474,#13862,#2953,.T.);
#19427=EDGE_CURVE('',#14474,#14473,#4453,.T.);
#19428=EDGE_CURVE('',#14473,#14475,#9702,.T.);
#19429=EDGE_CURVE('',#14476,#14474,#9703,.T.);
#19430=EDGE_CURVE('',#14476,#14475,#4454,.T.);
#19431=EDGE_CURVE('',#14475,#13727,#2954,.T.);
#19432=EDGE_CURVE('',#13728,#14476,#2955,.T.);
#19433=EDGE_CURVE('',#14477,#14478,#9704,.T.);
#19434=EDGE_CURVE('',#14478,#14479,#9705,.T.);
#19435=EDGE_CURVE('',#14479,#14480,#9706,.T.);
#19436=EDGE_CURVE('',#14480,#14481,#9707,.T.);
#19437=EDGE_CURVE('',#14481,#14482,#9708,.T.);
#19438=EDGE_CURVE('',#14482,#14477,#9709,.T.);
#19439=EDGE_CURVE('',#14478,#13563,#9710,.T.);
#19440=EDGE_CURVE('',#14479,#13562,#9711,.T.);
#19441=EDGE_CURVE('',#14480,#13561,#9712,.T.);
#19442=EDGE_CURVE('',#14481,#13559,#9713,.T.);
#19443=EDGE_CURVE('',#14482,#13565,#9714,.T.);
#19444=EDGE_CURVE('',#14477,#13564,#9715,.T.);
#19445=EDGE_CURVE('',#13496,#13378,#3351,.T.);
#19446=EDGE_CURVE('',#13376,#13494,#9716,.T.);
#19447=EDGE_CURVE('',#13860,#13729,#9717,.T.);
#19448=EDGE_CURVE('',#14150,#13730,#9718,.T.);
#19449=EDGE_CURVE('',#13865,#13725,#9719,.T.);
#19450=EDGE_CURVE('',#13864,#13726,#9720,.T.);
#19451=EDGE_CURVE('',#14147,#13733,#9721,.T.);
#19452=EDGE_CURVE('',#14146,#13734,#9722,.T.);
#19453=EDGE_CURVE('',#14143,#13737,#9723,.T.);
#19454=EDGE_CURVE('',#14142,#13738,#9724,.T.);
#19455=EDGE_CURVE('',#14139,#13741,#9725,.T.);
#19456=EDGE_CURVE('',#14138,#13742,#9726,.T.);
#19457=EDGE_CURVE('',#14135,#13745,#9727,.T.);
#19458=EDGE_CURVE('',#14134,#13746,#9728,.T.);
#19459=EDGE_CURVE('',#14131,#13749,#9729,.T.);
#19460=EDGE_CURVE('',#14130,#13750,#9730,.T.);
#19461=EDGE_CURVE('',#13869,#13721,#9731,.T.);
#19462=EDGE_CURVE('',#13868,#13722,#9732,.T.);
#19463=EDGE_CURVE('',#13873,#13717,#9733,.T.);
#19464=EDGE_CURVE('',#13872,#13718,#9734,.T.);
#19465=EDGE_CURVE('',#13877,#13713,#9735,.T.);
#19466=EDGE_CURVE('',#13876,#13714,#9736,.T.);
#19467=EDGE_CURVE('',#13881,#13709,#9737,.T.);
#19468=EDGE_CURVE('',#13880,#13710,#9738,.T.);
#19469=EDGE_CURVE('',#13885,#13705,#9739,.T.);
#19470=EDGE_CURVE('',#13884,#13706,#9740,.T.);
#19471=EDGE_CURVE('',#13889,#13701,#9741,.T.);
#19472=EDGE_CURVE('',#13888,#13702,#9742,.T.);
#19473=EDGE_CURVE('',#13893,#13697,#9743,.T.);
#19474=EDGE_CURVE('',#13892,#13698,#9744,.T.);
#19475=EDGE_CURVE('',#13897,#13693,#9745,.T.);
#19476=EDGE_CURVE('',#13896,#13694,#9746,.T.);
#19477=EDGE_CURVE('',#13901,#13689,#9747,.T.);
#19478=EDGE_CURVE('',#13900,#13690,#9748,.T.);
#19479=EDGE_CURVE('',#13905,#13685,#9749,.T.);
#19480=EDGE_CURVE('',#13904,#13686,#9750,.T.);
#19481=EDGE_CURVE('',#13909,#13681,#9751,.T.);
#19482=EDGE_CURVE('',#13908,#13682,#9752,.T.);
#19483=EDGE_CURVE('',#13913,#13677,#9753,.T.);
#19484=EDGE_CURVE('',#13912,#13678,#9754,.T.);
#19485=EDGE_CURVE('',#13917,#13673,#9755,.T.);
#19486=EDGE_CURVE('',#13916,#13674,#9756,.T.);
#19487=EDGE_CURVE('',#13921,#13669,#9757,.T.);
#19488=EDGE_CURVE('',#13920,#13670,#9758,.T.);
#19489=EDGE_CURVE('',#13925,#13665,#9759,.T.);
#19490=EDGE_CURVE('',#13924,#13666,#9760,.T.);
#19491=EDGE_CURVE('',#13929,#13661,#9761,.T.);
#19492=EDGE_CURVE('',#13928,#13662,#9762,.T.);
#19493=EDGE_CURVE('',#13933,#13657,#9763,.T.);
#19494=EDGE_CURVE('',#13932,#13658,#9764,.T.);
#19495=EDGE_CURVE('',#13937,#13653,#9765,.T.);
#19496=EDGE_CURVE('',#13936,#13654,#9766,.T.);
#19497=EDGE_CURVE('',#13941,#13649,#9767,.T.);
#19498=EDGE_CURVE('',#13940,#13650,#9768,.T.);
#19499=EDGE_CURVE('',#13945,#13645,#9769,.T.);
#19500=EDGE_CURVE('',#13944,#13646,#9770,.T.);
#19501=EDGE_CURVE('',#13949,#13641,#9771,.T.);
#19502=EDGE_CURVE('',#13948,#13642,#9772,.T.);
#19503=EDGE_CURVE('',#13953,#13637,#9773,.T.);
#19504=EDGE_CURVE('',#13952,#13638,#9774,.T.);
#19505=EDGE_CURVE('',#13957,#13633,#9775,.T.);
#19506=EDGE_CURVE('',#13956,#13634,#9776,.T.);
#19507=EDGE_CURVE('',#13961,#13629,#9777,.T.);
#19508=EDGE_CURVE('',#13960,#13630,#9778,.T.);
#19509=EDGE_CURVE('',#13965,#13625,#9779,.T.);
#19510=EDGE_CURVE('',#13964,#13626,#9780,.T.);
#19511=EDGE_CURVE('',#13969,#13621,#9781,.T.);
#19512=EDGE_CURVE('',#13968,#13622,#9782,.T.);
#19513=EDGE_CURVE('',#13973,#13617,#9783,.T.);
#19514=EDGE_CURVE('',#13972,#13618,#9784,.T.);
#19515=EDGE_CURVE('',#13977,#13613,#9785,.T.);
#19516=EDGE_CURVE('',#13976,#13614,#9786,.T.);
#19517=EDGE_CURVE('',#13981,#13609,#9787,.T.);
#19518=EDGE_CURVE('',#13980,#13610,#9788,.T.);
#19519=EDGE_CURVE('',#13985,#13605,#9789,.T.);
#19520=EDGE_CURVE('',#13984,#13606,#9790,.T.);
#19521=EDGE_CURVE('',#13989,#13601,#9791,.T.);
#19522=EDGE_CURVE('',#13988,#13602,#9792,.T.);
#19523=EDGE_CURVE('',#13993,#13597,#9793,.T.);
#19524=EDGE_CURVE('',#13992,#13598,#9794,.T.);
#19525=EDGE_CURVE('',#13997,#13593,#9795,.T.);
#19526=EDGE_CURVE('',#13996,#13594,#9796,.T.);
#19527=EDGE_CURVE('',#14001,#13589,#9797,.T.);
#19528=EDGE_CURVE('',#14000,#13590,#9798,.T.);
#19529=EDGE_CURVE('',#14005,#13585,#9799,.T.);
#19530=EDGE_CURVE('',#14004,#13586,#9800,.T.);
#19531=EDGE_CURVE('',#14009,#13581,#9801,.T.);
#19532=EDGE_CURVE('',#14008,#13582,#9802,.T.);
#19533=EDGE_CURVE('',#14013,#13577,#9803,.T.);
#19534=EDGE_CURVE('',#14012,#13578,#9804,.T.);
#19535=EDGE_CURVE('',#14017,#13573,#9805,.T.);
#19536=EDGE_CURVE('',#14016,#13574,#9806,.T.);
#19537=EDGE_CURVE('',#14021,#13859,#9807,.T.);
#19538=EDGE_CURVE('',#14020,#13569,#9808,.T.);
#19539=EDGE_CURVE('',#14025,#13855,#9809,.T.);
#19540=EDGE_CURVE('',#14024,#13856,#9810,.T.);
#19541=EDGE_CURVE('',#14029,#13851,#9811,.T.);
#19542=EDGE_CURVE('',#14028,#13852,#9812,.T.);
#19543=EDGE_CURVE('',#14033,#13847,#9813,.T.);
#19544=EDGE_CURVE('',#14032,#13848,#9814,.T.);
#19545=EDGE_CURVE('',#14037,#13843,#9815,.T.);
#19546=EDGE_CURVE('',#14036,#13844,#9816,.T.);
#19547=EDGE_CURVE('',#14041,#13839,#9817,.T.);
#19548=EDGE_CURVE('',#14040,#13840,#9818,.T.);
#19549=EDGE_CURVE('',#14045,#13835,#9819,.T.);
#19550=EDGE_CURVE('',#14044,#13836,#9820,.T.);
#19551=EDGE_CURVE('',#14049,#13831,#9821,.T.);
#19552=EDGE_CURVE('',#14048,#13832,#9822,.T.);
#19553=EDGE_CURVE('',#14053,#13827,#9823,.T.);
#19554=EDGE_CURVE('',#14052,#13828,#9824,.T.);
#19555=EDGE_CURVE('',#14057,#13823,#9825,.T.);
#19556=EDGE_CURVE('',#14056,#13824,#9826,.T.);
#19557=EDGE_CURVE('',#14061,#13819,#9827,.T.);
#19558=EDGE_CURVE('',#14060,#13820,#9828,.T.);
#19559=EDGE_CURVE('',#14065,#13815,#9829,.T.);
#19560=EDGE_CURVE('',#14064,#13816,#9830,.T.);
#19561=EDGE_CURVE('',#14069,#13811,#9831,.T.);
#19562=EDGE_CURVE('',#14068,#13812,#9832,.T.);
#19563=EDGE_CURVE('',#14073,#13807,#9833,.T.);
#19564=EDGE_CURVE('',#14072,#13808,#9834,.T.);
#19565=EDGE_CURVE('',#14077,#13803,#9835,.T.);
#19566=EDGE_CURVE('',#14076,#13804,#9836,.T.);
#19567=EDGE_CURVE('',#14081,#13799,#9837,.T.);
#19568=EDGE_CURVE('',#14080,#13800,#9838,.T.);
#19569=EDGE_CURVE('',#14085,#13795,#9839,.T.);
#19570=EDGE_CURVE('',#14084,#13796,#9840,.T.);
#19571=EDGE_CURVE('',#14089,#13791,#9841,.T.);
#19572=EDGE_CURVE('',#14088,#13792,#9842,.T.);
#19573=EDGE_CURVE('',#14093,#13787,#9843,.T.);
#19574=EDGE_CURVE('',#14092,#13788,#9844,.T.);
#19575=EDGE_CURVE('',#14097,#13783,#9845,.T.);
#19576=EDGE_CURVE('',#14096,#13784,#9846,.T.);
#19577=ORIENTED_EDGE('',*,*,#14483,.F.);
#19578=ORIENTED_EDGE('',*,*,#14484,.F.);
#19579=ORIENTED_EDGE('',*,*,#14485,.T.);
#19580=ORIENTED_EDGE('',*,*,#14486,.F.);
#19581=ORIENTED_EDGE('',*,*,#14487,.T.);
#19582=ORIENTED_EDGE('',*,*,#14488,.F.);
#19583=ORIENTED_EDGE('',*,*,#14489,.T.);
#19584=ORIENTED_EDGE('',*,*,#14490,.F.);
#19585=ORIENTED_EDGE('',*,*,#14491,.F.);
#19586=ORIENTED_EDGE('',*,*,#14490,.T.);
#19587=ORIENTED_EDGE('',*,*,#14492,.T.);
#19588=ORIENTED_EDGE('',*,*,#14493,.F.);
#19589=ORIENTED_EDGE('',*,*,#14492,.F.);
#19590=ORIENTED_EDGE('',*,*,#14489,.F.);
#19591=ORIENTED_EDGE('',*,*,#14494,.F.);
#19592=ORIENTED_EDGE('',*,*,#14487,.F.);
#19593=ORIENTED_EDGE('',*,*,#14486,.T.);
#19594=ORIENTED_EDGE('',*,*,#14495,.T.);
#19595=ORIENTED_EDGE('',*,*,#14496,.F.);
#19596=ORIENTED_EDGE('',*,*,#14495,.F.);
#19597=ORIENTED_EDGE('',*,*,#14485,.F.);
#19598=ORIENTED_EDGE('',*,*,#14497,.F.);
#19599=ORIENTED_EDGE('',*,*,#14483,.T.);
#19600=ORIENTED_EDGE('',*,*,#14498,.T.);
#19601=ORIENTED_EDGE('',*,*,#14499,.T.);
#19602=ORIENTED_EDGE('',*,*,#14500,.F.);
#19603=ORIENTED_EDGE('',*,*,#14491,.T.);
#19604=ORIENTED_EDGE('',*,*,#14501,.F.);
#19605=ORIENTED_EDGE('',*,*,#14502,.T.);
#19606=ORIENTED_EDGE('',*,*,#14498,.F.);
#19607=ORIENTED_EDGE('',*,*,#14499,.F.);
#19608=ORIENTED_EDGE('',*,*,#14502,.F.);
#19609=ORIENTED_EDGE('',*,*,#14503,.F.);
#19610=ORIENTED_EDGE('',*,*,#14504,.F.);
#19611=ORIENTED_EDGE('',*,*,#14505,.T.);
#19612=ORIENTED_EDGE('',*,*,#14506,.T.);
#19613=ORIENTED_EDGE('',*,*,#14505,.F.);
#19614=ORIENTED_EDGE('',*,*,#14504,.T.);
#19615=ORIENTED_EDGE('',*,*,#14484,.T.);
#19616=ORIENTED_EDGE('',*,*,#14500,.T.);
#19617=ORIENTED_EDGE('',*,*,#14503,.T.);
#19618=ORIENTED_EDGE('',*,*,#14501,.T.);
#19619=ORIENTED_EDGE('',*,*,#14493,.T.);
#19620=ORIENTED_EDGE('',*,*,#14494,.T.);
#19621=ORIENTED_EDGE('',*,*,#14488,.T.);
#19622=ORIENTED_EDGE('',*,*,#14496,.T.);
#19623=ORIENTED_EDGE('',*,*,#14497,.T.);
#19624=ORIENTED_EDGE('',*,*,#14506,.F.);
#19625=ORIENTED_EDGE('',*,*,#14507,.T.);
#19626=ORIENTED_EDGE('',*,*,#14507,.F.);
#19627=ORIENTED_EDGE('',*,*,#14508,.T.);
#19628=ORIENTED_EDGE('',*,*,#14508,.F.);
#19629=ORIENTED_EDGE('',*,*,#14509,.T.);
#19630=ORIENTED_EDGE('',*,*,#14509,.F.);
#19631=ORIENTED_EDGE('',*,*,#14510,.F.);
#19632=ORIENTED_EDGE('',*,*,#14511,.T.);
#19633=ORIENTED_EDGE('',*,*,#14512,.F.);
#19634=ORIENTED_EDGE('',*,*,#14511,.F.);
#19635=ORIENTED_EDGE('',*,*,#14513,.F.);
#19636=ORIENTED_EDGE('',*,*,#14514,.T.);
#19637=ORIENTED_EDGE('',*,*,#14515,.F.);
#19638=ORIENTED_EDGE('',*,*,#14514,.F.);
#19639=ORIENTED_EDGE('',*,*,#14516,.F.);
#19640=ORIENTED_EDGE('',*,*,#14517,.T.);
#19641=ORIENTED_EDGE('',*,*,#14518,.F.);
#19642=ORIENTED_EDGE('',*,*,#14517,.F.);
#19643=ORIENTED_EDGE('',*,*,#14519,.T.);
#19644=ORIENTED_EDGE('',*,*,#14520,.T.);
#19645=ORIENTED_EDGE('',*,*,#14521,.T.);
#19646=ORIENTED_EDGE('',*,*,#14522,.T.);
#19647=ORIENTED_EDGE('',*,*,#14520,.F.);
#19648=ORIENTED_EDGE('',*,*,#14523,.T.);
#19649=ORIENTED_EDGE('',*,*,#14524,.F.);
#19650=ORIENTED_EDGE('',*,*,#14525,.F.);
#19651=ORIENTED_EDGE('',*,*,#14526,.T.);
#19652=ORIENTED_EDGE('',*,*,#14527,.T.);
#19653=ORIENTED_EDGE('',*,*,#14528,.T.);
#19654=ORIENTED_EDGE('',*,*,#14529,.T.);
#19655=ORIENTED_EDGE('',*,*,#14527,.F.);
#19656=ORIENTED_EDGE('',*,*,#14530,.T.);
#19657=ORIENTED_EDGE('',*,*,#14531,.F.);
#19658=ORIENTED_EDGE('',*,*,#14532,.F.);
#19659=ORIENTED_EDGE('',*,*,#14533,.T.);
#19660=ORIENTED_EDGE('',*,*,#14534,.T.);
#19661=ORIENTED_EDGE('',*,*,#14535,.T.);
#19662=ORIENTED_EDGE('',*,*,#14536,.T.);
#19663=ORIENTED_EDGE('',*,*,#14534,.F.);
#19664=ORIENTED_EDGE('',*,*,#14537,.T.);
#19665=ORIENTED_EDGE('',*,*,#14538,.F.);
#19666=ORIENTED_EDGE('',*,*,#14539,.F.);
#19667=ORIENTED_EDGE('',*,*,#14540,.T.);
#19668=ORIENTED_EDGE('',*,*,#14541,.T.);
#19669=ORIENTED_EDGE('',*,*,#14542,.T.);
#19670=ORIENTED_EDGE('',*,*,#14543,.T.);
#19671=ORIENTED_EDGE('',*,*,#14541,.F.);
#19672=ORIENTED_EDGE('',*,*,#14544,.F.);
#19673=ORIENTED_EDGE('',*,*,#14545,.F.);
#19674=ORIENTED_EDGE('',*,*,#14546,.T.);
#19675=ORIENTED_EDGE('',*,*,#14540,.F.);
#19676=ORIENTED_EDGE('',*,*,#14547,.T.);
#19677=ORIENTED_EDGE('',*,*,#14528,.F.);
#19678=ORIENTED_EDGE('',*,*,#14532,.T.);
#19679=ORIENTED_EDGE('',*,*,#14548,.F.);
#19680=ORIENTED_EDGE('',*,*,#14549,.T.);
#19681=ORIENTED_EDGE('',*,*,#14550,.F.);
#19682=ORIENTED_EDGE('',*,*,#14551,.T.);
#19683=ORIENTED_EDGE('',*,*,#14521,.F.);
#19684=ORIENTED_EDGE('',*,*,#14525,.T.);
#19685=ORIENTED_EDGE('',*,*,#14552,.F.);
#19686=ORIENTED_EDGE('',*,*,#14553,.T.);
#19687=ORIENTED_EDGE('',*,*,#14554,.F.);
#19688=ORIENTED_EDGE('',*,*,#14555,.T.);
#19689=ORIENTED_EDGE('',*,*,#14535,.F.);
#19690=ORIENTED_EDGE('',*,*,#14539,.T.);
#19691=ORIENTED_EDGE('',*,*,#14556,.F.);
#19692=ORIENTED_EDGE('',*,*,#14544,.T.);
#19693=ORIENTED_EDGE('',*,*,#14510,.T.);
#19694=ORIENTED_EDGE('',*,*,#14513,.T.);
#19695=ORIENTED_EDGE('',*,*,#14516,.T.);
#19696=ORIENTED_EDGE('',*,*,#14548,.T.);
#19697=ORIENTED_EDGE('',*,*,#14531,.T.);
#19698=ORIENTED_EDGE('',*,*,#14557,.T.);
#19699=ORIENTED_EDGE('',*,*,#14558,.T.);
#19700=ORIENTED_EDGE('',*,*,#14558,.F.);
#19701=ORIENTED_EDGE('',*,*,#14559,.T.);
#19702=ORIENTED_EDGE('',*,*,#14560,.F.);
#19703=ORIENTED_EDGE('',*,*,#14549,.F.);
#19704=ORIENTED_EDGE('',*,*,#14550,.T.);
#19705=ORIENTED_EDGE('',*,*,#14560,.T.);
#19706=ORIENTED_EDGE('',*,*,#14561,.T.);
#19707=ORIENTED_EDGE('',*,*,#14562,.T.);
#19708=ORIENTED_EDGE('',*,*,#14552,.T.);
#19709=ORIENTED_EDGE('',*,*,#14524,.T.);
#19710=ORIENTED_EDGE('',*,*,#14563,.T.);
#19711=ORIENTED_EDGE('',*,*,#14564,.T.);
#19712=ORIENTED_EDGE('',*,*,#14556,.T.);
#19713=ORIENTED_EDGE('',*,*,#14538,.T.);
#19714=ORIENTED_EDGE('',*,*,#14565,.T.);
#19715=ORIENTED_EDGE('',*,*,#14545,.T.);
#19716=ORIENTED_EDGE('',*,*,#14554,.T.);
#19717=ORIENTED_EDGE('',*,*,#14566,.T.);
#19718=ORIENTED_EDGE('',*,*,#14567,.T.);
#19719=ORIENTED_EDGE('',*,*,#14568,.T.);
#19720=ORIENTED_EDGE('',*,*,#14536,.F.);
#19721=ORIENTED_EDGE('',*,*,#14555,.F.);
#19722=ORIENTED_EDGE('',*,*,#14568,.F.);
#19723=ORIENTED_EDGE('',*,*,#14569,.T.);
#19724=ORIENTED_EDGE('',*,*,#14564,.F.);
#19725=ORIENTED_EDGE('',*,*,#14570,.T.);
#19726=ORIENTED_EDGE('',*,*,#14566,.F.);
#19727=ORIENTED_EDGE('',*,*,#14553,.F.);
#19728=ORIENTED_EDGE('',*,*,#14522,.F.);
#19729=ORIENTED_EDGE('',*,*,#14551,.F.);
#19730=ORIENTED_EDGE('',*,*,#14562,.F.);
#19731=ORIENTED_EDGE('',*,*,#14571,.T.);
#19732=ORIENTED_EDGE('',*,*,#14529,.F.);
#19733=ORIENTED_EDGE('',*,*,#14547,.F.);
#19734=ORIENTED_EDGE('',*,*,#14543,.F.);
#19735=ORIENTED_EDGE('',*,*,#14572,.T.);
#19736=ORIENTED_EDGE('',*,*,#14542,.F.);
#19737=ORIENTED_EDGE('',*,*,#14546,.F.);
#19738=ORIENTED_EDGE('',*,*,#14565,.F.);
#19739=ORIENTED_EDGE('',*,*,#14537,.F.);
#19740=ORIENTED_EDGE('',*,*,#14533,.F.);
#19741=ORIENTED_EDGE('',*,*,#14569,.F.);
#19742=ORIENTED_EDGE('',*,*,#14567,.F.);
#19743=ORIENTED_EDGE('',*,*,#14570,.F.);
#19744=ORIENTED_EDGE('',*,*,#14563,.F.);
#19745=ORIENTED_EDGE('',*,*,#14523,.F.);
#19746=ORIENTED_EDGE('',*,*,#14519,.F.);
#19747=ORIENTED_EDGE('',*,*,#14571,.F.);
#19748=ORIENTED_EDGE('',*,*,#14561,.F.);
#19749=ORIENTED_EDGE('',*,*,#14559,.F.);
#19750=ORIENTED_EDGE('',*,*,#14557,.F.);
#19751=ORIENTED_EDGE('',*,*,#14530,.F.);
#19752=ORIENTED_EDGE('',*,*,#14526,.F.);
#19753=ORIENTED_EDGE('',*,*,#14572,.F.);
#19754=ORIENTED_EDGE('',*,*,#14512,.T.);
#19755=ORIENTED_EDGE('',*,*,#14515,.T.);
#19756=ORIENTED_EDGE('',*,*,#14518,.T.);
#19757=ORIENTED_EDGE('',*,*,#14573,.F.);
#19758=ORIENTED_EDGE('',*,*,#14574,.F.);
#19759=ORIENTED_EDGE('',*,*,#14575,.T.);
#19760=ORIENTED_EDGE('',*,*,#14576,.T.);
#19761=ORIENTED_EDGE('',*,*,#14575,.F.);
#19762=ORIENTED_EDGE('',*,*,#14577,.F.);
#19763=ORIENTED_EDGE('',*,*,#14578,.F.);
#19764=ORIENTED_EDGE('',*,*,#14579,.F.);
#19765=ORIENTED_EDGE('',*,*,#14580,.F.);
#19766=ORIENTED_EDGE('',*,*,#14573,.T.);
#19767=ORIENTED_EDGE('',*,*,#14581,.F.);
#19768=ORIENTED_EDGE('',*,*,#14582,.F.);
#19769=ORIENTED_EDGE('',*,*,#14583,.F.);
#19770=ORIENTED_EDGE('',*,*,#14579,.T.);
#19771=ORIENTED_EDGE('',*,*,#14584,.F.);
#19772=ORIENTED_EDGE('',*,*,#14585,.F.);
#19773=ORIENTED_EDGE('',*,*,#14586,.F.);
#19774=ORIENTED_EDGE('',*,*,#14582,.T.);
#19775=ORIENTED_EDGE('',*,*,#14587,.F.);
#19776=ORIENTED_EDGE('',*,*,#14588,.F.);
#19777=ORIENTED_EDGE('',*,*,#14589,.F.);
#19778=ORIENTED_EDGE('',*,*,#14585,.T.);
#19779=ORIENTED_EDGE('',*,*,#14590,.F.);
#19780=ORIENTED_EDGE('',*,*,#14591,.F.);
#19781=ORIENTED_EDGE('',*,*,#14592,.F.);
#19782=ORIENTED_EDGE('',*,*,#14588,.T.);
#19783=ORIENTED_EDGE('',*,*,#14593,.F.);
#19784=ORIENTED_EDGE('',*,*,#14594,.F.);
#19785=ORIENTED_EDGE('',*,*,#14595,.F.);
#19786=ORIENTED_EDGE('',*,*,#14591,.T.);
#19787=ORIENTED_EDGE('',*,*,#14596,.F.);
#19788=ORIENTED_EDGE('',*,*,#14597,.F.);
#19789=ORIENTED_EDGE('',*,*,#14598,.F.);
#19790=ORIENTED_EDGE('',*,*,#14594,.T.);
#19791=ORIENTED_EDGE('',*,*,#14599,.F.);
#19792=ORIENTED_EDGE('',*,*,#14600,.F.);
#19793=ORIENTED_EDGE('',*,*,#14601,.F.);
#19794=ORIENTED_EDGE('',*,*,#14597,.T.);
#19795=ORIENTED_EDGE('',*,*,#14602,.F.);
#19796=ORIENTED_EDGE('',*,*,#14603,.F.);
#19797=ORIENTED_EDGE('',*,*,#14604,.F.);
#19798=ORIENTED_EDGE('',*,*,#14600,.T.);
#19799=ORIENTED_EDGE('',*,*,#14605,.F.);
#19800=ORIENTED_EDGE('',*,*,#14606,.F.);
#19801=ORIENTED_EDGE('',*,*,#14607,.F.);
#19802=ORIENTED_EDGE('',*,*,#14603,.T.);
#19803=ORIENTED_EDGE('',*,*,#14608,.F.);
#19804=ORIENTED_EDGE('',*,*,#14609,.F.);
#19805=ORIENTED_EDGE('',*,*,#14610,.F.);
#19806=ORIENTED_EDGE('',*,*,#14606,.T.);
#19807=ORIENTED_EDGE('',*,*,#14611,.F.);
#19808=ORIENTED_EDGE('',*,*,#14612,.F.);
#19809=ORIENTED_EDGE('',*,*,#14613,.F.);
#19810=ORIENTED_EDGE('',*,*,#14609,.T.);
#19811=ORIENTED_EDGE('',*,*,#14614,.F.);
#19812=ORIENTED_EDGE('',*,*,#14615,.F.);
#19813=ORIENTED_EDGE('',*,*,#14616,.F.);
#19814=ORIENTED_EDGE('',*,*,#14612,.T.);
#19815=ORIENTED_EDGE('',*,*,#14617,.F.);
#19816=ORIENTED_EDGE('',*,*,#14618,.F.);
#19817=ORIENTED_EDGE('',*,*,#14619,.F.);
#19818=ORIENTED_EDGE('',*,*,#14615,.T.);
#19819=ORIENTED_EDGE('',*,*,#14620,.F.);
#19820=ORIENTED_EDGE('',*,*,#14621,.F.);
#19821=ORIENTED_EDGE('',*,*,#14622,.F.);
#19822=ORIENTED_EDGE('',*,*,#14618,.T.);
#19823=ORIENTED_EDGE('',*,*,#14623,.F.);
#19824=ORIENTED_EDGE('',*,*,#14624,.F.);
#19825=ORIENTED_EDGE('',*,*,#14625,.F.);
#19826=ORIENTED_EDGE('',*,*,#14621,.T.);
#19827=ORIENTED_EDGE('',*,*,#14626,.F.);
#19828=ORIENTED_EDGE('',*,*,#14627,.F.);
#19829=ORIENTED_EDGE('',*,*,#14628,.F.);
#19830=ORIENTED_EDGE('',*,*,#14624,.T.);
#19831=ORIENTED_EDGE('',*,*,#14629,.F.);
#19832=ORIENTED_EDGE('',*,*,#14630,.F.);
#19833=ORIENTED_EDGE('',*,*,#14631,.F.);
#19834=ORIENTED_EDGE('',*,*,#14627,.T.);
#19835=ORIENTED_EDGE('',*,*,#14632,.F.);
#19836=ORIENTED_EDGE('',*,*,#14633,.F.);
#19837=ORIENTED_EDGE('',*,*,#14634,.F.);
#19838=ORIENTED_EDGE('',*,*,#14630,.T.);
#19839=ORIENTED_EDGE('',*,*,#14635,.F.);
#19840=ORIENTED_EDGE('',*,*,#14636,.F.);
#19841=ORIENTED_EDGE('',*,*,#14637,.F.);
#19842=ORIENTED_EDGE('',*,*,#14633,.T.);
#19843=ORIENTED_EDGE('',*,*,#14638,.F.);
#19844=ORIENTED_EDGE('',*,*,#14639,.F.);
#19845=ORIENTED_EDGE('',*,*,#14640,.F.);
#19846=ORIENTED_EDGE('',*,*,#14636,.T.);
#19847=ORIENTED_EDGE('',*,*,#14641,.F.);
#19848=ORIENTED_EDGE('',*,*,#14642,.F.);
#19849=ORIENTED_EDGE('',*,*,#14643,.F.);
#19850=ORIENTED_EDGE('',*,*,#14639,.T.);
#19851=ORIENTED_EDGE('',*,*,#14644,.F.);
#19852=ORIENTED_EDGE('',*,*,#14645,.F.);
#19853=ORIENTED_EDGE('',*,*,#14646,.F.);
#19854=ORIENTED_EDGE('',*,*,#14642,.T.);
#19855=ORIENTED_EDGE('',*,*,#14647,.F.);
#19856=ORIENTED_EDGE('',*,*,#14648,.F.);
#19857=ORIENTED_EDGE('',*,*,#14649,.F.);
#19858=ORIENTED_EDGE('',*,*,#14645,.T.);
#19859=ORIENTED_EDGE('',*,*,#14650,.F.);
#19860=ORIENTED_EDGE('',*,*,#14651,.F.);
#19861=ORIENTED_EDGE('',*,*,#14652,.F.);
#19862=ORIENTED_EDGE('',*,*,#14648,.T.);
#19863=ORIENTED_EDGE('',*,*,#14653,.F.);
#19864=ORIENTED_EDGE('',*,*,#14654,.F.);
#19865=ORIENTED_EDGE('',*,*,#14655,.F.);
#19866=ORIENTED_EDGE('',*,*,#14651,.T.);
#19867=ORIENTED_EDGE('',*,*,#14656,.F.);
#19868=ORIENTED_EDGE('',*,*,#14657,.F.);
#19869=ORIENTED_EDGE('',*,*,#14658,.F.);
#19870=ORIENTED_EDGE('',*,*,#14654,.T.);
#19871=ORIENTED_EDGE('',*,*,#14659,.F.);
#19872=ORIENTED_EDGE('',*,*,#14660,.F.);
#19873=ORIENTED_EDGE('',*,*,#14661,.T.);
#19874=ORIENTED_EDGE('',*,*,#14662,.F.);
#19875=ORIENTED_EDGE('',*,*,#14663,.F.);
#19876=ORIENTED_EDGE('',*,*,#14664,.F.);
#19877=ORIENTED_EDGE('',*,*,#14665,.F.);
#19878=ORIENTED_EDGE('',*,*,#14666,.F.);
#19879=ORIENTED_EDGE('',*,*,#14667,.F.);
#19880=ORIENTED_EDGE('',*,*,#14663,.T.);
#19881=ORIENTED_EDGE('',*,*,#14668,.T.);
#19882=ORIENTED_EDGE('',*,*,#14669,.F.);
#19883=ORIENTED_EDGE('',*,*,#14670,.F.);
#19884=ORIENTED_EDGE('',*,*,#14666,.T.);
#19885=ORIENTED_EDGE('',*,*,#14671,.T.);
#19886=ORIENTED_EDGE('',*,*,#14672,.F.);
#19887=ORIENTED_EDGE('',*,*,#14673,.F.);
#19888=ORIENTED_EDGE('',*,*,#14669,.T.);
#19889=ORIENTED_EDGE('',*,*,#14674,.T.);
#19890=ORIENTED_EDGE('',*,*,#14675,.F.);
#19891=ORIENTED_EDGE('',*,*,#14676,.F.);
#19892=ORIENTED_EDGE('',*,*,#14672,.T.);
#19893=ORIENTED_EDGE('',*,*,#14677,.T.);
#19894=ORIENTED_EDGE('',*,*,#14678,.F.);
#19895=ORIENTED_EDGE('',*,*,#14679,.F.);
#19896=ORIENTED_EDGE('',*,*,#14675,.T.);
#19897=ORIENTED_EDGE('',*,*,#14680,.T.);
#19898=ORIENTED_EDGE('',*,*,#14681,.F.);
#19899=ORIENTED_EDGE('',*,*,#14682,.F.);
#19900=ORIENTED_EDGE('',*,*,#14678,.T.);
#19901=ORIENTED_EDGE('',*,*,#14683,.T.);
#19902=ORIENTED_EDGE('',*,*,#14684,.F.);
#19903=ORIENTED_EDGE('',*,*,#14685,.F.);
#19904=ORIENTED_EDGE('',*,*,#14681,.T.);
#19905=ORIENTED_EDGE('',*,*,#14686,.T.);
#19906=ORIENTED_EDGE('',*,*,#14687,.F.);
#19907=ORIENTED_EDGE('',*,*,#14688,.F.);
#19908=ORIENTED_EDGE('',*,*,#14684,.T.);
#19909=ORIENTED_EDGE('',*,*,#14689,.T.);
#19910=ORIENTED_EDGE('',*,*,#14690,.F.);
#19911=ORIENTED_EDGE('',*,*,#14691,.F.);
#19912=ORIENTED_EDGE('',*,*,#14687,.T.);
#19913=ORIENTED_EDGE('',*,*,#14692,.T.);
#19914=ORIENTED_EDGE('',*,*,#14693,.F.);
#19915=ORIENTED_EDGE('',*,*,#14694,.F.);
#19916=ORIENTED_EDGE('',*,*,#14690,.T.);
#19917=ORIENTED_EDGE('',*,*,#14695,.T.);
#19918=ORIENTED_EDGE('',*,*,#14696,.F.);
#19919=ORIENTED_EDGE('',*,*,#14697,.F.);
#19920=ORIENTED_EDGE('',*,*,#14693,.T.);
#19921=ORIENTED_EDGE('',*,*,#14698,.T.);
#19922=ORIENTED_EDGE('',*,*,#14699,.F.);
#19923=ORIENTED_EDGE('',*,*,#14700,.F.);
#19924=ORIENTED_EDGE('',*,*,#14696,.T.);
#19925=ORIENTED_EDGE('',*,*,#14701,.T.);
#19926=ORIENTED_EDGE('',*,*,#14702,.F.);
#19927=ORIENTED_EDGE('',*,*,#14703,.F.);
#19928=ORIENTED_EDGE('',*,*,#14699,.T.);
#19929=ORIENTED_EDGE('',*,*,#14704,.T.);
#19930=ORIENTED_EDGE('',*,*,#14705,.F.);
#19931=ORIENTED_EDGE('',*,*,#14706,.F.);
#19932=ORIENTED_EDGE('',*,*,#14702,.T.);
#19933=ORIENTED_EDGE('',*,*,#14707,.T.);
#19934=ORIENTED_EDGE('',*,*,#14708,.F.);
#19935=ORIENTED_EDGE('',*,*,#14709,.F.);
#19936=ORIENTED_EDGE('',*,*,#14705,.T.);
#19937=ORIENTED_EDGE('',*,*,#14710,.T.);
#19938=ORIENTED_EDGE('',*,*,#14711,.F.);
#19939=ORIENTED_EDGE('',*,*,#14712,.F.);
#19940=ORIENTED_EDGE('',*,*,#14708,.T.);
#19941=ORIENTED_EDGE('',*,*,#14713,.T.);
#19942=ORIENTED_EDGE('',*,*,#14714,.F.);
#19943=ORIENTED_EDGE('',*,*,#14715,.F.);
#19944=ORIENTED_EDGE('',*,*,#14711,.T.);
#19945=ORIENTED_EDGE('',*,*,#14716,.T.);
#19946=ORIENTED_EDGE('',*,*,#14717,.F.);
#19947=ORIENTED_EDGE('',*,*,#14718,.F.);
#19948=ORIENTED_EDGE('',*,*,#14714,.T.);
#19949=ORIENTED_EDGE('',*,*,#14719,.T.);
#19950=ORIENTED_EDGE('',*,*,#14720,.F.);
#19951=ORIENTED_EDGE('',*,*,#14721,.F.);
#19952=ORIENTED_EDGE('',*,*,#14717,.T.);
#19953=ORIENTED_EDGE('',*,*,#14722,.T.);
#19954=ORIENTED_EDGE('',*,*,#14723,.F.);
#19955=ORIENTED_EDGE('',*,*,#14724,.F.);
#19956=ORIENTED_EDGE('',*,*,#14720,.T.);
#19957=ORIENTED_EDGE('',*,*,#14725,.T.);
#19958=ORIENTED_EDGE('',*,*,#14726,.F.);
#19959=ORIENTED_EDGE('',*,*,#14727,.F.);
#19960=ORIENTED_EDGE('',*,*,#14723,.T.);
#19961=ORIENTED_EDGE('',*,*,#14728,.T.);
#19962=ORIENTED_EDGE('',*,*,#14729,.F.);
#19963=ORIENTED_EDGE('',*,*,#14730,.F.);
#19964=ORIENTED_EDGE('',*,*,#14726,.T.);
#19965=ORIENTED_EDGE('',*,*,#14731,.T.);
#19966=ORIENTED_EDGE('',*,*,#14732,.F.);
#19967=ORIENTED_EDGE('',*,*,#14733,.F.);
#19968=ORIENTED_EDGE('',*,*,#14729,.T.);
#19969=ORIENTED_EDGE('',*,*,#14734,.T.);
#19970=ORIENTED_EDGE('',*,*,#14735,.F.);
#19971=ORIENTED_EDGE('',*,*,#14736,.F.);
#19972=ORIENTED_EDGE('',*,*,#14732,.T.);
#19973=ORIENTED_EDGE('',*,*,#14737,.T.);
#19974=ORIENTED_EDGE('',*,*,#14738,.F.);
#19975=ORIENTED_EDGE('',*,*,#14739,.F.);
#19976=ORIENTED_EDGE('',*,*,#14735,.T.);
#19977=ORIENTED_EDGE('',*,*,#14740,.T.);
#19978=ORIENTED_EDGE('',*,*,#14741,.F.);
#19979=ORIENTED_EDGE('',*,*,#14742,.F.);
#19980=ORIENTED_EDGE('',*,*,#14738,.T.);
#19981=ORIENTED_EDGE('',*,*,#14743,.T.);
#19982=ORIENTED_EDGE('',*,*,#14744,.F.);
#19983=ORIENTED_EDGE('',*,*,#14745,.F.);
#19984=ORIENTED_EDGE('',*,*,#14741,.T.);
#19985=ORIENTED_EDGE('',*,*,#14746,.T.);
#19986=ORIENTED_EDGE('',*,*,#14747,.F.);
#19987=ORIENTED_EDGE('',*,*,#14748,.F.);
#19988=ORIENTED_EDGE('',*,*,#14744,.T.);
#19989=ORIENTED_EDGE('',*,*,#14749,.T.);
#19990=ORIENTED_EDGE('',*,*,#14750,.F.);
#19991=ORIENTED_EDGE('',*,*,#14751,.F.);
#19992=ORIENTED_EDGE('',*,*,#14747,.T.);
#19993=ORIENTED_EDGE('',*,*,#14752,.T.);
#19994=ORIENTED_EDGE('',*,*,#14750,.T.);
#19995=ORIENTED_EDGE('',*,*,#14753,.T.);
#19996=ORIENTED_EDGE('',*,*,#14754,.F.);
#19997=ORIENTED_EDGE('',*,*,#14660,.T.);
#19998=ORIENTED_EDGE('',*,*,#14755,.F.);
#19999=ORIENTED_EDGE('',*,*,#14756,.T.);
#20000=ORIENTED_EDGE('',*,*,#14757,.T.);
#20001=ORIENTED_EDGE('',*,*,#14758,.T.);
#20002=ORIENTED_EDGE('',*,*,#14657,.T.);
#20003=ORIENTED_EDGE('',*,*,#14759,.F.);
#20004=ORIENTED_EDGE('',*,*,#14757,.F.);
#20005=ORIENTED_EDGE('',*,*,#14760,.F.);
#20006=ORIENTED_EDGE('',*,*,#14761,.T.);
#20007=ORIENTED_EDGE('',*,*,#14762,.T.);
#20008=ORIENTED_EDGE('',*,*,#14763,.T.);
#20009=ORIENTED_EDGE('',*,*,#14764,.F.);
#20010=ORIENTED_EDGE('',*,*,#14765,.T.);
#20011=ORIENTED_EDGE('',*,*,#14766,.T.);
#20012=ORIENTED_EDGE('',*,*,#14767,.T.);
#20013=ORIENTED_EDGE('',*,*,#14768,.F.);
#20014=ORIENTED_EDGE('',*,*,#14769,.T.);
#20015=ORIENTED_EDGE('',*,*,#14770,.T.);
#20016=ORIENTED_EDGE('',*,*,#14771,.T.);
#20017=ORIENTED_EDGE('',*,*,#14772,.F.);
#20018=ORIENTED_EDGE('',*,*,#14773,.T.);
#20019=ORIENTED_EDGE('',*,*,#14774,.T.);
#20020=ORIENTED_EDGE('',*,*,#14775,.T.);
#20021=ORIENTED_EDGE('',*,*,#14776,.F.);
#20022=ORIENTED_EDGE('',*,*,#14777,.T.);
#20023=ORIENTED_EDGE('',*,*,#14778,.T.);
#20024=ORIENTED_EDGE('',*,*,#14779,.T.);
#20025=ORIENTED_EDGE('',*,*,#14780,.F.);
#20026=ORIENTED_EDGE('',*,*,#14781,.T.);
#20027=ORIENTED_EDGE('',*,*,#14782,.T.);
#20028=ORIENTED_EDGE('',*,*,#14783,.T.);
#20029=ORIENTED_EDGE('',*,*,#14784,.F.);
#20030=ORIENTED_EDGE('',*,*,#14785,.T.);
#20031=ORIENTED_EDGE('',*,*,#14786,.T.);
#20032=ORIENTED_EDGE('',*,*,#14787,.T.);
#20033=ORIENTED_EDGE('',*,*,#14788,.F.);
#20034=ORIENTED_EDGE('',*,*,#14789,.T.);
#20035=ORIENTED_EDGE('',*,*,#14790,.T.);
#20036=ORIENTED_EDGE('',*,*,#14791,.T.);
#20037=ORIENTED_EDGE('',*,*,#14792,.F.);
#20038=ORIENTED_EDGE('',*,*,#14793,.T.);
#20039=ORIENTED_EDGE('',*,*,#14794,.T.);
#20040=ORIENTED_EDGE('',*,*,#14795,.T.);
#20041=ORIENTED_EDGE('',*,*,#14796,.F.);
#20042=ORIENTED_EDGE('',*,*,#14797,.T.);
#20043=ORIENTED_EDGE('',*,*,#14798,.T.);
#20044=ORIENTED_EDGE('',*,*,#14799,.T.);
#20045=ORIENTED_EDGE('',*,*,#14800,.F.);
#20046=ORIENTED_EDGE('',*,*,#14801,.T.);
#20047=ORIENTED_EDGE('',*,*,#14802,.T.);
#20048=ORIENTED_EDGE('',*,*,#14803,.T.);
#20049=ORIENTED_EDGE('',*,*,#14804,.F.);
#20050=ORIENTED_EDGE('',*,*,#14805,.T.);
#20051=ORIENTED_EDGE('',*,*,#14806,.T.);
#20052=ORIENTED_EDGE('',*,*,#14807,.T.);
#20053=ORIENTED_EDGE('',*,*,#14808,.F.);
#20054=ORIENTED_EDGE('',*,*,#14809,.T.);
#20055=ORIENTED_EDGE('',*,*,#14810,.T.);
#20056=ORIENTED_EDGE('',*,*,#14811,.T.);
#20057=ORIENTED_EDGE('',*,*,#14812,.F.);
#20058=ORIENTED_EDGE('',*,*,#14813,.T.);
#20059=ORIENTED_EDGE('',*,*,#14814,.T.);
#20060=ORIENTED_EDGE('',*,*,#14815,.T.);
#20061=ORIENTED_EDGE('',*,*,#14816,.F.);
#20062=ORIENTED_EDGE('',*,*,#14817,.T.);
#20063=ORIENTED_EDGE('',*,*,#14818,.T.);
#20064=ORIENTED_EDGE('',*,*,#14819,.T.);
#20065=ORIENTED_EDGE('',*,*,#14820,.F.);
#20066=ORIENTED_EDGE('',*,*,#14821,.F.);
#20067=ORIENTED_EDGE('',*,*,#14822,.F.);
#20068=ORIENTED_EDGE('',*,*,#14823,.F.);
#20069=ORIENTED_EDGE('',*,*,#14824,.F.);
#20070=ORIENTED_EDGE('',*,*,#14825,.F.);
#20071=ORIENTED_EDGE('',*,*,#14826,.F.);
#20072=ORIENTED_EDGE('',*,*,#14827,.F.);
#20073=ORIENTED_EDGE('',*,*,#14828,.T.);
#20074=ORIENTED_EDGE('',*,*,#14829,.T.);
#20075=ORIENTED_EDGE('',*,*,#14828,.F.);
#20076=ORIENTED_EDGE('',*,*,#14830,.F.);
#20077=ORIENTED_EDGE('',*,*,#14831,.T.);
#20078=ORIENTED_EDGE('',*,*,#14832,.T.);
#20079=ORIENTED_EDGE('',*,*,#14831,.F.);
#20080=ORIENTED_EDGE('',*,*,#14833,.F.);
#20081=ORIENTED_EDGE('',*,*,#14834,.F.);
#20082=ORIENTED_EDGE('',*,*,#14835,.F.);
#20083=ORIENTED_EDGE('',*,*,#14836,.F.);
#20084=ORIENTED_EDGE('',*,*,#14837,.F.);
#20085=ORIENTED_EDGE('',*,*,#14838,.F.);
#20086=ORIENTED_EDGE('',*,*,#14839,.F.);
#20087=ORIENTED_EDGE('',*,*,#14840,.F.);
#20088=ORIENTED_EDGE('',*,*,#14841,.F.);
#20089=ORIENTED_EDGE('',*,*,#14842,.F.);
#20090=ORIENTED_EDGE('',*,*,#14843,.F.);
#20091=ORIENTED_EDGE('',*,*,#14844,.F.);
#20092=ORIENTED_EDGE('',*,*,#14845,.F.);
#20093=ORIENTED_EDGE('',*,*,#14846,.F.);
#20094=ORIENTED_EDGE('',*,*,#14847,.F.);
#20095=ORIENTED_EDGE('',*,*,#14848,.F.);
#20096=ORIENTED_EDGE('',*,*,#14849,.F.);
#20097=ORIENTED_EDGE('',*,*,#14850,.F.);
#20098=ORIENTED_EDGE('',*,*,#14851,.F.);
#20099=ORIENTED_EDGE('',*,*,#14852,.F.);
#20100=ORIENTED_EDGE('',*,*,#14853,.F.);
#20101=ORIENTED_EDGE('',*,*,#14854,.F.);
#20102=ORIENTED_EDGE('',*,*,#14855,.F.);
#20103=ORIENTED_EDGE('',*,*,#14856,.F.);
#20104=ORIENTED_EDGE('',*,*,#14857,.F.);
#20105=ORIENTED_EDGE('',*,*,#14858,.F.);
#20106=ORIENTED_EDGE('',*,*,#14859,.F.);
#20107=ORIENTED_EDGE('',*,*,#14860,.F.);
#20108=ORIENTED_EDGE('',*,*,#14861,.F.);
#20109=ORIENTED_EDGE('',*,*,#14862,.F.);
#20110=ORIENTED_EDGE('',*,*,#14863,.F.);
#20111=ORIENTED_EDGE('',*,*,#14864,.F.);
#20112=ORIENTED_EDGE('',*,*,#14865,.F.);
#20113=ORIENTED_EDGE('',*,*,#14866,.F.);
#20114=ORIENTED_EDGE('',*,*,#14867,.F.);
#20115=ORIENTED_EDGE('',*,*,#14868,.F.);
#20116=ORIENTED_EDGE('',*,*,#14869,.F.);
#20117=ORIENTED_EDGE('',*,*,#14870,.F.);
#20118=ORIENTED_EDGE('',*,*,#14871,.F.);
#20119=ORIENTED_EDGE('',*,*,#14872,.F.);
#20120=ORIENTED_EDGE('',*,*,#14873,.F.);
#20121=ORIENTED_EDGE('',*,*,#14874,.F.);
#20122=ORIENTED_EDGE('',*,*,#14875,.F.);
#20123=ORIENTED_EDGE('',*,*,#14876,.F.);
#20124=ORIENTED_EDGE('',*,*,#14877,.F.);
#20125=ORIENTED_EDGE('',*,*,#14878,.F.);
#20126=ORIENTED_EDGE('',*,*,#14879,.F.);
#20127=ORIENTED_EDGE('',*,*,#14880,.F.);
#20128=ORIENTED_EDGE('',*,*,#14881,.F.);
#20129=ORIENTED_EDGE('',*,*,#14882,.F.);
#20130=ORIENTED_EDGE('',*,*,#14883,.F.);
#20131=ORIENTED_EDGE('',*,*,#14884,.F.);
#20132=ORIENTED_EDGE('',*,*,#14885,.F.);
#20133=ORIENTED_EDGE('',*,*,#14886,.F.);
#20134=ORIENTED_EDGE('',*,*,#14887,.F.);
#20135=ORIENTED_EDGE('',*,*,#14888,.F.);
#20136=ORIENTED_EDGE('',*,*,#14889,.F.);
#20137=ORIENTED_EDGE('',*,*,#14890,.F.);
#20138=ORIENTED_EDGE('',*,*,#14891,.F.);
#20139=ORIENTED_EDGE('',*,*,#14892,.F.);
#20140=ORIENTED_EDGE('',*,*,#14893,.F.);
#20141=ORIENTED_EDGE('',*,*,#14894,.F.);
#20142=ORIENTED_EDGE('',*,*,#14895,.F.);
#20143=ORIENTED_EDGE('',*,*,#14896,.F.);
#20144=ORIENTED_EDGE('',*,*,#14897,.F.);
#20145=ORIENTED_EDGE('',*,*,#14898,.F.);
#20146=ORIENTED_EDGE('',*,*,#14899,.F.);
#20147=ORIENTED_EDGE('',*,*,#14900,.F.);
#20148=ORIENTED_EDGE('',*,*,#14901,.F.);
#20149=ORIENTED_EDGE('',*,*,#14902,.F.);
#20150=ORIENTED_EDGE('',*,*,#14903,.F.);
#20151=ORIENTED_EDGE('',*,*,#14904,.F.);
#20152=ORIENTED_EDGE('',*,*,#14905,.F.);
#20153=ORIENTED_EDGE('',*,*,#14906,.F.);
#20154=ORIENTED_EDGE('',*,*,#14907,.F.);
#20155=ORIENTED_EDGE('',*,*,#14908,.F.);
#20156=ORIENTED_EDGE('',*,*,#14909,.F.);
#20157=ORIENTED_EDGE('',*,*,#14910,.F.);
#20158=ORIENTED_EDGE('',*,*,#14911,.F.);
#20159=ORIENTED_EDGE('',*,*,#14912,.F.);
#20160=ORIENTED_EDGE('',*,*,#14913,.F.);
#20161=ORIENTED_EDGE('',*,*,#14914,.F.);
#20162=ORIENTED_EDGE('',*,*,#14915,.F.);
#20163=ORIENTED_EDGE('',*,*,#14916,.F.);
#20164=ORIENTED_EDGE('',*,*,#14917,.F.);
#20165=ORIENTED_EDGE('',*,*,#14918,.F.);
#20166=ORIENTED_EDGE('',*,*,#14919,.F.);
#20167=ORIENTED_EDGE('',*,*,#14920,.F.);
#20168=ORIENTED_EDGE('',*,*,#14921,.F.);
#20169=ORIENTED_EDGE('',*,*,#14922,.F.);
#20170=ORIENTED_EDGE('',*,*,#14923,.F.);
#20171=ORIENTED_EDGE('',*,*,#14924,.F.);
#20172=ORIENTED_EDGE('',*,*,#14925,.F.);
#20173=ORIENTED_EDGE('',*,*,#14926,.F.);
#20174=ORIENTED_EDGE('',*,*,#14927,.F.);
#20175=ORIENTED_EDGE('',*,*,#14928,.F.);
#20176=ORIENTED_EDGE('',*,*,#14929,.F.);
#20177=ORIENTED_EDGE('',*,*,#14930,.F.);
#20178=ORIENTED_EDGE('',*,*,#14931,.F.);
#20179=ORIENTED_EDGE('',*,*,#14932,.F.);
#20180=ORIENTED_EDGE('',*,*,#14933,.F.);
#20181=ORIENTED_EDGE('',*,*,#14934,.F.);
#20182=ORIENTED_EDGE('',*,*,#14935,.F.);
#20183=ORIENTED_EDGE('',*,*,#14936,.F.);
#20184=ORIENTED_EDGE('',*,*,#14937,.F.);
#20185=ORIENTED_EDGE('',*,*,#14938,.F.);
#20186=ORIENTED_EDGE('',*,*,#14939,.F.);
#20187=ORIENTED_EDGE('',*,*,#14940,.F.);
#20188=ORIENTED_EDGE('',*,*,#14941,.F.);
#20189=ORIENTED_EDGE('',*,*,#14942,.F.);
#20190=ORIENTED_EDGE('',*,*,#14943,.F.);
#20191=ORIENTED_EDGE('',*,*,#14944,.F.);
#20192=ORIENTED_EDGE('',*,*,#14945,.F.);
#20193=ORIENTED_EDGE('',*,*,#14946,.F.);
#20194=ORIENTED_EDGE('',*,*,#14947,.F.);
#20195=ORIENTED_EDGE('',*,*,#14948,.F.);
#20196=ORIENTED_EDGE('',*,*,#14949,.F.);
#20197=ORIENTED_EDGE('',*,*,#14950,.F.);
#20198=ORIENTED_EDGE('',*,*,#14951,.F.);
#20199=ORIENTED_EDGE('',*,*,#14952,.F.);
#20200=ORIENTED_EDGE('',*,*,#14953,.F.);
#20201=ORIENTED_EDGE('',*,*,#14954,.F.);
#20202=ORIENTED_EDGE('',*,*,#14955,.F.);
#20203=ORIENTED_EDGE('',*,*,#14956,.F.);
#20204=ORIENTED_EDGE('',*,*,#14957,.F.);
#20205=ORIENTED_EDGE('',*,*,#14958,.F.);
#20206=ORIENTED_EDGE('',*,*,#14959,.F.);
#20207=ORIENTED_EDGE('',*,*,#14960,.F.);
#20208=ORIENTED_EDGE('',*,*,#14961,.F.);
#20209=ORIENTED_EDGE('',*,*,#14962,.F.);
#20210=ORIENTED_EDGE('',*,*,#14963,.F.);
#20211=ORIENTED_EDGE('',*,*,#14964,.F.);
#20212=ORIENTED_EDGE('',*,*,#14965,.F.);
#20213=ORIENTED_EDGE('',*,*,#14966,.F.);
#20214=ORIENTED_EDGE('',*,*,#14967,.F.);
#20215=ORIENTED_EDGE('',*,*,#14968,.F.);
#20216=ORIENTED_EDGE('',*,*,#14969,.F.);
#20217=ORIENTED_EDGE('',*,*,#14970,.F.);
#20218=ORIENTED_EDGE('',*,*,#14971,.F.);
#20219=ORIENTED_EDGE('',*,*,#14972,.F.);
#20220=ORIENTED_EDGE('',*,*,#14973,.F.);
#20221=ORIENTED_EDGE('',*,*,#14974,.F.);
#20222=ORIENTED_EDGE('',*,*,#14975,.F.);
#20223=ORIENTED_EDGE('',*,*,#14976,.F.);
#20224=ORIENTED_EDGE('',*,*,#14977,.F.);
#20225=ORIENTED_EDGE('',*,*,#14978,.F.);
#20226=ORIENTED_EDGE('',*,*,#14979,.F.);
#20227=ORIENTED_EDGE('',*,*,#14980,.F.);
#20228=ORIENTED_EDGE('',*,*,#14981,.F.);
#20229=ORIENTED_EDGE('',*,*,#14982,.F.);
#20230=ORIENTED_EDGE('',*,*,#14983,.F.);
#20231=ORIENTED_EDGE('',*,*,#14984,.F.);
#20232=ORIENTED_EDGE('',*,*,#14985,.F.);
#20233=ORIENTED_EDGE('',*,*,#14986,.F.);
#20234=ORIENTED_EDGE('',*,*,#14987,.F.);
#20235=ORIENTED_EDGE('',*,*,#14988,.F.);
#20236=ORIENTED_EDGE('',*,*,#14989,.F.);
#20237=ORIENTED_EDGE('',*,*,#14990,.F.);
#20238=ORIENTED_EDGE('',*,*,#14991,.F.);
#20239=ORIENTED_EDGE('',*,*,#14992,.F.);
#20240=ORIENTED_EDGE('',*,*,#14993,.F.);
#20241=ORIENTED_EDGE('',*,*,#14994,.F.);
#20242=ORIENTED_EDGE('',*,*,#14995,.F.);
#20243=ORIENTED_EDGE('',*,*,#14996,.F.);
#20244=ORIENTED_EDGE('',*,*,#14997,.F.);
#20245=ORIENTED_EDGE('',*,*,#14998,.F.);
#20246=ORIENTED_EDGE('',*,*,#14999,.F.);
#20247=ORIENTED_EDGE('',*,*,#15000,.F.);
#20248=ORIENTED_EDGE('',*,*,#15001,.F.);
#20249=ORIENTED_EDGE('',*,*,#15002,.F.);
#20250=ORIENTED_EDGE('',*,*,#15003,.F.);
#20251=ORIENTED_EDGE('',*,*,#15004,.F.);
#20252=ORIENTED_EDGE('',*,*,#15005,.F.);
#20253=ORIENTED_EDGE('',*,*,#15006,.F.);
#20254=ORIENTED_EDGE('',*,*,#15007,.F.);
#20255=ORIENTED_EDGE('',*,*,#15008,.F.);
#20256=ORIENTED_EDGE('',*,*,#15009,.F.);
#20257=ORIENTED_EDGE('',*,*,#15010,.F.);
#20258=ORIENTED_EDGE('',*,*,#15011,.F.);
#20259=ORIENTED_EDGE('',*,*,#15012,.F.);
#20260=ORIENTED_EDGE('',*,*,#15013,.F.);
#20261=ORIENTED_EDGE('',*,*,#15014,.F.);
#20262=ORIENTED_EDGE('',*,*,#15015,.F.);
#20263=ORIENTED_EDGE('',*,*,#15016,.F.);
#20264=ORIENTED_EDGE('',*,*,#14819,.F.);
#20265=ORIENTED_EDGE('',*,*,#15017,.F.);
#20266=ORIENTED_EDGE('',*,*,#15018,.F.);
#20267=ORIENTED_EDGE('',*,*,#15019,.F.);
#20268=ORIENTED_EDGE('',*,*,#14815,.F.);
#20269=ORIENTED_EDGE('',*,*,#15020,.F.);
#20270=ORIENTED_EDGE('',*,*,#15021,.F.);
#20271=ORIENTED_EDGE('',*,*,#15022,.F.);
#20272=ORIENTED_EDGE('',*,*,#14811,.F.);
#20273=ORIENTED_EDGE('',*,*,#15023,.F.);
#20274=ORIENTED_EDGE('',*,*,#15024,.F.);
#20275=ORIENTED_EDGE('',*,*,#15025,.F.);
#20276=ORIENTED_EDGE('',*,*,#14807,.F.);
#20277=ORIENTED_EDGE('',*,*,#15026,.F.);
#20278=ORIENTED_EDGE('',*,*,#15027,.F.);
#20279=ORIENTED_EDGE('',*,*,#15028,.F.);
#20280=ORIENTED_EDGE('',*,*,#14803,.F.);
#20281=ORIENTED_EDGE('',*,*,#15029,.F.);
#20282=ORIENTED_EDGE('',*,*,#15030,.F.);
#20283=ORIENTED_EDGE('',*,*,#15031,.F.);
#20284=ORIENTED_EDGE('',*,*,#14799,.F.);
#20285=ORIENTED_EDGE('',*,*,#15032,.F.);
#20286=ORIENTED_EDGE('',*,*,#15033,.F.);
#20287=ORIENTED_EDGE('',*,*,#15034,.F.);
#20288=ORIENTED_EDGE('',*,*,#14795,.F.);
#20289=ORIENTED_EDGE('',*,*,#15035,.F.);
#20290=ORIENTED_EDGE('',*,*,#15036,.F.);
#20291=ORIENTED_EDGE('',*,*,#15037,.F.);
#20292=ORIENTED_EDGE('',*,*,#14791,.F.);
#20293=ORIENTED_EDGE('',*,*,#15038,.F.);
#20294=ORIENTED_EDGE('',*,*,#15039,.F.);
#20295=ORIENTED_EDGE('',*,*,#15040,.F.);
#20296=ORIENTED_EDGE('',*,*,#14787,.F.);
#20297=ORIENTED_EDGE('',*,*,#15041,.F.);
#20298=ORIENTED_EDGE('',*,*,#15042,.F.);
#20299=ORIENTED_EDGE('',*,*,#15043,.F.);
#20300=ORIENTED_EDGE('',*,*,#14763,.F.);
#20301=ORIENTED_EDGE('',*,*,#15044,.F.);
#20302=ORIENTED_EDGE('',*,*,#15045,.F.);
#20303=ORIENTED_EDGE('',*,*,#15046,.F.);
#20304=ORIENTED_EDGE('',*,*,#14767,.F.);
#20305=ORIENTED_EDGE('',*,*,#15047,.F.);
#20306=ORIENTED_EDGE('',*,*,#15048,.F.);
#20307=ORIENTED_EDGE('',*,*,#15049,.F.);
#20308=ORIENTED_EDGE('',*,*,#14771,.F.);
#20309=ORIENTED_EDGE('',*,*,#15050,.F.);
#20310=ORIENTED_EDGE('',*,*,#15051,.F.);
#20311=ORIENTED_EDGE('',*,*,#15052,.F.);
#20312=ORIENTED_EDGE('',*,*,#14775,.F.);
#20313=ORIENTED_EDGE('',*,*,#15053,.F.);
#20314=ORIENTED_EDGE('',*,*,#15054,.F.);
#20315=ORIENTED_EDGE('',*,*,#15055,.F.);
#20316=ORIENTED_EDGE('',*,*,#14779,.F.);
#20317=ORIENTED_EDGE('',*,*,#15056,.F.);
#20318=ORIENTED_EDGE('',*,*,#15057,.F.);
#20319=ORIENTED_EDGE('',*,*,#15058,.F.);
#20320=ORIENTED_EDGE('',*,*,#14783,.F.);
#20321=ORIENTED_EDGE('',*,*,#15059,.F.);
#20322=ORIENTED_EDGE('',*,*,#15060,.F.);
#20323=ORIENTED_EDGE('',*,*,#15061,.F.);
#20324=ORIENTED_EDGE('',*,*,#15062,.F.);
#20325=ORIENTED_EDGE('',*,*,#15063,.F.);
#20326=ORIENTED_EDGE('',*,*,#15064,.F.);
#20327=ORIENTED_EDGE('',*,*,#15065,.F.);
#20328=ORIENTED_EDGE('',*,*,#15066,.F.);
#20329=ORIENTED_EDGE('',*,*,#15067,.F.);
#20330=ORIENTED_EDGE('',*,*,#15068,.F.);
#20331=ORIENTED_EDGE('',*,*,#15069,.F.);
#20332=ORIENTED_EDGE('',*,*,#15070,.F.);
#20333=ORIENTED_EDGE('',*,*,#15071,.F.);
#20334=ORIENTED_EDGE('',*,*,#15072,.F.);
#20335=ORIENTED_EDGE('',*,*,#15073,.F.);
#20336=ORIENTED_EDGE('',*,*,#15074,.F.);
#20337=ORIENTED_EDGE('',*,*,#15075,.F.);
#20338=ORIENTED_EDGE('',*,*,#15076,.F.);
#20339=ORIENTED_EDGE('',*,*,#15077,.F.);
#20340=ORIENTED_EDGE('',*,*,#15078,.F.);
#20341=ORIENTED_EDGE('',*,*,#15079,.F.);
#20342=ORIENTED_EDGE('',*,*,#15080,.F.);
#20343=ORIENTED_EDGE('',*,*,#15081,.F.);
#20344=ORIENTED_EDGE('',*,*,#15082,.F.);
#20345=ORIENTED_EDGE('',*,*,#15083,.F.);
#20346=ORIENTED_EDGE('',*,*,#15084,.F.);
#20347=ORIENTED_EDGE('',*,*,#15085,.F.);
#20348=ORIENTED_EDGE('',*,*,#15086,.F.);
#20349=ORIENTED_EDGE('',*,*,#15087,.F.);
#20350=ORIENTED_EDGE('',*,*,#15088,.F.);
#20351=ORIENTED_EDGE('',*,*,#15089,.F.);
#20352=ORIENTED_EDGE('',*,*,#15090,.F.);
#20353=ORIENTED_EDGE('',*,*,#15091,.F.);
#20354=ORIENTED_EDGE('',*,*,#15092,.F.);
#20355=ORIENTED_EDGE('',*,*,#15093,.F.);
#20356=ORIENTED_EDGE('',*,*,#15094,.F.);
#20357=ORIENTED_EDGE('',*,*,#15095,.F.);
#20358=ORIENTED_EDGE('',*,*,#15096,.F.);
#20359=ORIENTED_EDGE('',*,*,#15097,.F.);
#20360=ORIENTED_EDGE('',*,*,#15098,.F.);
#20361=ORIENTED_EDGE('',*,*,#15099,.F.);
#20362=ORIENTED_EDGE('',*,*,#15100,.F.);
#20363=ORIENTED_EDGE('',*,*,#15101,.F.);
#20364=ORIENTED_EDGE('',*,*,#15102,.F.);
#20365=ORIENTED_EDGE('',*,*,#15103,.F.);
#20366=ORIENTED_EDGE('',*,*,#15104,.F.);
#20367=ORIENTED_EDGE('',*,*,#15105,.F.);
#20368=ORIENTED_EDGE('',*,*,#15106,.F.);
#20369=ORIENTED_EDGE('',*,*,#15107,.F.);
#20370=ORIENTED_EDGE('',*,*,#15108,.F.);
#20371=ORIENTED_EDGE('',*,*,#15109,.F.);
#20372=ORIENTED_EDGE('',*,*,#15110,.F.);
#20373=ORIENTED_EDGE('',*,*,#15111,.F.);
#20374=ORIENTED_EDGE('',*,*,#15112,.F.);
#20375=ORIENTED_EDGE('',*,*,#15113,.F.);
#20376=ORIENTED_EDGE('',*,*,#15114,.F.);
#20377=ORIENTED_EDGE('',*,*,#15115,.F.);
#20378=ORIENTED_EDGE('',*,*,#15116,.F.);
#20379=ORIENTED_EDGE('',*,*,#15117,.F.);
#20380=ORIENTED_EDGE('',*,*,#15118,.F.);
#20381=ORIENTED_EDGE('',*,*,#15119,.F.);
#20382=ORIENTED_EDGE('',*,*,#15120,.F.);
#20383=ORIENTED_EDGE('',*,*,#15121,.F.);
#20384=ORIENTED_EDGE('',*,*,#15122,.F.);
#20385=ORIENTED_EDGE('',*,*,#15123,.F.);
#20386=ORIENTED_EDGE('',*,*,#15124,.F.);
#20387=ORIENTED_EDGE('',*,*,#15125,.F.);
#20388=ORIENTED_EDGE('',*,*,#15126,.F.);
#20389=ORIENTED_EDGE('',*,*,#15127,.F.);
#20390=ORIENTED_EDGE('',*,*,#15128,.F.);
#20391=ORIENTED_EDGE('',*,*,#15129,.F.);
#20392=ORIENTED_EDGE('',*,*,#15130,.F.);
#20393=ORIENTED_EDGE('',*,*,#15131,.F.);
#20394=ORIENTED_EDGE('',*,*,#15132,.F.);
#20395=ORIENTED_EDGE('',*,*,#15133,.F.);
#20396=ORIENTED_EDGE('',*,*,#15134,.F.);
#20397=ORIENTED_EDGE('',*,*,#15135,.F.);
#20398=ORIENTED_EDGE('',*,*,#15136,.F.);
#20399=ORIENTED_EDGE('',*,*,#15137,.F.);
#20400=ORIENTED_EDGE('',*,*,#15138,.F.);
#20401=ORIENTED_EDGE('',*,*,#15139,.T.);
#20402=ORIENTED_EDGE('',*,*,#14830,.T.);
#20403=ORIENTED_EDGE('',*,*,#15139,.F.);
#20404=ORIENTED_EDGE('',*,*,#15140,.F.);
#20405=ORIENTED_EDGE('',*,*,#15141,.F.);
#20406=ORIENTED_EDGE('',*,*,#15142,.T.);
#20407=ORIENTED_EDGE('',*,*,#15143,.F.);
#20408=ORIENTED_EDGE('',*,*,#15144,.F.);
#20409=ORIENTED_EDGE('',*,*,#15145,.F.);
#20410=ORIENTED_EDGE('',*,*,#15146,.T.);
#20411=ORIENTED_EDGE('',*,*,#15147,.F.);
#20412=ORIENTED_EDGE('',*,*,#15148,.F.);
#20413=ORIENTED_EDGE('',*,*,#15149,.F.);
#20414=ORIENTED_EDGE('',*,*,#15150,.T.);
#20415=ORIENTED_EDGE('',*,*,#15151,.F.);
#20416=ORIENTED_EDGE('',*,*,#15152,.F.);
#20417=ORIENTED_EDGE('',*,*,#15153,.F.);
#20418=ORIENTED_EDGE('',*,*,#15154,.T.);
#20419=ORIENTED_EDGE('',*,*,#15155,.F.);
#20420=ORIENTED_EDGE('',*,*,#15156,.F.);
#20421=ORIENTED_EDGE('',*,*,#15157,.F.);
#20422=ORIENTED_EDGE('',*,*,#15158,.T.);
#20423=ORIENTED_EDGE('',*,*,#15159,.F.);
#20424=ORIENTED_EDGE('',*,*,#15160,.F.);
#20425=ORIENTED_EDGE('',*,*,#15161,.F.);
#20426=ORIENTED_EDGE('',*,*,#15162,.T.);
#20427=ORIENTED_EDGE('',*,*,#15163,.F.);
#20428=ORIENTED_EDGE('',*,*,#15164,.F.);
#20429=ORIENTED_EDGE('',*,*,#15165,.F.);
#20430=ORIENTED_EDGE('',*,*,#15166,.T.);
#20431=ORIENTED_EDGE('',*,*,#15167,.F.);
#20432=ORIENTED_EDGE('',*,*,#15168,.F.);
#20433=ORIENTED_EDGE('',*,*,#15169,.F.);
#20434=ORIENTED_EDGE('',*,*,#15170,.T.);
#20435=ORIENTED_EDGE('',*,*,#15171,.F.);
#20436=ORIENTED_EDGE('',*,*,#15172,.F.);
#20437=ORIENTED_EDGE('',*,*,#15173,.F.);
#20438=ORIENTED_EDGE('',*,*,#15174,.T.);
#20439=ORIENTED_EDGE('',*,*,#15175,.F.);
#20440=ORIENTED_EDGE('',*,*,#15176,.F.);
#20441=ORIENTED_EDGE('',*,*,#15177,.F.);
#20442=ORIENTED_EDGE('',*,*,#15178,.T.);
#20443=ORIENTED_EDGE('',*,*,#15179,.F.);
#20444=ORIENTED_EDGE('',*,*,#15180,.F.);
#20445=ORIENTED_EDGE('',*,*,#15181,.F.);
#20446=ORIENTED_EDGE('',*,*,#15182,.T.);
#20447=ORIENTED_EDGE('',*,*,#15183,.F.);
#20448=ORIENTED_EDGE('',*,*,#15184,.F.);
#20449=ORIENTED_EDGE('',*,*,#15185,.F.);
#20450=ORIENTED_EDGE('',*,*,#15186,.T.);
#20451=ORIENTED_EDGE('',*,*,#15187,.F.);
#20452=ORIENTED_EDGE('',*,*,#15188,.F.);
#20453=ORIENTED_EDGE('',*,*,#15189,.F.);
#20454=ORIENTED_EDGE('',*,*,#15190,.T.);
#20455=ORIENTED_EDGE('',*,*,#15191,.F.);
#20456=ORIENTED_EDGE('',*,*,#15192,.F.);
#20457=ORIENTED_EDGE('',*,*,#15193,.F.);
#20458=ORIENTED_EDGE('',*,*,#15194,.T.);
#20459=ORIENTED_EDGE('',*,*,#15195,.F.);
#20460=ORIENTED_EDGE('',*,*,#15196,.F.);
#20461=ORIENTED_EDGE('',*,*,#15197,.F.);
#20462=ORIENTED_EDGE('',*,*,#15198,.T.);
#20463=ORIENTED_EDGE('',*,*,#15199,.F.);
#20464=ORIENTED_EDGE('',*,*,#15200,.F.);
#20465=ORIENTED_EDGE('',*,*,#15201,.F.);
#20466=ORIENTED_EDGE('',*,*,#15202,.T.);
#20467=ORIENTED_EDGE('',*,*,#15203,.F.);
#20468=ORIENTED_EDGE('',*,*,#15204,.F.);
#20469=ORIENTED_EDGE('',*,*,#15205,.F.);
#20470=ORIENTED_EDGE('',*,*,#15206,.T.);
#20471=ORIENTED_EDGE('',*,*,#15207,.F.);
#20472=ORIENTED_EDGE('',*,*,#15208,.F.);
#20473=ORIENTED_EDGE('',*,*,#15209,.F.);
#20474=ORIENTED_EDGE('',*,*,#15210,.T.);
#20475=ORIENTED_EDGE('',*,*,#15211,.F.);
#20476=ORIENTED_EDGE('',*,*,#15212,.F.);
#20477=ORIENTED_EDGE('',*,*,#15213,.F.);
#20478=ORIENTED_EDGE('',*,*,#15214,.T.);
#20479=ORIENTED_EDGE('',*,*,#15215,.F.);
#20480=ORIENTED_EDGE('',*,*,#15216,.F.);
#20481=ORIENTED_EDGE('',*,*,#15217,.F.);
#20482=ORIENTED_EDGE('',*,*,#15218,.T.);
#20483=ORIENTED_EDGE('',*,*,#15219,.F.);
#20484=ORIENTED_EDGE('',*,*,#15220,.F.);
#20485=ORIENTED_EDGE('',*,*,#15221,.F.);
#20486=ORIENTED_EDGE('',*,*,#15222,.T.);
#20487=ORIENTED_EDGE('',*,*,#15223,.F.);
#20488=ORIENTED_EDGE('',*,*,#15224,.F.);
#20489=ORIENTED_EDGE('',*,*,#15225,.F.);
#20490=ORIENTED_EDGE('',*,*,#15226,.T.);
#20491=ORIENTED_EDGE('',*,*,#15227,.F.);
#20492=ORIENTED_EDGE('',*,*,#15228,.F.);
#20493=ORIENTED_EDGE('',*,*,#15229,.F.);
#20494=ORIENTED_EDGE('',*,*,#15230,.T.);
#20495=ORIENTED_EDGE('',*,*,#15231,.F.);
#20496=ORIENTED_EDGE('',*,*,#15232,.F.);
#20497=ORIENTED_EDGE('',*,*,#15233,.F.);
#20498=ORIENTED_EDGE('',*,*,#15234,.T.);
#20499=ORIENTED_EDGE('',*,*,#15235,.F.);
#20500=ORIENTED_EDGE('',*,*,#15236,.F.);
#20501=ORIENTED_EDGE('',*,*,#15237,.F.);
#20502=ORIENTED_EDGE('',*,*,#15238,.T.);
#20503=ORIENTED_EDGE('',*,*,#15239,.F.);
#20504=ORIENTED_EDGE('',*,*,#15240,.F.);
#20505=ORIENTED_EDGE('',*,*,#15241,.F.);
#20506=ORIENTED_EDGE('',*,*,#15242,.T.);
#20507=ORIENTED_EDGE('',*,*,#15243,.F.);
#20508=ORIENTED_EDGE('',*,*,#15244,.F.);
#20509=ORIENTED_EDGE('',*,*,#15245,.F.);
#20510=ORIENTED_EDGE('',*,*,#15246,.T.);
#20511=ORIENTED_EDGE('',*,*,#15247,.F.);
#20512=ORIENTED_EDGE('',*,*,#15248,.F.);
#20513=ORIENTED_EDGE('',*,*,#15249,.F.);
#20514=ORIENTED_EDGE('',*,*,#15250,.T.);
#20515=ORIENTED_EDGE('',*,*,#15251,.F.);
#20516=ORIENTED_EDGE('',*,*,#15252,.F.);
#20517=ORIENTED_EDGE('',*,*,#15253,.F.);
#20518=ORIENTED_EDGE('',*,*,#15254,.T.);
#20519=ORIENTED_EDGE('',*,*,#15255,.F.);
#20520=ORIENTED_EDGE('',*,*,#15256,.F.);
#20521=ORIENTED_EDGE('',*,*,#15257,.F.);
#20522=ORIENTED_EDGE('',*,*,#15258,.T.);
#20523=ORIENTED_EDGE('',*,*,#15259,.F.);
#20524=ORIENTED_EDGE('',*,*,#15260,.F.);
#20525=ORIENTED_EDGE('',*,*,#15261,.F.);
#20526=ORIENTED_EDGE('',*,*,#15262,.T.);
#20527=ORIENTED_EDGE('',*,*,#15263,.F.);
#20528=ORIENTED_EDGE('',*,*,#15264,.F.);
#20529=ORIENTED_EDGE('',*,*,#15265,.F.);
#20530=ORIENTED_EDGE('',*,*,#15266,.T.);
#20531=ORIENTED_EDGE('',*,*,#15267,.F.);
#20532=ORIENTED_EDGE('',*,*,#15268,.F.);
#20533=ORIENTED_EDGE('',*,*,#15269,.F.);
#20534=ORIENTED_EDGE('',*,*,#15270,.T.);
#20535=ORIENTED_EDGE('',*,*,#15271,.F.);
#20536=ORIENTED_EDGE('',*,*,#15272,.F.);
#20537=ORIENTED_EDGE('',*,*,#15273,.F.);
#20538=ORIENTED_EDGE('',*,*,#15274,.T.);
#20539=ORIENTED_EDGE('',*,*,#15275,.F.);
#20540=ORIENTED_EDGE('',*,*,#15276,.F.);
#20541=ORIENTED_EDGE('',*,*,#15277,.F.);
#20542=ORIENTED_EDGE('',*,*,#15278,.T.);
#20543=ORIENTED_EDGE('',*,*,#15279,.F.);
#20544=ORIENTED_EDGE('',*,*,#15280,.F.);
#20545=ORIENTED_EDGE('',*,*,#15281,.F.);
#20546=ORIENTED_EDGE('',*,*,#15282,.T.);
#20547=ORIENTED_EDGE('',*,*,#15283,.F.);
#20548=ORIENTED_EDGE('',*,*,#15284,.F.);
#20549=ORIENTED_EDGE('',*,*,#15285,.F.);
#20550=ORIENTED_EDGE('',*,*,#15286,.T.);
#20551=ORIENTED_EDGE('',*,*,#15287,.F.);
#20552=ORIENTED_EDGE('',*,*,#15288,.F.);
#20553=ORIENTED_EDGE('',*,*,#15289,.F.);
#20554=ORIENTED_EDGE('',*,*,#15290,.T.);
#20555=ORIENTED_EDGE('',*,*,#15291,.F.);
#20556=ORIENTED_EDGE('',*,*,#15292,.F.);
#20557=ORIENTED_EDGE('',*,*,#15293,.F.);
#20558=ORIENTED_EDGE('',*,*,#15294,.T.);
#20559=ORIENTED_EDGE('',*,*,#15295,.F.);
#20560=ORIENTED_EDGE('',*,*,#15296,.F.);
#20561=ORIENTED_EDGE('',*,*,#15297,.F.);
#20562=ORIENTED_EDGE('',*,*,#15298,.T.);
#20563=ORIENTED_EDGE('',*,*,#15299,.F.);
#20564=ORIENTED_EDGE('',*,*,#15300,.F.);
#20565=ORIENTED_EDGE('',*,*,#15301,.F.);
#20566=ORIENTED_EDGE('',*,*,#15302,.T.);
#20567=ORIENTED_EDGE('',*,*,#15303,.F.);
#20568=ORIENTED_EDGE('',*,*,#15304,.F.);
#20569=ORIENTED_EDGE('',*,*,#15305,.F.);
#20570=ORIENTED_EDGE('',*,*,#15306,.T.);
#20571=ORIENTED_EDGE('',*,*,#15307,.F.);
#20572=ORIENTED_EDGE('',*,*,#15308,.F.);
#20573=ORIENTED_EDGE('',*,*,#15309,.F.);
#20574=ORIENTED_EDGE('',*,*,#15310,.T.);
#20575=ORIENTED_EDGE('',*,*,#15311,.F.);
#20576=ORIENTED_EDGE('',*,*,#15312,.F.);
#20577=ORIENTED_EDGE('',*,*,#15313,.F.);
#20578=ORIENTED_EDGE('',*,*,#15314,.T.);
#20579=ORIENTED_EDGE('',*,*,#15315,.F.);
#20580=ORIENTED_EDGE('',*,*,#15316,.F.);
#20581=ORIENTED_EDGE('',*,*,#15317,.F.);
#20582=ORIENTED_EDGE('',*,*,#15318,.T.);
#20583=ORIENTED_EDGE('',*,*,#15319,.F.);
#20584=ORIENTED_EDGE('',*,*,#15320,.F.);
#20585=ORIENTED_EDGE('',*,*,#15321,.F.);
#20586=ORIENTED_EDGE('',*,*,#15322,.T.);
#20587=ORIENTED_EDGE('',*,*,#15323,.F.);
#20588=ORIENTED_EDGE('',*,*,#15324,.F.);
#20589=ORIENTED_EDGE('',*,*,#15325,.F.);
#20590=ORIENTED_EDGE('',*,*,#15326,.T.);
#20591=ORIENTED_EDGE('',*,*,#15327,.F.);
#20592=ORIENTED_EDGE('',*,*,#15328,.F.);
#20593=ORIENTED_EDGE('',*,*,#15329,.F.);
#20594=ORIENTED_EDGE('',*,*,#15330,.T.);
#20595=ORIENTED_EDGE('',*,*,#15331,.F.);
#20596=ORIENTED_EDGE('',*,*,#15332,.F.);
#20597=ORIENTED_EDGE('',*,*,#15333,.F.);
#20598=ORIENTED_EDGE('',*,*,#15334,.T.);
#20599=ORIENTED_EDGE('',*,*,#15335,.F.);
#20600=ORIENTED_EDGE('',*,*,#15336,.F.);
#20601=ORIENTED_EDGE('',*,*,#15337,.F.);
#20602=ORIENTED_EDGE('',*,*,#15338,.T.);
#20603=ORIENTED_EDGE('',*,*,#15339,.F.);
#20604=ORIENTED_EDGE('',*,*,#15340,.F.);
#20605=ORIENTED_EDGE('',*,*,#15341,.F.);
#20606=ORIENTED_EDGE('',*,*,#15342,.T.);
#20607=ORIENTED_EDGE('',*,*,#15343,.F.);
#20608=ORIENTED_EDGE('',*,*,#15344,.F.);
#20609=ORIENTED_EDGE('',*,*,#15345,.F.);
#20610=ORIENTED_EDGE('',*,*,#15346,.T.);
#20611=ORIENTED_EDGE('',*,*,#15347,.F.);
#20612=ORIENTED_EDGE('',*,*,#15348,.F.);
#20613=ORIENTED_EDGE('',*,*,#15349,.F.);
#20614=ORIENTED_EDGE('',*,*,#15350,.T.);
#20615=ORIENTED_EDGE('',*,*,#15351,.F.);
#20616=ORIENTED_EDGE('',*,*,#15352,.F.);
#20617=ORIENTED_EDGE('',*,*,#15353,.F.);
#20618=ORIENTED_EDGE('',*,*,#15354,.T.);
#20619=ORIENTED_EDGE('',*,*,#15355,.F.);
#20620=ORIENTED_EDGE('',*,*,#15356,.F.);
#20621=ORIENTED_EDGE('',*,*,#15357,.F.);
#20622=ORIENTED_EDGE('',*,*,#15358,.T.);
#20623=ORIENTED_EDGE('',*,*,#15359,.F.);
#20624=ORIENTED_EDGE('',*,*,#15360,.F.);
#20625=ORIENTED_EDGE('',*,*,#15361,.F.);
#20626=ORIENTED_EDGE('',*,*,#15362,.T.);
#20627=ORIENTED_EDGE('',*,*,#15363,.F.);
#20628=ORIENTED_EDGE('',*,*,#15364,.F.);
#20629=ORIENTED_EDGE('',*,*,#15365,.F.);
#20630=ORIENTED_EDGE('',*,*,#15366,.T.);
#20631=ORIENTED_EDGE('',*,*,#15367,.F.);
#20632=ORIENTED_EDGE('',*,*,#15368,.F.);
#20633=ORIENTED_EDGE('',*,*,#15369,.F.);
#20634=ORIENTED_EDGE('',*,*,#15370,.T.);
#20635=ORIENTED_EDGE('',*,*,#15371,.F.);
#20636=ORIENTED_EDGE('',*,*,#15372,.F.);
#20637=ORIENTED_EDGE('',*,*,#15373,.F.);
#20638=ORIENTED_EDGE('',*,*,#15374,.T.);
#20639=ORIENTED_EDGE('',*,*,#15375,.F.);
#20640=ORIENTED_EDGE('',*,*,#15376,.F.);
#20641=ORIENTED_EDGE('',*,*,#15377,.F.);
#20642=ORIENTED_EDGE('',*,*,#15378,.T.);
#20643=ORIENTED_EDGE('',*,*,#15379,.F.);
#20644=ORIENTED_EDGE('',*,*,#14781,.F.);
#20645=ORIENTED_EDGE('',*,*,#15380,.F.);
#20646=ORIENTED_EDGE('',*,*,#15381,.T.);
#20647=ORIENTED_EDGE('',*,*,#15382,.F.);
#20648=ORIENTED_EDGE('',*,*,#14777,.F.);
#20649=ORIENTED_EDGE('',*,*,#15383,.F.);
#20650=ORIENTED_EDGE('',*,*,#15384,.T.);
#20651=ORIENTED_EDGE('',*,*,#15385,.F.);
#20652=ORIENTED_EDGE('',*,*,#14773,.F.);
#20653=ORIENTED_EDGE('',*,*,#15386,.F.);
#20654=ORIENTED_EDGE('',*,*,#15387,.T.);
#20655=ORIENTED_EDGE('',*,*,#15388,.F.);
#20656=ORIENTED_EDGE('',*,*,#14769,.F.);
#20657=ORIENTED_EDGE('',*,*,#15389,.F.);
#20658=ORIENTED_EDGE('',*,*,#15390,.T.);
#20659=ORIENTED_EDGE('',*,*,#15391,.F.);
#20660=ORIENTED_EDGE('',*,*,#14765,.F.);
#20661=ORIENTED_EDGE('',*,*,#15392,.F.);
#20662=ORIENTED_EDGE('',*,*,#15393,.T.);
#20663=ORIENTED_EDGE('',*,*,#15394,.F.);
#20664=ORIENTED_EDGE('',*,*,#14761,.F.);
#20665=ORIENTED_EDGE('',*,*,#15395,.F.);
#20666=ORIENTED_EDGE('',*,*,#15396,.T.);
#20667=ORIENTED_EDGE('',*,*,#15397,.F.);
#20668=ORIENTED_EDGE('',*,*,#14785,.F.);
#20669=ORIENTED_EDGE('',*,*,#15398,.F.);
#20670=ORIENTED_EDGE('',*,*,#15399,.T.);
#20671=ORIENTED_EDGE('',*,*,#15400,.F.);
#20672=ORIENTED_EDGE('',*,*,#14789,.F.);
#20673=ORIENTED_EDGE('',*,*,#15401,.F.);
#20674=ORIENTED_EDGE('',*,*,#15402,.T.);
#20675=ORIENTED_EDGE('',*,*,#15403,.F.);
#20676=ORIENTED_EDGE('',*,*,#14793,.F.);
#20677=ORIENTED_EDGE('',*,*,#15404,.F.);
#20678=ORIENTED_EDGE('',*,*,#15405,.T.);
#20679=ORIENTED_EDGE('',*,*,#15406,.F.);
#20680=ORIENTED_EDGE('',*,*,#14797,.F.);
#20681=ORIENTED_EDGE('',*,*,#15407,.F.);
#20682=ORIENTED_EDGE('',*,*,#15408,.T.);
#20683=ORIENTED_EDGE('',*,*,#15409,.F.);
#20684=ORIENTED_EDGE('',*,*,#14801,.F.);
#20685=ORIENTED_EDGE('',*,*,#15410,.F.);
#20686=ORIENTED_EDGE('',*,*,#15411,.T.);
#20687=ORIENTED_EDGE('',*,*,#15412,.F.);
#20688=ORIENTED_EDGE('',*,*,#14805,.F.);
#20689=ORIENTED_EDGE('',*,*,#15413,.F.);
#20690=ORIENTED_EDGE('',*,*,#15414,.T.);
#20691=ORIENTED_EDGE('',*,*,#15415,.F.);
#20692=ORIENTED_EDGE('',*,*,#14809,.F.);
#20693=ORIENTED_EDGE('',*,*,#15416,.F.);
#20694=ORIENTED_EDGE('',*,*,#15417,.T.);
#20695=ORIENTED_EDGE('',*,*,#15418,.F.);
#20696=ORIENTED_EDGE('',*,*,#14813,.F.);
#20697=ORIENTED_EDGE('',*,*,#15419,.F.);
#20698=ORIENTED_EDGE('',*,*,#15420,.T.);
#20699=ORIENTED_EDGE('',*,*,#15421,.F.);
#20700=ORIENTED_EDGE('',*,*,#14817,.F.);
#20701=ORIENTED_EDGE('',*,*,#15422,.F.);
#20702=ORIENTED_EDGE('',*,*,#15423,.T.);
#20703=ORIENTED_EDGE('',*,*,#15424,.F.);
#20704=ORIENTED_EDGE('',*,*,#15425,.F.);
#20705=ORIENTED_EDGE('',*,*,#15426,.F.);
#20706=ORIENTED_EDGE('',*,*,#15427,.T.);
#20707=ORIENTED_EDGE('',*,*,#15428,.F.);
#20708=ORIENTED_EDGE('',*,*,#15429,.F.);
#20709=ORIENTED_EDGE('',*,*,#15430,.F.);
#20710=ORIENTED_EDGE('',*,*,#15431,.T.);
#20711=ORIENTED_EDGE('',*,*,#15432,.F.);
#20712=ORIENTED_EDGE('',*,*,#15433,.F.);
#20713=ORIENTED_EDGE('',*,*,#15434,.F.);
#20714=ORIENTED_EDGE('',*,*,#15435,.T.);
#20715=ORIENTED_EDGE('',*,*,#15436,.F.);
#20716=ORIENTED_EDGE('',*,*,#15437,.F.);
#20717=ORIENTED_EDGE('',*,*,#15438,.F.);
#20718=ORIENTED_EDGE('',*,*,#15439,.T.);
#20719=ORIENTED_EDGE('',*,*,#15440,.F.);
#20720=ORIENTED_EDGE('',*,*,#15441,.F.);
#20721=ORIENTED_EDGE('',*,*,#15442,.F.);
#20722=ORIENTED_EDGE('',*,*,#15443,.T.);
#20723=ORIENTED_EDGE('',*,*,#15444,.F.);
#20724=ORIENTED_EDGE('',*,*,#15445,.F.);
#20725=ORIENTED_EDGE('',*,*,#15446,.T.);
#20726=ORIENTED_EDGE('',*,*,#15447,.F.);
#20727=ORIENTED_EDGE('',*,*,#15448,.F.);
#20728=ORIENTED_EDGE('',*,*,#15446,.F.);
#20729=ORIENTED_EDGE('',*,*,#15449,.F.);
#20730=ORIENTED_EDGE('',*,*,#15450,.T.);
#20731=ORIENTED_EDGE('',*,*,#15447,.T.);
#20732=ORIENTED_EDGE('',*,*,#15448,.T.);
#20733=ORIENTED_EDGE('',*,*,#15450,.F.);
#20734=ORIENTED_EDGE('',*,*,#15451,.F.);
#20735=ORIENTED_EDGE('',*,*,#15452,.T.);
#20736=ORIENTED_EDGE('',*,*,#15449,.T.);
#20737=ORIENTED_EDGE('',*,*,#15452,.F.);
#20738=ORIENTED_EDGE('',*,*,#15453,.F.);
#20739=ORIENTED_EDGE('',*,*,#15454,.T.);
#20740=ORIENTED_EDGE('',*,*,#15451,.T.);
#20741=ORIENTED_EDGE('',*,*,#15454,.F.);
#20742=ORIENTED_EDGE('',*,*,#14576,.F.);
#20743=ORIENTED_EDGE('',*,*,#15455,.T.);
#20744=ORIENTED_EDGE('',*,*,#15456,.T.);
#20745=ORIENTED_EDGE('',*,*,#15455,.F.);
#20746=ORIENTED_EDGE('',*,*,#15457,.F.);
#20747=ORIENTED_EDGE('',*,*,#15458,.T.);
#20748=ORIENTED_EDGE('',*,*,#15459,.F.);
#20749=ORIENTED_EDGE('',*,*,#15396,.F.);
#20750=ORIENTED_EDGE('',*,*,#15460,.F.);
#20751=ORIENTED_EDGE('',*,*,#15393,.F.);
#20752=ORIENTED_EDGE('',*,*,#15461,.F.);
#20753=ORIENTED_EDGE('',*,*,#15462,.T.);
#20754=ORIENTED_EDGE('',*,*,#15463,.F.);
#20755=ORIENTED_EDGE('',*,*,#15390,.F.);
#20756=ORIENTED_EDGE('',*,*,#15464,.F.);
#20757=ORIENTED_EDGE('',*,*,#15465,.T.);
#20758=ORIENTED_EDGE('',*,*,#15466,.F.);
#20759=ORIENTED_EDGE('',*,*,#15387,.F.);
#20760=ORIENTED_EDGE('',*,*,#15467,.F.);
#20761=ORIENTED_EDGE('',*,*,#15468,.T.);
#20762=ORIENTED_EDGE('',*,*,#15469,.F.);
#20763=ORIENTED_EDGE('',*,*,#15384,.F.);
#20764=ORIENTED_EDGE('',*,*,#15470,.F.);
#20765=ORIENTED_EDGE('',*,*,#15471,.T.);
#20766=ORIENTED_EDGE('',*,*,#15472,.F.);
#20767=ORIENTED_EDGE('',*,*,#15381,.F.);
#20768=ORIENTED_EDGE('',*,*,#15473,.F.);
#20769=ORIENTED_EDGE('',*,*,#15474,.T.);
#20770=ORIENTED_EDGE('',*,*,#15475,.F.);
#20771=ORIENTED_EDGE('',*,*,#15378,.F.);
#20772=ORIENTED_EDGE('',*,*,#15476,.F.);
#20773=ORIENTED_EDGE('',*,*,#15477,.T.);
#20774=ORIENTED_EDGE('',*,*,#15478,.F.);
#20775=ORIENTED_EDGE('',*,*,#15374,.F.);
#20776=ORIENTED_EDGE('',*,*,#15479,.F.);
#20777=ORIENTED_EDGE('',*,*,#15480,.T.);
#20778=ORIENTED_EDGE('',*,*,#15481,.F.);
#20779=ORIENTED_EDGE('',*,*,#15370,.F.);
#20780=ORIENTED_EDGE('',*,*,#15482,.F.);
#20781=ORIENTED_EDGE('',*,*,#15483,.T.);
#20782=ORIENTED_EDGE('',*,*,#15484,.F.);
#20783=ORIENTED_EDGE('',*,*,#15366,.F.);
#20784=ORIENTED_EDGE('',*,*,#15485,.F.);
#20785=ORIENTED_EDGE('',*,*,#15486,.T.);
#20786=ORIENTED_EDGE('',*,*,#15487,.F.);
#20787=ORIENTED_EDGE('',*,*,#15362,.F.);
#20788=ORIENTED_EDGE('',*,*,#15488,.F.);
#20789=ORIENTED_EDGE('',*,*,#15489,.T.);
#20790=ORIENTED_EDGE('',*,*,#15490,.F.);
#20791=ORIENTED_EDGE('',*,*,#15358,.F.);
#20792=ORIENTED_EDGE('',*,*,#15491,.F.);
#20793=ORIENTED_EDGE('',*,*,#15492,.T.);
#20794=ORIENTED_EDGE('',*,*,#15493,.F.);
#20795=ORIENTED_EDGE('',*,*,#15354,.F.);
#20796=ORIENTED_EDGE('',*,*,#15494,.F.);
#20797=ORIENTED_EDGE('',*,*,#15495,.T.);
#20798=ORIENTED_EDGE('',*,*,#15496,.F.);
#20799=ORIENTED_EDGE('',*,*,#15350,.F.);
#20800=ORIENTED_EDGE('',*,*,#15497,.F.);
#20801=ORIENTED_EDGE('',*,*,#15498,.T.);
#20802=ORIENTED_EDGE('',*,*,#15499,.F.);
#20803=ORIENTED_EDGE('',*,*,#15346,.F.);
#20804=ORIENTED_EDGE('',*,*,#15500,.F.);
#20805=ORIENTED_EDGE('',*,*,#15501,.T.);
#20806=ORIENTED_EDGE('',*,*,#15502,.F.);
#20807=ORIENTED_EDGE('',*,*,#15342,.F.);
#20808=ORIENTED_EDGE('',*,*,#15503,.F.);
#20809=ORIENTED_EDGE('',*,*,#15504,.T.);
#20810=ORIENTED_EDGE('',*,*,#15505,.F.);
#20811=ORIENTED_EDGE('',*,*,#15338,.F.);
#20812=ORIENTED_EDGE('',*,*,#15506,.F.);
#20813=ORIENTED_EDGE('',*,*,#15507,.T.);
#20814=ORIENTED_EDGE('',*,*,#15508,.F.);
#20815=ORIENTED_EDGE('',*,*,#15334,.F.);
#20816=ORIENTED_EDGE('',*,*,#15509,.F.);
#20817=ORIENTED_EDGE('',*,*,#15510,.T.);
#20818=ORIENTED_EDGE('',*,*,#15511,.F.);
#20819=ORIENTED_EDGE('',*,*,#15330,.F.);
#20820=ORIENTED_EDGE('',*,*,#15512,.F.);
#20821=ORIENTED_EDGE('',*,*,#15513,.T.);
#20822=ORIENTED_EDGE('',*,*,#15514,.F.);
#20823=ORIENTED_EDGE('',*,*,#15326,.F.);
#20824=ORIENTED_EDGE('',*,*,#15515,.F.);
#20825=ORIENTED_EDGE('',*,*,#15516,.T.);
#20826=ORIENTED_EDGE('',*,*,#15517,.F.);
#20827=ORIENTED_EDGE('',*,*,#15322,.F.);
#20828=ORIENTED_EDGE('',*,*,#15518,.F.);
#20829=ORIENTED_EDGE('',*,*,#15519,.T.);
#20830=ORIENTED_EDGE('',*,*,#15520,.F.);
#20831=ORIENTED_EDGE('',*,*,#15318,.F.);
#20832=ORIENTED_EDGE('',*,*,#15521,.F.);
#20833=ORIENTED_EDGE('',*,*,#15522,.T.);
#20834=ORIENTED_EDGE('',*,*,#15523,.F.);
#20835=ORIENTED_EDGE('',*,*,#15314,.F.);
#20836=ORIENTED_EDGE('',*,*,#15524,.F.);
#20837=ORIENTED_EDGE('',*,*,#15525,.T.);
#20838=ORIENTED_EDGE('',*,*,#15526,.F.);
#20839=ORIENTED_EDGE('',*,*,#15310,.F.);
#20840=ORIENTED_EDGE('',*,*,#15527,.F.);
#20841=ORIENTED_EDGE('',*,*,#15528,.T.);
#20842=ORIENTED_EDGE('',*,*,#15529,.F.);
#20843=ORIENTED_EDGE('',*,*,#15306,.F.);
#20844=ORIENTED_EDGE('',*,*,#15530,.F.);
#20845=ORIENTED_EDGE('',*,*,#15531,.T.);
#20846=ORIENTED_EDGE('',*,*,#15532,.F.);
#20847=ORIENTED_EDGE('',*,*,#15302,.F.);
#20848=ORIENTED_EDGE('',*,*,#15533,.F.);
#20849=ORIENTED_EDGE('',*,*,#15534,.T.);
#20850=ORIENTED_EDGE('',*,*,#15535,.F.);
#20851=ORIENTED_EDGE('',*,*,#15298,.F.);
#20852=ORIENTED_EDGE('',*,*,#15536,.F.);
#20853=ORIENTED_EDGE('',*,*,#15537,.T.);
#20854=ORIENTED_EDGE('',*,*,#15538,.F.);
#20855=ORIENTED_EDGE('',*,*,#15294,.F.);
#20856=ORIENTED_EDGE('',*,*,#15539,.F.);
#20857=ORIENTED_EDGE('',*,*,#15540,.T.);
#20858=ORIENTED_EDGE('',*,*,#15541,.F.);
#20859=ORIENTED_EDGE('',*,*,#15290,.F.);
#20860=ORIENTED_EDGE('',*,*,#15542,.F.);
#20861=ORIENTED_EDGE('',*,*,#15543,.T.);
#20862=ORIENTED_EDGE('',*,*,#15544,.F.);
#20863=ORIENTED_EDGE('',*,*,#15286,.F.);
#20864=ORIENTED_EDGE('',*,*,#15545,.F.);
#20865=ORIENTED_EDGE('',*,*,#15546,.T.);
#20866=ORIENTED_EDGE('',*,*,#15547,.F.);
#20867=ORIENTED_EDGE('',*,*,#15282,.F.);
#20868=ORIENTED_EDGE('',*,*,#15548,.F.);
#20869=ORIENTED_EDGE('',*,*,#15549,.T.);
#20870=ORIENTED_EDGE('',*,*,#15550,.F.);
#20871=ORIENTED_EDGE('',*,*,#15278,.F.);
#20872=ORIENTED_EDGE('',*,*,#15551,.F.);
#20873=ORIENTED_EDGE('',*,*,#15552,.T.);
#20874=ORIENTED_EDGE('',*,*,#15553,.F.);
#20875=ORIENTED_EDGE('',*,*,#15274,.F.);
#20876=ORIENTED_EDGE('',*,*,#15554,.F.);
#20877=ORIENTED_EDGE('',*,*,#15555,.T.);
#20878=ORIENTED_EDGE('',*,*,#15556,.F.);
#20879=ORIENTED_EDGE('',*,*,#15270,.F.);
#20880=ORIENTED_EDGE('',*,*,#15557,.F.);
#20881=ORIENTED_EDGE('',*,*,#15558,.T.);
#20882=ORIENTED_EDGE('',*,*,#15559,.F.);
#20883=ORIENTED_EDGE('',*,*,#15266,.F.);
#20884=ORIENTED_EDGE('',*,*,#15560,.F.);
#20885=ORIENTED_EDGE('',*,*,#15561,.T.);
#20886=ORIENTED_EDGE('',*,*,#15562,.F.);
#20887=ORIENTED_EDGE('',*,*,#15262,.F.);
#20888=ORIENTED_EDGE('',*,*,#15563,.F.);
#20889=ORIENTED_EDGE('',*,*,#15564,.T.);
#20890=ORIENTED_EDGE('',*,*,#15565,.F.);
#20891=ORIENTED_EDGE('',*,*,#15258,.F.);
#20892=ORIENTED_EDGE('',*,*,#15566,.F.);
#20893=ORIENTED_EDGE('',*,*,#15567,.T.);
#20894=ORIENTED_EDGE('',*,*,#15568,.F.);
#20895=ORIENTED_EDGE('',*,*,#15254,.F.);
#20896=ORIENTED_EDGE('',*,*,#15569,.F.);
#20897=ORIENTED_EDGE('',*,*,#15570,.T.);
#20898=ORIENTED_EDGE('',*,*,#15571,.F.);
#20899=ORIENTED_EDGE('',*,*,#15250,.F.);
#20900=ORIENTED_EDGE('',*,*,#15572,.F.);
#20901=ORIENTED_EDGE('',*,*,#15573,.T.);
#20902=ORIENTED_EDGE('',*,*,#15574,.F.);
#20903=ORIENTED_EDGE('',*,*,#15246,.F.);
#20904=ORIENTED_EDGE('',*,*,#15575,.F.);
#20905=ORIENTED_EDGE('',*,*,#15576,.T.);
#20906=ORIENTED_EDGE('',*,*,#15577,.F.);
#20907=ORIENTED_EDGE('',*,*,#15242,.F.);
#20908=ORIENTED_EDGE('',*,*,#15578,.F.);
#20909=ORIENTED_EDGE('',*,*,#15579,.T.);
#20910=ORIENTED_EDGE('',*,*,#15580,.F.);
#20911=ORIENTED_EDGE('',*,*,#15238,.F.);
#20912=ORIENTED_EDGE('',*,*,#15581,.F.);
#20913=ORIENTED_EDGE('',*,*,#15582,.T.);
#20914=ORIENTED_EDGE('',*,*,#15583,.F.);
#20915=ORIENTED_EDGE('',*,*,#15234,.F.);
#20916=ORIENTED_EDGE('',*,*,#15584,.F.);
#20917=ORIENTED_EDGE('',*,*,#15585,.T.);
#20918=ORIENTED_EDGE('',*,*,#15586,.F.);
#20919=ORIENTED_EDGE('',*,*,#15230,.F.);
#20920=ORIENTED_EDGE('',*,*,#15587,.F.);
#20921=ORIENTED_EDGE('',*,*,#15588,.T.);
#20922=ORIENTED_EDGE('',*,*,#15589,.F.);
#20923=ORIENTED_EDGE('',*,*,#15226,.F.);
#20924=ORIENTED_EDGE('',*,*,#15590,.F.);
#20925=ORIENTED_EDGE('',*,*,#15591,.T.);
#20926=ORIENTED_EDGE('',*,*,#15592,.F.);
#20927=ORIENTED_EDGE('',*,*,#15222,.F.);
#20928=ORIENTED_EDGE('',*,*,#15593,.F.);
#20929=ORIENTED_EDGE('',*,*,#15594,.T.);
#20930=ORIENTED_EDGE('',*,*,#15595,.F.);
#20931=ORIENTED_EDGE('',*,*,#15218,.F.);
#20932=ORIENTED_EDGE('',*,*,#15596,.F.);
#20933=ORIENTED_EDGE('',*,*,#15597,.T.);
#20934=ORIENTED_EDGE('',*,*,#15598,.F.);
#20935=ORIENTED_EDGE('',*,*,#15214,.F.);
#20936=ORIENTED_EDGE('',*,*,#15599,.F.);
#20937=ORIENTED_EDGE('',*,*,#15600,.T.);
#20938=ORIENTED_EDGE('',*,*,#15601,.F.);
#20939=ORIENTED_EDGE('',*,*,#15210,.F.);
#20940=ORIENTED_EDGE('',*,*,#15602,.F.);
#20941=ORIENTED_EDGE('',*,*,#15603,.T.);
#20942=ORIENTED_EDGE('',*,*,#15604,.F.);
#20943=ORIENTED_EDGE('',*,*,#15206,.F.);
#20944=ORIENTED_EDGE('',*,*,#15605,.F.);
#20945=ORIENTED_EDGE('',*,*,#15606,.T.);
#20946=ORIENTED_EDGE('',*,*,#15607,.F.);
#20947=ORIENTED_EDGE('',*,*,#15202,.F.);
#20948=ORIENTED_EDGE('',*,*,#15608,.F.);
#20949=ORIENTED_EDGE('',*,*,#15609,.T.);
#20950=ORIENTED_EDGE('',*,*,#15610,.F.);
#20951=ORIENTED_EDGE('',*,*,#15198,.F.);
#20952=ORIENTED_EDGE('',*,*,#15611,.F.);
#20953=ORIENTED_EDGE('',*,*,#15612,.T.);
#20954=ORIENTED_EDGE('',*,*,#15613,.F.);
#20955=ORIENTED_EDGE('',*,*,#15194,.F.);
#20956=ORIENTED_EDGE('',*,*,#15614,.F.);
#20957=ORIENTED_EDGE('',*,*,#15615,.T.);
#20958=ORIENTED_EDGE('',*,*,#15616,.F.);
#20959=ORIENTED_EDGE('',*,*,#15190,.F.);
#20960=ORIENTED_EDGE('',*,*,#15617,.F.);
#20961=ORIENTED_EDGE('',*,*,#15618,.T.);
#20962=ORIENTED_EDGE('',*,*,#15619,.F.);
#20963=ORIENTED_EDGE('',*,*,#15186,.F.);
#20964=ORIENTED_EDGE('',*,*,#15620,.F.);
#20965=ORIENTED_EDGE('',*,*,#15621,.T.);
#20966=ORIENTED_EDGE('',*,*,#15622,.F.);
#20967=ORIENTED_EDGE('',*,*,#15182,.F.);
#20968=ORIENTED_EDGE('',*,*,#15623,.F.);
#20969=ORIENTED_EDGE('',*,*,#15624,.T.);
#20970=ORIENTED_EDGE('',*,*,#15625,.F.);
#20971=ORIENTED_EDGE('',*,*,#15178,.F.);
#20972=ORIENTED_EDGE('',*,*,#15626,.F.);
#20973=ORIENTED_EDGE('',*,*,#15627,.T.);
#20974=ORIENTED_EDGE('',*,*,#15628,.F.);
#20975=ORIENTED_EDGE('',*,*,#15174,.F.);
#20976=ORIENTED_EDGE('',*,*,#15629,.F.);
#20977=ORIENTED_EDGE('',*,*,#15630,.T.);
#20978=ORIENTED_EDGE('',*,*,#15631,.F.);
#20979=ORIENTED_EDGE('',*,*,#15170,.F.);
#20980=ORIENTED_EDGE('',*,*,#15632,.F.);
#20981=ORIENTED_EDGE('',*,*,#15633,.T.);
#20982=ORIENTED_EDGE('',*,*,#15634,.F.);
#20983=ORIENTED_EDGE('',*,*,#15166,.F.);
#20984=ORIENTED_EDGE('',*,*,#15635,.F.);
#20985=ORIENTED_EDGE('',*,*,#15636,.T.);
#20986=ORIENTED_EDGE('',*,*,#15637,.F.);
#20987=ORIENTED_EDGE('',*,*,#15162,.F.);
#20988=ORIENTED_EDGE('',*,*,#15638,.F.);
#20989=ORIENTED_EDGE('',*,*,#15639,.T.);
#20990=ORIENTED_EDGE('',*,*,#15640,.F.);
#20991=ORIENTED_EDGE('',*,*,#15158,.F.);
#20992=ORIENTED_EDGE('',*,*,#15641,.F.);
#20993=ORIENTED_EDGE('',*,*,#15642,.T.);
#20994=ORIENTED_EDGE('',*,*,#15643,.F.);
#20995=ORIENTED_EDGE('',*,*,#15154,.F.);
#20996=ORIENTED_EDGE('',*,*,#15644,.F.);
#20997=ORIENTED_EDGE('',*,*,#15645,.T.);
#20998=ORIENTED_EDGE('',*,*,#15646,.F.);
#20999=ORIENTED_EDGE('',*,*,#15150,.F.);
#21000=ORIENTED_EDGE('',*,*,#15647,.F.);
#21001=ORIENTED_EDGE('',*,*,#15648,.T.);
#21002=ORIENTED_EDGE('',*,*,#15649,.F.);
#21003=ORIENTED_EDGE('',*,*,#15650,.T.);
#21004=ORIENTED_EDGE('',*,*,#15651,.F.);
#21005=ORIENTED_EDGE('',*,*,#15399,.F.);
#21006=ORIENTED_EDGE('',*,*,#15652,.F.);
#21007=ORIENTED_EDGE('',*,*,#15653,.T.);
#21008=ORIENTED_EDGE('',*,*,#15654,.F.);
#21009=ORIENTED_EDGE('',*,*,#15402,.F.);
#21010=ORIENTED_EDGE('',*,*,#15655,.F.);
#21011=ORIENTED_EDGE('',*,*,#15656,.T.);
#21012=ORIENTED_EDGE('',*,*,#15657,.F.);
#21013=ORIENTED_EDGE('',*,*,#15405,.F.);
#21014=ORIENTED_EDGE('',*,*,#15658,.F.);
#21015=ORIENTED_EDGE('',*,*,#15659,.T.);
#21016=ORIENTED_EDGE('',*,*,#15660,.F.);
#21017=ORIENTED_EDGE('',*,*,#15408,.F.);
#21018=ORIENTED_EDGE('',*,*,#15661,.F.);
#21019=ORIENTED_EDGE('',*,*,#15662,.T.);
#21020=ORIENTED_EDGE('',*,*,#15663,.F.);
#21021=ORIENTED_EDGE('',*,*,#15411,.F.);
#21022=ORIENTED_EDGE('',*,*,#15664,.F.);
#21023=ORIENTED_EDGE('',*,*,#15665,.T.);
#21024=ORIENTED_EDGE('',*,*,#15666,.F.);
#21025=ORIENTED_EDGE('',*,*,#15414,.F.);
#21026=ORIENTED_EDGE('',*,*,#15667,.F.);
#21027=ORIENTED_EDGE('',*,*,#15668,.T.);
#21028=ORIENTED_EDGE('',*,*,#15669,.F.);
#21029=ORIENTED_EDGE('',*,*,#15417,.F.);
#21030=ORIENTED_EDGE('',*,*,#15670,.F.);
#21031=ORIENTED_EDGE('',*,*,#15671,.T.);
#21032=ORIENTED_EDGE('',*,*,#15672,.F.);
#21033=ORIENTED_EDGE('',*,*,#15420,.F.);
#21034=ORIENTED_EDGE('',*,*,#15673,.F.);
#21035=ORIENTED_EDGE('',*,*,#15674,.T.);
#21036=ORIENTED_EDGE('',*,*,#15675,.F.);
#21037=ORIENTED_EDGE('',*,*,#15423,.F.);
#21038=ORIENTED_EDGE('',*,*,#15676,.F.);
#21039=ORIENTED_EDGE('',*,*,#15677,.T.);
#21040=ORIENTED_EDGE('',*,*,#15678,.F.);
#21041=ORIENTED_EDGE('',*,*,#15427,.F.);
#21042=ORIENTED_EDGE('',*,*,#15679,.F.);
#21043=ORIENTED_EDGE('',*,*,#15680,.T.);
#21044=ORIENTED_EDGE('',*,*,#15681,.F.);
#21045=ORIENTED_EDGE('',*,*,#15431,.F.);
#21046=ORIENTED_EDGE('',*,*,#15682,.F.);
#21047=ORIENTED_EDGE('',*,*,#15683,.T.);
#21048=ORIENTED_EDGE('',*,*,#15684,.F.);
#21049=ORIENTED_EDGE('',*,*,#15435,.F.);
#21050=ORIENTED_EDGE('',*,*,#15685,.F.);
#21051=ORIENTED_EDGE('',*,*,#15686,.T.);
#21052=ORIENTED_EDGE('',*,*,#15687,.F.);
#21053=ORIENTED_EDGE('',*,*,#15439,.F.);
#21054=ORIENTED_EDGE('',*,*,#15688,.F.);
#21055=ORIENTED_EDGE('',*,*,#15689,.T.);
#21056=ORIENTED_EDGE('',*,*,#15690,.F.);
#21057=ORIENTED_EDGE('',*,*,#15443,.F.);
#21058=ORIENTED_EDGE('',*,*,#15691,.F.);
#21059=ORIENTED_EDGE('',*,*,#15146,.F.);
#21060=ORIENTED_EDGE('',*,*,#15692,.F.);
#21061=ORIENTED_EDGE('',*,*,#15693,.T.);
#21062=ORIENTED_EDGE('',*,*,#15694,.F.);
#21063=ORIENTED_EDGE('',*,*,#15695,.T.);
#21064=ORIENTED_EDGE('',*,*,#15696,.F.);
#21065=ORIENTED_EDGE('',*,*,#15458,.F.);
#21066=ORIENTED_EDGE('',*,*,#15697,.F.);
#21067=ORIENTED_EDGE('',*,*,#15462,.F.);
#21068=ORIENTED_EDGE('',*,*,#15698,.F.);
#21069=ORIENTED_EDGE('',*,*,#15699,.T.);
#21070=ORIENTED_EDGE('',*,*,#15700,.F.);
#21071=ORIENTED_EDGE('',*,*,#15465,.F.);
#21072=ORIENTED_EDGE('',*,*,#15701,.F.);
#21073=ORIENTED_EDGE('',*,*,#15702,.T.);
#21074=ORIENTED_EDGE('',*,*,#15703,.F.);
#21075=ORIENTED_EDGE('',*,*,#15468,.F.);
#21076=ORIENTED_EDGE('',*,*,#15704,.F.);
#21077=ORIENTED_EDGE('',*,*,#15705,.T.);
#21078=ORIENTED_EDGE('',*,*,#15706,.F.);
#21079=ORIENTED_EDGE('',*,*,#15471,.F.);
#21080=ORIENTED_EDGE('',*,*,#15707,.F.);
#21081=ORIENTED_EDGE('',*,*,#15708,.T.);
#21082=ORIENTED_EDGE('',*,*,#15709,.F.);
#21083=ORIENTED_EDGE('',*,*,#15474,.F.);
#21084=ORIENTED_EDGE('',*,*,#15710,.F.);
#21085=ORIENTED_EDGE('',*,*,#15711,.T.);
#21086=ORIENTED_EDGE('',*,*,#15712,.F.);
#21087=ORIENTED_EDGE('',*,*,#15477,.F.);
#21088=ORIENTED_EDGE('',*,*,#15713,.F.);
#21089=ORIENTED_EDGE('',*,*,#15714,.T.);
#21090=ORIENTED_EDGE('',*,*,#15715,.F.);
#21091=ORIENTED_EDGE('',*,*,#15480,.F.);
#21092=ORIENTED_EDGE('',*,*,#15716,.F.);
#21093=ORIENTED_EDGE('',*,*,#15717,.T.);
#21094=ORIENTED_EDGE('',*,*,#15718,.F.);
#21095=ORIENTED_EDGE('',*,*,#15483,.F.);
#21096=ORIENTED_EDGE('',*,*,#15719,.F.);
#21097=ORIENTED_EDGE('',*,*,#15720,.T.);
#21098=ORIENTED_EDGE('',*,*,#15721,.F.);
#21099=ORIENTED_EDGE('',*,*,#15486,.F.);
#21100=ORIENTED_EDGE('',*,*,#15722,.F.);
#21101=ORIENTED_EDGE('',*,*,#15723,.T.);
#21102=ORIENTED_EDGE('',*,*,#15724,.F.);
#21103=ORIENTED_EDGE('',*,*,#15489,.F.);
#21104=ORIENTED_EDGE('',*,*,#15725,.F.);
#21105=ORIENTED_EDGE('',*,*,#15726,.T.);
#21106=ORIENTED_EDGE('',*,*,#15727,.F.);
#21107=ORIENTED_EDGE('',*,*,#15492,.F.);
#21108=ORIENTED_EDGE('',*,*,#15728,.F.);
#21109=ORIENTED_EDGE('',*,*,#15729,.T.);
#21110=ORIENTED_EDGE('',*,*,#15730,.F.);
#21111=ORIENTED_EDGE('',*,*,#15495,.F.);
#21112=ORIENTED_EDGE('',*,*,#15731,.F.);
#21113=ORIENTED_EDGE('',*,*,#15732,.T.);
#21114=ORIENTED_EDGE('',*,*,#15733,.F.);
#21115=ORIENTED_EDGE('',*,*,#15498,.F.);
#21116=ORIENTED_EDGE('',*,*,#15734,.F.);
#21117=ORIENTED_EDGE('',*,*,#15735,.T.);
#21118=ORIENTED_EDGE('',*,*,#15736,.F.);
#21119=ORIENTED_EDGE('',*,*,#15501,.F.);
#21120=ORIENTED_EDGE('',*,*,#15737,.F.);
#21121=ORIENTED_EDGE('',*,*,#15738,.T.);
#21122=ORIENTED_EDGE('',*,*,#15739,.F.);
#21123=ORIENTED_EDGE('',*,*,#15504,.F.);
#21124=ORIENTED_EDGE('',*,*,#15740,.F.);
#21125=ORIENTED_EDGE('',*,*,#15741,.T.);
#21126=ORIENTED_EDGE('',*,*,#15742,.F.);
#21127=ORIENTED_EDGE('',*,*,#15507,.F.);
#21128=ORIENTED_EDGE('',*,*,#15743,.F.);
#21129=ORIENTED_EDGE('',*,*,#15744,.T.);
#21130=ORIENTED_EDGE('',*,*,#15745,.F.);
#21131=ORIENTED_EDGE('',*,*,#15510,.F.);
#21132=ORIENTED_EDGE('',*,*,#15746,.F.);
#21133=ORIENTED_EDGE('',*,*,#15747,.T.);
#21134=ORIENTED_EDGE('',*,*,#15748,.F.);
#21135=ORIENTED_EDGE('',*,*,#15513,.F.);
#21136=ORIENTED_EDGE('',*,*,#15749,.F.);
#21137=ORIENTED_EDGE('',*,*,#15750,.T.);
#21138=ORIENTED_EDGE('',*,*,#15751,.F.);
#21139=ORIENTED_EDGE('',*,*,#15516,.F.);
#21140=ORIENTED_EDGE('',*,*,#15752,.F.);
#21141=ORIENTED_EDGE('',*,*,#15753,.T.);
#21142=ORIENTED_EDGE('',*,*,#15754,.F.);
#21143=ORIENTED_EDGE('',*,*,#15519,.F.);
#21144=ORIENTED_EDGE('',*,*,#15755,.F.);
#21145=ORIENTED_EDGE('',*,*,#15756,.T.);
#21146=ORIENTED_EDGE('',*,*,#15757,.F.);
#21147=ORIENTED_EDGE('',*,*,#15522,.F.);
#21148=ORIENTED_EDGE('',*,*,#15758,.F.);
#21149=ORIENTED_EDGE('',*,*,#15759,.T.);
#21150=ORIENTED_EDGE('',*,*,#15760,.F.);
#21151=ORIENTED_EDGE('',*,*,#15525,.F.);
#21152=ORIENTED_EDGE('',*,*,#15761,.F.);
#21153=ORIENTED_EDGE('',*,*,#15762,.T.);
#21154=ORIENTED_EDGE('',*,*,#15763,.F.);
#21155=ORIENTED_EDGE('',*,*,#15528,.F.);
#21156=ORIENTED_EDGE('',*,*,#15764,.F.);
#21157=ORIENTED_EDGE('',*,*,#15765,.T.);
#21158=ORIENTED_EDGE('',*,*,#15766,.F.);
#21159=ORIENTED_EDGE('',*,*,#15531,.F.);
#21160=ORIENTED_EDGE('',*,*,#15767,.F.);
#21161=ORIENTED_EDGE('',*,*,#15768,.T.);
#21162=ORIENTED_EDGE('',*,*,#15769,.F.);
#21163=ORIENTED_EDGE('',*,*,#15534,.F.);
#21164=ORIENTED_EDGE('',*,*,#15770,.F.);
#21165=ORIENTED_EDGE('',*,*,#15771,.T.);
#21166=ORIENTED_EDGE('',*,*,#15772,.F.);
#21167=ORIENTED_EDGE('',*,*,#15537,.F.);
#21168=ORIENTED_EDGE('',*,*,#15773,.F.);
#21169=ORIENTED_EDGE('',*,*,#15774,.T.);
#21170=ORIENTED_EDGE('',*,*,#15775,.F.);
#21171=ORIENTED_EDGE('',*,*,#15540,.F.);
#21172=ORIENTED_EDGE('',*,*,#15776,.F.);
#21173=ORIENTED_EDGE('',*,*,#15777,.T.);
#21174=ORIENTED_EDGE('',*,*,#15778,.F.);
#21175=ORIENTED_EDGE('',*,*,#15543,.F.);
#21176=ORIENTED_EDGE('',*,*,#15779,.F.);
#21177=ORIENTED_EDGE('',*,*,#15780,.T.);
#21178=ORIENTED_EDGE('',*,*,#15781,.F.);
#21179=ORIENTED_EDGE('',*,*,#15546,.F.);
#21180=ORIENTED_EDGE('',*,*,#15782,.F.);
#21181=ORIENTED_EDGE('',*,*,#15783,.T.);
#21182=ORIENTED_EDGE('',*,*,#15784,.F.);
#21183=ORIENTED_EDGE('',*,*,#15549,.F.);
#21184=ORIENTED_EDGE('',*,*,#15785,.F.);
#21185=ORIENTED_EDGE('',*,*,#15786,.T.);
#21186=ORIENTED_EDGE('',*,*,#15787,.F.);
#21187=ORIENTED_EDGE('',*,*,#15552,.F.);
#21188=ORIENTED_EDGE('',*,*,#15788,.F.);
#21189=ORIENTED_EDGE('',*,*,#15789,.T.);
#21190=ORIENTED_EDGE('',*,*,#15790,.F.);
#21191=ORIENTED_EDGE('',*,*,#15555,.F.);
#21192=ORIENTED_EDGE('',*,*,#15791,.F.);
#21193=ORIENTED_EDGE('',*,*,#15792,.T.);
#21194=ORIENTED_EDGE('',*,*,#15793,.F.);
#21195=ORIENTED_EDGE('',*,*,#15558,.F.);
#21196=ORIENTED_EDGE('',*,*,#15794,.F.);
#21197=ORIENTED_EDGE('',*,*,#15795,.T.);
#21198=ORIENTED_EDGE('',*,*,#15796,.F.);
#21199=ORIENTED_EDGE('',*,*,#15561,.F.);
#21200=ORIENTED_EDGE('',*,*,#15797,.F.);
#21201=ORIENTED_EDGE('',*,*,#15798,.T.);
#21202=ORIENTED_EDGE('',*,*,#15799,.F.);
#21203=ORIENTED_EDGE('',*,*,#15564,.F.);
#21204=ORIENTED_EDGE('',*,*,#15800,.F.);
#21205=ORIENTED_EDGE('',*,*,#15801,.T.);
#21206=ORIENTED_EDGE('',*,*,#15802,.F.);
#21207=ORIENTED_EDGE('',*,*,#15567,.F.);
#21208=ORIENTED_EDGE('',*,*,#15803,.F.);
#21209=ORIENTED_EDGE('',*,*,#15804,.T.);
#21210=ORIENTED_EDGE('',*,*,#15805,.F.);
#21211=ORIENTED_EDGE('',*,*,#15570,.F.);
#21212=ORIENTED_EDGE('',*,*,#15806,.F.);
#21213=ORIENTED_EDGE('',*,*,#15807,.T.);
#21214=ORIENTED_EDGE('',*,*,#15808,.F.);
#21215=ORIENTED_EDGE('',*,*,#15573,.F.);
#21216=ORIENTED_EDGE('',*,*,#15809,.F.);
#21217=ORIENTED_EDGE('',*,*,#15810,.T.);
#21218=ORIENTED_EDGE('',*,*,#15811,.F.);
#21219=ORIENTED_EDGE('',*,*,#15576,.F.);
#21220=ORIENTED_EDGE('',*,*,#15812,.F.);
#21221=ORIENTED_EDGE('',*,*,#15813,.T.);
#21222=ORIENTED_EDGE('',*,*,#15814,.F.);
#21223=ORIENTED_EDGE('',*,*,#15579,.F.);
#21224=ORIENTED_EDGE('',*,*,#15815,.F.);
#21225=ORIENTED_EDGE('',*,*,#15816,.T.);
#21226=ORIENTED_EDGE('',*,*,#15817,.F.);
#21227=ORIENTED_EDGE('',*,*,#15582,.F.);
#21228=ORIENTED_EDGE('',*,*,#15818,.F.);
#21229=ORIENTED_EDGE('',*,*,#15819,.T.);
#21230=ORIENTED_EDGE('',*,*,#15820,.F.);
#21231=ORIENTED_EDGE('',*,*,#15585,.F.);
#21232=ORIENTED_EDGE('',*,*,#15821,.F.);
#21233=ORIENTED_EDGE('',*,*,#15822,.T.);
#21234=ORIENTED_EDGE('',*,*,#15823,.F.);
#21235=ORIENTED_EDGE('',*,*,#15588,.F.);
#21236=ORIENTED_EDGE('',*,*,#15824,.F.);
#21237=ORIENTED_EDGE('',*,*,#15825,.T.);
#21238=ORIENTED_EDGE('',*,*,#15826,.F.);
#21239=ORIENTED_EDGE('',*,*,#15591,.F.);
#21240=ORIENTED_EDGE('',*,*,#15827,.F.);
#21241=ORIENTED_EDGE('',*,*,#15828,.T.);
#21242=ORIENTED_EDGE('',*,*,#15829,.F.);
#21243=ORIENTED_EDGE('',*,*,#15594,.F.);
#21244=ORIENTED_EDGE('',*,*,#15830,.F.);
#21245=ORIENTED_EDGE('',*,*,#15831,.T.);
#21246=ORIENTED_EDGE('',*,*,#15832,.F.);
#21247=ORIENTED_EDGE('',*,*,#15597,.F.);
#21248=ORIENTED_EDGE('',*,*,#15833,.F.);
#21249=ORIENTED_EDGE('',*,*,#15834,.T.);
#21250=ORIENTED_EDGE('',*,*,#15835,.F.);
#21251=ORIENTED_EDGE('',*,*,#15600,.F.);
#21252=ORIENTED_EDGE('',*,*,#15836,.F.);
#21253=ORIENTED_EDGE('',*,*,#15837,.T.);
#21254=ORIENTED_EDGE('',*,*,#15838,.F.);
#21255=ORIENTED_EDGE('',*,*,#15603,.F.);
#21256=ORIENTED_EDGE('',*,*,#15839,.F.);
#21257=ORIENTED_EDGE('',*,*,#15840,.T.);
#21258=ORIENTED_EDGE('',*,*,#15841,.F.);
#21259=ORIENTED_EDGE('',*,*,#15606,.F.);
#21260=ORIENTED_EDGE('',*,*,#15842,.F.);
#21261=ORIENTED_EDGE('',*,*,#15843,.T.);
#21262=ORIENTED_EDGE('',*,*,#15844,.F.);
#21263=ORIENTED_EDGE('',*,*,#15609,.F.);
#21264=ORIENTED_EDGE('',*,*,#15845,.F.);
#21265=ORIENTED_EDGE('',*,*,#15846,.T.);
#21266=ORIENTED_EDGE('',*,*,#15847,.F.);
#21267=ORIENTED_EDGE('',*,*,#15612,.F.);
#21268=ORIENTED_EDGE('',*,*,#15848,.F.);
#21269=ORIENTED_EDGE('',*,*,#15849,.T.);
#21270=ORIENTED_EDGE('',*,*,#15850,.F.);
#21271=ORIENTED_EDGE('',*,*,#15615,.F.);
#21272=ORIENTED_EDGE('',*,*,#15851,.F.);
#21273=ORIENTED_EDGE('',*,*,#15852,.T.);
#21274=ORIENTED_EDGE('',*,*,#15853,.F.);
#21275=ORIENTED_EDGE('',*,*,#15618,.F.);
#21276=ORIENTED_EDGE('',*,*,#15854,.F.);
#21277=ORIENTED_EDGE('',*,*,#15855,.T.);
#21278=ORIENTED_EDGE('',*,*,#15856,.F.);
#21279=ORIENTED_EDGE('',*,*,#15621,.F.);
#21280=ORIENTED_EDGE('',*,*,#15857,.F.);
#21281=ORIENTED_EDGE('',*,*,#15858,.T.);
#21282=ORIENTED_EDGE('',*,*,#15859,.F.);
#21283=ORIENTED_EDGE('',*,*,#15624,.F.);
#21284=ORIENTED_EDGE('',*,*,#15860,.F.);
#21285=ORIENTED_EDGE('',*,*,#15861,.T.);
#21286=ORIENTED_EDGE('',*,*,#15862,.F.);
#21287=ORIENTED_EDGE('',*,*,#15627,.F.);
#21288=ORIENTED_EDGE('',*,*,#15863,.F.);
#21289=ORIENTED_EDGE('',*,*,#15864,.T.);
#21290=ORIENTED_EDGE('',*,*,#15865,.F.);
#21291=ORIENTED_EDGE('',*,*,#15630,.F.);
#21292=ORIENTED_EDGE('',*,*,#15866,.F.);
#21293=ORIENTED_EDGE('',*,*,#15867,.T.);
#21294=ORIENTED_EDGE('',*,*,#15868,.F.);
#21295=ORIENTED_EDGE('',*,*,#15633,.F.);
#21296=ORIENTED_EDGE('',*,*,#15869,.F.);
#21297=ORIENTED_EDGE('',*,*,#15870,.T.);
#21298=ORIENTED_EDGE('',*,*,#15871,.F.);
#21299=ORIENTED_EDGE('',*,*,#15636,.F.);
#21300=ORIENTED_EDGE('',*,*,#15872,.F.);
#21301=ORIENTED_EDGE('',*,*,#15873,.T.);
#21302=ORIENTED_EDGE('',*,*,#15874,.F.);
#21303=ORIENTED_EDGE('',*,*,#15639,.F.);
#21304=ORIENTED_EDGE('',*,*,#15875,.F.);
#21305=ORIENTED_EDGE('',*,*,#15876,.T.);
#21306=ORIENTED_EDGE('',*,*,#15877,.F.);
#21307=ORIENTED_EDGE('',*,*,#15642,.F.);
#21308=ORIENTED_EDGE('',*,*,#15878,.F.);
#21309=ORIENTED_EDGE('',*,*,#15879,.T.);
#21310=ORIENTED_EDGE('',*,*,#15880,.F.);
#21311=ORIENTED_EDGE('',*,*,#15645,.F.);
#21312=ORIENTED_EDGE('',*,*,#15881,.F.);
#21313=ORIENTED_EDGE('',*,*,#15882,.T.);
#21314=ORIENTED_EDGE('',*,*,#15883,.F.);
#21315=ORIENTED_EDGE('',*,*,#15648,.F.);
#21316=ORIENTED_EDGE('',*,*,#15884,.F.);
#21317=ORIENTED_EDGE('',*,*,#15885,.T.);
#21318=ORIENTED_EDGE('',*,*,#15886,.F.);
#21319=ORIENTED_EDGE('',*,*,#15887,.T.);
#21320=ORIENTED_EDGE('',*,*,#15888,.F.);
#21321=ORIENTED_EDGE('',*,*,#15650,.F.);
#21322=ORIENTED_EDGE('',*,*,#15889,.F.);
#21323=ORIENTED_EDGE('',*,*,#15890,.T.);
#21324=ORIENTED_EDGE('',*,*,#15891,.F.);
#21325=ORIENTED_EDGE('',*,*,#15653,.F.);
#21326=ORIENTED_EDGE('',*,*,#15892,.F.);
#21327=ORIENTED_EDGE('',*,*,#15893,.T.);
#21328=ORIENTED_EDGE('',*,*,#15894,.F.);
#21329=ORIENTED_EDGE('',*,*,#15656,.F.);
#21330=ORIENTED_EDGE('',*,*,#15895,.F.);
#21331=ORIENTED_EDGE('',*,*,#15896,.T.);
#21332=ORIENTED_EDGE('',*,*,#15897,.F.);
#21333=ORIENTED_EDGE('',*,*,#15659,.F.);
#21334=ORIENTED_EDGE('',*,*,#15898,.F.);
#21335=ORIENTED_EDGE('',*,*,#15899,.T.);
#21336=ORIENTED_EDGE('',*,*,#15900,.F.);
#21337=ORIENTED_EDGE('',*,*,#15662,.F.);
#21338=ORIENTED_EDGE('',*,*,#15901,.F.);
#21339=ORIENTED_EDGE('',*,*,#15902,.T.);
#21340=ORIENTED_EDGE('',*,*,#15903,.F.);
#21341=ORIENTED_EDGE('',*,*,#15665,.F.);
#21342=ORIENTED_EDGE('',*,*,#15904,.F.);
#21343=ORIENTED_EDGE('',*,*,#15905,.T.);
#21344=ORIENTED_EDGE('',*,*,#15906,.F.);
#21345=ORIENTED_EDGE('',*,*,#15668,.F.);
#21346=ORIENTED_EDGE('',*,*,#15907,.F.);
#21347=ORIENTED_EDGE('',*,*,#15908,.T.);
#21348=ORIENTED_EDGE('',*,*,#15909,.F.);
#21349=ORIENTED_EDGE('',*,*,#15671,.F.);
#21350=ORIENTED_EDGE('',*,*,#15910,.F.);
#21351=ORIENTED_EDGE('',*,*,#15911,.T.);
#21352=ORIENTED_EDGE('',*,*,#15912,.F.);
#21353=ORIENTED_EDGE('',*,*,#15674,.F.);
#21354=ORIENTED_EDGE('',*,*,#15913,.F.);
#21355=ORIENTED_EDGE('',*,*,#15914,.T.);
#21356=ORIENTED_EDGE('',*,*,#15915,.F.);
#21357=ORIENTED_EDGE('',*,*,#15677,.F.);
#21358=ORIENTED_EDGE('',*,*,#15916,.F.);
#21359=ORIENTED_EDGE('',*,*,#15917,.T.);
#21360=ORIENTED_EDGE('',*,*,#15918,.F.);
#21361=ORIENTED_EDGE('',*,*,#15680,.F.);
#21362=ORIENTED_EDGE('',*,*,#15919,.F.);
#21363=ORIENTED_EDGE('',*,*,#15920,.T.);
#21364=ORIENTED_EDGE('',*,*,#15921,.F.);
#21365=ORIENTED_EDGE('',*,*,#15683,.F.);
#21366=ORIENTED_EDGE('',*,*,#15922,.F.);
#21367=ORIENTED_EDGE('',*,*,#15923,.T.);
#21368=ORIENTED_EDGE('',*,*,#15924,.F.);
#21369=ORIENTED_EDGE('',*,*,#15686,.F.);
#21370=ORIENTED_EDGE('',*,*,#15925,.F.);
#21371=ORIENTED_EDGE('',*,*,#15926,.T.);
#21372=ORIENTED_EDGE('',*,*,#15927,.F.);
#21373=ORIENTED_EDGE('',*,*,#15689,.F.);
#21374=ORIENTED_EDGE('',*,*,#15928,.F.);
#21375=ORIENTED_EDGE('',*,*,#15693,.F.);
#21376=ORIENTED_EDGE('',*,*,#15929,.F.);
#21377=ORIENTED_EDGE('',*,*,#15930,.T.);
#21378=ORIENTED_EDGE('',*,*,#15931,.F.);
#21379=ORIENTED_EDGE('',*,*,#15042,.T.);
#21380=ORIENTED_EDGE('',*,*,#15932,.F.);
#21381=ORIENTED_EDGE('',*,*,#15695,.F.);
#21382=ORIENTED_EDGE('',*,*,#15933,.F.);
#21383=ORIENTED_EDGE('',*,*,#15699,.F.);
#21384=ORIENTED_EDGE('',*,*,#15934,.F.);
#21385=ORIENTED_EDGE('',*,*,#15045,.T.);
#21386=ORIENTED_EDGE('',*,*,#15935,.F.);
#21387=ORIENTED_EDGE('',*,*,#15702,.F.);
#21388=ORIENTED_EDGE('',*,*,#15936,.F.);
#21389=ORIENTED_EDGE('',*,*,#15048,.T.);
#21390=ORIENTED_EDGE('',*,*,#15937,.F.);
#21391=ORIENTED_EDGE('',*,*,#15705,.F.);
#21392=ORIENTED_EDGE('',*,*,#15938,.F.);
#21393=ORIENTED_EDGE('',*,*,#15051,.T.);
#21394=ORIENTED_EDGE('',*,*,#15939,.F.);
#21395=ORIENTED_EDGE('',*,*,#15708,.F.);
#21396=ORIENTED_EDGE('',*,*,#15940,.F.);
#21397=ORIENTED_EDGE('',*,*,#15054,.T.);
#21398=ORIENTED_EDGE('',*,*,#15941,.F.);
#21399=ORIENTED_EDGE('',*,*,#15711,.F.);
#21400=ORIENTED_EDGE('',*,*,#15942,.F.);
#21401=ORIENTED_EDGE('',*,*,#15057,.T.);
#21402=ORIENTED_EDGE('',*,*,#15943,.F.);
#21403=ORIENTED_EDGE('',*,*,#15714,.F.);
#21404=ORIENTED_EDGE('',*,*,#15944,.F.);
#21405=ORIENTED_EDGE('',*,*,#15060,.T.);
#21406=ORIENTED_EDGE('',*,*,#15945,.F.);
#21407=ORIENTED_EDGE('',*,*,#15717,.F.);
#21408=ORIENTED_EDGE('',*,*,#15946,.F.);
#21409=ORIENTED_EDGE('',*,*,#15064,.T.);
#21410=ORIENTED_EDGE('',*,*,#15947,.F.);
#21411=ORIENTED_EDGE('',*,*,#15720,.F.);
#21412=ORIENTED_EDGE('',*,*,#15948,.F.);
#21413=ORIENTED_EDGE('',*,*,#15068,.T.);
#21414=ORIENTED_EDGE('',*,*,#15949,.F.);
#21415=ORIENTED_EDGE('',*,*,#15723,.F.);
#21416=ORIENTED_EDGE('',*,*,#15950,.F.);
#21417=ORIENTED_EDGE('',*,*,#15072,.T.);
#21418=ORIENTED_EDGE('',*,*,#15951,.F.);
#21419=ORIENTED_EDGE('',*,*,#15726,.F.);
#21420=ORIENTED_EDGE('',*,*,#15952,.F.);
#21421=ORIENTED_EDGE('',*,*,#15076,.T.);
#21422=ORIENTED_EDGE('',*,*,#15953,.F.);
#21423=ORIENTED_EDGE('',*,*,#15729,.F.);
#21424=ORIENTED_EDGE('',*,*,#15954,.F.);
#21425=ORIENTED_EDGE('',*,*,#15080,.T.);
#21426=ORIENTED_EDGE('',*,*,#15955,.F.);
#21427=ORIENTED_EDGE('',*,*,#15732,.F.);
#21428=ORIENTED_EDGE('',*,*,#15956,.F.);
#21429=ORIENTED_EDGE('',*,*,#15084,.T.);
#21430=ORIENTED_EDGE('',*,*,#15957,.F.);
#21431=ORIENTED_EDGE('',*,*,#15735,.F.);
#21432=ORIENTED_EDGE('',*,*,#15958,.F.);
#21433=ORIENTED_EDGE('',*,*,#15088,.T.);
#21434=ORIENTED_EDGE('',*,*,#15959,.F.);
#21435=ORIENTED_EDGE('',*,*,#15738,.F.);
#21436=ORIENTED_EDGE('',*,*,#15960,.F.);
#21437=ORIENTED_EDGE('',*,*,#15092,.T.);
#21438=ORIENTED_EDGE('',*,*,#15961,.F.);
#21439=ORIENTED_EDGE('',*,*,#15741,.F.);
#21440=ORIENTED_EDGE('',*,*,#15962,.F.);
#21441=ORIENTED_EDGE('',*,*,#15096,.T.);
#21442=ORIENTED_EDGE('',*,*,#15963,.F.);
#21443=ORIENTED_EDGE('',*,*,#15744,.F.);
#21444=ORIENTED_EDGE('',*,*,#15964,.F.);
#21445=ORIENTED_EDGE('',*,*,#15100,.T.);
#21446=ORIENTED_EDGE('',*,*,#15965,.F.);
#21447=ORIENTED_EDGE('',*,*,#15747,.F.);
#21448=ORIENTED_EDGE('',*,*,#15966,.F.);
#21449=ORIENTED_EDGE('',*,*,#15104,.T.);
#21450=ORIENTED_EDGE('',*,*,#15967,.F.);
#21451=ORIENTED_EDGE('',*,*,#15750,.F.);
#21452=ORIENTED_EDGE('',*,*,#15968,.F.);
#21453=ORIENTED_EDGE('',*,*,#15108,.T.);
#21454=ORIENTED_EDGE('',*,*,#15969,.F.);
#21455=ORIENTED_EDGE('',*,*,#15753,.F.);
#21456=ORIENTED_EDGE('',*,*,#15970,.F.);
#21457=ORIENTED_EDGE('',*,*,#15112,.T.);
#21458=ORIENTED_EDGE('',*,*,#15971,.F.);
#21459=ORIENTED_EDGE('',*,*,#15756,.F.);
#21460=ORIENTED_EDGE('',*,*,#15972,.F.);
#21461=ORIENTED_EDGE('',*,*,#15116,.T.);
#21462=ORIENTED_EDGE('',*,*,#15973,.F.);
#21463=ORIENTED_EDGE('',*,*,#15759,.F.);
#21464=ORIENTED_EDGE('',*,*,#15974,.F.);
#21465=ORIENTED_EDGE('',*,*,#15120,.T.);
#21466=ORIENTED_EDGE('',*,*,#15975,.F.);
#21467=ORIENTED_EDGE('',*,*,#15762,.F.);
#21468=ORIENTED_EDGE('',*,*,#15976,.F.);
#21469=ORIENTED_EDGE('',*,*,#15124,.T.);
#21470=ORIENTED_EDGE('',*,*,#15977,.F.);
#21471=ORIENTED_EDGE('',*,*,#15765,.F.);
#21472=ORIENTED_EDGE('',*,*,#15978,.F.);
#21473=ORIENTED_EDGE('',*,*,#15128,.T.);
#21474=ORIENTED_EDGE('',*,*,#15979,.F.);
#21475=ORIENTED_EDGE('',*,*,#15768,.F.);
#21476=ORIENTED_EDGE('',*,*,#15980,.F.);
#21477=ORIENTED_EDGE('',*,*,#15132,.T.);
#21478=ORIENTED_EDGE('',*,*,#15981,.F.);
#21479=ORIENTED_EDGE('',*,*,#15771,.F.);
#21480=ORIENTED_EDGE('',*,*,#15982,.F.);
#21481=ORIENTED_EDGE('',*,*,#15136,.T.);
#21482=ORIENTED_EDGE('',*,*,#15983,.F.);
#21483=ORIENTED_EDGE('',*,*,#15774,.F.);
#21484=ORIENTED_EDGE('',*,*,#15984,.F.);
#21485=ORIENTED_EDGE('',*,*,#14835,.T.);
#21486=ORIENTED_EDGE('',*,*,#15985,.F.);
#21487=ORIENTED_EDGE('',*,*,#15777,.F.);
#21488=ORIENTED_EDGE('',*,*,#15986,.F.);
#21489=ORIENTED_EDGE('',*,*,#14839,.T.);
#21490=ORIENTED_EDGE('',*,*,#15987,.F.);
#21491=ORIENTED_EDGE('',*,*,#15780,.F.);
#21492=ORIENTED_EDGE('',*,*,#15988,.F.);
#21493=ORIENTED_EDGE('',*,*,#14843,.T.);
#21494=ORIENTED_EDGE('',*,*,#15989,.F.);
#21495=ORIENTED_EDGE('',*,*,#15783,.F.);
#21496=ORIENTED_EDGE('',*,*,#15990,.F.);
#21497=ORIENTED_EDGE('',*,*,#14847,.T.);
#21498=ORIENTED_EDGE('',*,*,#15991,.F.);
#21499=ORIENTED_EDGE('',*,*,#15786,.F.);
#21500=ORIENTED_EDGE('',*,*,#15992,.F.);
#21501=ORIENTED_EDGE('',*,*,#14851,.T.);
#21502=ORIENTED_EDGE('',*,*,#15993,.F.);
#21503=ORIENTED_EDGE('',*,*,#15789,.F.);
#21504=ORIENTED_EDGE('',*,*,#15994,.F.);
#21505=ORIENTED_EDGE('',*,*,#14855,.T.);
#21506=ORIENTED_EDGE('',*,*,#15995,.F.);
#21507=ORIENTED_EDGE('',*,*,#15792,.F.);
#21508=ORIENTED_EDGE('',*,*,#15996,.F.);
#21509=ORIENTED_EDGE('',*,*,#14859,.T.);
#21510=ORIENTED_EDGE('',*,*,#15997,.F.);
#21511=ORIENTED_EDGE('',*,*,#15795,.F.);
#21512=ORIENTED_EDGE('',*,*,#15998,.F.);
#21513=ORIENTED_EDGE('',*,*,#14863,.T.);
#21514=ORIENTED_EDGE('',*,*,#15999,.F.);
#21515=ORIENTED_EDGE('',*,*,#15798,.F.);
#21516=ORIENTED_EDGE('',*,*,#16000,.F.);
#21517=ORIENTED_EDGE('',*,*,#14867,.T.);
#21518=ORIENTED_EDGE('',*,*,#16001,.F.);
#21519=ORIENTED_EDGE('',*,*,#15801,.F.);
#21520=ORIENTED_EDGE('',*,*,#16002,.F.);
#21521=ORIENTED_EDGE('',*,*,#14871,.T.);
#21522=ORIENTED_EDGE('',*,*,#16003,.F.);
#21523=ORIENTED_EDGE('',*,*,#15804,.F.);
#21524=ORIENTED_EDGE('',*,*,#16004,.F.);
#21525=ORIENTED_EDGE('',*,*,#14875,.T.);
#21526=ORIENTED_EDGE('',*,*,#16005,.F.);
#21527=ORIENTED_EDGE('',*,*,#15807,.F.);
#21528=ORIENTED_EDGE('',*,*,#16006,.F.);
#21529=ORIENTED_EDGE('',*,*,#14879,.T.);
#21530=ORIENTED_EDGE('',*,*,#16007,.F.);
#21531=ORIENTED_EDGE('',*,*,#15810,.F.);
#21532=ORIENTED_EDGE('',*,*,#16008,.F.);
#21533=ORIENTED_EDGE('',*,*,#14883,.T.);
#21534=ORIENTED_EDGE('',*,*,#16009,.F.);
#21535=ORIENTED_EDGE('',*,*,#15813,.F.);
#21536=ORIENTED_EDGE('',*,*,#16010,.F.);
#21537=ORIENTED_EDGE('',*,*,#14887,.T.);
#21538=ORIENTED_EDGE('',*,*,#16011,.F.);
#21539=ORIENTED_EDGE('',*,*,#15816,.F.);
#21540=ORIENTED_EDGE('',*,*,#16012,.F.);
#21541=ORIENTED_EDGE('',*,*,#14891,.T.);
#21542=ORIENTED_EDGE('',*,*,#16013,.F.);
#21543=ORIENTED_EDGE('',*,*,#15819,.F.);
#21544=ORIENTED_EDGE('',*,*,#16014,.F.);
#21545=ORIENTED_EDGE('',*,*,#14895,.T.);
#21546=ORIENTED_EDGE('',*,*,#16015,.F.);
#21547=ORIENTED_EDGE('',*,*,#15822,.F.);
#21548=ORIENTED_EDGE('',*,*,#16016,.F.);
#21549=ORIENTED_EDGE('',*,*,#14899,.T.);
#21550=ORIENTED_EDGE('',*,*,#16017,.F.);
#21551=ORIENTED_EDGE('',*,*,#15825,.F.);
#21552=ORIENTED_EDGE('',*,*,#16018,.F.);
#21553=ORIENTED_EDGE('',*,*,#14903,.T.);
#21554=ORIENTED_EDGE('',*,*,#16019,.F.);
#21555=ORIENTED_EDGE('',*,*,#15828,.F.);
#21556=ORIENTED_EDGE('',*,*,#16020,.F.);
#21557=ORIENTED_EDGE('',*,*,#14907,.T.);
#21558=ORIENTED_EDGE('',*,*,#16021,.F.);
#21559=ORIENTED_EDGE('',*,*,#15831,.F.);
#21560=ORIENTED_EDGE('',*,*,#16022,.F.);
#21561=ORIENTED_EDGE('',*,*,#14911,.T.);
#21562=ORIENTED_EDGE('',*,*,#16023,.F.);
#21563=ORIENTED_EDGE('',*,*,#15834,.F.);
#21564=ORIENTED_EDGE('',*,*,#16024,.F.);
#21565=ORIENTED_EDGE('',*,*,#14915,.T.);
#21566=ORIENTED_EDGE('',*,*,#16025,.F.);
#21567=ORIENTED_EDGE('',*,*,#15837,.F.);
#21568=ORIENTED_EDGE('',*,*,#16026,.F.);
#21569=ORIENTED_EDGE('',*,*,#14919,.T.);
#21570=ORIENTED_EDGE('',*,*,#16027,.F.);
#21571=ORIENTED_EDGE('',*,*,#15840,.F.);
#21572=ORIENTED_EDGE('',*,*,#16028,.F.);
#21573=ORIENTED_EDGE('',*,*,#14923,.T.);
#21574=ORIENTED_EDGE('',*,*,#16029,.F.);
#21575=ORIENTED_EDGE('',*,*,#15843,.F.);
#21576=ORIENTED_EDGE('',*,*,#16030,.F.);
#21577=ORIENTED_EDGE('',*,*,#14927,.T.);
#21578=ORIENTED_EDGE('',*,*,#16031,.F.);
#21579=ORIENTED_EDGE('',*,*,#15846,.F.);
#21580=ORIENTED_EDGE('',*,*,#16032,.F.);
#21581=ORIENTED_EDGE('',*,*,#14931,.T.);
#21582=ORIENTED_EDGE('',*,*,#16033,.F.);
#21583=ORIENTED_EDGE('',*,*,#15849,.F.);
#21584=ORIENTED_EDGE('',*,*,#16034,.F.);
#21585=ORIENTED_EDGE('',*,*,#14935,.T.);
#21586=ORIENTED_EDGE('',*,*,#16035,.F.);
#21587=ORIENTED_EDGE('',*,*,#15852,.F.);
#21588=ORIENTED_EDGE('',*,*,#16036,.F.);
#21589=ORIENTED_EDGE('',*,*,#14939,.T.);
#21590=ORIENTED_EDGE('',*,*,#16037,.F.);
#21591=ORIENTED_EDGE('',*,*,#15855,.F.);
#21592=ORIENTED_EDGE('',*,*,#16038,.F.);
#21593=ORIENTED_EDGE('',*,*,#14943,.T.);
#21594=ORIENTED_EDGE('',*,*,#16039,.F.);
#21595=ORIENTED_EDGE('',*,*,#15858,.F.);
#21596=ORIENTED_EDGE('',*,*,#16040,.F.);
#21597=ORIENTED_EDGE('',*,*,#14947,.T.);
#21598=ORIENTED_EDGE('',*,*,#16041,.F.);
#21599=ORIENTED_EDGE('',*,*,#15861,.F.);
#21600=ORIENTED_EDGE('',*,*,#16042,.F.);
#21601=ORIENTED_EDGE('',*,*,#14951,.T.);
#21602=ORIENTED_EDGE('',*,*,#16043,.F.);
#21603=ORIENTED_EDGE('',*,*,#15864,.F.);
#21604=ORIENTED_EDGE('',*,*,#16044,.F.);
#21605=ORIENTED_EDGE('',*,*,#14955,.T.);
#21606=ORIENTED_EDGE('',*,*,#16045,.F.);
#21607=ORIENTED_EDGE('',*,*,#15867,.F.);
#21608=ORIENTED_EDGE('',*,*,#16046,.F.);
#21609=ORIENTED_EDGE('',*,*,#14959,.T.);
#21610=ORIENTED_EDGE('',*,*,#16047,.F.);
#21611=ORIENTED_EDGE('',*,*,#15870,.F.);
#21612=ORIENTED_EDGE('',*,*,#16048,.F.);
#21613=ORIENTED_EDGE('',*,*,#14963,.T.);
#21614=ORIENTED_EDGE('',*,*,#16049,.F.);
#21615=ORIENTED_EDGE('',*,*,#15873,.F.);
#21616=ORIENTED_EDGE('',*,*,#16050,.F.);
#21617=ORIENTED_EDGE('',*,*,#14967,.T.);
#21618=ORIENTED_EDGE('',*,*,#16051,.F.);
#21619=ORIENTED_EDGE('',*,*,#15876,.F.);
#21620=ORIENTED_EDGE('',*,*,#16052,.F.);
#21621=ORIENTED_EDGE('',*,*,#14971,.T.);
#21622=ORIENTED_EDGE('',*,*,#16053,.F.);
#21623=ORIENTED_EDGE('',*,*,#15879,.F.);
#21624=ORIENTED_EDGE('',*,*,#16054,.F.);
#21625=ORIENTED_EDGE('',*,*,#14975,.T.);
#21626=ORIENTED_EDGE('',*,*,#16055,.F.);
#21627=ORIENTED_EDGE('',*,*,#15882,.F.);
#21628=ORIENTED_EDGE('',*,*,#16056,.F.);
#21629=ORIENTED_EDGE('',*,*,#14979,.T.);
#21630=ORIENTED_EDGE('',*,*,#16057,.F.);
#21631=ORIENTED_EDGE('',*,*,#15885,.F.);
#21632=ORIENTED_EDGE('',*,*,#16058,.F.);
#21633=ORIENTED_EDGE('',*,*,#14983,.T.);
#21634=ORIENTED_EDGE('',*,*,#16059,.F.);
#21635=ORIENTED_EDGE('',*,*,#15039,.T.);
#21636=ORIENTED_EDGE('',*,*,#16060,.F.);
#21637=ORIENTED_EDGE('',*,*,#15887,.F.);
#21638=ORIENTED_EDGE('',*,*,#16061,.F.);
#21639=ORIENTED_EDGE('',*,*,#15036,.T.);
#21640=ORIENTED_EDGE('',*,*,#16062,.F.);
#21641=ORIENTED_EDGE('',*,*,#15890,.F.);
#21642=ORIENTED_EDGE('',*,*,#16063,.F.);
#21643=ORIENTED_EDGE('',*,*,#15033,.T.);
#21644=ORIENTED_EDGE('',*,*,#16064,.F.);
#21645=ORIENTED_EDGE('',*,*,#15893,.F.);
#21646=ORIENTED_EDGE('',*,*,#16065,.F.);
#21647=ORIENTED_EDGE('',*,*,#15030,.T.);
#21648=ORIENTED_EDGE('',*,*,#16066,.F.);
#21649=ORIENTED_EDGE('',*,*,#15896,.F.);
#21650=ORIENTED_EDGE('',*,*,#16067,.F.);
#21651=ORIENTED_EDGE('',*,*,#15027,.T.);
#21652=ORIENTED_EDGE('',*,*,#16068,.F.);
#21653=ORIENTED_EDGE('',*,*,#15899,.F.);
#21654=ORIENTED_EDGE('',*,*,#16069,.F.);
#21655=ORIENTED_EDGE('',*,*,#15024,.T.);
#21656=ORIENTED_EDGE('',*,*,#16070,.F.);
#21657=ORIENTED_EDGE('',*,*,#15902,.F.);
#21658=ORIENTED_EDGE('',*,*,#16071,.F.);
#21659=ORIENTED_EDGE('',*,*,#15021,.T.);
#21660=ORIENTED_EDGE('',*,*,#16072,.F.);
#21661=ORIENTED_EDGE('',*,*,#15905,.F.);
#21662=ORIENTED_EDGE('',*,*,#16073,.F.);
#21663=ORIENTED_EDGE('',*,*,#15018,.T.);
#21664=ORIENTED_EDGE('',*,*,#16074,.F.);
#21665=ORIENTED_EDGE('',*,*,#15908,.F.);
#21666=ORIENTED_EDGE('',*,*,#16075,.F.);
#21667=ORIENTED_EDGE('',*,*,#15015,.T.);
#21668=ORIENTED_EDGE('',*,*,#16076,.F.);
#21669=ORIENTED_EDGE('',*,*,#15911,.F.);
#21670=ORIENTED_EDGE('',*,*,#16077,.F.);
#21671=ORIENTED_EDGE('',*,*,#15011,.T.);
#21672=ORIENTED_EDGE('',*,*,#16078,.F.);
#21673=ORIENTED_EDGE('',*,*,#15914,.F.);
#21674=ORIENTED_EDGE('',*,*,#16079,.F.);
#21675=ORIENTED_EDGE('',*,*,#15007,.T.);
#21676=ORIENTED_EDGE('',*,*,#16080,.F.);
#21677=ORIENTED_EDGE('',*,*,#15917,.F.);
#21678=ORIENTED_EDGE('',*,*,#16081,.F.);
#21679=ORIENTED_EDGE('',*,*,#15003,.T.);
#21680=ORIENTED_EDGE('',*,*,#16082,.F.);
#21681=ORIENTED_EDGE('',*,*,#15920,.F.);
#21682=ORIENTED_EDGE('',*,*,#16083,.F.);
#21683=ORIENTED_EDGE('',*,*,#14999,.T.);
#21684=ORIENTED_EDGE('',*,*,#16084,.F.);
#21685=ORIENTED_EDGE('',*,*,#15923,.F.);
#21686=ORIENTED_EDGE('',*,*,#16085,.F.);
#21687=ORIENTED_EDGE('',*,*,#14995,.T.);
#21688=ORIENTED_EDGE('',*,*,#16086,.F.);
#21689=ORIENTED_EDGE('',*,*,#15926,.F.);
#21690=ORIENTED_EDGE('',*,*,#16087,.F.);
#21691=ORIENTED_EDGE('',*,*,#15930,.F.);
#21692=ORIENTED_EDGE('',*,*,#16088,.F.);
#21693=ORIENTED_EDGE('',*,*,#14987,.T.);
#21694=ORIENTED_EDGE('',*,*,#14665,.T.);
#21695=ORIENTED_EDGE('',*,*,#14755,.T.);
#21696=ORIENTED_EDGE('',*,*,#14662,.T.);
#21697=ORIENTED_EDGE('',*,*,#15453,.T.);
#21698=ORIENTED_EDGE('',*,*,#15456,.F.);
#21699=ORIENTED_EDGE('',*,*,#16089,.F.);
#21700=ORIENTED_EDGE('',*,*,#15142,.F.);
#21701=ORIENTED_EDGE('',*,*,#16090,.F.);
#21702=ORIENTED_EDGE('',*,*,#16091,.T.);
#21703=ORIENTED_EDGE('',*,*,#16092,.F.);
#21704=ORIENTED_EDGE('',*,*,#16091,.F.);
#21705=ORIENTED_EDGE('',*,*,#16093,.F.);
#21706=ORIENTED_EDGE('',*,*,#16094,.T.);
#21707=ORIENTED_EDGE('',*,*,#16095,.F.);
#21708=ORIENTED_EDGE('',*,*,#16094,.F.);
#21709=ORIENTED_EDGE('',*,*,#16096,.F.);
#21710=ORIENTED_EDGE('',*,*,#14991,.T.);
#21711=ORIENTED_EDGE('',*,*,#14832,.F.);
#21712=ORIENTED_EDGE('',*,*,#14829,.F.);
#21713=ORIENTED_EDGE('',*,*,#16097,.T.);
#21714=ORIENTED_EDGE('',*,*,#16098,.T.);
#21715=ORIENTED_EDGE('',*,*,#16099,.T.);
#21716=ORIENTED_EDGE('',*,*,#16100,.T.);
#21717=ORIENTED_EDGE('',*,*,#16101,.T.);
#21718=ORIENTED_EDGE('',*,*,#16102,.T.);
#21719=ORIENTED_EDGE('',*,*,#16103,.T.);
#21720=ORIENTED_EDGE('',*,*,#14824,.T.);
#21721=ORIENTED_EDGE('',*,*,#16104,.F.);
#21722=ORIENTED_EDGE('',*,*,#16098,.F.);
#21723=ORIENTED_EDGE('',*,*,#16104,.T.);
#21724=ORIENTED_EDGE('',*,*,#14823,.T.);
#21725=ORIENTED_EDGE('',*,*,#16105,.F.);
#21726=ORIENTED_EDGE('',*,*,#16099,.F.);
#21727=ORIENTED_EDGE('',*,*,#16105,.T.);
#21728=ORIENTED_EDGE('',*,*,#14822,.T.);
#21729=ORIENTED_EDGE('',*,*,#16106,.F.);
#21730=ORIENTED_EDGE('',*,*,#16100,.F.);
#21731=ORIENTED_EDGE('',*,*,#16106,.T.);
#21732=ORIENTED_EDGE('',*,*,#14821,.T.);
#21733=ORIENTED_EDGE('',*,*,#14827,.T.);
#21734=ORIENTED_EDGE('',*,*,#16107,.F.);
#21735=ORIENTED_EDGE('',*,*,#16101,.F.);
#21736=ORIENTED_EDGE('',*,*,#16107,.T.);
#21737=ORIENTED_EDGE('',*,*,#14826,.T.);
#21738=ORIENTED_EDGE('',*,*,#16108,.F.);
#21739=ORIENTED_EDGE('',*,*,#16102,.F.);
#21740=ORIENTED_EDGE('',*,*,#16108,.T.);
#21741=ORIENTED_EDGE('',*,*,#14825,.T.);
#21742=ORIENTED_EDGE('',*,*,#16103,.F.);
#21743=ORIENTED_EDGE('',*,*,#16097,.F.);
#21744=ORIENTED_EDGE('',*,*,#16109,.F.);
#21745=ORIENTED_EDGE('',*,*,#14753,.F.);
#21746=ORIENTED_EDGE('',*,*,#14752,.F.);
#21747=ORIENTED_EDGE('',*,*,#14749,.F.);
#21748=ORIENTED_EDGE('',*,*,#14746,.F.);
#21749=ORIENTED_EDGE('',*,*,#14743,.F.);
#21750=ORIENTED_EDGE('',*,*,#14740,.F.);
#21751=ORIENTED_EDGE('',*,*,#14737,.F.);
#21752=ORIENTED_EDGE('',*,*,#14734,.F.);
#21753=ORIENTED_EDGE('',*,*,#14731,.F.);
#21754=ORIENTED_EDGE('',*,*,#14728,.F.);
#21755=ORIENTED_EDGE('',*,*,#14725,.F.);
#21756=ORIENTED_EDGE('',*,*,#14722,.F.);
#21757=ORIENTED_EDGE('',*,*,#14719,.F.);
#21758=ORIENTED_EDGE('',*,*,#14716,.F.);
#21759=ORIENTED_EDGE('',*,*,#14713,.F.);
#21760=ORIENTED_EDGE('',*,*,#14710,.F.);
#21761=ORIENTED_EDGE('',*,*,#14707,.F.);
#21762=ORIENTED_EDGE('',*,*,#14704,.F.);
#21763=ORIENTED_EDGE('',*,*,#14701,.F.);
#21764=ORIENTED_EDGE('',*,*,#14698,.F.);
#21765=ORIENTED_EDGE('',*,*,#14695,.F.);
#21766=ORIENTED_EDGE('',*,*,#14692,.F.);
#21767=ORIENTED_EDGE('',*,*,#14689,.F.);
#21768=ORIENTED_EDGE('',*,*,#14686,.F.);
#21769=ORIENTED_EDGE('',*,*,#14683,.F.);
#21770=ORIENTED_EDGE('',*,*,#14680,.F.);
#21771=ORIENTED_EDGE('',*,*,#14677,.F.);
#21772=ORIENTED_EDGE('',*,*,#14674,.F.);
#21773=ORIENTED_EDGE('',*,*,#14671,.F.);
#21774=ORIENTED_EDGE('',*,*,#14668,.F.);
#21775=ORIENTED_EDGE('',*,*,#14661,.F.);
#21776=ORIENTED_EDGE('',*,*,#14758,.F.);
#21777=ORIENTED_EDGE('',*,*,#14759,.T.);
#21778=ORIENTED_EDGE('',*,*,#14659,.T.);
#21779=ORIENTED_EDGE('',*,*,#14656,.T.);
#21780=ORIENTED_EDGE('',*,*,#14653,.T.);
#21781=ORIENTED_EDGE('',*,*,#14650,.T.);
#21782=ORIENTED_EDGE('',*,*,#14647,.T.);
#21783=ORIENTED_EDGE('',*,*,#14644,.T.);
#21784=ORIENTED_EDGE('',*,*,#14641,.T.);
#21785=ORIENTED_EDGE('',*,*,#14638,.T.);
#21786=ORIENTED_EDGE('',*,*,#14635,.T.);
#21787=ORIENTED_EDGE('',*,*,#14632,.T.);
#21788=ORIENTED_EDGE('',*,*,#14629,.T.);
#21789=ORIENTED_EDGE('',*,*,#14626,.T.);
#21790=ORIENTED_EDGE('',*,*,#14623,.T.);
#21791=ORIENTED_EDGE('',*,*,#14620,.T.);
#21792=ORIENTED_EDGE('',*,*,#14617,.T.);
#21793=ORIENTED_EDGE('',*,*,#14614,.T.);
#21794=ORIENTED_EDGE('',*,*,#14611,.T.);
#21795=ORIENTED_EDGE('',*,*,#14608,.T.);
#21796=ORIENTED_EDGE('',*,*,#14605,.T.);
#21797=ORIENTED_EDGE('',*,*,#14602,.T.);
#21798=ORIENTED_EDGE('',*,*,#14599,.T.);
#21799=ORIENTED_EDGE('',*,*,#14596,.T.);
#21800=ORIENTED_EDGE('',*,*,#14593,.T.);
#21801=ORIENTED_EDGE('',*,*,#14590,.T.);
#21802=ORIENTED_EDGE('',*,*,#14587,.T.);
#21803=ORIENTED_EDGE('',*,*,#14584,.T.);
#21804=ORIENTED_EDGE('',*,*,#14581,.T.);
#21805=ORIENTED_EDGE('',*,*,#14578,.T.);
#21806=ORIENTED_EDGE('',*,*,#16110,.F.);
#21807=ORIENTED_EDGE('',*,*,#14574,.T.);
#21808=ORIENTED_EDGE('',*,*,#14580,.T.);
#21809=ORIENTED_EDGE('',*,*,#14583,.T.);
#21810=ORIENTED_EDGE('',*,*,#14586,.T.);
#21811=ORIENTED_EDGE('',*,*,#14589,.T.);
#21812=ORIENTED_EDGE('',*,*,#14592,.T.);
#21813=ORIENTED_EDGE('',*,*,#14595,.T.);
#21814=ORIENTED_EDGE('',*,*,#14598,.T.);
#21815=ORIENTED_EDGE('',*,*,#14601,.T.);
#21816=ORIENTED_EDGE('',*,*,#14604,.T.);
#21817=ORIENTED_EDGE('',*,*,#14607,.T.);
#21818=ORIENTED_EDGE('',*,*,#14610,.T.);
#21819=ORIENTED_EDGE('',*,*,#14613,.T.);
#21820=ORIENTED_EDGE('',*,*,#14616,.T.);
#21821=ORIENTED_EDGE('',*,*,#14619,.T.);
#21822=ORIENTED_EDGE('',*,*,#14622,.T.);
#21823=ORIENTED_EDGE('',*,*,#14625,.T.);
#21824=ORIENTED_EDGE('',*,*,#14628,.T.);
#21825=ORIENTED_EDGE('',*,*,#14631,.T.);
#21826=ORIENTED_EDGE('',*,*,#14634,.T.);
#21827=ORIENTED_EDGE('',*,*,#14637,.T.);
#21828=ORIENTED_EDGE('',*,*,#14640,.T.);
#21829=ORIENTED_EDGE('',*,*,#14643,.T.);
#21830=ORIENTED_EDGE('',*,*,#14646,.T.);
#21831=ORIENTED_EDGE('',*,*,#14649,.T.);
#21832=ORIENTED_EDGE('',*,*,#14652,.T.);
#21833=ORIENTED_EDGE('',*,*,#14655,.T.);
#21834=ORIENTED_EDGE('',*,*,#14658,.T.);
#21835=ORIENTED_EDGE('',*,*,#14760,.T.);
#21836=ORIENTED_EDGE('',*,*,#14756,.F.);
#21837=ORIENTED_EDGE('',*,*,#14664,.T.);
#21838=ORIENTED_EDGE('',*,*,#14667,.T.);
#21839=ORIENTED_EDGE('',*,*,#14670,.T.);
#21840=ORIENTED_EDGE('',*,*,#14673,.T.);
#21841=ORIENTED_EDGE('',*,*,#14676,.T.);
#21842=ORIENTED_EDGE('',*,*,#14679,.T.);
#21843=ORIENTED_EDGE('',*,*,#14682,.T.);
#21844=ORIENTED_EDGE('',*,*,#14685,.T.);
#21845=ORIENTED_EDGE('',*,*,#14688,.T.);
#21846=ORIENTED_EDGE('',*,*,#14691,.T.);
#21847=ORIENTED_EDGE('',*,*,#14694,.T.);
#21848=ORIENTED_EDGE('',*,*,#14697,.T.);
#21849=ORIENTED_EDGE('',*,*,#14700,.T.);
#21850=ORIENTED_EDGE('',*,*,#14703,.T.);
#21851=ORIENTED_EDGE('',*,*,#14706,.T.);
#21852=ORIENTED_EDGE('',*,*,#14709,.T.);
#21853=ORIENTED_EDGE('',*,*,#14712,.T.);
#21854=ORIENTED_EDGE('',*,*,#14715,.T.);
#21855=ORIENTED_EDGE('',*,*,#14718,.T.);
#21856=ORIENTED_EDGE('',*,*,#14721,.T.);
#21857=ORIENTED_EDGE('',*,*,#14724,.T.);
#21858=ORIENTED_EDGE('',*,*,#14727,.T.);
#21859=ORIENTED_EDGE('',*,*,#14730,.T.);
#21860=ORIENTED_EDGE('',*,*,#14733,.T.);
#21861=ORIENTED_EDGE('',*,*,#14736,.T.);
#21862=ORIENTED_EDGE('',*,*,#14739,.T.);
#21863=ORIENTED_EDGE('',*,*,#14742,.T.);
#21864=ORIENTED_EDGE('',*,*,#14745,.T.);
#21865=ORIENTED_EDGE('',*,*,#14748,.T.);
#21866=ORIENTED_EDGE('',*,*,#14751,.T.);
#21867=ORIENTED_EDGE('',*,*,#14754,.T.);
#21868=ORIENTED_EDGE('',*,*,#16109,.T.);
#21869=ORIENTED_EDGE('',*,*,#14577,.T.);
#21870=ORIENTED_EDGE('',*,*,#16110,.T.);
#21871=ORIENTED_EDGE('',*,*,#15141,.T.);
#21872=ORIENTED_EDGE('',*,*,#16111,.T.);
#21873=ORIENTED_EDGE('',*,*,#14992,.T.);
#21874=ORIENTED_EDGE('',*,*,#16096,.T.);
#21875=ORIENTED_EDGE('',*,*,#16093,.T.);
#21876=ORIENTED_EDGE('',*,*,#16090,.T.);
#21877=ORIENTED_EDGE('',*,*,#15140,.T.);
#21878=ORIENTED_EDGE('',*,*,#15445,.T.);
#21879=ORIENTED_EDGE('',*,*,#16112,.T.);
#21880=ORIENTED_EDGE('',*,*,#14993,.T.);
#21881=ORIENTED_EDGE('',*,*,#16111,.F.);
#21882=ORIENTED_EDGE('',*,*,#15444,.T.);
#21883=ORIENTED_EDGE('',*,*,#15690,.T.);
#21884=ORIENTED_EDGE('',*,*,#15927,.T.);
#21885=ORIENTED_EDGE('',*,*,#16086,.T.);
#21886=ORIENTED_EDGE('',*,*,#14994,.T.);
#21887=ORIENTED_EDGE('',*,*,#16112,.F.);
#21888=ORIENTED_EDGE('',*,*,#15145,.T.);
#21889=ORIENTED_EDGE('',*,*,#16113,.T.);
#21890=ORIENTED_EDGE('',*,*,#14988,.T.);
#21891=ORIENTED_EDGE('',*,*,#16088,.T.);
#21892=ORIENTED_EDGE('',*,*,#15929,.T.);
#21893=ORIENTED_EDGE('',*,*,#15692,.T.);
#21894=ORIENTED_EDGE('',*,*,#15144,.T.);
#21895=ORIENTED_EDGE('',*,*,#16114,.T.);
#21896=ORIENTED_EDGE('',*,*,#14989,.T.);
#21897=ORIENTED_EDGE('',*,*,#16113,.F.);
#21898=ORIENTED_EDGE('',*,*,#15143,.T.);
#21899=ORIENTED_EDGE('',*,*,#16089,.T.);
#21900=ORIENTED_EDGE('',*,*,#16092,.T.);
#21901=ORIENTED_EDGE('',*,*,#16095,.T.);
#21902=ORIENTED_EDGE('',*,*,#14990,.T.);
#21903=ORIENTED_EDGE('',*,*,#16114,.F.);
#21904=ORIENTED_EDGE('',*,*,#15442,.T.);
#21905=ORIENTED_EDGE('',*,*,#16115,.T.);
#21906=ORIENTED_EDGE('',*,*,#14996,.T.);
#21907=ORIENTED_EDGE('',*,*,#16085,.T.);
#21908=ORIENTED_EDGE('',*,*,#15925,.T.);
#21909=ORIENTED_EDGE('',*,*,#15688,.T.);
#21910=ORIENTED_EDGE('',*,*,#15441,.T.);
#21911=ORIENTED_EDGE('',*,*,#16116,.T.);
#21912=ORIENTED_EDGE('',*,*,#14997,.T.);
#21913=ORIENTED_EDGE('',*,*,#16115,.F.);
#21914=ORIENTED_EDGE('',*,*,#15440,.T.);
#21915=ORIENTED_EDGE('',*,*,#15687,.T.);
#21916=ORIENTED_EDGE('',*,*,#15924,.T.);
#21917=ORIENTED_EDGE('',*,*,#16084,.T.);
#21918=ORIENTED_EDGE('',*,*,#14998,.T.);
#21919=ORIENTED_EDGE('',*,*,#16116,.F.);
#21920=ORIENTED_EDGE('',*,*,#15438,.T.);
#21921=ORIENTED_EDGE('',*,*,#16117,.T.);
#21922=ORIENTED_EDGE('',*,*,#15000,.T.);
#21923=ORIENTED_EDGE('',*,*,#16083,.T.);
#21924=ORIENTED_EDGE('',*,*,#15922,.T.);
#21925=ORIENTED_EDGE('',*,*,#15685,.T.);
#21926=ORIENTED_EDGE('',*,*,#15437,.T.);
#21927=ORIENTED_EDGE('',*,*,#16118,.T.);
#21928=ORIENTED_EDGE('',*,*,#15001,.T.);
#21929=ORIENTED_EDGE('',*,*,#16117,.F.);
#21930=ORIENTED_EDGE('',*,*,#15436,.T.);
#21931=ORIENTED_EDGE('',*,*,#15684,.T.);
#21932=ORIENTED_EDGE('',*,*,#15921,.T.);
#21933=ORIENTED_EDGE('',*,*,#16082,.T.);
#21934=ORIENTED_EDGE('',*,*,#15002,.T.);
#21935=ORIENTED_EDGE('',*,*,#16118,.F.);
#21936=ORIENTED_EDGE('',*,*,#15434,.T.);
#21937=ORIENTED_EDGE('',*,*,#16119,.T.);
#21938=ORIENTED_EDGE('',*,*,#15004,.T.);
#21939=ORIENTED_EDGE('',*,*,#16081,.T.);
#21940=ORIENTED_EDGE('',*,*,#15919,.T.);
#21941=ORIENTED_EDGE('',*,*,#15682,.T.);
#21942=ORIENTED_EDGE('',*,*,#15433,.T.);
#21943=ORIENTED_EDGE('',*,*,#16120,.T.);
#21944=ORIENTED_EDGE('',*,*,#15005,.T.);
#21945=ORIENTED_EDGE('',*,*,#16119,.F.);
#21946=ORIENTED_EDGE('',*,*,#15432,.T.);
#21947=ORIENTED_EDGE('',*,*,#15681,.T.);
#21948=ORIENTED_EDGE('',*,*,#15918,.T.);
#21949=ORIENTED_EDGE('',*,*,#16080,.T.);
#21950=ORIENTED_EDGE('',*,*,#15006,.T.);
#21951=ORIENTED_EDGE('',*,*,#16120,.F.);
#21952=ORIENTED_EDGE('',*,*,#15430,.T.);
#21953=ORIENTED_EDGE('',*,*,#16121,.T.);
#21954=ORIENTED_EDGE('',*,*,#15008,.T.);
#21955=ORIENTED_EDGE('',*,*,#16079,.T.);
#21956=ORIENTED_EDGE('',*,*,#15916,.T.);
#21957=ORIENTED_EDGE('',*,*,#15679,.T.);
#21958=ORIENTED_EDGE('',*,*,#15429,.T.);
#21959=ORIENTED_EDGE('',*,*,#16122,.T.);
#21960=ORIENTED_EDGE('',*,*,#15009,.T.);
#21961=ORIENTED_EDGE('',*,*,#16121,.F.);
#21962=ORIENTED_EDGE('',*,*,#15428,.T.);
#21963=ORIENTED_EDGE('',*,*,#15678,.T.);
#21964=ORIENTED_EDGE('',*,*,#15915,.T.);
#21965=ORIENTED_EDGE('',*,*,#16078,.T.);
#21966=ORIENTED_EDGE('',*,*,#15010,.T.);
#21967=ORIENTED_EDGE('',*,*,#16122,.F.);
#21968=ORIENTED_EDGE('',*,*,#15426,.T.);
#21969=ORIENTED_EDGE('',*,*,#16123,.T.);
#21970=ORIENTED_EDGE('',*,*,#15012,.T.);
#21971=ORIENTED_EDGE('',*,*,#16077,.T.);
#21972=ORIENTED_EDGE('',*,*,#15913,.T.);
#21973=ORIENTED_EDGE('',*,*,#15676,.T.);
#21974=ORIENTED_EDGE('',*,*,#15425,.T.);
#21975=ORIENTED_EDGE('',*,*,#16124,.T.);
#21976=ORIENTED_EDGE('',*,*,#15013,.T.);
#21977=ORIENTED_EDGE('',*,*,#16123,.F.);
#21978=ORIENTED_EDGE('',*,*,#15424,.T.);
#21979=ORIENTED_EDGE('',*,*,#15675,.T.);
#21980=ORIENTED_EDGE('',*,*,#15912,.T.);
#21981=ORIENTED_EDGE('',*,*,#16076,.T.);
#21982=ORIENTED_EDGE('',*,*,#15014,.T.);
#21983=ORIENTED_EDGE('',*,*,#16124,.F.);
#21984=ORIENTED_EDGE('',*,*,#15422,.T.);
#21985=ORIENTED_EDGE('',*,*,#14820,.T.);
#21986=ORIENTED_EDGE('',*,*,#15016,.T.);
#21987=ORIENTED_EDGE('',*,*,#16075,.T.);
#21988=ORIENTED_EDGE('',*,*,#15910,.T.);
#21989=ORIENTED_EDGE('',*,*,#15673,.T.);
#21990=ORIENTED_EDGE('',*,*,#15421,.T.);
#21991=ORIENTED_EDGE('',*,*,#15672,.T.);
#21992=ORIENTED_EDGE('',*,*,#15909,.T.);
#21993=ORIENTED_EDGE('',*,*,#16074,.T.);
#21994=ORIENTED_EDGE('',*,*,#15017,.T.);
#21995=ORIENTED_EDGE('',*,*,#14818,.F.);
#21996=ORIENTED_EDGE('',*,*,#15419,.T.);
#21997=ORIENTED_EDGE('',*,*,#14816,.T.);
#21998=ORIENTED_EDGE('',*,*,#15019,.T.);
#21999=ORIENTED_EDGE('',*,*,#16073,.T.);
#22000=ORIENTED_EDGE('',*,*,#15907,.T.);
#22001=ORIENTED_EDGE('',*,*,#15670,.T.);
#22002=ORIENTED_EDGE('',*,*,#15418,.T.);
#22003=ORIENTED_EDGE('',*,*,#15669,.T.);
#22004=ORIENTED_EDGE('',*,*,#15906,.T.);
#22005=ORIENTED_EDGE('',*,*,#16072,.T.);
#22006=ORIENTED_EDGE('',*,*,#15020,.T.);
#22007=ORIENTED_EDGE('',*,*,#14814,.F.);
#22008=ORIENTED_EDGE('',*,*,#15416,.T.);
#22009=ORIENTED_EDGE('',*,*,#14812,.T.);
#22010=ORIENTED_EDGE('',*,*,#15022,.T.);
#22011=ORIENTED_EDGE('',*,*,#16071,.T.);
#22012=ORIENTED_EDGE('',*,*,#15904,.T.);
#22013=ORIENTED_EDGE('',*,*,#15667,.T.);
#22014=ORIENTED_EDGE('',*,*,#15415,.T.);
#22015=ORIENTED_EDGE('',*,*,#15666,.T.);
#22016=ORIENTED_EDGE('',*,*,#15903,.T.);
#22017=ORIENTED_EDGE('',*,*,#16070,.T.);
#22018=ORIENTED_EDGE('',*,*,#15023,.T.);
#22019=ORIENTED_EDGE('',*,*,#14810,.F.);
#22020=ORIENTED_EDGE('',*,*,#15413,.T.);
#22021=ORIENTED_EDGE('',*,*,#14808,.T.);
#22022=ORIENTED_EDGE('',*,*,#15025,.T.);
#22023=ORIENTED_EDGE('',*,*,#16069,.T.);
#22024=ORIENTED_EDGE('',*,*,#15901,.T.);
#22025=ORIENTED_EDGE('',*,*,#15664,.T.);
#22026=ORIENTED_EDGE('',*,*,#15412,.T.);
#22027=ORIENTED_EDGE('',*,*,#15663,.T.);
#22028=ORIENTED_EDGE('',*,*,#15900,.T.);
#22029=ORIENTED_EDGE('',*,*,#16068,.T.);
#22030=ORIENTED_EDGE('',*,*,#15026,.T.);
#22031=ORIENTED_EDGE('',*,*,#14806,.F.);
#22032=ORIENTED_EDGE('',*,*,#15410,.T.);
#22033=ORIENTED_EDGE('',*,*,#14804,.T.);
#22034=ORIENTED_EDGE('',*,*,#15028,.T.);
#22035=ORIENTED_EDGE('',*,*,#16067,.T.);
#22036=ORIENTED_EDGE('',*,*,#15898,.T.);
#22037=ORIENTED_EDGE('',*,*,#15661,.T.);
#22038=ORIENTED_EDGE('',*,*,#15409,.T.);
#22039=ORIENTED_EDGE('',*,*,#15660,.T.);
#22040=ORIENTED_EDGE('',*,*,#15897,.T.);
#22041=ORIENTED_EDGE('',*,*,#16066,.T.);
#22042=ORIENTED_EDGE('',*,*,#15029,.T.);
#22043=ORIENTED_EDGE('',*,*,#14802,.F.);
#22044=ORIENTED_EDGE('',*,*,#15407,.T.);
#22045=ORIENTED_EDGE('',*,*,#14800,.T.);
#22046=ORIENTED_EDGE('',*,*,#15031,.T.);
#22047=ORIENTED_EDGE('',*,*,#16065,.T.);
#22048=ORIENTED_EDGE('',*,*,#15895,.T.);
#22049=ORIENTED_EDGE('',*,*,#15658,.T.);
#22050=ORIENTED_EDGE('',*,*,#15406,.T.);
#22051=ORIENTED_EDGE('',*,*,#15657,.T.);
#22052=ORIENTED_EDGE('',*,*,#15894,.T.);
#22053=ORIENTED_EDGE('',*,*,#16064,.T.);
#22054=ORIENTED_EDGE('',*,*,#15032,.T.);
#22055=ORIENTED_EDGE('',*,*,#14798,.F.);
#22056=ORIENTED_EDGE('',*,*,#15404,.T.);
#22057=ORIENTED_EDGE('',*,*,#14796,.T.);
#22058=ORIENTED_EDGE('',*,*,#15034,.T.);
#22059=ORIENTED_EDGE('',*,*,#16063,.T.);
#22060=ORIENTED_EDGE('',*,*,#15892,.T.);
#22061=ORIENTED_EDGE('',*,*,#15655,.T.);
#22062=ORIENTED_EDGE('',*,*,#15403,.T.);
#22063=ORIENTED_EDGE('',*,*,#15654,.T.);
#22064=ORIENTED_EDGE('',*,*,#15891,.T.);
#22065=ORIENTED_EDGE('',*,*,#16062,.T.);
#22066=ORIENTED_EDGE('',*,*,#15035,.T.);
#22067=ORIENTED_EDGE('',*,*,#14794,.F.);
#22068=ORIENTED_EDGE('',*,*,#15401,.T.);
#22069=ORIENTED_EDGE('',*,*,#14792,.T.);
#22070=ORIENTED_EDGE('',*,*,#15037,.T.);
#22071=ORIENTED_EDGE('',*,*,#16061,.T.);
#22072=ORIENTED_EDGE('',*,*,#15889,.T.);
#22073=ORIENTED_EDGE('',*,*,#15652,.T.);
#22074=ORIENTED_EDGE('',*,*,#15400,.T.);
#22075=ORIENTED_EDGE('',*,*,#15651,.T.);
#22076=ORIENTED_EDGE('',*,*,#15888,.T.);
#22077=ORIENTED_EDGE('',*,*,#16060,.T.);
#22078=ORIENTED_EDGE('',*,*,#15038,.T.);
#22079=ORIENTED_EDGE('',*,*,#14790,.F.);
#22080=ORIENTED_EDGE('',*,*,#15398,.T.);
#22081=ORIENTED_EDGE('',*,*,#14788,.T.);
#22082=ORIENTED_EDGE('',*,*,#15040,.T.);
#22083=ORIENTED_EDGE('',*,*,#16059,.T.);
#22084=ORIENTED_EDGE('',*,*,#15886,.T.);
#22085=ORIENTED_EDGE('',*,*,#15649,.T.);
#22086=ORIENTED_EDGE('',*,*,#15397,.T.);
#22087=ORIENTED_EDGE('',*,*,#15459,.T.);
#22088=ORIENTED_EDGE('',*,*,#15696,.T.);
#22089=ORIENTED_EDGE('',*,*,#15932,.T.);
#22090=ORIENTED_EDGE('',*,*,#15041,.T.);
#22091=ORIENTED_EDGE('',*,*,#14786,.F.);
#22092=ORIENTED_EDGE('',*,*,#15149,.T.);
#22093=ORIENTED_EDGE('',*,*,#16125,.T.);
#22094=ORIENTED_EDGE('',*,*,#14984,.T.);
#22095=ORIENTED_EDGE('',*,*,#16058,.T.);
#22096=ORIENTED_EDGE('',*,*,#15884,.T.);
#22097=ORIENTED_EDGE('',*,*,#15647,.T.);
#22098=ORIENTED_EDGE('',*,*,#15148,.T.);
#22099=ORIENTED_EDGE('',*,*,#16126,.T.);
#22100=ORIENTED_EDGE('',*,*,#14985,.T.);
#22101=ORIENTED_EDGE('',*,*,#16125,.F.);
#22102=ORIENTED_EDGE('',*,*,#15147,.T.);
#22103=ORIENTED_EDGE('',*,*,#15691,.T.);
#22104=ORIENTED_EDGE('',*,*,#15928,.T.);
#22105=ORIENTED_EDGE('',*,*,#16087,.T.);
#22106=ORIENTED_EDGE('',*,*,#14986,.T.);
#22107=ORIENTED_EDGE('',*,*,#16126,.F.);
#22108=ORIENTED_EDGE('',*,*,#15153,.T.);
#22109=ORIENTED_EDGE('',*,*,#16127,.T.);
#22110=ORIENTED_EDGE('',*,*,#14980,.T.);
#22111=ORIENTED_EDGE('',*,*,#16056,.T.);
#22112=ORIENTED_EDGE('',*,*,#15881,.T.);
#22113=ORIENTED_EDGE('',*,*,#15644,.T.);
#22114=ORIENTED_EDGE('',*,*,#15152,.T.);
#22115=ORIENTED_EDGE('',*,*,#16128,.T.);
#22116=ORIENTED_EDGE('',*,*,#14981,.T.);
#22117=ORIENTED_EDGE('',*,*,#16127,.F.);
#22118=ORIENTED_EDGE('',*,*,#15151,.T.);
#22119=ORIENTED_EDGE('',*,*,#15646,.T.);
#22120=ORIENTED_EDGE('',*,*,#15883,.T.);
#22121=ORIENTED_EDGE('',*,*,#16057,.T.);
#22122=ORIENTED_EDGE('',*,*,#14982,.T.);
#22123=ORIENTED_EDGE('',*,*,#16128,.F.);
#22124=ORIENTED_EDGE('',*,*,#15157,.T.);
#22125=ORIENTED_EDGE('',*,*,#16129,.T.);
#22126=ORIENTED_EDGE('',*,*,#14976,.T.);
#22127=ORIENTED_EDGE('',*,*,#16054,.T.);
#22128=ORIENTED_EDGE('',*,*,#15878,.T.);
#22129=ORIENTED_EDGE('',*,*,#15641,.T.);
#22130=ORIENTED_EDGE('',*,*,#15156,.T.);
#22131=ORIENTED_EDGE('',*,*,#16130,.T.);
#22132=ORIENTED_EDGE('',*,*,#14977,.T.);
#22133=ORIENTED_EDGE('',*,*,#16129,.F.);
#22134=ORIENTED_EDGE('',*,*,#15155,.T.);
#22135=ORIENTED_EDGE('',*,*,#15643,.T.);
#22136=ORIENTED_EDGE('',*,*,#15880,.T.);
#22137=ORIENTED_EDGE('',*,*,#16055,.T.);
#22138=ORIENTED_EDGE('',*,*,#14978,.T.);
#22139=ORIENTED_EDGE('',*,*,#16130,.F.);
#22140=ORIENTED_EDGE('',*,*,#15161,.T.);
#22141=ORIENTED_EDGE('',*,*,#16131,.T.);
#22142=ORIENTED_EDGE('',*,*,#14972,.T.);
#22143=ORIENTED_EDGE('',*,*,#16052,.T.);
#22144=ORIENTED_EDGE('',*,*,#15875,.T.);
#22145=ORIENTED_EDGE('',*,*,#15638,.T.);
#22146=ORIENTED_EDGE('',*,*,#15160,.T.);
#22147=ORIENTED_EDGE('',*,*,#16132,.T.);
#22148=ORIENTED_EDGE('',*,*,#14973,.T.);
#22149=ORIENTED_EDGE('',*,*,#16131,.F.);
#22150=ORIENTED_EDGE('',*,*,#15159,.T.);
#22151=ORIENTED_EDGE('',*,*,#15640,.T.);
#22152=ORIENTED_EDGE('',*,*,#15877,.T.);
#22153=ORIENTED_EDGE('',*,*,#16053,.T.);
#22154=ORIENTED_EDGE('',*,*,#14974,.T.);
#22155=ORIENTED_EDGE('',*,*,#16132,.F.);
#22156=ORIENTED_EDGE('',*,*,#15165,.T.);
#22157=ORIENTED_EDGE('',*,*,#16133,.T.);
#22158=ORIENTED_EDGE('',*,*,#14968,.T.);
#22159=ORIENTED_EDGE('',*,*,#16050,.T.);
#22160=ORIENTED_EDGE('',*,*,#15872,.T.);
#22161=ORIENTED_EDGE('',*,*,#15635,.T.);
#22162=ORIENTED_EDGE('',*,*,#15164,.T.);
#22163=ORIENTED_EDGE('',*,*,#16134,.T.);
#22164=ORIENTED_EDGE('',*,*,#14969,.T.);
#22165=ORIENTED_EDGE('',*,*,#16133,.F.);
#22166=ORIENTED_EDGE('',*,*,#15163,.T.);
#22167=ORIENTED_EDGE('',*,*,#15637,.T.);
#22168=ORIENTED_EDGE('',*,*,#15874,.T.);
#22169=ORIENTED_EDGE('',*,*,#16051,.T.);
#22170=ORIENTED_EDGE('',*,*,#14970,.T.);
#22171=ORIENTED_EDGE('',*,*,#16134,.F.);
#22172=ORIENTED_EDGE('',*,*,#15169,.T.);
#22173=ORIENTED_EDGE('',*,*,#16135,.T.);
#22174=ORIENTED_EDGE('',*,*,#14964,.T.);
#22175=ORIENTED_EDGE('',*,*,#16048,.T.);
#22176=ORIENTED_EDGE('',*,*,#15869,.T.);
#22177=ORIENTED_EDGE('',*,*,#15632,.T.);
#22178=ORIENTED_EDGE('',*,*,#15168,.T.);
#22179=ORIENTED_EDGE('',*,*,#16136,.T.);
#22180=ORIENTED_EDGE('',*,*,#14965,.T.);
#22181=ORIENTED_EDGE('',*,*,#16135,.F.);
#22182=ORIENTED_EDGE('',*,*,#15167,.T.);
#22183=ORIENTED_EDGE('',*,*,#15634,.T.);
#22184=ORIENTED_EDGE('',*,*,#15871,.T.);
#22185=ORIENTED_EDGE('',*,*,#16049,.T.);
#22186=ORIENTED_EDGE('',*,*,#14966,.T.);
#22187=ORIENTED_EDGE('',*,*,#16136,.F.);
#22188=ORIENTED_EDGE('',*,*,#15173,.T.);
#22189=ORIENTED_EDGE('',*,*,#16137,.T.);
#22190=ORIENTED_EDGE('',*,*,#14960,.T.);
#22191=ORIENTED_EDGE('',*,*,#16046,.T.);
#22192=ORIENTED_EDGE('',*,*,#15866,.T.);
#22193=ORIENTED_EDGE('',*,*,#15629,.T.);
#22194=ORIENTED_EDGE('',*,*,#15172,.T.);
#22195=ORIENTED_EDGE('',*,*,#16138,.T.);
#22196=ORIENTED_EDGE('',*,*,#14961,.T.);
#22197=ORIENTED_EDGE('',*,*,#16137,.F.);
#22198=ORIENTED_EDGE('',*,*,#15171,.T.);
#22199=ORIENTED_EDGE('',*,*,#15631,.T.);
#22200=ORIENTED_EDGE('',*,*,#15868,.T.);
#22201=ORIENTED_EDGE('',*,*,#16047,.T.);
#22202=ORIENTED_EDGE('',*,*,#14962,.T.);
#22203=ORIENTED_EDGE('',*,*,#16138,.F.);
#22204=ORIENTED_EDGE('',*,*,#15177,.T.);
#22205=ORIENTED_EDGE('',*,*,#16139,.T.);
#22206=ORIENTED_EDGE('',*,*,#14956,.T.);
#22207=ORIENTED_EDGE('',*,*,#16044,.T.);
#22208=ORIENTED_EDGE('',*,*,#15863,.T.);
#22209=ORIENTED_EDGE('',*,*,#15626,.T.);
#22210=ORIENTED_EDGE('',*,*,#15176,.T.);
#22211=ORIENTED_EDGE('',*,*,#16140,.T.);
#22212=ORIENTED_EDGE('',*,*,#14957,.T.);
#22213=ORIENTED_EDGE('',*,*,#16139,.F.);
#22214=ORIENTED_EDGE('',*,*,#15175,.T.);
#22215=ORIENTED_EDGE('',*,*,#15628,.T.);
#22216=ORIENTED_EDGE('',*,*,#15865,.T.);
#22217=ORIENTED_EDGE('',*,*,#16045,.T.);
#22218=ORIENTED_EDGE('',*,*,#14958,.T.);
#22219=ORIENTED_EDGE('',*,*,#16140,.F.);
#22220=ORIENTED_EDGE('',*,*,#15181,.T.);
#22221=ORIENTED_EDGE('',*,*,#16141,.T.);
#22222=ORIENTED_EDGE('',*,*,#14952,.T.);
#22223=ORIENTED_EDGE('',*,*,#16042,.T.);
#22224=ORIENTED_EDGE('',*,*,#15860,.T.);
#22225=ORIENTED_EDGE('',*,*,#15623,.T.);
#22226=ORIENTED_EDGE('',*,*,#15180,.T.);
#22227=ORIENTED_EDGE('',*,*,#16142,.T.);
#22228=ORIENTED_EDGE('',*,*,#14953,.T.);
#22229=ORIENTED_EDGE('',*,*,#16141,.F.);
#22230=ORIENTED_EDGE('',*,*,#15179,.T.);
#22231=ORIENTED_EDGE('',*,*,#15625,.T.);
#22232=ORIENTED_EDGE('',*,*,#15862,.T.);
#22233=ORIENTED_EDGE('',*,*,#16043,.T.);
#22234=ORIENTED_EDGE('',*,*,#14954,.T.);
#22235=ORIENTED_EDGE('',*,*,#16142,.F.);
#22236=ORIENTED_EDGE('',*,*,#15185,.T.);
#22237=ORIENTED_EDGE('',*,*,#16143,.T.);
#22238=ORIENTED_EDGE('',*,*,#14948,.T.);
#22239=ORIENTED_EDGE('',*,*,#16040,.T.);
#22240=ORIENTED_EDGE('',*,*,#15857,.T.);
#22241=ORIENTED_EDGE('',*,*,#15620,.T.);
#22242=ORIENTED_EDGE('',*,*,#15184,.T.);
#22243=ORIENTED_EDGE('',*,*,#16144,.T.);
#22244=ORIENTED_EDGE('',*,*,#14949,.T.);
#22245=ORIENTED_EDGE('',*,*,#16143,.F.);
#22246=ORIENTED_EDGE('',*,*,#15183,.T.);
#22247=ORIENTED_EDGE('',*,*,#15622,.T.);
#22248=ORIENTED_EDGE('',*,*,#15859,.T.);
#22249=ORIENTED_EDGE('',*,*,#16041,.T.);
#22250=ORIENTED_EDGE('',*,*,#14950,.T.);
#22251=ORIENTED_EDGE('',*,*,#16144,.F.);
#22252=ORIENTED_EDGE('',*,*,#15189,.T.);
#22253=ORIENTED_EDGE('',*,*,#16145,.T.);
#22254=ORIENTED_EDGE('',*,*,#14944,.T.);
#22255=ORIENTED_EDGE('',*,*,#16038,.T.);
#22256=ORIENTED_EDGE('',*,*,#15854,.T.);
#22257=ORIENTED_EDGE('',*,*,#15617,.T.);
#22258=ORIENTED_EDGE('',*,*,#15188,.T.);
#22259=ORIENTED_EDGE('',*,*,#16146,.T.);
#22260=ORIENTED_EDGE('',*,*,#14945,.T.);
#22261=ORIENTED_EDGE('',*,*,#16145,.F.);
#22262=ORIENTED_EDGE('',*,*,#15187,.T.);
#22263=ORIENTED_EDGE('',*,*,#15619,.T.);
#22264=ORIENTED_EDGE('',*,*,#15856,.T.);
#22265=ORIENTED_EDGE('',*,*,#16039,.T.);
#22266=ORIENTED_EDGE('',*,*,#14946,.T.);
#22267=ORIENTED_EDGE('',*,*,#16146,.F.);
#22268=ORIENTED_EDGE('',*,*,#15193,.T.);
#22269=ORIENTED_EDGE('',*,*,#16147,.T.);
#22270=ORIENTED_EDGE('',*,*,#14940,.T.);
#22271=ORIENTED_EDGE('',*,*,#16036,.T.);
#22272=ORIENTED_EDGE('',*,*,#15851,.T.);
#22273=ORIENTED_EDGE('',*,*,#15614,.T.);
#22274=ORIENTED_EDGE('',*,*,#15192,.T.);
#22275=ORIENTED_EDGE('',*,*,#16148,.T.);
#22276=ORIENTED_EDGE('',*,*,#14941,.T.);
#22277=ORIENTED_EDGE('',*,*,#16147,.F.);
#22278=ORIENTED_EDGE('',*,*,#15191,.T.);
#22279=ORIENTED_EDGE('',*,*,#15616,.T.);
#22280=ORIENTED_EDGE('',*,*,#15853,.T.);
#22281=ORIENTED_EDGE('',*,*,#16037,.T.);
#22282=ORIENTED_EDGE('',*,*,#14942,.T.);
#22283=ORIENTED_EDGE('',*,*,#16148,.F.);
#22284=ORIENTED_EDGE('',*,*,#15197,.T.);
#22285=ORIENTED_EDGE('',*,*,#16149,.T.);
#22286=ORIENTED_EDGE('',*,*,#14936,.T.);
#22287=ORIENTED_EDGE('',*,*,#16034,.T.);
#22288=ORIENTED_EDGE('',*,*,#15848,.T.);
#22289=ORIENTED_EDGE('',*,*,#15611,.T.);
#22290=ORIENTED_EDGE('',*,*,#15196,.T.);
#22291=ORIENTED_EDGE('',*,*,#16150,.T.);
#22292=ORIENTED_EDGE('',*,*,#14937,.T.);
#22293=ORIENTED_EDGE('',*,*,#16149,.F.);
#22294=ORIENTED_EDGE('',*,*,#15195,.T.);
#22295=ORIENTED_EDGE('',*,*,#15613,.T.);
#22296=ORIENTED_EDGE('',*,*,#15850,.T.);
#22297=ORIENTED_EDGE('',*,*,#16035,.T.);
#22298=ORIENTED_EDGE('',*,*,#14938,.T.);
#22299=ORIENTED_EDGE('',*,*,#16150,.F.);
#22300=ORIENTED_EDGE('',*,*,#15201,.T.);
#22301=ORIENTED_EDGE('',*,*,#16151,.T.);
#22302=ORIENTED_EDGE('',*,*,#14932,.T.);
#22303=ORIENTED_EDGE('',*,*,#16032,.T.);
#22304=ORIENTED_EDGE('',*,*,#15845,.T.);
#22305=ORIENTED_EDGE('',*,*,#15608,.T.);
#22306=ORIENTED_EDGE('',*,*,#15200,.T.);
#22307=ORIENTED_EDGE('',*,*,#16152,.T.);
#22308=ORIENTED_EDGE('',*,*,#14933,.T.);
#22309=ORIENTED_EDGE('',*,*,#16151,.F.);
#22310=ORIENTED_EDGE('',*,*,#15199,.T.);
#22311=ORIENTED_EDGE('',*,*,#15610,.T.);
#22312=ORIENTED_EDGE('',*,*,#15847,.T.);
#22313=ORIENTED_EDGE('',*,*,#16033,.T.);
#22314=ORIENTED_EDGE('',*,*,#14934,.T.);
#22315=ORIENTED_EDGE('',*,*,#16152,.F.);
#22316=ORIENTED_EDGE('',*,*,#15205,.T.);
#22317=ORIENTED_EDGE('',*,*,#16153,.T.);
#22318=ORIENTED_EDGE('',*,*,#14928,.T.);
#22319=ORIENTED_EDGE('',*,*,#16030,.T.);
#22320=ORIENTED_EDGE('',*,*,#15842,.T.);
#22321=ORIENTED_EDGE('',*,*,#15605,.T.);
#22322=ORIENTED_EDGE('',*,*,#15204,.T.);
#22323=ORIENTED_EDGE('',*,*,#16154,.T.);
#22324=ORIENTED_EDGE('',*,*,#14929,.T.);
#22325=ORIENTED_EDGE('',*,*,#16153,.F.);
#22326=ORIENTED_EDGE('',*,*,#15203,.T.);
#22327=ORIENTED_EDGE('',*,*,#15607,.T.);
#22328=ORIENTED_EDGE('',*,*,#15844,.T.);
#22329=ORIENTED_EDGE('',*,*,#16031,.T.);
#22330=ORIENTED_EDGE('',*,*,#14930,.T.);
#22331=ORIENTED_EDGE('',*,*,#16154,.F.);
#22332=ORIENTED_EDGE('',*,*,#15209,.T.);
#22333=ORIENTED_EDGE('',*,*,#16155,.T.);
#22334=ORIENTED_EDGE('',*,*,#14924,.T.);
#22335=ORIENTED_EDGE('',*,*,#16028,.T.);
#22336=ORIENTED_EDGE('',*,*,#15839,.T.);
#22337=ORIENTED_EDGE('',*,*,#15602,.T.);
#22338=ORIENTED_EDGE('',*,*,#15208,.T.);
#22339=ORIENTED_EDGE('',*,*,#16156,.T.);
#22340=ORIENTED_EDGE('',*,*,#14925,.T.);
#22341=ORIENTED_EDGE('',*,*,#16155,.F.);
#22342=ORIENTED_EDGE('',*,*,#15207,.T.);
#22343=ORIENTED_EDGE('',*,*,#15604,.T.);
#22344=ORIENTED_EDGE('',*,*,#15841,.T.);
#22345=ORIENTED_EDGE('',*,*,#16029,.T.);
#22346=ORIENTED_EDGE('',*,*,#14926,.T.);
#22347=ORIENTED_EDGE('',*,*,#16156,.F.);
#22348=ORIENTED_EDGE('',*,*,#15213,.T.);
#22349=ORIENTED_EDGE('',*,*,#16157,.T.);
#22350=ORIENTED_EDGE('',*,*,#14920,.T.);
#22351=ORIENTED_EDGE('',*,*,#16026,.T.);
#22352=ORIENTED_EDGE('',*,*,#15836,.T.);
#22353=ORIENTED_EDGE('',*,*,#15599,.T.);
#22354=ORIENTED_EDGE('',*,*,#15212,.T.);
#22355=ORIENTED_EDGE('',*,*,#16158,.T.);
#22356=ORIENTED_EDGE('',*,*,#14921,.T.);
#22357=ORIENTED_EDGE('',*,*,#16157,.F.);
#22358=ORIENTED_EDGE('',*,*,#15211,.T.);
#22359=ORIENTED_EDGE('',*,*,#15601,.T.);
#22360=ORIENTED_EDGE('',*,*,#15838,.T.);
#22361=ORIENTED_EDGE('',*,*,#16027,.T.);
#22362=ORIENTED_EDGE('',*,*,#14922,.T.);
#22363=ORIENTED_EDGE('',*,*,#16158,.F.);
#22364=ORIENTED_EDGE('',*,*,#15217,.T.);
#22365=ORIENTED_EDGE('',*,*,#16159,.T.);
#22366=ORIENTED_EDGE('',*,*,#14916,.T.);
#22367=ORIENTED_EDGE('',*,*,#16024,.T.);
#22368=ORIENTED_EDGE('',*,*,#15833,.T.);
#22369=ORIENTED_EDGE('',*,*,#15596,.T.);
#22370=ORIENTED_EDGE('',*,*,#15216,.T.);
#22371=ORIENTED_EDGE('',*,*,#16160,.T.);
#22372=ORIENTED_EDGE('',*,*,#14917,.T.);
#22373=ORIENTED_EDGE('',*,*,#16159,.F.);
#22374=ORIENTED_EDGE('',*,*,#15215,.T.);
#22375=ORIENTED_EDGE('',*,*,#15598,.T.);
#22376=ORIENTED_EDGE('',*,*,#15835,.T.);
#22377=ORIENTED_EDGE('',*,*,#16025,.T.);
#22378=ORIENTED_EDGE('',*,*,#14918,.T.);
#22379=ORIENTED_EDGE('',*,*,#16160,.F.);
#22380=ORIENTED_EDGE('',*,*,#15221,.T.);
#22381=ORIENTED_EDGE('',*,*,#16161,.T.);
#22382=ORIENTED_EDGE('',*,*,#14912,.T.);
#22383=ORIENTED_EDGE('',*,*,#16022,.T.);
#22384=ORIENTED_EDGE('',*,*,#15830,.T.);
#22385=ORIENTED_EDGE('',*,*,#15593,.T.);
#22386=ORIENTED_EDGE('',*,*,#15220,.T.);
#22387=ORIENTED_EDGE('',*,*,#16162,.T.);
#22388=ORIENTED_EDGE('',*,*,#14913,.T.);
#22389=ORIENTED_EDGE('',*,*,#16161,.F.);
#22390=ORIENTED_EDGE('',*,*,#15219,.T.);
#22391=ORIENTED_EDGE('',*,*,#15595,.T.);
#22392=ORIENTED_EDGE('',*,*,#15832,.T.);
#22393=ORIENTED_EDGE('',*,*,#16023,.T.);
#22394=ORIENTED_EDGE('',*,*,#14914,.T.);
#22395=ORIENTED_EDGE('',*,*,#16162,.F.);
#22396=ORIENTED_EDGE('',*,*,#15225,.T.);
#22397=ORIENTED_EDGE('',*,*,#16163,.T.);
#22398=ORIENTED_EDGE('',*,*,#14908,.T.);
#22399=ORIENTED_EDGE('',*,*,#16020,.T.);
#22400=ORIENTED_EDGE('',*,*,#15827,.T.);
#22401=ORIENTED_EDGE('',*,*,#15590,.T.);
#22402=ORIENTED_EDGE('',*,*,#15224,.T.);
#22403=ORIENTED_EDGE('',*,*,#16164,.T.);
#22404=ORIENTED_EDGE('',*,*,#14909,.T.);
#22405=ORIENTED_EDGE('',*,*,#16163,.F.);
#22406=ORIENTED_EDGE('',*,*,#15223,.T.);
#22407=ORIENTED_EDGE('',*,*,#15592,.T.);
#22408=ORIENTED_EDGE('',*,*,#15829,.T.);
#22409=ORIENTED_EDGE('',*,*,#16021,.T.);
#22410=ORIENTED_EDGE('',*,*,#14910,.T.);
#22411=ORIENTED_EDGE('',*,*,#16164,.F.);
#22412=ORIENTED_EDGE('',*,*,#15229,.T.);
#22413=ORIENTED_EDGE('',*,*,#16165,.T.);
#22414=ORIENTED_EDGE('',*,*,#14904,.T.);
#22415=ORIENTED_EDGE('',*,*,#16018,.T.);
#22416=ORIENTED_EDGE('',*,*,#15824,.T.);
#22417=ORIENTED_EDGE('',*,*,#15587,.T.);
#22418=ORIENTED_EDGE('',*,*,#15228,.T.);
#22419=ORIENTED_EDGE('',*,*,#16166,.T.);
#22420=ORIENTED_EDGE('',*,*,#14905,.T.);
#22421=ORIENTED_EDGE('',*,*,#16165,.F.);
#22422=ORIENTED_EDGE('',*,*,#15227,.T.);
#22423=ORIENTED_EDGE('',*,*,#15589,.T.);
#22424=ORIENTED_EDGE('',*,*,#15826,.T.);
#22425=ORIENTED_EDGE('',*,*,#16019,.T.);
#22426=ORIENTED_EDGE('',*,*,#14906,.T.);
#22427=ORIENTED_EDGE('',*,*,#16166,.F.);
#22428=ORIENTED_EDGE('',*,*,#15233,.T.);
#22429=ORIENTED_EDGE('',*,*,#16167,.T.);
#22430=ORIENTED_EDGE('',*,*,#14900,.T.);
#22431=ORIENTED_EDGE('',*,*,#16016,.T.);
#22432=ORIENTED_EDGE('',*,*,#15821,.T.);
#22433=ORIENTED_EDGE('',*,*,#15584,.T.);
#22434=ORIENTED_EDGE('',*,*,#15232,.T.);
#22435=ORIENTED_EDGE('',*,*,#16168,.T.);
#22436=ORIENTED_EDGE('',*,*,#14901,.T.);
#22437=ORIENTED_EDGE('',*,*,#16167,.F.);
#22438=ORIENTED_EDGE('',*,*,#15231,.T.);
#22439=ORIENTED_EDGE('',*,*,#15586,.T.);
#22440=ORIENTED_EDGE('',*,*,#15823,.T.);
#22441=ORIENTED_EDGE('',*,*,#16017,.T.);
#22442=ORIENTED_EDGE('',*,*,#14902,.T.);
#22443=ORIENTED_EDGE('',*,*,#16168,.F.);
#22444=ORIENTED_EDGE('',*,*,#15237,.T.);
#22445=ORIENTED_EDGE('',*,*,#16169,.T.);
#22446=ORIENTED_EDGE('',*,*,#14896,.T.);
#22447=ORIENTED_EDGE('',*,*,#16014,.T.);
#22448=ORIENTED_EDGE('',*,*,#15818,.T.);
#22449=ORIENTED_EDGE('',*,*,#15581,.T.);
#22450=ORIENTED_EDGE('',*,*,#15236,.T.);
#22451=ORIENTED_EDGE('',*,*,#16170,.T.);
#22452=ORIENTED_EDGE('',*,*,#14897,.T.);
#22453=ORIENTED_EDGE('',*,*,#16169,.F.);
#22454=ORIENTED_EDGE('',*,*,#15235,.T.);
#22455=ORIENTED_EDGE('',*,*,#15583,.T.);
#22456=ORIENTED_EDGE('',*,*,#15820,.T.);
#22457=ORIENTED_EDGE('',*,*,#16015,.T.);
#22458=ORIENTED_EDGE('',*,*,#14898,.T.);
#22459=ORIENTED_EDGE('',*,*,#16170,.F.);
#22460=ORIENTED_EDGE('',*,*,#15241,.T.);
#22461=ORIENTED_EDGE('',*,*,#16171,.T.);
#22462=ORIENTED_EDGE('',*,*,#14892,.T.);
#22463=ORIENTED_EDGE('',*,*,#16012,.T.);
#22464=ORIENTED_EDGE('',*,*,#15815,.T.);
#22465=ORIENTED_EDGE('',*,*,#15578,.T.);
#22466=ORIENTED_EDGE('',*,*,#15240,.T.);
#22467=ORIENTED_EDGE('',*,*,#16172,.T.);
#22468=ORIENTED_EDGE('',*,*,#14893,.T.);
#22469=ORIENTED_EDGE('',*,*,#16171,.F.);
#22470=ORIENTED_EDGE('',*,*,#15239,.T.);
#22471=ORIENTED_EDGE('',*,*,#15580,.T.);
#22472=ORIENTED_EDGE('',*,*,#15817,.T.);
#22473=ORIENTED_EDGE('',*,*,#16013,.T.);
#22474=ORIENTED_EDGE('',*,*,#14894,.T.);
#22475=ORIENTED_EDGE('',*,*,#16172,.F.);
#22476=ORIENTED_EDGE('',*,*,#15245,.T.);
#22477=ORIENTED_EDGE('',*,*,#16173,.T.);
#22478=ORIENTED_EDGE('',*,*,#14888,.T.);
#22479=ORIENTED_EDGE('',*,*,#16010,.T.);
#22480=ORIENTED_EDGE('',*,*,#15812,.T.);
#22481=ORIENTED_EDGE('',*,*,#15575,.T.);
#22482=ORIENTED_EDGE('',*,*,#15244,.T.);
#22483=ORIENTED_EDGE('',*,*,#16174,.T.);
#22484=ORIENTED_EDGE('',*,*,#14889,.T.);
#22485=ORIENTED_EDGE('',*,*,#16173,.F.);
#22486=ORIENTED_EDGE('',*,*,#15243,.T.);
#22487=ORIENTED_EDGE('',*,*,#15577,.T.);
#22488=ORIENTED_EDGE('',*,*,#15814,.T.);
#22489=ORIENTED_EDGE('',*,*,#16011,.T.);
#22490=ORIENTED_EDGE('',*,*,#14890,.T.);
#22491=ORIENTED_EDGE('',*,*,#16174,.F.);
#22492=ORIENTED_EDGE('',*,*,#15249,.T.);
#22493=ORIENTED_EDGE('',*,*,#16175,.T.);
#22494=ORIENTED_EDGE('',*,*,#14884,.T.);
#22495=ORIENTED_EDGE('',*,*,#16008,.T.);
#22496=ORIENTED_EDGE('',*,*,#15809,.T.);
#22497=ORIENTED_EDGE('',*,*,#15572,.T.);
#22498=ORIENTED_EDGE('',*,*,#15248,.T.);
#22499=ORIENTED_EDGE('',*,*,#16176,.T.);
#22500=ORIENTED_EDGE('',*,*,#14885,.T.);
#22501=ORIENTED_EDGE('',*,*,#16175,.F.);
#22502=ORIENTED_EDGE('',*,*,#15247,.T.);
#22503=ORIENTED_EDGE('',*,*,#15574,.T.);
#22504=ORIENTED_EDGE('',*,*,#15811,.T.);
#22505=ORIENTED_EDGE('',*,*,#16009,.T.);
#22506=ORIENTED_EDGE('',*,*,#14886,.T.);
#22507=ORIENTED_EDGE('',*,*,#16176,.F.);
#22508=ORIENTED_EDGE('',*,*,#15253,.T.);
#22509=ORIENTED_EDGE('',*,*,#16177,.T.);
#22510=ORIENTED_EDGE('',*,*,#14880,.T.);
#22511=ORIENTED_EDGE('',*,*,#16006,.T.);
#22512=ORIENTED_EDGE('',*,*,#15806,.T.);
#22513=ORIENTED_EDGE('',*,*,#15569,.T.);
#22514=ORIENTED_EDGE('',*,*,#15252,.T.);
#22515=ORIENTED_EDGE('',*,*,#16178,.T.);
#22516=ORIENTED_EDGE('',*,*,#14881,.T.);
#22517=ORIENTED_EDGE('',*,*,#16177,.F.);
#22518=ORIENTED_EDGE('',*,*,#15251,.T.);
#22519=ORIENTED_EDGE('',*,*,#15571,.T.);
#22520=ORIENTED_EDGE('',*,*,#15808,.T.);
#22521=ORIENTED_EDGE('',*,*,#16007,.T.);
#22522=ORIENTED_EDGE('',*,*,#14882,.T.);
#22523=ORIENTED_EDGE('',*,*,#16178,.F.);
#22524=ORIENTED_EDGE('',*,*,#15257,.T.);
#22525=ORIENTED_EDGE('',*,*,#16179,.T.);
#22526=ORIENTED_EDGE('',*,*,#14876,.T.);
#22527=ORIENTED_EDGE('',*,*,#16004,.T.);
#22528=ORIENTED_EDGE('',*,*,#15803,.T.);
#22529=ORIENTED_EDGE('',*,*,#15566,.T.);
#22530=ORIENTED_EDGE('',*,*,#15256,.T.);
#22531=ORIENTED_EDGE('',*,*,#16180,.T.);
#22532=ORIENTED_EDGE('',*,*,#14877,.T.);
#22533=ORIENTED_EDGE('',*,*,#16179,.F.);
#22534=ORIENTED_EDGE('',*,*,#15255,.T.);
#22535=ORIENTED_EDGE('',*,*,#15568,.T.);
#22536=ORIENTED_EDGE('',*,*,#15805,.T.);
#22537=ORIENTED_EDGE('',*,*,#16005,.T.);
#22538=ORIENTED_EDGE('',*,*,#14878,.T.);
#22539=ORIENTED_EDGE('',*,*,#16180,.F.);
#22540=ORIENTED_EDGE('',*,*,#15261,.T.);
#22541=ORIENTED_EDGE('',*,*,#16181,.T.);
#22542=ORIENTED_EDGE('',*,*,#14872,.T.);
#22543=ORIENTED_EDGE('',*,*,#16002,.T.);
#22544=ORIENTED_EDGE('',*,*,#15800,.T.);
#22545=ORIENTED_EDGE('',*,*,#15563,.T.);
#22546=ORIENTED_EDGE('',*,*,#15260,.T.);
#22547=ORIENTED_EDGE('',*,*,#16182,.T.);
#22548=ORIENTED_EDGE('',*,*,#14873,.T.);
#22549=ORIENTED_EDGE('',*,*,#16181,.F.);
#22550=ORIENTED_EDGE('',*,*,#15259,.T.);
#22551=ORIENTED_EDGE('',*,*,#15565,.T.);
#22552=ORIENTED_EDGE('',*,*,#15802,.T.);
#22553=ORIENTED_EDGE('',*,*,#16003,.T.);
#22554=ORIENTED_EDGE('',*,*,#14874,.T.);
#22555=ORIENTED_EDGE('',*,*,#16182,.F.);
#22556=ORIENTED_EDGE('',*,*,#15265,.T.);
#22557=ORIENTED_EDGE('',*,*,#16183,.T.);
#22558=ORIENTED_EDGE('',*,*,#14868,.T.);
#22559=ORIENTED_EDGE('',*,*,#16000,.T.);
#22560=ORIENTED_EDGE('',*,*,#15797,.T.);
#22561=ORIENTED_EDGE('',*,*,#15560,.T.);
#22562=ORIENTED_EDGE('',*,*,#15264,.T.);
#22563=ORIENTED_EDGE('',*,*,#16184,.T.);
#22564=ORIENTED_EDGE('',*,*,#14869,.T.);
#22565=ORIENTED_EDGE('',*,*,#16183,.F.);
#22566=ORIENTED_EDGE('',*,*,#15263,.T.);
#22567=ORIENTED_EDGE('',*,*,#15562,.T.);
#22568=ORIENTED_EDGE('',*,*,#15799,.T.);
#22569=ORIENTED_EDGE('',*,*,#16001,.T.);
#22570=ORIENTED_EDGE('',*,*,#14870,.T.);
#22571=ORIENTED_EDGE('',*,*,#16184,.F.);
#22572=ORIENTED_EDGE('',*,*,#15269,.T.);
#22573=ORIENTED_EDGE('',*,*,#16185,.T.);
#22574=ORIENTED_EDGE('',*,*,#14864,.T.);
#22575=ORIENTED_EDGE('',*,*,#15998,.T.);
#22576=ORIENTED_EDGE('',*,*,#15794,.T.);
#22577=ORIENTED_EDGE('',*,*,#15557,.T.);
#22578=ORIENTED_EDGE('',*,*,#15268,.T.);
#22579=ORIENTED_EDGE('',*,*,#16186,.T.);
#22580=ORIENTED_EDGE('',*,*,#14865,.T.);
#22581=ORIENTED_EDGE('',*,*,#16185,.F.);
#22582=ORIENTED_EDGE('',*,*,#15267,.T.);
#22583=ORIENTED_EDGE('',*,*,#15559,.T.);
#22584=ORIENTED_EDGE('',*,*,#15796,.T.);
#22585=ORIENTED_EDGE('',*,*,#15999,.T.);
#22586=ORIENTED_EDGE('',*,*,#14866,.T.);
#22587=ORIENTED_EDGE('',*,*,#16186,.F.);
#22588=ORIENTED_EDGE('',*,*,#15273,.T.);
#22589=ORIENTED_EDGE('',*,*,#16187,.T.);
#22590=ORIENTED_EDGE('',*,*,#14860,.T.);
#22591=ORIENTED_EDGE('',*,*,#15996,.T.);
#22592=ORIENTED_EDGE('',*,*,#15791,.T.);
#22593=ORIENTED_EDGE('',*,*,#15554,.T.);
#22594=ORIENTED_EDGE('',*,*,#15272,.T.);
#22595=ORIENTED_EDGE('',*,*,#16188,.T.);
#22596=ORIENTED_EDGE('',*,*,#14861,.T.);
#22597=ORIENTED_EDGE('',*,*,#16187,.F.);
#22598=ORIENTED_EDGE('',*,*,#15271,.T.);
#22599=ORIENTED_EDGE('',*,*,#15556,.T.);
#22600=ORIENTED_EDGE('',*,*,#15793,.T.);
#22601=ORIENTED_EDGE('',*,*,#15997,.T.);
#22602=ORIENTED_EDGE('',*,*,#14862,.T.);
#22603=ORIENTED_EDGE('',*,*,#16188,.F.);
#22604=ORIENTED_EDGE('',*,*,#15277,.T.);
#22605=ORIENTED_EDGE('',*,*,#16189,.T.);
#22606=ORIENTED_EDGE('',*,*,#14856,.T.);
#22607=ORIENTED_EDGE('',*,*,#15994,.T.);
#22608=ORIENTED_EDGE('',*,*,#15788,.T.);
#22609=ORIENTED_EDGE('',*,*,#15551,.T.);
#22610=ORIENTED_EDGE('',*,*,#15276,.T.);
#22611=ORIENTED_EDGE('',*,*,#16190,.T.);
#22612=ORIENTED_EDGE('',*,*,#14857,.T.);
#22613=ORIENTED_EDGE('',*,*,#16189,.F.);
#22614=ORIENTED_EDGE('',*,*,#15275,.T.);
#22615=ORIENTED_EDGE('',*,*,#15553,.T.);
#22616=ORIENTED_EDGE('',*,*,#15790,.T.);
#22617=ORIENTED_EDGE('',*,*,#15995,.T.);
#22618=ORIENTED_EDGE('',*,*,#14858,.T.);
#22619=ORIENTED_EDGE('',*,*,#16190,.F.);
#22620=ORIENTED_EDGE('',*,*,#15281,.T.);
#22621=ORIENTED_EDGE('',*,*,#16191,.T.);
#22622=ORIENTED_EDGE('',*,*,#14852,.T.);
#22623=ORIENTED_EDGE('',*,*,#15992,.T.);
#22624=ORIENTED_EDGE('',*,*,#15785,.T.);
#22625=ORIENTED_EDGE('',*,*,#15548,.T.);
#22626=ORIENTED_EDGE('',*,*,#15280,.T.);
#22627=ORIENTED_EDGE('',*,*,#16192,.T.);
#22628=ORIENTED_EDGE('',*,*,#14853,.T.);
#22629=ORIENTED_EDGE('',*,*,#16191,.F.);
#22630=ORIENTED_EDGE('',*,*,#15279,.T.);
#22631=ORIENTED_EDGE('',*,*,#15550,.T.);
#22632=ORIENTED_EDGE('',*,*,#15787,.T.);
#22633=ORIENTED_EDGE('',*,*,#15993,.T.);
#22634=ORIENTED_EDGE('',*,*,#14854,.T.);
#22635=ORIENTED_EDGE('',*,*,#16192,.F.);
#22636=ORIENTED_EDGE('',*,*,#15285,.T.);
#22637=ORIENTED_EDGE('',*,*,#16193,.T.);
#22638=ORIENTED_EDGE('',*,*,#14848,.T.);
#22639=ORIENTED_EDGE('',*,*,#15990,.T.);
#22640=ORIENTED_EDGE('',*,*,#15782,.T.);
#22641=ORIENTED_EDGE('',*,*,#15545,.T.);
#22642=ORIENTED_EDGE('',*,*,#15284,.T.);
#22643=ORIENTED_EDGE('',*,*,#16194,.T.);
#22644=ORIENTED_EDGE('',*,*,#14849,.T.);
#22645=ORIENTED_EDGE('',*,*,#16193,.F.);
#22646=ORIENTED_EDGE('',*,*,#15283,.T.);
#22647=ORIENTED_EDGE('',*,*,#15547,.T.);
#22648=ORIENTED_EDGE('',*,*,#15784,.T.);
#22649=ORIENTED_EDGE('',*,*,#15991,.T.);
#22650=ORIENTED_EDGE('',*,*,#14850,.T.);
#22651=ORIENTED_EDGE('',*,*,#16194,.F.);
#22652=ORIENTED_EDGE('',*,*,#15289,.T.);
#22653=ORIENTED_EDGE('',*,*,#16195,.T.);
#22654=ORIENTED_EDGE('',*,*,#14844,.T.);
#22655=ORIENTED_EDGE('',*,*,#15988,.T.);
#22656=ORIENTED_EDGE('',*,*,#15779,.T.);
#22657=ORIENTED_EDGE('',*,*,#15542,.T.);
#22658=ORIENTED_EDGE('',*,*,#15288,.T.);
#22659=ORIENTED_EDGE('',*,*,#16196,.T.);
#22660=ORIENTED_EDGE('',*,*,#14845,.T.);
#22661=ORIENTED_EDGE('',*,*,#16195,.F.);
#22662=ORIENTED_EDGE('',*,*,#15287,.T.);
#22663=ORIENTED_EDGE('',*,*,#15544,.T.);
#22664=ORIENTED_EDGE('',*,*,#15781,.T.);
#22665=ORIENTED_EDGE('',*,*,#15989,.T.);
#22666=ORIENTED_EDGE('',*,*,#14846,.T.);
#22667=ORIENTED_EDGE('',*,*,#16196,.F.);
#22668=ORIENTED_EDGE('',*,*,#15293,.T.);
#22669=ORIENTED_EDGE('',*,*,#16197,.T.);
#22670=ORIENTED_EDGE('',*,*,#14840,.T.);
#22671=ORIENTED_EDGE('',*,*,#15986,.T.);
#22672=ORIENTED_EDGE('',*,*,#15776,.T.);
#22673=ORIENTED_EDGE('',*,*,#15539,.T.);
#22674=ORIENTED_EDGE('',*,*,#15292,.T.);
#22675=ORIENTED_EDGE('',*,*,#16198,.T.);
#22676=ORIENTED_EDGE('',*,*,#14841,.T.);
#22677=ORIENTED_EDGE('',*,*,#16197,.F.);
#22678=ORIENTED_EDGE('',*,*,#15291,.T.);
#22679=ORIENTED_EDGE('',*,*,#15541,.T.);
#22680=ORIENTED_EDGE('',*,*,#15778,.T.);
#22681=ORIENTED_EDGE('',*,*,#15987,.T.);
#22682=ORIENTED_EDGE('',*,*,#14842,.T.);
#22683=ORIENTED_EDGE('',*,*,#16198,.F.);
#22684=ORIENTED_EDGE('',*,*,#15297,.T.);
#22685=ORIENTED_EDGE('',*,*,#16199,.T.);
#22686=ORIENTED_EDGE('',*,*,#14836,.T.);
#22687=ORIENTED_EDGE('',*,*,#15984,.T.);
#22688=ORIENTED_EDGE('',*,*,#15773,.T.);
#22689=ORIENTED_EDGE('',*,*,#15536,.T.);
#22690=ORIENTED_EDGE('',*,*,#15296,.T.);
#22691=ORIENTED_EDGE('',*,*,#16200,.T.);
#22692=ORIENTED_EDGE('',*,*,#14837,.T.);
#22693=ORIENTED_EDGE('',*,*,#16199,.F.);
#22694=ORIENTED_EDGE('',*,*,#15295,.T.);
#22695=ORIENTED_EDGE('',*,*,#15538,.T.);
#22696=ORIENTED_EDGE('',*,*,#15775,.T.);
#22697=ORIENTED_EDGE('',*,*,#15985,.T.);
#22698=ORIENTED_EDGE('',*,*,#14838,.T.);
#22699=ORIENTED_EDGE('',*,*,#16200,.F.);
#22700=ORIENTED_EDGE('',*,*,#15301,.T.);
#22701=ORIENTED_EDGE('',*,*,#16201,.T.);
#22702=ORIENTED_EDGE('',*,*,#15137,.T.);
#22703=ORIENTED_EDGE('',*,*,#15982,.T.);
#22704=ORIENTED_EDGE('',*,*,#15770,.T.);
#22705=ORIENTED_EDGE('',*,*,#15533,.T.);
#22706=ORIENTED_EDGE('',*,*,#15300,.T.);
#22707=ORIENTED_EDGE('',*,*,#16202,.T.);
#22708=ORIENTED_EDGE('',*,*,#14833,.T.);
#22709=ORIENTED_EDGE('',*,*,#15138,.T.);
#22710=ORIENTED_EDGE('',*,*,#16201,.F.);
#22711=ORIENTED_EDGE('',*,*,#15299,.T.);
#22712=ORIENTED_EDGE('',*,*,#15535,.T.);
#22713=ORIENTED_EDGE('',*,*,#15772,.T.);
#22714=ORIENTED_EDGE('',*,*,#15983,.T.);
#22715=ORIENTED_EDGE('',*,*,#14834,.T.);
#22716=ORIENTED_EDGE('',*,*,#16202,.F.);
#22717=ORIENTED_EDGE('',*,*,#15305,.T.);
#22718=ORIENTED_EDGE('',*,*,#16203,.T.);
#22719=ORIENTED_EDGE('',*,*,#15133,.T.);
#22720=ORIENTED_EDGE('',*,*,#15980,.T.);
#22721=ORIENTED_EDGE('',*,*,#15767,.T.);
#22722=ORIENTED_EDGE('',*,*,#15530,.T.);
#22723=ORIENTED_EDGE('',*,*,#15304,.T.);
#22724=ORIENTED_EDGE('',*,*,#16204,.T.);
#22725=ORIENTED_EDGE('',*,*,#15134,.T.);
#22726=ORIENTED_EDGE('',*,*,#16203,.F.);
#22727=ORIENTED_EDGE('',*,*,#15303,.T.);
#22728=ORIENTED_EDGE('',*,*,#15532,.T.);
#22729=ORIENTED_EDGE('',*,*,#15769,.T.);
#22730=ORIENTED_EDGE('',*,*,#15981,.T.);
#22731=ORIENTED_EDGE('',*,*,#15135,.T.);
#22732=ORIENTED_EDGE('',*,*,#16204,.F.);
#22733=ORIENTED_EDGE('',*,*,#15309,.T.);
#22734=ORIENTED_EDGE('',*,*,#16205,.T.);
#22735=ORIENTED_EDGE('',*,*,#15129,.T.);
#22736=ORIENTED_EDGE('',*,*,#15978,.T.);
#22737=ORIENTED_EDGE('',*,*,#15764,.T.);
#22738=ORIENTED_EDGE('',*,*,#15527,.T.);
#22739=ORIENTED_EDGE('',*,*,#15308,.T.);
#22740=ORIENTED_EDGE('',*,*,#16206,.T.);
#22741=ORIENTED_EDGE('',*,*,#15130,.T.);
#22742=ORIENTED_EDGE('',*,*,#16205,.F.);
#22743=ORIENTED_EDGE('',*,*,#15307,.T.);
#22744=ORIENTED_EDGE('',*,*,#15529,.T.);
#22745=ORIENTED_EDGE('',*,*,#15766,.T.);
#22746=ORIENTED_EDGE('',*,*,#15979,.T.);
#22747=ORIENTED_EDGE('',*,*,#15131,.T.);
#22748=ORIENTED_EDGE('',*,*,#16206,.F.);
#22749=ORIENTED_EDGE('',*,*,#15313,.T.);
#22750=ORIENTED_EDGE('',*,*,#16207,.T.);
#22751=ORIENTED_EDGE('',*,*,#15125,.T.);
#22752=ORIENTED_EDGE('',*,*,#15976,.T.);
#22753=ORIENTED_EDGE('',*,*,#15761,.T.);
#22754=ORIENTED_EDGE('',*,*,#15524,.T.);
#22755=ORIENTED_EDGE('',*,*,#15312,.T.);
#22756=ORIENTED_EDGE('',*,*,#16208,.T.);
#22757=ORIENTED_EDGE('',*,*,#15126,.T.);
#22758=ORIENTED_EDGE('',*,*,#16207,.F.);
#22759=ORIENTED_EDGE('',*,*,#15311,.T.);
#22760=ORIENTED_EDGE('',*,*,#15526,.T.);
#22761=ORIENTED_EDGE('',*,*,#15763,.T.);
#22762=ORIENTED_EDGE('',*,*,#15977,.T.);
#22763=ORIENTED_EDGE('',*,*,#15127,.T.);
#22764=ORIENTED_EDGE('',*,*,#16208,.F.);
#22765=ORIENTED_EDGE('',*,*,#15317,.T.);
#22766=ORIENTED_EDGE('',*,*,#16209,.T.);
#22767=ORIENTED_EDGE('',*,*,#15121,.T.);
#22768=ORIENTED_EDGE('',*,*,#15974,.T.);
#22769=ORIENTED_EDGE('',*,*,#15758,.T.);
#22770=ORIENTED_EDGE('',*,*,#15521,.T.);
#22771=ORIENTED_EDGE('',*,*,#15316,.T.);
#22772=ORIENTED_EDGE('',*,*,#16210,.T.);
#22773=ORIENTED_EDGE('',*,*,#15122,.T.);
#22774=ORIENTED_EDGE('',*,*,#16209,.F.);
#22775=ORIENTED_EDGE('',*,*,#15315,.T.);
#22776=ORIENTED_EDGE('',*,*,#15523,.T.);
#22777=ORIENTED_EDGE('',*,*,#15760,.T.);
#22778=ORIENTED_EDGE('',*,*,#15975,.T.);
#22779=ORIENTED_EDGE('',*,*,#15123,.T.);
#22780=ORIENTED_EDGE('',*,*,#16210,.F.);
#22781=ORIENTED_EDGE('',*,*,#15321,.T.);
#22782=ORIENTED_EDGE('',*,*,#16211,.T.);
#22783=ORIENTED_EDGE('',*,*,#15117,.T.);
#22784=ORIENTED_EDGE('',*,*,#15972,.T.);
#22785=ORIENTED_EDGE('',*,*,#15755,.T.);
#22786=ORIENTED_EDGE('',*,*,#15518,.T.);
#22787=ORIENTED_EDGE('',*,*,#15320,.T.);
#22788=ORIENTED_EDGE('',*,*,#16212,.T.);
#22789=ORIENTED_EDGE('',*,*,#15118,.T.);
#22790=ORIENTED_EDGE('',*,*,#16211,.F.);
#22791=ORIENTED_EDGE('',*,*,#15319,.T.);
#22792=ORIENTED_EDGE('',*,*,#15520,.T.);
#22793=ORIENTED_EDGE('',*,*,#15757,.T.);
#22794=ORIENTED_EDGE('',*,*,#15973,.T.);
#22795=ORIENTED_EDGE('',*,*,#15119,.T.);
#22796=ORIENTED_EDGE('',*,*,#16212,.F.);
#22797=ORIENTED_EDGE('',*,*,#15325,.T.);
#22798=ORIENTED_EDGE('',*,*,#16213,.T.);
#22799=ORIENTED_EDGE('',*,*,#15113,.T.);
#22800=ORIENTED_EDGE('',*,*,#15970,.T.);
#22801=ORIENTED_EDGE('',*,*,#15752,.T.);
#22802=ORIENTED_EDGE('',*,*,#15515,.T.);
#22803=ORIENTED_EDGE('',*,*,#15324,.T.);
#22804=ORIENTED_EDGE('',*,*,#16214,.T.);
#22805=ORIENTED_EDGE('',*,*,#15114,.T.);
#22806=ORIENTED_EDGE('',*,*,#16213,.F.);
#22807=ORIENTED_EDGE('',*,*,#15323,.T.);
#22808=ORIENTED_EDGE('',*,*,#15517,.T.);
#22809=ORIENTED_EDGE('',*,*,#15754,.T.);
#22810=ORIENTED_EDGE('',*,*,#15971,.T.);
#22811=ORIENTED_EDGE('',*,*,#15115,.T.);
#22812=ORIENTED_EDGE('',*,*,#16214,.F.);
#22813=ORIENTED_EDGE('',*,*,#15329,.T.);
#22814=ORIENTED_EDGE('',*,*,#16215,.T.);
#22815=ORIENTED_EDGE('',*,*,#15109,.T.);
#22816=ORIENTED_EDGE('',*,*,#15968,.T.);
#22817=ORIENTED_EDGE('',*,*,#15749,.T.);
#22818=ORIENTED_EDGE('',*,*,#15512,.T.);
#22819=ORIENTED_EDGE('',*,*,#15328,.T.);
#22820=ORIENTED_EDGE('',*,*,#16216,.T.);
#22821=ORIENTED_EDGE('',*,*,#15110,.T.);
#22822=ORIENTED_EDGE('',*,*,#16215,.F.);
#22823=ORIENTED_EDGE('',*,*,#15327,.T.);
#22824=ORIENTED_EDGE('',*,*,#15514,.T.);
#22825=ORIENTED_EDGE('',*,*,#15751,.T.);
#22826=ORIENTED_EDGE('',*,*,#15969,.T.);
#22827=ORIENTED_EDGE('',*,*,#15111,.T.);
#22828=ORIENTED_EDGE('',*,*,#16216,.F.);
#22829=ORIENTED_EDGE('',*,*,#15333,.T.);
#22830=ORIENTED_EDGE('',*,*,#16217,.T.);
#22831=ORIENTED_EDGE('',*,*,#15105,.T.);
#22832=ORIENTED_EDGE('',*,*,#15966,.T.);
#22833=ORIENTED_EDGE('',*,*,#15746,.T.);
#22834=ORIENTED_EDGE('',*,*,#15509,.T.);
#22835=ORIENTED_EDGE('',*,*,#15332,.T.);
#22836=ORIENTED_EDGE('',*,*,#16218,.T.);
#22837=ORIENTED_EDGE('',*,*,#15106,.T.);
#22838=ORIENTED_EDGE('',*,*,#16217,.F.);
#22839=ORIENTED_EDGE('',*,*,#15331,.T.);
#22840=ORIENTED_EDGE('',*,*,#15511,.T.);
#22841=ORIENTED_EDGE('',*,*,#15748,.T.);
#22842=ORIENTED_EDGE('',*,*,#15967,.T.);
#22843=ORIENTED_EDGE('',*,*,#15107,.T.);
#22844=ORIENTED_EDGE('',*,*,#16218,.F.);
#22845=ORIENTED_EDGE('',*,*,#15337,.T.);
#22846=ORIENTED_EDGE('',*,*,#16219,.T.);
#22847=ORIENTED_EDGE('',*,*,#15101,.T.);
#22848=ORIENTED_EDGE('',*,*,#15964,.T.);
#22849=ORIENTED_EDGE('',*,*,#15743,.T.);
#22850=ORIENTED_EDGE('',*,*,#15506,.T.);
#22851=ORIENTED_EDGE('',*,*,#15336,.T.);
#22852=ORIENTED_EDGE('',*,*,#16220,.T.);
#22853=ORIENTED_EDGE('',*,*,#15102,.T.);
#22854=ORIENTED_EDGE('',*,*,#16219,.F.);
#22855=ORIENTED_EDGE('',*,*,#15335,.T.);
#22856=ORIENTED_EDGE('',*,*,#15508,.T.);
#22857=ORIENTED_EDGE('',*,*,#15745,.T.);
#22858=ORIENTED_EDGE('',*,*,#15965,.T.);
#22859=ORIENTED_EDGE('',*,*,#15103,.T.);
#22860=ORIENTED_EDGE('',*,*,#16220,.F.);
#22861=ORIENTED_EDGE('',*,*,#15341,.T.);
#22862=ORIENTED_EDGE('',*,*,#16221,.T.);
#22863=ORIENTED_EDGE('',*,*,#15097,.T.);
#22864=ORIENTED_EDGE('',*,*,#15962,.T.);
#22865=ORIENTED_EDGE('',*,*,#15740,.T.);
#22866=ORIENTED_EDGE('',*,*,#15503,.T.);
#22867=ORIENTED_EDGE('',*,*,#15340,.T.);
#22868=ORIENTED_EDGE('',*,*,#16222,.T.);
#22869=ORIENTED_EDGE('',*,*,#15098,.T.);
#22870=ORIENTED_EDGE('',*,*,#16221,.F.);
#22871=ORIENTED_EDGE('',*,*,#15339,.T.);
#22872=ORIENTED_EDGE('',*,*,#15505,.T.);
#22873=ORIENTED_EDGE('',*,*,#15742,.T.);
#22874=ORIENTED_EDGE('',*,*,#15963,.T.);
#22875=ORIENTED_EDGE('',*,*,#15099,.T.);
#22876=ORIENTED_EDGE('',*,*,#16222,.F.);
#22877=ORIENTED_EDGE('',*,*,#15345,.T.);
#22878=ORIENTED_EDGE('',*,*,#16223,.T.);
#22879=ORIENTED_EDGE('',*,*,#15093,.T.);
#22880=ORIENTED_EDGE('',*,*,#15960,.T.);
#22881=ORIENTED_EDGE('',*,*,#15737,.T.);
#22882=ORIENTED_EDGE('',*,*,#15500,.T.);
#22883=ORIENTED_EDGE('',*,*,#15344,.T.);
#22884=ORIENTED_EDGE('',*,*,#16224,.T.);
#22885=ORIENTED_EDGE('',*,*,#15094,.T.);
#22886=ORIENTED_EDGE('',*,*,#16223,.F.);
#22887=ORIENTED_EDGE('',*,*,#15343,.T.);
#22888=ORIENTED_EDGE('',*,*,#15502,.T.);
#22889=ORIENTED_EDGE('',*,*,#15739,.T.);
#22890=ORIENTED_EDGE('',*,*,#15961,.T.);
#22891=ORIENTED_EDGE('',*,*,#15095,.T.);
#22892=ORIENTED_EDGE('',*,*,#16224,.F.);
#22893=ORIENTED_EDGE('',*,*,#15349,.T.);
#22894=ORIENTED_EDGE('',*,*,#16225,.T.);
#22895=ORIENTED_EDGE('',*,*,#15089,.T.);
#22896=ORIENTED_EDGE('',*,*,#15958,.T.);
#22897=ORIENTED_EDGE('',*,*,#15734,.T.);
#22898=ORIENTED_EDGE('',*,*,#15497,.T.);
#22899=ORIENTED_EDGE('',*,*,#15348,.T.);
#22900=ORIENTED_EDGE('',*,*,#16226,.T.);
#22901=ORIENTED_EDGE('',*,*,#15090,.T.);
#22902=ORIENTED_EDGE('',*,*,#16225,.F.);
#22903=ORIENTED_EDGE('',*,*,#15347,.T.);
#22904=ORIENTED_EDGE('',*,*,#15499,.T.);
#22905=ORIENTED_EDGE('',*,*,#15736,.T.);
#22906=ORIENTED_EDGE('',*,*,#15959,.T.);
#22907=ORIENTED_EDGE('',*,*,#15091,.T.);
#22908=ORIENTED_EDGE('',*,*,#16226,.F.);
#22909=ORIENTED_EDGE('',*,*,#15353,.T.);
#22910=ORIENTED_EDGE('',*,*,#16227,.T.);
#22911=ORIENTED_EDGE('',*,*,#15085,.T.);
#22912=ORIENTED_EDGE('',*,*,#15956,.T.);
#22913=ORIENTED_EDGE('',*,*,#15731,.T.);
#22914=ORIENTED_EDGE('',*,*,#15494,.T.);
#22915=ORIENTED_EDGE('',*,*,#15352,.T.);
#22916=ORIENTED_EDGE('',*,*,#16228,.T.);
#22917=ORIENTED_EDGE('',*,*,#15086,.T.);
#22918=ORIENTED_EDGE('',*,*,#16227,.F.);
#22919=ORIENTED_EDGE('',*,*,#15351,.T.);
#22920=ORIENTED_EDGE('',*,*,#15496,.T.);
#22921=ORIENTED_EDGE('',*,*,#15733,.T.);
#22922=ORIENTED_EDGE('',*,*,#15957,.T.);
#22923=ORIENTED_EDGE('',*,*,#15087,.T.);
#22924=ORIENTED_EDGE('',*,*,#16228,.F.);
#22925=ORIENTED_EDGE('',*,*,#15357,.T.);
#22926=ORIENTED_EDGE('',*,*,#16229,.T.);
#22927=ORIENTED_EDGE('',*,*,#15081,.T.);
#22928=ORIENTED_EDGE('',*,*,#15954,.T.);
#22929=ORIENTED_EDGE('',*,*,#15728,.T.);
#22930=ORIENTED_EDGE('',*,*,#15491,.T.);
#22931=ORIENTED_EDGE('',*,*,#15356,.T.);
#22932=ORIENTED_EDGE('',*,*,#16230,.T.);
#22933=ORIENTED_EDGE('',*,*,#15082,.T.);
#22934=ORIENTED_EDGE('',*,*,#16229,.F.);
#22935=ORIENTED_EDGE('',*,*,#15355,.T.);
#22936=ORIENTED_EDGE('',*,*,#15493,.T.);
#22937=ORIENTED_EDGE('',*,*,#15730,.T.);
#22938=ORIENTED_EDGE('',*,*,#15955,.T.);
#22939=ORIENTED_EDGE('',*,*,#15083,.T.);
#22940=ORIENTED_EDGE('',*,*,#16230,.F.);
#22941=ORIENTED_EDGE('',*,*,#15361,.T.);
#22942=ORIENTED_EDGE('',*,*,#16231,.T.);
#22943=ORIENTED_EDGE('',*,*,#15077,.T.);
#22944=ORIENTED_EDGE('',*,*,#15952,.T.);
#22945=ORIENTED_EDGE('',*,*,#15725,.T.);
#22946=ORIENTED_EDGE('',*,*,#15488,.T.);
#22947=ORIENTED_EDGE('',*,*,#15360,.T.);
#22948=ORIENTED_EDGE('',*,*,#16232,.T.);
#22949=ORIENTED_EDGE('',*,*,#15078,.T.);
#22950=ORIENTED_EDGE('',*,*,#16231,.F.);
#22951=ORIENTED_EDGE('',*,*,#15359,.T.);
#22952=ORIENTED_EDGE('',*,*,#15490,.T.);
#22953=ORIENTED_EDGE('',*,*,#15727,.T.);
#22954=ORIENTED_EDGE('',*,*,#15953,.T.);
#22955=ORIENTED_EDGE('',*,*,#15079,.T.);
#22956=ORIENTED_EDGE('',*,*,#16232,.F.);
#22957=ORIENTED_EDGE('',*,*,#15365,.T.);
#22958=ORIENTED_EDGE('',*,*,#16233,.T.);
#22959=ORIENTED_EDGE('',*,*,#15073,.T.);
#22960=ORIENTED_EDGE('',*,*,#15950,.T.);
#22961=ORIENTED_EDGE('',*,*,#15722,.T.);
#22962=ORIENTED_EDGE('',*,*,#15485,.T.);
#22963=ORIENTED_EDGE('',*,*,#15364,.T.);
#22964=ORIENTED_EDGE('',*,*,#16234,.T.);
#22965=ORIENTED_EDGE('',*,*,#15074,.T.);
#22966=ORIENTED_EDGE('',*,*,#16233,.F.);
#22967=ORIENTED_EDGE('',*,*,#15363,.T.);
#22968=ORIENTED_EDGE('',*,*,#15487,.T.);
#22969=ORIENTED_EDGE('',*,*,#15724,.T.);
#22970=ORIENTED_EDGE('',*,*,#15951,.T.);
#22971=ORIENTED_EDGE('',*,*,#15075,.T.);
#22972=ORIENTED_EDGE('',*,*,#16234,.F.);
#22973=ORIENTED_EDGE('',*,*,#15369,.T.);
#22974=ORIENTED_EDGE('',*,*,#16235,.T.);
#22975=ORIENTED_EDGE('',*,*,#15069,.T.);
#22976=ORIENTED_EDGE('',*,*,#15948,.T.);
#22977=ORIENTED_EDGE('',*,*,#15719,.T.);
#22978=ORIENTED_EDGE('',*,*,#15482,.T.);
#22979=ORIENTED_EDGE('',*,*,#15368,.T.);
#22980=ORIENTED_EDGE('',*,*,#16236,.T.);
#22981=ORIENTED_EDGE('',*,*,#15070,.T.);
#22982=ORIENTED_EDGE('',*,*,#16235,.F.);
#22983=ORIENTED_EDGE('',*,*,#15367,.T.);
#22984=ORIENTED_EDGE('',*,*,#15484,.T.);
#22985=ORIENTED_EDGE('',*,*,#15721,.T.);
#22986=ORIENTED_EDGE('',*,*,#15949,.T.);
#22987=ORIENTED_EDGE('',*,*,#15071,.T.);
#22988=ORIENTED_EDGE('',*,*,#16236,.F.);
#22989=ORIENTED_EDGE('',*,*,#15373,.T.);
#22990=ORIENTED_EDGE('',*,*,#16237,.T.);
#22991=ORIENTED_EDGE('',*,*,#15065,.T.);
#22992=ORIENTED_EDGE('',*,*,#15946,.T.);
#22993=ORIENTED_EDGE('',*,*,#15716,.T.);
#22994=ORIENTED_EDGE('',*,*,#15479,.T.);
#22995=ORIENTED_EDGE('',*,*,#15372,.T.);
#22996=ORIENTED_EDGE('',*,*,#16238,.T.);
#22997=ORIENTED_EDGE('',*,*,#15066,.T.);
#22998=ORIENTED_EDGE('',*,*,#16237,.F.);
#22999=ORIENTED_EDGE('',*,*,#15371,.T.);
#23000=ORIENTED_EDGE('',*,*,#15481,.T.);
#23001=ORIENTED_EDGE('',*,*,#15718,.T.);
#23002=ORIENTED_EDGE('',*,*,#15947,.T.);
#23003=ORIENTED_EDGE('',*,*,#15067,.T.);
#23004=ORIENTED_EDGE('',*,*,#16238,.F.);
#23005=ORIENTED_EDGE('',*,*,#15377,.T.);
#23006=ORIENTED_EDGE('',*,*,#16239,.T.);
#23007=ORIENTED_EDGE('',*,*,#15061,.T.);
#23008=ORIENTED_EDGE('',*,*,#15944,.T.);
#23009=ORIENTED_EDGE('',*,*,#15713,.T.);
#23010=ORIENTED_EDGE('',*,*,#15476,.T.);
#23011=ORIENTED_EDGE('',*,*,#15376,.T.);
#23012=ORIENTED_EDGE('',*,*,#16240,.T.);
#23013=ORIENTED_EDGE('',*,*,#15062,.T.);
#23014=ORIENTED_EDGE('',*,*,#16239,.F.);
#23015=ORIENTED_EDGE('',*,*,#15375,.T.);
#23016=ORIENTED_EDGE('',*,*,#15478,.T.);
#23017=ORIENTED_EDGE('',*,*,#15715,.T.);
#23018=ORIENTED_EDGE('',*,*,#15945,.T.);
#23019=ORIENTED_EDGE('',*,*,#15063,.T.);
#23020=ORIENTED_EDGE('',*,*,#16240,.F.);
#23021=ORIENTED_EDGE('',*,*,#15380,.T.);
#23022=ORIENTED_EDGE('',*,*,#14784,.T.);
#23023=ORIENTED_EDGE('',*,*,#15058,.T.);
#23024=ORIENTED_EDGE('',*,*,#15942,.T.);
#23025=ORIENTED_EDGE('',*,*,#15710,.T.);
#23026=ORIENTED_EDGE('',*,*,#15473,.T.);
#23027=ORIENTED_EDGE('',*,*,#15379,.T.);
#23028=ORIENTED_EDGE('',*,*,#15475,.T.);
#23029=ORIENTED_EDGE('',*,*,#15712,.T.);
#23030=ORIENTED_EDGE('',*,*,#15943,.T.);
#23031=ORIENTED_EDGE('',*,*,#15059,.T.);
#23032=ORIENTED_EDGE('',*,*,#14782,.F.);
#23033=ORIENTED_EDGE('',*,*,#15383,.T.);
#23034=ORIENTED_EDGE('',*,*,#14780,.T.);
#23035=ORIENTED_EDGE('',*,*,#15055,.T.);
#23036=ORIENTED_EDGE('',*,*,#15940,.T.);
#23037=ORIENTED_EDGE('',*,*,#15707,.T.);
#23038=ORIENTED_EDGE('',*,*,#15470,.T.);
#23039=ORIENTED_EDGE('',*,*,#15382,.T.);
#23040=ORIENTED_EDGE('',*,*,#15472,.T.);
#23041=ORIENTED_EDGE('',*,*,#15709,.T.);
#23042=ORIENTED_EDGE('',*,*,#15941,.T.);
#23043=ORIENTED_EDGE('',*,*,#15056,.T.);
#23044=ORIENTED_EDGE('',*,*,#14778,.F.);
#23045=ORIENTED_EDGE('',*,*,#15386,.T.);
#23046=ORIENTED_EDGE('',*,*,#14776,.T.);
#23047=ORIENTED_EDGE('',*,*,#15052,.T.);
#23048=ORIENTED_EDGE('',*,*,#15938,.T.);
#23049=ORIENTED_EDGE('',*,*,#15704,.T.);
#23050=ORIENTED_EDGE('',*,*,#15467,.T.);
#23051=ORIENTED_EDGE('',*,*,#15385,.T.);
#23052=ORIENTED_EDGE('',*,*,#15469,.T.);
#23053=ORIENTED_EDGE('',*,*,#15706,.T.);
#23054=ORIENTED_EDGE('',*,*,#15939,.T.);
#23055=ORIENTED_EDGE('',*,*,#15053,.T.);
#23056=ORIENTED_EDGE('',*,*,#14774,.F.);
#23057=ORIENTED_EDGE('',*,*,#15389,.T.);
#23058=ORIENTED_EDGE('',*,*,#14772,.T.);
#23059=ORIENTED_EDGE('',*,*,#15049,.T.);
#23060=ORIENTED_EDGE('',*,*,#15936,.T.);
#23061=ORIENTED_EDGE('',*,*,#15701,.T.);
#23062=ORIENTED_EDGE('',*,*,#15464,.T.);
#23063=ORIENTED_EDGE('',*,*,#15388,.T.);
#23064=ORIENTED_EDGE('',*,*,#15466,.T.);
#23065=ORIENTED_EDGE('',*,*,#15703,.T.);
#23066=ORIENTED_EDGE('',*,*,#15937,.T.);
#23067=ORIENTED_EDGE('',*,*,#15050,.T.);
#23068=ORIENTED_EDGE('',*,*,#14770,.F.);
#23069=ORIENTED_EDGE('',*,*,#15392,.T.);
#23070=ORIENTED_EDGE('',*,*,#14768,.T.);
#23071=ORIENTED_EDGE('',*,*,#15046,.T.);
#23072=ORIENTED_EDGE('',*,*,#15934,.T.);
#23073=ORIENTED_EDGE('',*,*,#15698,.T.);
#23074=ORIENTED_EDGE('',*,*,#15461,.T.);
#23075=ORIENTED_EDGE('',*,*,#15391,.T.);
#23076=ORIENTED_EDGE('',*,*,#15463,.T.);
#23077=ORIENTED_EDGE('',*,*,#15700,.T.);
#23078=ORIENTED_EDGE('',*,*,#15935,.T.);
#23079=ORIENTED_EDGE('',*,*,#15047,.T.);
#23080=ORIENTED_EDGE('',*,*,#14766,.F.);
#23081=ORIENTED_EDGE('',*,*,#15395,.T.);
#23082=ORIENTED_EDGE('',*,*,#14764,.T.);
#23083=ORIENTED_EDGE('',*,*,#15043,.T.);
#23084=ORIENTED_EDGE('',*,*,#15931,.T.);
#23085=ORIENTED_EDGE('',*,*,#15694,.T.);
#23086=ORIENTED_EDGE('',*,*,#15457,.T.);
#23087=ORIENTED_EDGE('',*,*,#15394,.T.);
#23088=ORIENTED_EDGE('',*,*,#15460,.T.);
#23089=ORIENTED_EDGE('',*,*,#15697,.T.);
#23090=ORIENTED_EDGE('',*,*,#15933,.T.);
#23091=ORIENTED_EDGE('',*,*,#15044,.T.);
#23092=ORIENTED_EDGE('',*,*,#14762,.F.);
#23093=ORIENTED_EDGE('',*,*,#16241,.F.);
#23094=ORIENTED_EDGE('',*,*,#16242,.F.);
#23095=ORIENTED_EDGE('',*,*,#16243,.T.);
#23096=ORIENTED_EDGE('',*,*,#16244,.T.);
#23097=ORIENTED_EDGE('',*,*,#16243,.F.);
#23098=ORIENTED_EDGE('',*,*,#16245,.F.);
#23099=ORIENTED_EDGE('',*,*,#16246,.F.);
#23100=ORIENTED_EDGE('',*,*,#16247,.F.);
#23101=ORIENTED_EDGE('',*,*,#16248,.F.);
#23102=ORIENTED_EDGE('',*,*,#16241,.T.);
#23103=ORIENTED_EDGE('',*,*,#16249,.F.);
#23104=ORIENTED_EDGE('',*,*,#16250,.F.);
#23105=ORIENTED_EDGE('',*,*,#16251,.F.);
#23106=ORIENTED_EDGE('',*,*,#16247,.T.);
#23107=ORIENTED_EDGE('',*,*,#16252,.F.);
#23108=ORIENTED_EDGE('',*,*,#16253,.F.);
#23109=ORIENTED_EDGE('',*,*,#16254,.F.);
#23110=ORIENTED_EDGE('',*,*,#16250,.T.);
#23111=ORIENTED_EDGE('',*,*,#16255,.F.);
#23112=ORIENTED_EDGE('',*,*,#16256,.F.);
#23113=ORIENTED_EDGE('',*,*,#16257,.F.);
#23114=ORIENTED_EDGE('',*,*,#16253,.T.);
#23115=ORIENTED_EDGE('',*,*,#16258,.F.);
#23116=ORIENTED_EDGE('',*,*,#16259,.F.);
#23117=ORIENTED_EDGE('',*,*,#16260,.F.);
#23118=ORIENTED_EDGE('',*,*,#16256,.T.);
#23119=ORIENTED_EDGE('',*,*,#16261,.F.);
#23120=ORIENTED_EDGE('',*,*,#16262,.F.);
#23121=ORIENTED_EDGE('',*,*,#16263,.F.);
#23122=ORIENTED_EDGE('',*,*,#16259,.T.);
#23123=ORIENTED_EDGE('',*,*,#16264,.F.);
#23124=ORIENTED_EDGE('',*,*,#16265,.F.);
#23125=ORIENTED_EDGE('',*,*,#16266,.F.);
#23126=ORIENTED_EDGE('',*,*,#16262,.T.);
#23127=ORIENTED_EDGE('',*,*,#16267,.F.);
#23128=ORIENTED_EDGE('',*,*,#16268,.F.);
#23129=ORIENTED_EDGE('',*,*,#16269,.F.);
#23130=ORIENTED_EDGE('',*,*,#16265,.T.);
#23131=ORIENTED_EDGE('',*,*,#16270,.F.);
#23132=ORIENTED_EDGE('',*,*,#16271,.F.);
#23133=ORIENTED_EDGE('',*,*,#16272,.F.);
#23134=ORIENTED_EDGE('',*,*,#16268,.T.);
#23135=ORIENTED_EDGE('',*,*,#16273,.F.);
#23136=ORIENTED_EDGE('',*,*,#16274,.F.);
#23137=ORIENTED_EDGE('',*,*,#16275,.F.);
#23138=ORIENTED_EDGE('',*,*,#16271,.T.);
#23139=ORIENTED_EDGE('',*,*,#16276,.F.);
#23140=ORIENTED_EDGE('',*,*,#16277,.F.);
#23141=ORIENTED_EDGE('',*,*,#16278,.F.);
#23142=ORIENTED_EDGE('',*,*,#16274,.T.);
#23143=ORIENTED_EDGE('',*,*,#16279,.F.);
#23144=ORIENTED_EDGE('',*,*,#16280,.F.);
#23145=ORIENTED_EDGE('',*,*,#16281,.F.);
#23146=ORIENTED_EDGE('',*,*,#16277,.T.);
#23147=ORIENTED_EDGE('',*,*,#16282,.F.);
#23148=ORIENTED_EDGE('',*,*,#16283,.F.);
#23149=ORIENTED_EDGE('',*,*,#16284,.F.);
#23150=ORIENTED_EDGE('',*,*,#16280,.T.);
#23151=ORIENTED_EDGE('',*,*,#16285,.F.);
#23152=ORIENTED_EDGE('',*,*,#16286,.F.);
#23153=ORIENTED_EDGE('',*,*,#16287,.F.);
#23154=ORIENTED_EDGE('',*,*,#16283,.T.);
#23155=ORIENTED_EDGE('',*,*,#16288,.F.);
#23156=ORIENTED_EDGE('',*,*,#16289,.F.);
#23157=ORIENTED_EDGE('',*,*,#16290,.F.);
#23158=ORIENTED_EDGE('',*,*,#16286,.T.);
#23159=ORIENTED_EDGE('',*,*,#16291,.F.);
#23160=ORIENTED_EDGE('',*,*,#16292,.F.);
#23161=ORIENTED_EDGE('',*,*,#16293,.F.);
#23162=ORIENTED_EDGE('',*,*,#16289,.T.);
#23163=ORIENTED_EDGE('',*,*,#16294,.F.);
#23164=ORIENTED_EDGE('',*,*,#16295,.F.);
#23165=ORIENTED_EDGE('',*,*,#16296,.F.);
#23166=ORIENTED_EDGE('',*,*,#16292,.T.);
#23167=ORIENTED_EDGE('',*,*,#16297,.F.);
#23168=ORIENTED_EDGE('',*,*,#16298,.F.);
#23169=ORIENTED_EDGE('',*,*,#16299,.F.);
#23170=ORIENTED_EDGE('',*,*,#16295,.T.);
#23171=ORIENTED_EDGE('',*,*,#16300,.F.);
#23172=ORIENTED_EDGE('',*,*,#16301,.F.);
#23173=ORIENTED_EDGE('',*,*,#16302,.F.);
#23174=ORIENTED_EDGE('',*,*,#16298,.T.);
#23175=ORIENTED_EDGE('',*,*,#16303,.F.);
#23176=ORIENTED_EDGE('',*,*,#16304,.F.);
#23177=ORIENTED_EDGE('',*,*,#16305,.F.);
#23178=ORIENTED_EDGE('',*,*,#16301,.T.);
#23179=ORIENTED_EDGE('',*,*,#16306,.F.);
#23180=ORIENTED_EDGE('',*,*,#16307,.F.);
#23181=ORIENTED_EDGE('',*,*,#16308,.F.);
#23182=ORIENTED_EDGE('',*,*,#16304,.T.);
#23183=ORIENTED_EDGE('',*,*,#16309,.F.);
#23184=ORIENTED_EDGE('',*,*,#16310,.F.);
#23185=ORIENTED_EDGE('',*,*,#16311,.F.);
#23186=ORIENTED_EDGE('',*,*,#16307,.T.);
#23187=ORIENTED_EDGE('',*,*,#16312,.F.);
#23188=ORIENTED_EDGE('',*,*,#16313,.F.);
#23189=ORIENTED_EDGE('',*,*,#16314,.F.);
#23190=ORIENTED_EDGE('',*,*,#16310,.T.);
#23191=ORIENTED_EDGE('',*,*,#16315,.F.);
#23192=ORIENTED_EDGE('',*,*,#16316,.F.);
#23193=ORIENTED_EDGE('',*,*,#16317,.F.);
#23194=ORIENTED_EDGE('',*,*,#16313,.T.);
#23195=ORIENTED_EDGE('',*,*,#16318,.F.);
#23196=ORIENTED_EDGE('',*,*,#16319,.F.);
#23197=ORIENTED_EDGE('',*,*,#16320,.F.);
#23198=ORIENTED_EDGE('',*,*,#16316,.T.);
#23199=ORIENTED_EDGE('',*,*,#16321,.F.);
#23200=ORIENTED_EDGE('',*,*,#16322,.F.);
#23201=ORIENTED_EDGE('',*,*,#16323,.F.);
#23202=ORIENTED_EDGE('',*,*,#16319,.T.);
#23203=ORIENTED_EDGE('',*,*,#16324,.F.);
#23204=ORIENTED_EDGE('',*,*,#16325,.F.);
#23205=ORIENTED_EDGE('',*,*,#16326,.F.);
#23206=ORIENTED_EDGE('',*,*,#16322,.T.);
#23207=ORIENTED_EDGE('',*,*,#16327,.F.);
#23208=ORIENTED_EDGE('',*,*,#16328,.F.);
#23209=ORIENTED_EDGE('',*,*,#16329,.T.);
#23210=ORIENTED_EDGE('',*,*,#16330,.F.);
#23211=ORIENTED_EDGE('',*,*,#16331,.F.);
#23212=ORIENTED_EDGE('',*,*,#16332,.F.);
#23213=ORIENTED_EDGE('',*,*,#16333,.F.);
#23214=ORIENTED_EDGE('',*,*,#16334,.F.);
#23215=ORIENTED_EDGE('',*,*,#16335,.F.);
#23216=ORIENTED_EDGE('',*,*,#16331,.T.);
#23217=ORIENTED_EDGE('',*,*,#16336,.T.);
#23218=ORIENTED_EDGE('',*,*,#16337,.F.);
#23219=ORIENTED_EDGE('',*,*,#16338,.F.);
#23220=ORIENTED_EDGE('',*,*,#16334,.T.);
#23221=ORIENTED_EDGE('',*,*,#16339,.T.);
#23222=ORIENTED_EDGE('',*,*,#16340,.F.);
#23223=ORIENTED_EDGE('',*,*,#16341,.F.);
#23224=ORIENTED_EDGE('',*,*,#16337,.T.);
#23225=ORIENTED_EDGE('',*,*,#16342,.T.);
#23226=ORIENTED_EDGE('',*,*,#16343,.F.);
#23227=ORIENTED_EDGE('',*,*,#16344,.F.);
#23228=ORIENTED_EDGE('',*,*,#16340,.T.);
#23229=ORIENTED_EDGE('',*,*,#16345,.T.);
#23230=ORIENTED_EDGE('',*,*,#16346,.F.);
#23231=ORIENTED_EDGE('',*,*,#16347,.F.);
#23232=ORIENTED_EDGE('',*,*,#16343,.T.);
#23233=ORIENTED_EDGE('',*,*,#16348,.T.);
#23234=ORIENTED_EDGE('',*,*,#16349,.F.);
#23235=ORIENTED_EDGE('',*,*,#16350,.F.);
#23236=ORIENTED_EDGE('',*,*,#16346,.T.);
#23237=ORIENTED_EDGE('',*,*,#16351,.T.);
#23238=ORIENTED_EDGE('',*,*,#16352,.F.);
#23239=ORIENTED_EDGE('',*,*,#16353,.F.);
#23240=ORIENTED_EDGE('',*,*,#16349,.T.);
#23241=ORIENTED_EDGE('',*,*,#16354,.T.);
#23242=ORIENTED_EDGE('',*,*,#16355,.F.);
#23243=ORIENTED_EDGE('',*,*,#16356,.F.);
#23244=ORIENTED_EDGE('',*,*,#16352,.T.);
#23245=ORIENTED_EDGE('',*,*,#16357,.T.);
#23246=ORIENTED_EDGE('',*,*,#16358,.F.);
#23247=ORIENTED_EDGE('',*,*,#16359,.F.);
#23248=ORIENTED_EDGE('',*,*,#16355,.T.);
#23249=ORIENTED_EDGE('',*,*,#16360,.T.);
#23250=ORIENTED_EDGE('',*,*,#16361,.F.);
#23251=ORIENTED_EDGE('',*,*,#16362,.F.);
#23252=ORIENTED_EDGE('',*,*,#16358,.T.);
#23253=ORIENTED_EDGE('',*,*,#16363,.T.);
#23254=ORIENTED_EDGE('',*,*,#16364,.F.);
#23255=ORIENTED_EDGE('',*,*,#16365,.F.);
#23256=ORIENTED_EDGE('',*,*,#16361,.T.);
#23257=ORIENTED_EDGE('',*,*,#16366,.T.);
#23258=ORIENTED_EDGE('',*,*,#16367,.F.);
#23259=ORIENTED_EDGE('',*,*,#16368,.F.);
#23260=ORIENTED_EDGE('',*,*,#16364,.T.);
#23261=ORIENTED_EDGE('',*,*,#16369,.T.);
#23262=ORIENTED_EDGE('',*,*,#16370,.F.);
#23263=ORIENTED_EDGE('',*,*,#16371,.F.);
#23264=ORIENTED_EDGE('',*,*,#16367,.T.);
#23265=ORIENTED_EDGE('',*,*,#16372,.T.);
#23266=ORIENTED_EDGE('',*,*,#16373,.F.);
#23267=ORIENTED_EDGE('',*,*,#16374,.F.);
#23268=ORIENTED_EDGE('',*,*,#16370,.T.);
#23269=ORIENTED_EDGE('',*,*,#16375,.T.);
#23270=ORIENTED_EDGE('',*,*,#16376,.F.);
#23271=ORIENTED_EDGE('',*,*,#16377,.F.);
#23272=ORIENTED_EDGE('',*,*,#16373,.T.);
#23273=ORIENTED_EDGE('',*,*,#16378,.T.);
#23274=ORIENTED_EDGE('',*,*,#16379,.F.);
#23275=ORIENTED_EDGE('',*,*,#16380,.F.);
#23276=ORIENTED_EDGE('',*,*,#16376,.T.);
#23277=ORIENTED_EDGE('',*,*,#16381,.T.);
#23278=ORIENTED_EDGE('',*,*,#16382,.F.);
#23279=ORIENTED_EDGE('',*,*,#16383,.F.);
#23280=ORIENTED_EDGE('',*,*,#16379,.T.);
#23281=ORIENTED_EDGE('',*,*,#16384,.T.);
#23282=ORIENTED_EDGE('',*,*,#16385,.F.);
#23283=ORIENTED_EDGE('',*,*,#16386,.F.);
#23284=ORIENTED_EDGE('',*,*,#16382,.T.);
#23285=ORIENTED_EDGE('',*,*,#16387,.T.);
#23286=ORIENTED_EDGE('',*,*,#16388,.F.);
#23287=ORIENTED_EDGE('',*,*,#16389,.F.);
#23288=ORIENTED_EDGE('',*,*,#16385,.T.);
#23289=ORIENTED_EDGE('',*,*,#16390,.T.);
#23290=ORIENTED_EDGE('',*,*,#16391,.F.);
#23291=ORIENTED_EDGE('',*,*,#16392,.F.);
#23292=ORIENTED_EDGE('',*,*,#16388,.T.);
#23293=ORIENTED_EDGE('',*,*,#16393,.T.);
#23294=ORIENTED_EDGE('',*,*,#16394,.F.);
#23295=ORIENTED_EDGE('',*,*,#16395,.F.);
#23296=ORIENTED_EDGE('',*,*,#16391,.T.);
#23297=ORIENTED_EDGE('',*,*,#16396,.T.);
#23298=ORIENTED_EDGE('',*,*,#16397,.F.);
#23299=ORIENTED_EDGE('',*,*,#16398,.F.);
#23300=ORIENTED_EDGE('',*,*,#16394,.T.);
#23301=ORIENTED_EDGE('',*,*,#16399,.T.);
#23302=ORIENTED_EDGE('',*,*,#16400,.F.);
#23303=ORIENTED_EDGE('',*,*,#16401,.F.);
#23304=ORIENTED_EDGE('',*,*,#16397,.T.);
#23305=ORIENTED_EDGE('',*,*,#16402,.T.);
#23306=ORIENTED_EDGE('',*,*,#16403,.F.);
#23307=ORIENTED_EDGE('',*,*,#16404,.F.);
#23308=ORIENTED_EDGE('',*,*,#16400,.T.);
#23309=ORIENTED_EDGE('',*,*,#16405,.T.);
#23310=ORIENTED_EDGE('',*,*,#16406,.F.);
#23311=ORIENTED_EDGE('',*,*,#16407,.F.);
#23312=ORIENTED_EDGE('',*,*,#16403,.T.);
#23313=ORIENTED_EDGE('',*,*,#16408,.T.);
#23314=ORIENTED_EDGE('',*,*,#16409,.F.);
#23315=ORIENTED_EDGE('',*,*,#16410,.F.);
#23316=ORIENTED_EDGE('',*,*,#16406,.T.);
#23317=ORIENTED_EDGE('',*,*,#16411,.T.);
#23318=ORIENTED_EDGE('',*,*,#16412,.F.);
#23319=ORIENTED_EDGE('',*,*,#16413,.F.);
#23320=ORIENTED_EDGE('',*,*,#16409,.T.);
#23321=ORIENTED_EDGE('',*,*,#16414,.T.);
#23322=ORIENTED_EDGE('',*,*,#16415,.F.);
#23323=ORIENTED_EDGE('',*,*,#16416,.F.);
#23324=ORIENTED_EDGE('',*,*,#16412,.T.);
#23325=ORIENTED_EDGE('',*,*,#16417,.T.);
#23326=ORIENTED_EDGE('',*,*,#16418,.F.);
#23327=ORIENTED_EDGE('',*,*,#16419,.F.);
#23328=ORIENTED_EDGE('',*,*,#16415,.T.);
#23329=ORIENTED_EDGE('',*,*,#16420,.T.);
#23330=ORIENTED_EDGE('',*,*,#16418,.T.);
#23331=ORIENTED_EDGE('',*,*,#16421,.T.);
#23332=ORIENTED_EDGE('',*,*,#16422,.F.);
#23333=ORIENTED_EDGE('',*,*,#16328,.T.);
#23334=ORIENTED_EDGE('',*,*,#16423,.F.);
#23335=ORIENTED_EDGE('',*,*,#16424,.T.);
#23336=ORIENTED_EDGE('',*,*,#16425,.T.);
#23337=ORIENTED_EDGE('',*,*,#16426,.T.);
#23338=ORIENTED_EDGE('',*,*,#16325,.T.);
#23339=ORIENTED_EDGE('',*,*,#16427,.F.);
#23340=ORIENTED_EDGE('',*,*,#16425,.F.);
#23341=ORIENTED_EDGE('',*,*,#16428,.F.);
#23342=ORIENTED_EDGE('',*,*,#16429,.T.);
#23343=ORIENTED_EDGE('',*,*,#16430,.T.);
#23344=ORIENTED_EDGE('',*,*,#16431,.T.);
#23345=ORIENTED_EDGE('',*,*,#16432,.F.);
#23346=ORIENTED_EDGE('',*,*,#16433,.T.);
#23347=ORIENTED_EDGE('',*,*,#16434,.T.);
#23348=ORIENTED_EDGE('',*,*,#16435,.T.);
#23349=ORIENTED_EDGE('',*,*,#16436,.F.);
#23350=ORIENTED_EDGE('',*,*,#16437,.T.);
#23351=ORIENTED_EDGE('',*,*,#16438,.T.);
#23352=ORIENTED_EDGE('',*,*,#16439,.T.);
#23353=ORIENTED_EDGE('',*,*,#16440,.F.);
#23354=ORIENTED_EDGE('',*,*,#16441,.T.);
#23355=ORIENTED_EDGE('',*,*,#16442,.T.);
#23356=ORIENTED_EDGE('',*,*,#16443,.T.);
#23357=ORIENTED_EDGE('',*,*,#16444,.F.);
#23358=ORIENTED_EDGE('',*,*,#16445,.T.);
#23359=ORIENTED_EDGE('',*,*,#16446,.T.);
#23360=ORIENTED_EDGE('',*,*,#16447,.T.);
#23361=ORIENTED_EDGE('',*,*,#16448,.F.);
#23362=ORIENTED_EDGE('',*,*,#16449,.T.);
#23363=ORIENTED_EDGE('',*,*,#16450,.T.);
#23364=ORIENTED_EDGE('',*,*,#16451,.T.);
#23365=ORIENTED_EDGE('',*,*,#16452,.F.);
#23366=ORIENTED_EDGE('',*,*,#16453,.T.);
#23367=ORIENTED_EDGE('',*,*,#16454,.T.);
#23368=ORIENTED_EDGE('',*,*,#16455,.T.);
#23369=ORIENTED_EDGE('',*,*,#16456,.F.);
#23370=ORIENTED_EDGE('',*,*,#16457,.T.);
#23371=ORIENTED_EDGE('',*,*,#16458,.T.);
#23372=ORIENTED_EDGE('',*,*,#16459,.T.);
#23373=ORIENTED_EDGE('',*,*,#16460,.F.);
#23374=ORIENTED_EDGE('',*,*,#16461,.T.);
#23375=ORIENTED_EDGE('',*,*,#16462,.T.);
#23376=ORIENTED_EDGE('',*,*,#16463,.T.);
#23377=ORIENTED_EDGE('',*,*,#16464,.F.);
#23378=ORIENTED_EDGE('',*,*,#16465,.T.);
#23379=ORIENTED_EDGE('',*,*,#16466,.T.);
#23380=ORIENTED_EDGE('',*,*,#16467,.T.);
#23381=ORIENTED_EDGE('',*,*,#16468,.F.);
#23382=ORIENTED_EDGE('',*,*,#16469,.T.);
#23383=ORIENTED_EDGE('',*,*,#16470,.T.);
#23384=ORIENTED_EDGE('',*,*,#16471,.T.);
#23385=ORIENTED_EDGE('',*,*,#16472,.F.);
#23386=ORIENTED_EDGE('',*,*,#16473,.T.);
#23387=ORIENTED_EDGE('',*,*,#16474,.T.);
#23388=ORIENTED_EDGE('',*,*,#16475,.T.);
#23389=ORIENTED_EDGE('',*,*,#16476,.F.);
#23390=ORIENTED_EDGE('',*,*,#16477,.T.);
#23391=ORIENTED_EDGE('',*,*,#16478,.T.);
#23392=ORIENTED_EDGE('',*,*,#16479,.T.);
#23393=ORIENTED_EDGE('',*,*,#16480,.F.);
#23394=ORIENTED_EDGE('',*,*,#16481,.T.);
#23395=ORIENTED_EDGE('',*,*,#16482,.T.);
#23396=ORIENTED_EDGE('',*,*,#16483,.T.);
#23397=ORIENTED_EDGE('',*,*,#16484,.F.);
#23398=ORIENTED_EDGE('',*,*,#16485,.T.);
#23399=ORIENTED_EDGE('',*,*,#16486,.T.);
#23400=ORIENTED_EDGE('',*,*,#16487,.T.);
#23401=ORIENTED_EDGE('',*,*,#16488,.F.);
#23402=ORIENTED_EDGE('',*,*,#16489,.F.);
#23403=ORIENTED_EDGE('',*,*,#16490,.F.);
#23404=ORIENTED_EDGE('',*,*,#16491,.F.);
#23405=ORIENTED_EDGE('',*,*,#16492,.F.);
#23406=ORIENTED_EDGE('',*,*,#16493,.F.);
#23407=ORIENTED_EDGE('',*,*,#16494,.F.);
#23408=ORIENTED_EDGE('',*,*,#16495,.F.);
#23409=ORIENTED_EDGE('',*,*,#16496,.T.);
#23410=ORIENTED_EDGE('',*,*,#16497,.T.);
#23411=ORIENTED_EDGE('',*,*,#16496,.F.);
#23412=ORIENTED_EDGE('',*,*,#16498,.F.);
#23413=ORIENTED_EDGE('',*,*,#16499,.T.);
#23414=ORIENTED_EDGE('',*,*,#16500,.T.);
#23415=ORIENTED_EDGE('',*,*,#16499,.F.);
#23416=ORIENTED_EDGE('',*,*,#16501,.F.);
#23417=ORIENTED_EDGE('',*,*,#16502,.F.);
#23418=ORIENTED_EDGE('',*,*,#16503,.F.);
#23419=ORIENTED_EDGE('',*,*,#16504,.F.);
#23420=ORIENTED_EDGE('',*,*,#16505,.F.);
#23421=ORIENTED_EDGE('',*,*,#16506,.F.);
#23422=ORIENTED_EDGE('',*,*,#16507,.F.);
#23423=ORIENTED_EDGE('',*,*,#16508,.F.);
#23424=ORIENTED_EDGE('',*,*,#16509,.F.);
#23425=ORIENTED_EDGE('',*,*,#16510,.F.);
#23426=ORIENTED_EDGE('',*,*,#16511,.F.);
#23427=ORIENTED_EDGE('',*,*,#16512,.F.);
#23428=ORIENTED_EDGE('',*,*,#16513,.F.);
#23429=ORIENTED_EDGE('',*,*,#16514,.F.);
#23430=ORIENTED_EDGE('',*,*,#16515,.F.);
#23431=ORIENTED_EDGE('',*,*,#16516,.F.);
#23432=ORIENTED_EDGE('',*,*,#16517,.F.);
#23433=ORIENTED_EDGE('',*,*,#16518,.F.);
#23434=ORIENTED_EDGE('',*,*,#16519,.F.);
#23435=ORIENTED_EDGE('',*,*,#16520,.F.);
#23436=ORIENTED_EDGE('',*,*,#16521,.F.);
#23437=ORIENTED_EDGE('',*,*,#16522,.F.);
#23438=ORIENTED_EDGE('',*,*,#16523,.F.);
#23439=ORIENTED_EDGE('',*,*,#16524,.F.);
#23440=ORIENTED_EDGE('',*,*,#16525,.F.);
#23441=ORIENTED_EDGE('',*,*,#16526,.F.);
#23442=ORIENTED_EDGE('',*,*,#16527,.F.);
#23443=ORIENTED_EDGE('',*,*,#16528,.F.);
#23444=ORIENTED_EDGE('',*,*,#16529,.F.);
#23445=ORIENTED_EDGE('',*,*,#16530,.F.);
#23446=ORIENTED_EDGE('',*,*,#16531,.F.);
#23447=ORIENTED_EDGE('',*,*,#16532,.F.);
#23448=ORIENTED_EDGE('',*,*,#16533,.F.);
#23449=ORIENTED_EDGE('',*,*,#16534,.F.);
#23450=ORIENTED_EDGE('',*,*,#16535,.F.);
#23451=ORIENTED_EDGE('',*,*,#16536,.F.);
#23452=ORIENTED_EDGE('',*,*,#16537,.F.);
#23453=ORIENTED_EDGE('',*,*,#16538,.F.);
#23454=ORIENTED_EDGE('',*,*,#16539,.F.);
#23455=ORIENTED_EDGE('',*,*,#16540,.F.);
#23456=ORIENTED_EDGE('',*,*,#16541,.F.);
#23457=ORIENTED_EDGE('',*,*,#16542,.F.);
#23458=ORIENTED_EDGE('',*,*,#16543,.F.);
#23459=ORIENTED_EDGE('',*,*,#16544,.F.);
#23460=ORIENTED_EDGE('',*,*,#16545,.F.);
#23461=ORIENTED_EDGE('',*,*,#16546,.F.);
#23462=ORIENTED_EDGE('',*,*,#16547,.F.);
#23463=ORIENTED_EDGE('',*,*,#16548,.F.);
#23464=ORIENTED_EDGE('',*,*,#16549,.F.);
#23465=ORIENTED_EDGE('',*,*,#16550,.F.);
#23466=ORIENTED_EDGE('',*,*,#16551,.F.);
#23467=ORIENTED_EDGE('',*,*,#16552,.F.);
#23468=ORIENTED_EDGE('',*,*,#16553,.F.);
#23469=ORIENTED_EDGE('',*,*,#16554,.F.);
#23470=ORIENTED_EDGE('',*,*,#16555,.F.);
#23471=ORIENTED_EDGE('',*,*,#16556,.F.);
#23472=ORIENTED_EDGE('',*,*,#16557,.F.);
#23473=ORIENTED_EDGE('',*,*,#16558,.F.);
#23474=ORIENTED_EDGE('',*,*,#16559,.F.);
#23475=ORIENTED_EDGE('',*,*,#16560,.F.);
#23476=ORIENTED_EDGE('',*,*,#16561,.F.);
#23477=ORIENTED_EDGE('',*,*,#16562,.F.);
#23478=ORIENTED_EDGE('',*,*,#16563,.F.);
#23479=ORIENTED_EDGE('',*,*,#16564,.F.);
#23480=ORIENTED_EDGE('',*,*,#16565,.F.);
#23481=ORIENTED_EDGE('',*,*,#16566,.F.);
#23482=ORIENTED_EDGE('',*,*,#16567,.F.);
#23483=ORIENTED_EDGE('',*,*,#16568,.F.);
#23484=ORIENTED_EDGE('',*,*,#16569,.F.);
#23485=ORIENTED_EDGE('',*,*,#16570,.F.);
#23486=ORIENTED_EDGE('',*,*,#16571,.F.);
#23487=ORIENTED_EDGE('',*,*,#16572,.F.);
#23488=ORIENTED_EDGE('',*,*,#16573,.F.);
#23489=ORIENTED_EDGE('',*,*,#16574,.F.);
#23490=ORIENTED_EDGE('',*,*,#16575,.F.);
#23491=ORIENTED_EDGE('',*,*,#16576,.F.);
#23492=ORIENTED_EDGE('',*,*,#16577,.F.);
#23493=ORIENTED_EDGE('',*,*,#16578,.F.);
#23494=ORIENTED_EDGE('',*,*,#16579,.F.);
#23495=ORIENTED_EDGE('',*,*,#16580,.F.);
#23496=ORIENTED_EDGE('',*,*,#16581,.F.);
#23497=ORIENTED_EDGE('',*,*,#16582,.F.);
#23498=ORIENTED_EDGE('',*,*,#16583,.F.);
#23499=ORIENTED_EDGE('',*,*,#16584,.F.);
#23500=ORIENTED_EDGE('',*,*,#16585,.F.);
#23501=ORIENTED_EDGE('',*,*,#16586,.F.);
#23502=ORIENTED_EDGE('',*,*,#16587,.F.);
#23503=ORIENTED_EDGE('',*,*,#16588,.F.);
#23504=ORIENTED_EDGE('',*,*,#16589,.F.);
#23505=ORIENTED_EDGE('',*,*,#16590,.F.);
#23506=ORIENTED_EDGE('',*,*,#16591,.F.);
#23507=ORIENTED_EDGE('',*,*,#16592,.F.);
#23508=ORIENTED_EDGE('',*,*,#16593,.F.);
#23509=ORIENTED_EDGE('',*,*,#16594,.F.);
#23510=ORIENTED_EDGE('',*,*,#16595,.F.);
#23511=ORIENTED_EDGE('',*,*,#16596,.F.);
#23512=ORIENTED_EDGE('',*,*,#16597,.F.);
#23513=ORIENTED_EDGE('',*,*,#16598,.F.);
#23514=ORIENTED_EDGE('',*,*,#16599,.F.);
#23515=ORIENTED_EDGE('',*,*,#16600,.F.);
#23516=ORIENTED_EDGE('',*,*,#16601,.F.);
#23517=ORIENTED_EDGE('',*,*,#16602,.F.);
#23518=ORIENTED_EDGE('',*,*,#16603,.F.);
#23519=ORIENTED_EDGE('',*,*,#16604,.F.);
#23520=ORIENTED_EDGE('',*,*,#16605,.F.);
#23521=ORIENTED_EDGE('',*,*,#16606,.F.);
#23522=ORIENTED_EDGE('',*,*,#16607,.F.);
#23523=ORIENTED_EDGE('',*,*,#16608,.F.);
#23524=ORIENTED_EDGE('',*,*,#16609,.F.);
#23525=ORIENTED_EDGE('',*,*,#16610,.F.);
#23526=ORIENTED_EDGE('',*,*,#16611,.F.);
#23527=ORIENTED_EDGE('',*,*,#16612,.F.);
#23528=ORIENTED_EDGE('',*,*,#16613,.F.);
#23529=ORIENTED_EDGE('',*,*,#16614,.F.);
#23530=ORIENTED_EDGE('',*,*,#16615,.F.);
#23531=ORIENTED_EDGE('',*,*,#16616,.F.);
#23532=ORIENTED_EDGE('',*,*,#16617,.F.);
#23533=ORIENTED_EDGE('',*,*,#16618,.F.);
#23534=ORIENTED_EDGE('',*,*,#16619,.F.);
#23535=ORIENTED_EDGE('',*,*,#16620,.F.);
#23536=ORIENTED_EDGE('',*,*,#16621,.F.);
#23537=ORIENTED_EDGE('',*,*,#16622,.F.);
#23538=ORIENTED_EDGE('',*,*,#16623,.F.);
#23539=ORIENTED_EDGE('',*,*,#16624,.F.);
#23540=ORIENTED_EDGE('',*,*,#16625,.F.);
#23541=ORIENTED_EDGE('',*,*,#16626,.F.);
#23542=ORIENTED_EDGE('',*,*,#16627,.F.);
#23543=ORIENTED_EDGE('',*,*,#16628,.F.);
#23544=ORIENTED_EDGE('',*,*,#16629,.F.);
#23545=ORIENTED_EDGE('',*,*,#16630,.F.);
#23546=ORIENTED_EDGE('',*,*,#16631,.F.);
#23547=ORIENTED_EDGE('',*,*,#16632,.F.);
#23548=ORIENTED_EDGE('',*,*,#16633,.F.);
#23549=ORIENTED_EDGE('',*,*,#16634,.F.);
#23550=ORIENTED_EDGE('',*,*,#16635,.F.);
#23551=ORIENTED_EDGE('',*,*,#16636,.F.);
#23552=ORIENTED_EDGE('',*,*,#16637,.F.);
#23553=ORIENTED_EDGE('',*,*,#16638,.F.);
#23554=ORIENTED_EDGE('',*,*,#16639,.F.);
#23555=ORIENTED_EDGE('',*,*,#16640,.F.);
#23556=ORIENTED_EDGE('',*,*,#16641,.F.);
#23557=ORIENTED_EDGE('',*,*,#16642,.F.);
#23558=ORIENTED_EDGE('',*,*,#16643,.F.);
#23559=ORIENTED_EDGE('',*,*,#16644,.F.);
#23560=ORIENTED_EDGE('',*,*,#16645,.F.);
#23561=ORIENTED_EDGE('',*,*,#16646,.F.);
#23562=ORIENTED_EDGE('',*,*,#16647,.F.);
#23563=ORIENTED_EDGE('',*,*,#16648,.F.);
#23564=ORIENTED_EDGE('',*,*,#16649,.F.);
#23565=ORIENTED_EDGE('',*,*,#16650,.F.);
#23566=ORIENTED_EDGE('',*,*,#16651,.F.);
#23567=ORIENTED_EDGE('',*,*,#16652,.F.);
#23568=ORIENTED_EDGE('',*,*,#16653,.F.);
#23569=ORIENTED_EDGE('',*,*,#16654,.F.);
#23570=ORIENTED_EDGE('',*,*,#16655,.F.);
#23571=ORIENTED_EDGE('',*,*,#16656,.F.);
#23572=ORIENTED_EDGE('',*,*,#16657,.F.);
#23573=ORIENTED_EDGE('',*,*,#16658,.F.);
#23574=ORIENTED_EDGE('',*,*,#16659,.F.);
#23575=ORIENTED_EDGE('',*,*,#16660,.F.);
#23576=ORIENTED_EDGE('',*,*,#16661,.F.);
#23577=ORIENTED_EDGE('',*,*,#16662,.F.);
#23578=ORIENTED_EDGE('',*,*,#16663,.F.);
#23579=ORIENTED_EDGE('',*,*,#16664,.F.);
#23580=ORIENTED_EDGE('',*,*,#16665,.F.);
#23581=ORIENTED_EDGE('',*,*,#16666,.F.);
#23582=ORIENTED_EDGE('',*,*,#16667,.F.);
#23583=ORIENTED_EDGE('',*,*,#16668,.F.);
#23584=ORIENTED_EDGE('',*,*,#16669,.F.);
#23585=ORIENTED_EDGE('',*,*,#16670,.F.);
#23586=ORIENTED_EDGE('',*,*,#16671,.F.);
#23587=ORIENTED_EDGE('',*,*,#16672,.F.);
#23588=ORIENTED_EDGE('',*,*,#16673,.F.);
#23589=ORIENTED_EDGE('',*,*,#16674,.F.);
#23590=ORIENTED_EDGE('',*,*,#16675,.F.);
#23591=ORIENTED_EDGE('',*,*,#16676,.F.);
#23592=ORIENTED_EDGE('',*,*,#16677,.F.);
#23593=ORIENTED_EDGE('',*,*,#16678,.F.);
#23594=ORIENTED_EDGE('',*,*,#16679,.F.);
#23595=ORIENTED_EDGE('',*,*,#16680,.F.);
#23596=ORIENTED_EDGE('',*,*,#16681,.F.);
#23597=ORIENTED_EDGE('',*,*,#16682,.F.);
#23598=ORIENTED_EDGE('',*,*,#16683,.F.);
#23599=ORIENTED_EDGE('',*,*,#16684,.F.);
#23600=ORIENTED_EDGE('',*,*,#16487,.F.);
#23601=ORIENTED_EDGE('',*,*,#16685,.F.);
#23602=ORIENTED_EDGE('',*,*,#16686,.F.);
#23603=ORIENTED_EDGE('',*,*,#16687,.F.);
#23604=ORIENTED_EDGE('',*,*,#16483,.F.);
#23605=ORIENTED_EDGE('',*,*,#16688,.F.);
#23606=ORIENTED_EDGE('',*,*,#16689,.F.);
#23607=ORIENTED_EDGE('',*,*,#16690,.F.);
#23608=ORIENTED_EDGE('',*,*,#16479,.F.);
#23609=ORIENTED_EDGE('',*,*,#16691,.F.);
#23610=ORIENTED_EDGE('',*,*,#16692,.F.);
#23611=ORIENTED_EDGE('',*,*,#16693,.F.);
#23612=ORIENTED_EDGE('',*,*,#16475,.F.);
#23613=ORIENTED_EDGE('',*,*,#16694,.F.);
#23614=ORIENTED_EDGE('',*,*,#16695,.F.);
#23615=ORIENTED_EDGE('',*,*,#16696,.F.);
#23616=ORIENTED_EDGE('',*,*,#16471,.F.);
#23617=ORIENTED_EDGE('',*,*,#16697,.F.);
#23618=ORIENTED_EDGE('',*,*,#16698,.F.);
#23619=ORIENTED_EDGE('',*,*,#16699,.F.);
#23620=ORIENTED_EDGE('',*,*,#16467,.F.);
#23621=ORIENTED_EDGE('',*,*,#16700,.F.);
#23622=ORIENTED_EDGE('',*,*,#16701,.F.);
#23623=ORIENTED_EDGE('',*,*,#16702,.F.);
#23624=ORIENTED_EDGE('',*,*,#16463,.F.);
#23625=ORIENTED_EDGE('',*,*,#16703,.F.);
#23626=ORIENTED_EDGE('',*,*,#16704,.F.);
#23627=ORIENTED_EDGE('',*,*,#16705,.F.);
#23628=ORIENTED_EDGE('',*,*,#16459,.F.);
#23629=ORIENTED_EDGE('',*,*,#16706,.F.);
#23630=ORIENTED_EDGE('',*,*,#16707,.F.);
#23631=ORIENTED_EDGE('',*,*,#16708,.F.);
#23632=ORIENTED_EDGE('',*,*,#16455,.F.);
#23633=ORIENTED_EDGE('',*,*,#16709,.F.);
#23634=ORIENTED_EDGE('',*,*,#16710,.F.);
#23635=ORIENTED_EDGE('',*,*,#16711,.F.);
#23636=ORIENTED_EDGE('',*,*,#16431,.F.);
#23637=ORIENTED_EDGE('',*,*,#16712,.F.);
#23638=ORIENTED_EDGE('',*,*,#16713,.F.);
#23639=ORIENTED_EDGE('',*,*,#16714,.F.);
#23640=ORIENTED_EDGE('',*,*,#16435,.F.);
#23641=ORIENTED_EDGE('',*,*,#16715,.F.);
#23642=ORIENTED_EDGE('',*,*,#16716,.F.);
#23643=ORIENTED_EDGE('',*,*,#16717,.F.);
#23644=ORIENTED_EDGE('',*,*,#16439,.F.);
#23645=ORIENTED_EDGE('',*,*,#16718,.F.);
#23646=ORIENTED_EDGE('',*,*,#16719,.F.);
#23647=ORIENTED_EDGE('',*,*,#16720,.F.);
#23648=ORIENTED_EDGE('',*,*,#16443,.F.);
#23649=ORIENTED_EDGE('',*,*,#16721,.F.);
#23650=ORIENTED_EDGE('',*,*,#16722,.F.);
#23651=ORIENTED_EDGE('',*,*,#16723,.F.);
#23652=ORIENTED_EDGE('',*,*,#16447,.F.);
#23653=ORIENTED_EDGE('',*,*,#16724,.F.);
#23654=ORIENTED_EDGE('',*,*,#16725,.F.);
#23655=ORIENTED_EDGE('',*,*,#16726,.F.);
#23656=ORIENTED_EDGE('',*,*,#16451,.F.);
#23657=ORIENTED_EDGE('',*,*,#16727,.F.);
#23658=ORIENTED_EDGE('',*,*,#16728,.F.);
#23659=ORIENTED_EDGE('',*,*,#16729,.F.);
#23660=ORIENTED_EDGE('',*,*,#16730,.F.);
#23661=ORIENTED_EDGE('',*,*,#16731,.F.);
#23662=ORIENTED_EDGE('',*,*,#16732,.F.);
#23663=ORIENTED_EDGE('',*,*,#16733,.F.);
#23664=ORIENTED_EDGE('',*,*,#16734,.F.);
#23665=ORIENTED_EDGE('',*,*,#16735,.F.);
#23666=ORIENTED_EDGE('',*,*,#16736,.F.);
#23667=ORIENTED_EDGE('',*,*,#16737,.F.);
#23668=ORIENTED_EDGE('',*,*,#16738,.F.);
#23669=ORIENTED_EDGE('',*,*,#16739,.F.);
#23670=ORIENTED_EDGE('',*,*,#16740,.F.);
#23671=ORIENTED_EDGE('',*,*,#16741,.F.);
#23672=ORIENTED_EDGE('',*,*,#16742,.F.);
#23673=ORIENTED_EDGE('',*,*,#16743,.F.);
#23674=ORIENTED_EDGE('',*,*,#16744,.F.);
#23675=ORIENTED_EDGE('',*,*,#16745,.F.);
#23676=ORIENTED_EDGE('',*,*,#16746,.F.);
#23677=ORIENTED_EDGE('',*,*,#16747,.F.);
#23678=ORIENTED_EDGE('',*,*,#16748,.F.);
#23679=ORIENTED_EDGE('',*,*,#16749,.F.);
#23680=ORIENTED_EDGE('',*,*,#16750,.F.);
#23681=ORIENTED_EDGE('',*,*,#16751,.F.);
#23682=ORIENTED_EDGE('',*,*,#16752,.F.);
#23683=ORIENTED_EDGE('',*,*,#16753,.F.);
#23684=ORIENTED_EDGE('',*,*,#16754,.F.);
#23685=ORIENTED_EDGE('',*,*,#16755,.F.);
#23686=ORIENTED_EDGE('',*,*,#16756,.F.);
#23687=ORIENTED_EDGE('',*,*,#16757,.F.);
#23688=ORIENTED_EDGE('',*,*,#16758,.F.);
#23689=ORIENTED_EDGE('',*,*,#16759,.F.);
#23690=ORIENTED_EDGE('',*,*,#16760,.F.);
#23691=ORIENTED_EDGE('',*,*,#16761,.F.);
#23692=ORIENTED_EDGE('',*,*,#16762,.F.);
#23693=ORIENTED_EDGE('',*,*,#16763,.F.);
#23694=ORIENTED_EDGE('',*,*,#16764,.F.);
#23695=ORIENTED_EDGE('',*,*,#16765,.F.);
#23696=ORIENTED_EDGE('',*,*,#16766,.F.);
#23697=ORIENTED_EDGE('',*,*,#16767,.F.);
#23698=ORIENTED_EDGE('',*,*,#16768,.F.);
#23699=ORIENTED_EDGE('',*,*,#16769,.F.);
#23700=ORIENTED_EDGE('',*,*,#16770,.F.);
#23701=ORIENTED_EDGE('',*,*,#16771,.F.);
#23702=ORIENTED_EDGE('',*,*,#16772,.F.);
#23703=ORIENTED_EDGE('',*,*,#16773,.F.);
#23704=ORIENTED_EDGE('',*,*,#16774,.F.);
#23705=ORIENTED_EDGE('',*,*,#16775,.F.);
#23706=ORIENTED_EDGE('',*,*,#16776,.F.);
#23707=ORIENTED_EDGE('',*,*,#16777,.F.);
#23708=ORIENTED_EDGE('',*,*,#16778,.F.);
#23709=ORIENTED_EDGE('',*,*,#16779,.F.);
#23710=ORIENTED_EDGE('',*,*,#16780,.F.);
#23711=ORIENTED_EDGE('',*,*,#16781,.F.);
#23712=ORIENTED_EDGE('',*,*,#16782,.F.);
#23713=ORIENTED_EDGE('',*,*,#16783,.F.);
#23714=ORIENTED_EDGE('',*,*,#16784,.F.);
#23715=ORIENTED_EDGE('',*,*,#16785,.F.);
#23716=ORIENTED_EDGE('',*,*,#16786,.F.);
#23717=ORIENTED_EDGE('',*,*,#16787,.F.);
#23718=ORIENTED_EDGE('',*,*,#16788,.F.);
#23719=ORIENTED_EDGE('',*,*,#16789,.F.);
#23720=ORIENTED_EDGE('',*,*,#16790,.F.);
#23721=ORIENTED_EDGE('',*,*,#16791,.F.);
#23722=ORIENTED_EDGE('',*,*,#16792,.F.);
#23723=ORIENTED_EDGE('',*,*,#16793,.F.);
#23724=ORIENTED_EDGE('',*,*,#16794,.F.);
#23725=ORIENTED_EDGE('',*,*,#16795,.F.);
#23726=ORIENTED_EDGE('',*,*,#16796,.F.);
#23727=ORIENTED_EDGE('',*,*,#16797,.F.);
#23728=ORIENTED_EDGE('',*,*,#16798,.F.);
#23729=ORIENTED_EDGE('',*,*,#16799,.F.);
#23730=ORIENTED_EDGE('',*,*,#16800,.F.);
#23731=ORIENTED_EDGE('',*,*,#16801,.F.);
#23732=ORIENTED_EDGE('',*,*,#16802,.F.);
#23733=ORIENTED_EDGE('',*,*,#16803,.F.);
#23734=ORIENTED_EDGE('',*,*,#16804,.F.);
#23735=ORIENTED_EDGE('',*,*,#16805,.F.);
#23736=ORIENTED_EDGE('',*,*,#16806,.F.);
#23737=ORIENTED_EDGE('',*,*,#16807,.T.);
#23738=ORIENTED_EDGE('',*,*,#16498,.T.);
#23739=ORIENTED_EDGE('',*,*,#16807,.F.);
#23740=ORIENTED_EDGE('',*,*,#16808,.F.);
#23741=ORIENTED_EDGE('',*,*,#16809,.F.);
#23742=ORIENTED_EDGE('',*,*,#16810,.T.);
#23743=ORIENTED_EDGE('',*,*,#16811,.F.);
#23744=ORIENTED_EDGE('',*,*,#16812,.F.);
#23745=ORIENTED_EDGE('',*,*,#16813,.F.);
#23746=ORIENTED_EDGE('',*,*,#16814,.T.);
#23747=ORIENTED_EDGE('',*,*,#16815,.F.);
#23748=ORIENTED_EDGE('',*,*,#16816,.F.);
#23749=ORIENTED_EDGE('',*,*,#16817,.F.);
#23750=ORIENTED_EDGE('',*,*,#16818,.T.);
#23751=ORIENTED_EDGE('',*,*,#16819,.F.);
#23752=ORIENTED_EDGE('',*,*,#16820,.F.);
#23753=ORIENTED_EDGE('',*,*,#16821,.F.);
#23754=ORIENTED_EDGE('',*,*,#16822,.T.);
#23755=ORIENTED_EDGE('',*,*,#16823,.F.);
#23756=ORIENTED_EDGE('',*,*,#16824,.F.);
#23757=ORIENTED_EDGE('',*,*,#16825,.F.);
#23758=ORIENTED_EDGE('',*,*,#16826,.T.);
#23759=ORIENTED_EDGE('',*,*,#16827,.F.);
#23760=ORIENTED_EDGE('',*,*,#16828,.F.);
#23761=ORIENTED_EDGE('',*,*,#16829,.F.);
#23762=ORIENTED_EDGE('',*,*,#16830,.T.);
#23763=ORIENTED_EDGE('',*,*,#16831,.F.);
#23764=ORIENTED_EDGE('',*,*,#16832,.F.);
#23765=ORIENTED_EDGE('',*,*,#16833,.F.);
#23766=ORIENTED_EDGE('',*,*,#16834,.T.);
#23767=ORIENTED_EDGE('',*,*,#16835,.F.);
#23768=ORIENTED_EDGE('',*,*,#16836,.F.);
#23769=ORIENTED_EDGE('',*,*,#16837,.F.);
#23770=ORIENTED_EDGE('',*,*,#16838,.T.);
#23771=ORIENTED_EDGE('',*,*,#16839,.F.);
#23772=ORIENTED_EDGE('',*,*,#16840,.F.);
#23773=ORIENTED_EDGE('',*,*,#16841,.F.);
#23774=ORIENTED_EDGE('',*,*,#16842,.T.);
#23775=ORIENTED_EDGE('',*,*,#16843,.F.);
#23776=ORIENTED_EDGE('',*,*,#16844,.F.);
#23777=ORIENTED_EDGE('',*,*,#16845,.F.);
#23778=ORIENTED_EDGE('',*,*,#16846,.T.);
#23779=ORIENTED_EDGE('',*,*,#16847,.F.);
#23780=ORIENTED_EDGE('',*,*,#16848,.F.);
#23781=ORIENTED_EDGE('',*,*,#16849,.F.);
#23782=ORIENTED_EDGE('',*,*,#16850,.T.);
#23783=ORIENTED_EDGE('',*,*,#16851,.F.);
#23784=ORIENTED_EDGE('',*,*,#16852,.F.);
#23785=ORIENTED_EDGE('',*,*,#16853,.F.);
#23786=ORIENTED_EDGE('',*,*,#16854,.T.);
#23787=ORIENTED_EDGE('',*,*,#16855,.F.);
#23788=ORIENTED_EDGE('',*,*,#16856,.F.);
#23789=ORIENTED_EDGE('',*,*,#16857,.F.);
#23790=ORIENTED_EDGE('',*,*,#16858,.T.);
#23791=ORIENTED_EDGE('',*,*,#16859,.F.);
#23792=ORIENTED_EDGE('',*,*,#16860,.F.);
#23793=ORIENTED_EDGE('',*,*,#16861,.F.);
#23794=ORIENTED_EDGE('',*,*,#16862,.T.);
#23795=ORIENTED_EDGE('',*,*,#16863,.F.);
#23796=ORIENTED_EDGE('',*,*,#16864,.F.);
#23797=ORIENTED_EDGE('',*,*,#16865,.F.);
#23798=ORIENTED_EDGE('',*,*,#16866,.T.);
#23799=ORIENTED_EDGE('',*,*,#16867,.F.);
#23800=ORIENTED_EDGE('',*,*,#16868,.F.);
#23801=ORIENTED_EDGE('',*,*,#16869,.F.);
#23802=ORIENTED_EDGE('',*,*,#16870,.T.);
#23803=ORIENTED_EDGE('',*,*,#16871,.F.);
#23804=ORIENTED_EDGE('',*,*,#16872,.F.);
#23805=ORIENTED_EDGE('',*,*,#16873,.F.);
#23806=ORIENTED_EDGE('',*,*,#16874,.T.);
#23807=ORIENTED_EDGE('',*,*,#16875,.F.);
#23808=ORIENTED_EDGE('',*,*,#16876,.F.);
#23809=ORIENTED_EDGE('',*,*,#16877,.F.);
#23810=ORIENTED_EDGE('',*,*,#16878,.T.);
#23811=ORIENTED_EDGE('',*,*,#16879,.F.);
#23812=ORIENTED_EDGE('',*,*,#16880,.F.);
#23813=ORIENTED_EDGE('',*,*,#16881,.F.);
#23814=ORIENTED_EDGE('',*,*,#16882,.T.);
#23815=ORIENTED_EDGE('',*,*,#16883,.F.);
#23816=ORIENTED_EDGE('',*,*,#16884,.F.);
#23817=ORIENTED_EDGE('',*,*,#16885,.F.);
#23818=ORIENTED_EDGE('',*,*,#16886,.T.);
#23819=ORIENTED_EDGE('',*,*,#16887,.F.);
#23820=ORIENTED_EDGE('',*,*,#16888,.F.);
#23821=ORIENTED_EDGE('',*,*,#16889,.F.);
#23822=ORIENTED_EDGE('',*,*,#16890,.T.);
#23823=ORIENTED_EDGE('',*,*,#16891,.F.);
#23824=ORIENTED_EDGE('',*,*,#16892,.F.);
#23825=ORIENTED_EDGE('',*,*,#16893,.F.);
#23826=ORIENTED_EDGE('',*,*,#16894,.T.);
#23827=ORIENTED_EDGE('',*,*,#16895,.F.);
#23828=ORIENTED_EDGE('',*,*,#16896,.F.);
#23829=ORIENTED_EDGE('',*,*,#16897,.F.);
#23830=ORIENTED_EDGE('',*,*,#16898,.T.);
#23831=ORIENTED_EDGE('',*,*,#16899,.F.);
#23832=ORIENTED_EDGE('',*,*,#16900,.F.);
#23833=ORIENTED_EDGE('',*,*,#16901,.F.);
#23834=ORIENTED_EDGE('',*,*,#16902,.T.);
#23835=ORIENTED_EDGE('',*,*,#16903,.F.);
#23836=ORIENTED_EDGE('',*,*,#16904,.F.);
#23837=ORIENTED_EDGE('',*,*,#16905,.F.);
#23838=ORIENTED_EDGE('',*,*,#16906,.T.);
#23839=ORIENTED_EDGE('',*,*,#16907,.F.);
#23840=ORIENTED_EDGE('',*,*,#16908,.F.);
#23841=ORIENTED_EDGE('',*,*,#16909,.F.);
#23842=ORIENTED_EDGE('',*,*,#16910,.T.);
#23843=ORIENTED_EDGE('',*,*,#16911,.F.);
#23844=ORIENTED_EDGE('',*,*,#16912,.F.);
#23845=ORIENTED_EDGE('',*,*,#16913,.F.);
#23846=ORIENTED_EDGE('',*,*,#16914,.T.);
#23847=ORIENTED_EDGE('',*,*,#16915,.F.);
#23848=ORIENTED_EDGE('',*,*,#16916,.F.);
#23849=ORIENTED_EDGE('',*,*,#16917,.F.);
#23850=ORIENTED_EDGE('',*,*,#16918,.T.);
#23851=ORIENTED_EDGE('',*,*,#16919,.F.);
#23852=ORIENTED_EDGE('',*,*,#16920,.F.);
#23853=ORIENTED_EDGE('',*,*,#16921,.F.);
#23854=ORIENTED_EDGE('',*,*,#16922,.T.);
#23855=ORIENTED_EDGE('',*,*,#16923,.F.);
#23856=ORIENTED_EDGE('',*,*,#16924,.F.);
#23857=ORIENTED_EDGE('',*,*,#16925,.F.);
#23858=ORIENTED_EDGE('',*,*,#16926,.T.);
#23859=ORIENTED_EDGE('',*,*,#16927,.F.);
#23860=ORIENTED_EDGE('',*,*,#16928,.F.);
#23861=ORIENTED_EDGE('',*,*,#16929,.F.);
#23862=ORIENTED_EDGE('',*,*,#16930,.T.);
#23863=ORIENTED_EDGE('',*,*,#16931,.F.);
#23864=ORIENTED_EDGE('',*,*,#16932,.F.);
#23865=ORIENTED_EDGE('',*,*,#16933,.F.);
#23866=ORIENTED_EDGE('',*,*,#16934,.T.);
#23867=ORIENTED_EDGE('',*,*,#16935,.F.);
#23868=ORIENTED_EDGE('',*,*,#16936,.F.);
#23869=ORIENTED_EDGE('',*,*,#16937,.F.);
#23870=ORIENTED_EDGE('',*,*,#16938,.T.);
#23871=ORIENTED_EDGE('',*,*,#16939,.F.);
#23872=ORIENTED_EDGE('',*,*,#16940,.F.);
#23873=ORIENTED_EDGE('',*,*,#16941,.F.);
#23874=ORIENTED_EDGE('',*,*,#16942,.T.);
#23875=ORIENTED_EDGE('',*,*,#16943,.F.);
#23876=ORIENTED_EDGE('',*,*,#16944,.F.);
#23877=ORIENTED_EDGE('',*,*,#16945,.F.);
#23878=ORIENTED_EDGE('',*,*,#16946,.T.);
#23879=ORIENTED_EDGE('',*,*,#16947,.F.);
#23880=ORIENTED_EDGE('',*,*,#16948,.F.);
#23881=ORIENTED_EDGE('',*,*,#16949,.F.);
#23882=ORIENTED_EDGE('',*,*,#16950,.T.);
#23883=ORIENTED_EDGE('',*,*,#16951,.F.);
#23884=ORIENTED_EDGE('',*,*,#16952,.F.);
#23885=ORIENTED_EDGE('',*,*,#16953,.F.);
#23886=ORIENTED_EDGE('',*,*,#16954,.T.);
#23887=ORIENTED_EDGE('',*,*,#16955,.F.);
#23888=ORIENTED_EDGE('',*,*,#16956,.F.);
#23889=ORIENTED_EDGE('',*,*,#16957,.F.);
#23890=ORIENTED_EDGE('',*,*,#16958,.T.);
#23891=ORIENTED_EDGE('',*,*,#16959,.F.);
#23892=ORIENTED_EDGE('',*,*,#16960,.F.);
#23893=ORIENTED_EDGE('',*,*,#16961,.F.);
#23894=ORIENTED_EDGE('',*,*,#16962,.T.);
#23895=ORIENTED_EDGE('',*,*,#16963,.F.);
#23896=ORIENTED_EDGE('',*,*,#16964,.F.);
#23897=ORIENTED_EDGE('',*,*,#16965,.F.);
#23898=ORIENTED_EDGE('',*,*,#16966,.T.);
#23899=ORIENTED_EDGE('',*,*,#16967,.F.);
#23900=ORIENTED_EDGE('',*,*,#16968,.F.);
#23901=ORIENTED_EDGE('',*,*,#16969,.F.);
#23902=ORIENTED_EDGE('',*,*,#16970,.T.);
#23903=ORIENTED_EDGE('',*,*,#16971,.F.);
#23904=ORIENTED_EDGE('',*,*,#16972,.F.);
#23905=ORIENTED_EDGE('',*,*,#16973,.F.);
#23906=ORIENTED_EDGE('',*,*,#16974,.T.);
#23907=ORIENTED_EDGE('',*,*,#16975,.F.);
#23908=ORIENTED_EDGE('',*,*,#16976,.F.);
#23909=ORIENTED_EDGE('',*,*,#16977,.F.);
#23910=ORIENTED_EDGE('',*,*,#16978,.T.);
#23911=ORIENTED_EDGE('',*,*,#16979,.F.);
#23912=ORIENTED_EDGE('',*,*,#16980,.F.);
#23913=ORIENTED_EDGE('',*,*,#16981,.F.);
#23914=ORIENTED_EDGE('',*,*,#16982,.T.);
#23915=ORIENTED_EDGE('',*,*,#16983,.F.);
#23916=ORIENTED_EDGE('',*,*,#16984,.F.);
#23917=ORIENTED_EDGE('',*,*,#16985,.F.);
#23918=ORIENTED_EDGE('',*,*,#16986,.T.);
#23919=ORIENTED_EDGE('',*,*,#16987,.F.);
#23920=ORIENTED_EDGE('',*,*,#16988,.F.);
#23921=ORIENTED_EDGE('',*,*,#16989,.F.);
#23922=ORIENTED_EDGE('',*,*,#16990,.T.);
#23923=ORIENTED_EDGE('',*,*,#16991,.F.);
#23924=ORIENTED_EDGE('',*,*,#16992,.F.);
#23925=ORIENTED_EDGE('',*,*,#16993,.F.);
#23926=ORIENTED_EDGE('',*,*,#16994,.T.);
#23927=ORIENTED_EDGE('',*,*,#16995,.F.);
#23928=ORIENTED_EDGE('',*,*,#16996,.F.);
#23929=ORIENTED_EDGE('',*,*,#16997,.F.);
#23930=ORIENTED_EDGE('',*,*,#16998,.T.);
#23931=ORIENTED_EDGE('',*,*,#16999,.F.);
#23932=ORIENTED_EDGE('',*,*,#17000,.F.);
#23933=ORIENTED_EDGE('',*,*,#17001,.F.);
#23934=ORIENTED_EDGE('',*,*,#17002,.T.);
#23935=ORIENTED_EDGE('',*,*,#17003,.F.);
#23936=ORIENTED_EDGE('',*,*,#17004,.F.);
#23937=ORIENTED_EDGE('',*,*,#17005,.F.);
#23938=ORIENTED_EDGE('',*,*,#17006,.T.);
#23939=ORIENTED_EDGE('',*,*,#17007,.F.);
#23940=ORIENTED_EDGE('',*,*,#17008,.F.);
#23941=ORIENTED_EDGE('',*,*,#17009,.F.);
#23942=ORIENTED_EDGE('',*,*,#17010,.T.);
#23943=ORIENTED_EDGE('',*,*,#17011,.F.);
#23944=ORIENTED_EDGE('',*,*,#17012,.F.);
#23945=ORIENTED_EDGE('',*,*,#17013,.F.);
#23946=ORIENTED_EDGE('',*,*,#17014,.T.);
#23947=ORIENTED_EDGE('',*,*,#17015,.F.);
#23948=ORIENTED_EDGE('',*,*,#17016,.F.);
#23949=ORIENTED_EDGE('',*,*,#17017,.F.);
#23950=ORIENTED_EDGE('',*,*,#17018,.T.);
#23951=ORIENTED_EDGE('',*,*,#17019,.F.);
#23952=ORIENTED_EDGE('',*,*,#17020,.F.);
#23953=ORIENTED_EDGE('',*,*,#17021,.F.);
#23954=ORIENTED_EDGE('',*,*,#17022,.T.);
#23955=ORIENTED_EDGE('',*,*,#17023,.F.);
#23956=ORIENTED_EDGE('',*,*,#17024,.F.);
#23957=ORIENTED_EDGE('',*,*,#17025,.F.);
#23958=ORIENTED_EDGE('',*,*,#17026,.T.);
#23959=ORIENTED_EDGE('',*,*,#17027,.F.);
#23960=ORIENTED_EDGE('',*,*,#17028,.F.);
#23961=ORIENTED_EDGE('',*,*,#17029,.F.);
#23962=ORIENTED_EDGE('',*,*,#17030,.T.);
#23963=ORIENTED_EDGE('',*,*,#17031,.F.);
#23964=ORIENTED_EDGE('',*,*,#17032,.F.);
#23965=ORIENTED_EDGE('',*,*,#17033,.F.);
#23966=ORIENTED_EDGE('',*,*,#17034,.T.);
#23967=ORIENTED_EDGE('',*,*,#17035,.F.);
#23968=ORIENTED_EDGE('',*,*,#17036,.F.);
#23969=ORIENTED_EDGE('',*,*,#17037,.F.);
#23970=ORIENTED_EDGE('',*,*,#17038,.T.);
#23971=ORIENTED_EDGE('',*,*,#17039,.F.);
#23972=ORIENTED_EDGE('',*,*,#17040,.F.);
#23973=ORIENTED_EDGE('',*,*,#17041,.F.);
#23974=ORIENTED_EDGE('',*,*,#17042,.T.);
#23975=ORIENTED_EDGE('',*,*,#17043,.F.);
#23976=ORIENTED_EDGE('',*,*,#17044,.F.);
#23977=ORIENTED_EDGE('',*,*,#17045,.F.);
#23978=ORIENTED_EDGE('',*,*,#17046,.T.);
#23979=ORIENTED_EDGE('',*,*,#17047,.F.);
#23980=ORIENTED_EDGE('',*,*,#16449,.F.);
#23981=ORIENTED_EDGE('',*,*,#17048,.F.);
#23982=ORIENTED_EDGE('',*,*,#17049,.T.);
#23983=ORIENTED_EDGE('',*,*,#17050,.F.);
#23984=ORIENTED_EDGE('',*,*,#16445,.F.);
#23985=ORIENTED_EDGE('',*,*,#17051,.F.);
#23986=ORIENTED_EDGE('',*,*,#17052,.T.);
#23987=ORIENTED_EDGE('',*,*,#17053,.F.);
#23988=ORIENTED_EDGE('',*,*,#16441,.F.);
#23989=ORIENTED_EDGE('',*,*,#17054,.F.);
#23990=ORIENTED_EDGE('',*,*,#17055,.T.);
#23991=ORIENTED_EDGE('',*,*,#17056,.F.);
#23992=ORIENTED_EDGE('',*,*,#16437,.F.);
#23993=ORIENTED_EDGE('',*,*,#17057,.F.);
#23994=ORIENTED_EDGE('',*,*,#17058,.T.);
#23995=ORIENTED_EDGE('',*,*,#17059,.F.);
#23996=ORIENTED_EDGE('',*,*,#16433,.F.);
#23997=ORIENTED_EDGE('',*,*,#17060,.F.);
#23998=ORIENTED_EDGE('',*,*,#17061,.T.);
#23999=ORIENTED_EDGE('',*,*,#17062,.F.);
#24000=ORIENTED_EDGE('',*,*,#16429,.F.);
#24001=ORIENTED_EDGE('',*,*,#17063,.F.);
#24002=ORIENTED_EDGE('',*,*,#17064,.T.);
#24003=ORIENTED_EDGE('',*,*,#17065,.F.);
#24004=ORIENTED_EDGE('',*,*,#16453,.F.);
#24005=ORIENTED_EDGE('',*,*,#17066,.F.);
#24006=ORIENTED_EDGE('',*,*,#17067,.T.);
#24007=ORIENTED_EDGE('',*,*,#17068,.F.);
#24008=ORIENTED_EDGE('',*,*,#16457,.F.);
#24009=ORIENTED_EDGE('',*,*,#17069,.F.);
#24010=ORIENTED_EDGE('',*,*,#17070,.T.);
#24011=ORIENTED_EDGE('',*,*,#17071,.F.);
#24012=ORIENTED_EDGE('',*,*,#16461,.F.);
#24013=ORIENTED_EDGE('',*,*,#17072,.F.);
#24014=ORIENTED_EDGE('',*,*,#17073,.T.);
#24015=ORIENTED_EDGE('',*,*,#17074,.F.);
#24016=ORIENTED_EDGE('',*,*,#16465,.F.);
#24017=ORIENTED_EDGE('',*,*,#17075,.F.);
#24018=ORIENTED_EDGE('',*,*,#17076,.T.);
#24019=ORIENTED_EDGE('',*,*,#17077,.F.);
#24020=ORIENTED_EDGE('',*,*,#16469,.F.);
#24021=ORIENTED_EDGE('',*,*,#17078,.F.);
#24022=ORIENTED_EDGE('',*,*,#17079,.T.);
#24023=ORIENTED_EDGE('',*,*,#17080,.F.);
#24024=ORIENTED_EDGE('',*,*,#16473,.F.);
#24025=ORIENTED_EDGE('',*,*,#17081,.F.);
#24026=ORIENTED_EDGE('',*,*,#17082,.T.);
#24027=ORIENTED_EDGE('',*,*,#17083,.F.);
#24028=ORIENTED_EDGE('',*,*,#16477,.F.);
#24029=ORIENTED_EDGE('',*,*,#17084,.F.);
#24030=ORIENTED_EDGE('',*,*,#17085,.T.);
#24031=ORIENTED_EDGE('',*,*,#17086,.F.);
#24032=ORIENTED_EDGE('',*,*,#16481,.F.);
#24033=ORIENTED_EDGE('',*,*,#17087,.F.);
#24034=ORIENTED_EDGE('',*,*,#17088,.T.);
#24035=ORIENTED_EDGE('',*,*,#17089,.F.);
#24036=ORIENTED_EDGE('',*,*,#16485,.F.);
#24037=ORIENTED_EDGE('',*,*,#17090,.F.);
#24038=ORIENTED_EDGE('',*,*,#17091,.T.);
#24039=ORIENTED_EDGE('',*,*,#17092,.F.);
#24040=ORIENTED_EDGE('',*,*,#17093,.F.);
#24041=ORIENTED_EDGE('',*,*,#17094,.F.);
#24042=ORIENTED_EDGE('',*,*,#17095,.T.);
#24043=ORIENTED_EDGE('',*,*,#17096,.F.);
#24044=ORIENTED_EDGE('',*,*,#17097,.F.);
#24045=ORIENTED_EDGE('',*,*,#17098,.F.);
#24046=ORIENTED_EDGE('',*,*,#17099,.T.);
#24047=ORIENTED_EDGE('',*,*,#17100,.F.);
#24048=ORIENTED_EDGE('',*,*,#17101,.F.);
#24049=ORIENTED_EDGE('',*,*,#17102,.F.);
#24050=ORIENTED_EDGE('',*,*,#17103,.T.);
#24051=ORIENTED_EDGE('',*,*,#17104,.F.);
#24052=ORIENTED_EDGE('',*,*,#17105,.F.);
#24053=ORIENTED_EDGE('',*,*,#17106,.F.);
#24054=ORIENTED_EDGE('',*,*,#17107,.T.);
#24055=ORIENTED_EDGE('',*,*,#17108,.F.);
#24056=ORIENTED_EDGE('',*,*,#17109,.F.);
#24057=ORIENTED_EDGE('',*,*,#17110,.F.);
#24058=ORIENTED_EDGE('',*,*,#17111,.T.);
#24059=ORIENTED_EDGE('',*,*,#17112,.F.);
#24060=ORIENTED_EDGE('',*,*,#17113,.F.);
#24061=ORIENTED_EDGE('',*,*,#17114,.T.);
#24062=ORIENTED_EDGE('',*,*,#17115,.F.);
#24063=ORIENTED_EDGE('',*,*,#17116,.F.);
#24064=ORIENTED_EDGE('',*,*,#17114,.F.);
#24065=ORIENTED_EDGE('',*,*,#17117,.F.);
#24066=ORIENTED_EDGE('',*,*,#17118,.T.);
#24067=ORIENTED_EDGE('',*,*,#17115,.T.);
#24068=ORIENTED_EDGE('',*,*,#17116,.T.);
#24069=ORIENTED_EDGE('',*,*,#17118,.F.);
#24070=ORIENTED_EDGE('',*,*,#17119,.F.);
#24071=ORIENTED_EDGE('',*,*,#17120,.T.);
#24072=ORIENTED_EDGE('',*,*,#17117,.T.);
#24073=ORIENTED_EDGE('',*,*,#17120,.F.);
#24074=ORIENTED_EDGE('',*,*,#17121,.F.);
#24075=ORIENTED_EDGE('',*,*,#17122,.T.);
#24076=ORIENTED_EDGE('',*,*,#17119,.T.);
#24077=ORIENTED_EDGE('',*,*,#17122,.F.);
#24078=ORIENTED_EDGE('',*,*,#16244,.F.);
#24079=ORIENTED_EDGE('',*,*,#17123,.T.);
#24080=ORIENTED_EDGE('',*,*,#17124,.T.);
#24081=ORIENTED_EDGE('',*,*,#17123,.F.);
#24082=ORIENTED_EDGE('',*,*,#17125,.F.);
#24083=ORIENTED_EDGE('',*,*,#17126,.T.);
#24084=ORIENTED_EDGE('',*,*,#17127,.F.);
#24085=ORIENTED_EDGE('',*,*,#17064,.F.);
#24086=ORIENTED_EDGE('',*,*,#17128,.F.);
#24087=ORIENTED_EDGE('',*,*,#17061,.F.);
#24088=ORIENTED_EDGE('',*,*,#17129,.F.);
#24089=ORIENTED_EDGE('',*,*,#17130,.T.);
#24090=ORIENTED_EDGE('',*,*,#17131,.F.);
#24091=ORIENTED_EDGE('',*,*,#17058,.F.);
#24092=ORIENTED_EDGE('',*,*,#17132,.F.);
#24093=ORIENTED_EDGE('',*,*,#17133,.T.);
#24094=ORIENTED_EDGE('',*,*,#17134,.F.);
#24095=ORIENTED_EDGE('',*,*,#17055,.F.);
#24096=ORIENTED_EDGE('',*,*,#17135,.F.);
#24097=ORIENTED_EDGE('',*,*,#17136,.T.);
#24098=ORIENTED_EDGE('',*,*,#17137,.F.);
#24099=ORIENTED_EDGE('',*,*,#17052,.F.);
#24100=ORIENTED_EDGE('',*,*,#17138,.F.);
#24101=ORIENTED_EDGE('',*,*,#17139,.T.);
#24102=ORIENTED_EDGE('',*,*,#17140,.F.);
#24103=ORIENTED_EDGE('',*,*,#17049,.F.);
#24104=ORIENTED_EDGE('',*,*,#17141,.F.);
#24105=ORIENTED_EDGE('',*,*,#17142,.T.);
#24106=ORIENTED_EDGE('',*,*,#17143,.F.);
#24107=ORIENTED_EDGE('',*,*,#17046,.F.);
#24108=ORIENTED_EDGE('',*,*,#17144,.F.);
#24109=ORIENTED_EDGE('',*,*,#17145,.T.);
#24110=ORIENTED_EDGE('',*,*,#17146,.F.);
#24111=ORIENTED_EDGE('',*,*,#17042,.F.);
#24112=ORIENTED_EDGE('',*,*,#17147,.F.);
#24113=ORIENTED_EDGE('',*,*,#17148,.T.);
#24114=ORIENTED_EDGE('',*,*,#17149,.F.);
#24115=ORIENTED_EDGE('',*,*,#17038,.F.);
#24116=ORIENTED_EDGE('',*,*,#17150,.F.);
#24117=ORIENTED_EDGE('',*,*,#17151,.T.);
#24118=ORIENTED_EDGE('',*,*,#17152,.F.);
#24119=ORIENTED_EDGE('',*,*,#17034,.F.);
#24120=ORIENTED_EDGE('',*,*,#17153,.F.);
#24121=ORIENTED_EDGE('',*,*,#17154,.T.);
#24122=ORIENTED_EDGE('',*,*,#17155,.F.);
#24123=ORIENTED_EDGE('',*,*,#17030,.F.);
#24124=ORIENTED_EDGE('',*,*,#17156,.F.);
#24125=ORIENTED_EDGE('',*,*,#17157,.T.);
#24126=ORIENTED_EDGE('',*,*,#17158,.F.);
#24127=ORIENTED_EDGE('',*,*,#17026,.F.);
#24128=ORIENTED_EDGE('',*,*,#17159,.F.);
#24129=ORIENTED_EDGE('',*,*,#17160,.T.);
#24130=ORIENTED_EDGE('',*,*,#17161,.F.);
#24131=ORIENTED_EDGE('',*,*,#17022,.F.);
#24132=ORIENTED_EDGE('',*,*,#17162,.F.);
#24133=ORIENTED_EDGE('',*,*,#17163,.T.);
#24134=ORIENTED_EDGE('',*,*,#17164,.F.);
#24135=ORIENTED_EDGE('',*,*,#17018,.F.);
#24136=ORIENTED_EDGE('',*,*,#17165,.F.);
#24137=ORIENTED_EDGE('',*,*,#17166,.T.);
#24138=ORIENTED_EDGE('',*,*,#17167,.F.);
#24139=ORIENTED_EDGE('',*,*,#17014,.F.);
#24140=ORIENTED_EDGE('',*,*,#17168,.F.);
#24141=ORIENTED_EDGE('',*,*,#17169,.T.);
#24142=ORIENTED_EDGE('',*,*,#17170,.F.);
#24143=ORIENTED_EDGE('',*,*,#17010,.F.);
#24144=ORIENTED_EDGE('',*,*,#17171,.F.);
#24145=ORIENTED_EDGE('',*,*,#17172,.T.);
#24146=ORIENTED_EDGE('',*,*,#17173,.F.);
#24147=ORIENTED_EDGE('',*,*,#17006,.F.);
#24148=ORIENTED_EDGE('',*,*,#17174,.F.);
#24149=ORIENTED_EDGE('',*,*,#17175,.T.);
#24150=ORIENTED_EDGE('',*,*,#17176,.F.);
#24151=ORIENTED_EDGE('',*,*,#17002,.F.);
#24152=ORIENTED_EDGE('',*,*,#17177,.F.);
#24153=ORIENTED_EDGE('',*,*,#17178,.T.);
#24154=ORIENTED_EDGE('',*,*,#17179,.F.);
#24155=ORIENTED_EDGE('',*,*,#16998,.F.);
#24156=ORIENTED_EDGE('',*,*,#17180,.F.);
#24157=ORIENTED_EDGE('',*,*,#17181,.T.);
#24158=ORIENTED_EDGE('',*,*,#17182,.F.);
#24159=ORIENTED_EDGE('',*,*,#16994,.F.);
#24160=ORIENTED_EDGE('',*,*,#17183,.F.);
#24161=ORIENTED_EDGE('',*,*,#17184,.T.);
#24162=ORIENTED_EDGE('',*,*,#17185,.F.);
#24163=ORIENTED_EDGE('',*,*,#16990,.F.);
#24164=ORIENTED_EDGE('',*,*,#17186,.F.);
#24165=ORIENTED_EDGE('',*,*,#17187,.T.);
#24166=ORIENTED_EDGE('',*,*,#17188,.F.);
#24167=ORIENTED_EDGE('',*,*,#16986,.F.);
#24168=ORIENTED_EDGE('',*,*,#17189,.F.);
#24169=ORIENTED_EDGE('',*,*,#17190,.T.);
#24170=ORIENTED_EDGE('',*,*,#17191,.F.);
#24171=ORIENTED_EDGE('',*,*,#16982,.F.);
#24172=ORIENTED_EDGE('',*,*,#17192,.F.);
#24173=ORIENTED_EDGE('',*,*,#17193,.T.);
#24174=ORIENTED_EDGE('',*,*,#17194,.F.);
#24175=ORIENTED_EDGE('',*,*,#16978,.F.);
#24176=ORIENTED_EDGE('',*,*,#17195,.F.);
#24177=ORIENTED_EDGE('',*,*,#17196,.T.);
#24178=ORIENTED_EDGE('',*,*,#17197,.F.);
#24179=ORIENTED_EDGE('',*,*,#16974,.F.);
#24180=ORIENTED_EDGE('',*,*,#17198,.F.);
#24181=ORIENTED_EDGE('',*,*,#17199,.T.);
#24182=ORIENTED_EDGE('',*,*,#17200,.F.);
#24183=ORIENTED_EDGE('',*,*,#16970,.F.);
#24184=ORIENTED_EDGE('',*,*,#17201,.F.);
#24185=ORIENTED_EDGE('',*,*,#17202,.T.);
#24186=ORIENTED_EDGE('',*,*,#17203,.F.);
#24187=ORIENTED_EDGE('',*,*,#16966,.F.);
#24188=ORIENTED_EDGE('',*,*,#17204,.F.);
#24189=ORIENTED_EDGE('',*,*,#17205,.T.);
#24190=ORIENTED_EDGE('',*,*,#17206,.F.);
#24191=ORIENTED_EDGE('',*,*,#16962,.F.);
#24192=ORIENTED_EDGE('',*,*,#17207,.F.);
#24193=ORIENTED_EDGE('',*,*,#17208,.T.);
#24194=ORIENTED_EDGE('',*,*,#17209,.F.);
#24195=ORIENTED_EDGE('',*,*,#16958,.F.);
#24196=ORIENTED_EDGE('',*,*,#17210,.F.);
#24197=ORIENTED_EDGE('',*,*,#17211,.T.);
#24198=ORIENTED_EDGE('',*,*,#17212,.F.);
#24199=ORIENTED_EDGE('',*,*,#16954,.F.);
#24200=ORIENTED_EDGE('',*,*,#17213,.F.);
#24201=ORIENTED_EDGE('',*,*,#17214,.T.);
#24202=ORIENTED_EDGE('',*,*,#17215,.F.);
#24203=ORIENTED_EDGE('',*,*,#16950,.F.);
#24204=ORIENTED_EDGE('',*,*,#17216,.F.);
#24205=ORIENTED_EDGE('',*,*,#17217,.T.);
#24206=ORIENTED_EDGE('',*,*,#17218,.F.);
#24207=ORIENTED_EDGE('',*,*,#16946,.F.);
#24208=ORIENTED_EDGE('',*,*,#17219,.F.);
#24209=ORIENTED_EDGE('',*,*,#17220,.T.);
#24210=ORIENTED_EDGE('',*,*,#17221,.F.);
#24211=ORIENTED_EDGE('',*,*,#16942,.F.);
#24212=ORIENTED_EDGE('',*,*,#17222,.F.);
#24213=ORIENTED_EDGE('',*,*,#17223,.T.);
#24214=ORIENTED_EDGE('',*,*,#17224,.F.);
#24215=ORIENTED_EDGE('',*,*,#16938,.F.);
#24216=ORIENTED_EDGE('',*,*,#17225,.F.);
#24217=ORIENTED_EDGE('',*,*,#17226,.T.);
#24218=ORIENTED_EDGE('',*,*,#17227,.F.);
#24219=ORIENTED_EDGE('',*,*,#16934,.F.);
#24220=ORIENTED_EDGE('',*,*,#17228,.F.);
#24221=ORIENTED_EDGE('',*,*,#17229,.T.);
#24222=ORIENTED_EDGE('',*,*,#17230,.F.);
#24223=ORIENTED_EDGE('',*,*,#16930,.F.);
#24224=ORIENTED_EDGE('',*,*,#17231,.F.);
#24225=ORIENTED_EDGE('',*,*,#17232,.T.);
#24226=ORIENTED_EDGE('',*,*,#17233,.F.);
#24227=ORIENTED_EDGE('',*,*,#16926,.F.);
#24228=ORIENTED_EDGE('',*,*,#17234,.F.);
#24229=ORIENTED_EDGE('',*,*,#17235,.T.);
#24230=ORIENTED_EDGE('',*,*,#17236,.F.);
#24231=ORIENTED_EDGE('',*,*,#16922,.F.);
#24232=ORIENTED_EDGE('',*,*,#17237,.F.);
#24233=ORIENTED_EDGE('',*,*,#17238,.T.);
#24234=ORIENTED_EDGE('',*,*,#17239,.F.);
#24235=ORIENTED_EDGE('',*,*,#16918,.F.);
#24236=ORIENTED_EDGE('',*,*,#17240,.F.);
#24237=ORIENTED_EDGE('',*,*,#17241,.T.);
#24238=ORIENTED_EDGE('',*,*,#17242,.F.);
#24239=ORIENTED_EDGE('',*,*,#16914,.F.);
#24240=ORIENTED_EDGE('',*,*,#17243,.F.);
#24241=ORIENTED_EDGE('',*,*,#17244,.T.);
#24242=ORIENTED_EDGE('',*,*,#17245,.F.);
#24243=ORIENTED_EDGE('',*,*,#16910,.F.);
#24244=ORIENTED_EDGE('',*,*,#17246,.F.);
#24245=ORIENTED_EDGE('',*,*,#17247,.T.);
#24246=ORIENTED_EDGE('',*,*,#17248,.F.);
#24247=ORIENTED_EDGE('',*,*,#16906,.F.);
#24248=ORIENTED_EDGE('',*,*,#17249,.F.);
#24249=ORIENTED_EDGE('',*,*,#17250,.T.);
#24250=ORIENTED_EDGE('',*,*,#17251,.F.);
#24251=ORIENTED_EDGE('',*,*,#16902,.F.);
#24252=ORIENTED_EDGE('',*,*,#17252,.F.);
#24253=ORIENTED_EDGE('',*,*,#17253,.T.);
#24254=ORIENTED_EDGE('',*,*,#17254,.F.);
#24255=ORIENTED_EDGE('',*,*,#16898,.F.);
#24256=ORIENTED_EDGE('',*,*,#17255,.F.);
#24257=ORIENTED_EDGE('',*,*,#17256,.T.);
#24258=ORIENTED_EDGE('',*,*,#17257,.F.);
#24259=ORIENTED_EDGE('',*,*,#16894,.F.);
#24260=ORIENTED_EDGE('',*,*,#17258,.F.);
#24261=ORIENTED_EDGE('',*,*,#17259,.T.);
#24262=ORIENTED_EDGE('',*,*,#17260,.F.);
#24263=ORIENTED_EDGE('',*,*,#16890,.F.);
#24264=ORIENTED_EDGE('',*,*,#17261,.F.);
#24265=ORIENTED_EDGE('',*,*,#17262,.T.);
#24266=ORIENTED_EDGE('',*,*,#17263,.F.);
#24267=ORIENTED_EDGE('',*,*,#16886,.F.);
#24268=ORIENTED_EDGE('',*,*,#17264,.F.);
#24269=ORIENTED_EDGE('',*,*,#17265,.T.);
#24270=ORIENTED_EDGE('',*,*,#17266,.F.);
#24271=ORIENTED_EDGE('',*,*,#16882,.F.);
#24272=ORIENTED_EDGE('',*,*,#17267,.F.);
#24273=ORIENTED_EDGE('',*,*,#17268,.T.);
#24274=ORIENTED_EDGE('',*,*,#17269,.F.);
#24275=ORIENTED_EDGE('',*,*,#16878,.F.);
#24276=ORIENTED_EDGE('',*,*,#17270,.F.);
#24277=ORIENTED_EDGE('',*,*,#17271,.T.);
#24278=ORIENTED_EDGE('',*,*,#17272,.F.);
#24279=ORIENTED_EDGE('',*,*,#16874,.F.);
#24280=ORIENTED_EDGE('',*,*,#17273,.F.);
#24281=ORIENTED_EDGE('',*,*,#17274,.T.);
#24282=ORIENTED_EDGE('',*,*,#17275,.F.);
#24283=ORIENTED_EDGE('',*,*,#16870,.F.);
#24284=ORIENTED_EDGE('',*,*,#17276,.F.);
#24285=ORIENTED_EDGE('',*,*,#17277,.T.);
#24286=ORIENTED_EDGE('',*,*,#17278,.F.);
#24287=ORIENTED_EDGE('',*,*,#16866,.F.);
#24288=ORIENTED_EDGE('',*,*,#17279,.F.);
#24289=ORIENTED_EDGE('',*,*,#17280,.T.);
#24290=ORIENTED_EDGE('',*,*,#17281,.F.);
#24291=ORIENTED_EDGE('',*,*,#16862,.F.);
#24292=ORIENTED_EDGE('',*,*,#17282,.F.);
#24293=ORIENTED_EDGE('',*,*,#17283,.T.);
#24294=ORIENTED_EDGE('',*,*,#17284,.F.);
#24295=ORIENTED_EDGE('',*,*,#16858,.F.);
#24296=ORIENTED_EDGE('',*,*,#17285,.F.);
#24297=ORIENTED_EDGE('',*,*,#17286,.T.);
#24298=ORIENTED_EDGE('',*,*,#17287,.F.);
#24299=ORIENTED_EDGE('',*,*,#16854,.F.);
#24300=ORIENTED_EDGE('',*,*,#17288,.F.);
#24301=ORIENTED_EDGE('',*,*,#17289,.T.);
#24302=ORIENTED_EDGE('',*,*,#17290,.F.);
#24303=ORIENTED_EDGE('',*,*,#16850,.F.);
#24304=ORIENTED_EDGE('',*,*,#17291,.F.);
#24305=ORIENTED_EDGE('',*,*,#17292,.T.);
#24306=ORIENTED_EDGE('',*,*,#17293,.F.);
#24307=ORIENTED_EDGE('',*,*,#16846,.F.);
#24308=ORIENTED_EDGE('',*,*,#17294,.F.);
#24309=ORIENTED_EDGE('',*,*,#17295,.T.);
#24310=ORIENTED_EDGE('',*,*,#17296,.F.);
#24311=ORIENTED_EDGE('',*,*,#16842,.F.);
#24312=ORIENTED_EDGE('',*,*,#17297,.F.);
#24313=ORIENTED_EDGE('',*,*,#17298,.T.);
#24314=ORIENTED_EDGE('',*,*,#17299,.F.);
#24315=ORIENTED_EDGE('',*,*,#16838,.F.);
#24316=ORIENTED_EDGE('',*,*,#17300,.F.);
#24317=ORIENTED_EDGE('',*,*,#17301,.T.);
#24318=ORIENTED_EDGE('',*,*,#17302,.F.);
#24319=ORIENTED_EDGE('',*,*,#16834,.F.);
#24320=ORIENTED_EDGE('',*,*,#17303,.F.);
#24321=ORIENTED_EDGE('',*,*,#17304,.T.);
#24322=ORIENTED_EDGE('',*,*,#17305,.F.);
#24323=ORIENTED_EDGE('',*,*,#16830,.F.);
#24324=ORIENTED_EDGE('',*,*,#17306,.F.);
#24325=ORIENTED_EDGE('',*,*,#17307,.T.);
#24326=ORIENTED_EDGE('',*,*,#17308,.F.);
#24327=ORIENTED_EDGE('',*,*,#16826,.F.);
#24328=ORIENTED_EDGE('',*,*,#17309,.F.);
#24329=ORIENTED_EDGE('',*,*,#17310,.T.);
#24330=ORIENTED_EDGE('',*,*,#17311,.F.);
#24331=ORIENTED_EDGE('',*,*,#16822,.F.);
#24332=ORIENTED_EDGE('',*,*,#17312,.F.);
#24333=ORIENTED_EDGE('',*,*,#17313,.T.);
#24334=ORIENTED_EDGE('',*,*,#17314,.F.);
#24335=ORIENTED_EDGE('',*,*,#16818,.F.);
#24336=ORIENTED_EDGE('',*,*,#17315,.F.);
#24337=ORIENTED_EDGE('',*,*,#17316,.T.);
#24338=ORIENTED_EDGE('',*,*,#17317,.F.);
#24339=ORIENTED_EDGE('',*,*,#17318,.T.);
#24340=ORIENTED_EDGE('',*,*,#17319,.F.);
#24341=ORIENTED_EDGE('',*,*,#17067,.F.);
#24342=ORIENTED_EDGE('',*,*,#17320,.F.);
#24343=ORIENTED_EDGE('',*,*,#17321,.T.);
#24344=ORIENTED_EDGE('',*,*,#17322,.F.);
#24345=ORIENTED_EDGE('',*,*,#17070,.F.);
#24346=ORIENTED_EDGE('',*,*,#17323,.F.);
#24347=ORIENTED_EDGE('',*,*,#17324,.T.);
#24348=ORIENTED_EDGE('',*,*,#17325,.F.);
#24349=ORIENTED_EDGE('',*,*,#17073,.F.);
#24350=ORIENTED_EDGE('',*,*,#17326,.F.);
#24351=ORIENTED_EDGE('',*,*,#17327,.T.);
#24352=ORIENTED_EDGE('',*,*,#17328,.F.);
#24353=ORIENTED_EDGE('',*,*,#17076,.F.);
#24354=ORIENTED_EDGE('',*,*,#17329,.F.);
#24355=ORIENTED_EDGE('',*,*,#17330,.T.);
#24356=ORIENTED_EDGE('',*,*,#17331,.F.);
#24357=ORIENTED_EDGE('',*,*,#17079,.F.);
#24358=ORIENTED_EDGE('',*,*,#17332,.F.);
#24359=ORIENTED_EDGE('',*,*,#17333,.T.);
#24360=ORIENTED_EDGE('',*,*,#17334,.F.);
#24361=ORIENTED_EDGE('',*,*,#17082,.F.);
#24362=ORIENTED_EDGE('',*,*,#17335,.F.);
#24363=ORIENTED_EDGE('',*,*,#17336,.T.);
#24364=ORIENTED_EDGE('',*,*,#17337,.F.);
#24365=ORIENTED_EDGE('',*,*,#17085,.F.);
#24366=ORIENTED_EDGE('',*,*,#17338,.F.);
#24367=ORIENTED_EDGE('',*,*,#17339,.T.);
#24368=ORIENTED_EDGE('',*,*,#17340,.F.);
#24369=ORIENTED_EDGE('',*,*,#17088,.F.);
#24370=ORIENTED_EDGE('',*,*,#17341,.F.);
#24371=ORIENTED_EDGE('',*,*,#17342,.T.);
#24372=ORIENTED_EDGE('',*,*,#17343,.F.);
#24373=ORIENTED_EDGE('',*,*,#17091,.F.);
#24374=ORIENTED_EDGE('',*,*,#17344,.F.);
#24375=ORIENTED_EDGE('',*,*,#17345,.T.);
#24376=ORIENTED_EDGE('',*,*,#17346,.F.);
#24377=ORIENTED_EDGE('',*,*,#17095,.F.);
#24378=ORIENTED_EDGE('',*,*,#17347,.F.);
#24379=ORIENTED_EDGE('',*,*,#17348,.T.);
#24380=ORIENTED_EDGE('',*,*,#17349,.F.);
#24381=ORIENTED_EDGE('',*,*,#17099,.F.);
#24382=ORIENTED_EDGE('',*,*,#17350,.F.);
#24383=ORIENTED_EDGE('',*,*,#17351,.T.);
#24384=ORIENTED_EDGE('',*,*,#17352,.F.);
#24385=ORIENTED_EDGE('',*,*,#17103,.F.);
#24386=ORIENTED_EDGE('',*,*,#17353,.F.);
#24387=ORIENTED_EDGE('',*,*,#17354,.T.);
#24388=ORIENTED_EDGE('',*,*,#17355,.F.);
#24389=ORIENTED_EDGE('',*,*,#17107,.F.);
#24390=ORIENTED_EDGE('',*,*,#17356,.F.);
#24391=ORIENTED_EDGE('',*,*,#17357,.T.);
#24392=ORIENTED_EDGE('',*,*,#17358,.F.);
#24393=ORIENTED_EDGE('',*,*,#17111,.F.);
#24394=ORIENTED_EDGE('',*,*,#17359,.F.);
#24395=ORIENTED_EDGE('',*,*,#16814,.F.);
#24396=ORIENTED_EDGE('',*,*,#17360,.F.);
#24397=ORIENTED_EDGE('',*,*,#17361,.T.);
#24398=ORIENTED_EDGE('',*,*,#17362,.F.);
#24399=ORIENTED_EDGE('',*,*,#17363,.T.);
#24400=ORIENTED_EDGE('',*,*,#17364,.F.);
#24401=ORIENTED_EDGE('',*,*,#17126,.F.);
#24402=ORIENTED_EDGE('',*,*,#17365,.F.);
#24403=ORIENTED_EDGE('',*,*,#17130,.F.);
#24404=ORIENTED_EDGE('',*,*,#17366,.F.);
#24405=ORIENTED_EDGE('',*,*,#17367,.T.);
#24406=ORIENTED_EDGE('',*,*,#17368,.F.);
#24407=ORIENTED_EDGE('',*,*,#17133,.F.);
#24408=ORIENTED_EDGE('',*,*,#17369,.F.);
#24409=ORIENTED_EDGE('',*,*,#17370,.T.);
#24410=ORIENTED_EDGE('',*,*,#17371,.F.);
#24411=ORIENTED_EDGE('',*,*,#17136,.F.);
#24412=ORIENTED_EDGE('',*,*,#17372,.F.);
#24413=ORIENTED_EDGE('',*,*,#17373,.T.);
#24414=ORIENTED_EDGE('',*,*,#17374,.F.);
#24415=ORIENTED_EDGE('',*,*,#17139,.F.);
#24416=ORIENTED_EDGE('',*,*,#17375,.F.);
#24417=ORIENTED_EDGE('',*,*,#17376,.T.);
#24418=ORIENTED_EDGE('',*,*,#17377,.F.);
#24419=ORIENTED_EDGE('',*,*,#17142,.F.);
#24420=ORIENTED_EDGE('',*,*,#17378,.F.);
#24421=ORIENTED_EDGE('',*,*,#17379,.T.);
#24422=ORIENTED_EDGE('',*,*,#17380,.F.);
#24423=ORIENTED_EDGE('',*,*,#17145,.F.);
#24424=ORIENTED_EDGE('',*,*,#17381,.F.);
#24425=ORIENTED_EDGE('',*,*,#17382,.T.);
#24426=ORIENTED_EDGE('',*,*,#17383,.F.);
#24427=ORIENTED_EDGE('',*,*,#17148,.F.);
#24428=ORIENTED_EDGE('',*,*,#17384,.F.);
#24429=ORIENTED_EDGE('',*,*,#17385,.T.);
#24430=ORIENTED_EDGE('',*,*,#17386,.F.);
#24431=ORIENTED_EDGE('',*,*,#17151,.F.);
#24432=ORIENTED_EDGE('',*,*,#17387,.F.);
#24433=ORIENTED_EDGE('',*,*,#17388,.T.);
#24434=ORIENTED_EDGE('',*,*,#17389,.F.);
#24435=ORIENTED_EDGE('',*,*,#17154,.F.);
#24436=ORIENTED_EDGE('',*,*,#17390,.F.);
#24437=ORIENTED_EDGE('',*,*,#17391,.T.);
#24438=ORIENTED_EDGE('',*,*,#17392,.F.);
#24439=ORIENTED_EDGE('',*,*,#17157,.F.);
#24440=ORIENTED_EDGE('',*,*,#17393,.F.);
#24441=ORIENTED_EDGE('',*,*,#17394,.T.);
#24442=ORIENTED_EDGE('',*,*,#17395,.F.);
#24443=ORIENTED_EDGE('',*,*,#17160,.F.);
#24444=ORIENTED_EDGE('',*,*,#17396,.F.);
#24445=ORIENTED_EDGE('',*,*,#17397,.T.);
#24446=ORIENTED_EDGE('',*,*,#17398,.F.);
#24447=ORIENTED_EDGE('',*,*,#17163,.F.);
#24448=ORIENTED_EDGE('',*,*,#17399,.F.);
#24449=ORIENTED_EDGE('',*,*,#17400,.T.);
#24450=ORIENTED_EDGE('',*,*,#17401,.F.);
#24451=ORIENTED_EDGE('',*,*,#17166,.F.);
#24452=ORIENTED_EDGE('',*,*,#17402,.F.);
#24453=ORIENTED_EDGE('',*,*,#17403,.T.);
#24454=ORIENTED_EDGE('',*,*,#17404,.F.);
#24455=ORIENTED_EDGE('',*,*,#17169,.F.);
#24456=ORIENTED_EDGE('',*,*,#17405,.F.);
#24457=ORIENTED_EDGE('',*,*,#17406,.T.);
#24458=ORIENTED_EDGE('',*,*,#17407,.F.);
#24459=ORIENTED_EDGE('',*,*,#17172,.F.);
#24460=ORIENTED_EDGE('',*,*,#17408,.F.);
#24461=ORIENTED_EDGE('',*,*,#17409,.T.);
#24462=ORIENTED_EDGE('',*,*,#17410,.F.);
#24463=ORIENTED_EDGE('',*,*,#17175,.F.);
#24464=ORIENTED_EDGE('',*,*,#17411,.F.);
#24465=ORIENTED_EDGE('',*,*,#17412,.T.);
#24466=ORIENTED_EDGE('',*,*,#17413,.F.);
#24467=ORIENTED_EDGE('',*,*,#17178,.F.);
#24468=ORIENTED_EDGE('',*,*,#17414,.F.);
#24469=ORIENTED_EDGE('',*,*,#17415,.T.);
#24470=ORIENTED_EDGE('',*,*,#17416,.F.);
#24471=ORIENTED_EDGE('',*,*,#17181,.F.);
#24472=ORIENTED_EDGE('',*,*,#17417,.F.);
#24473=ORIENTED_EDGE('',*,*,#17418,.T.);
#24474=ORIENTED_EDGE('',*,*,#17419,.F.);
#24475=ORIENTED_EDGE('',*,*,#17184,.F.);
#24476=ORIENTED_EDGE('',*,*,#17420,.F.);
#24477=ORIENTED_EDGE('',*,*,#17421,.T.);
#24478=ORIENTED_EDGE('',*,*,#17422,.F.);
#24479=ORIENTED_EDGE('',*,*,#17187,.F.);
#24480=ORIENTED_EDGE('',*,*,#17423,.F.);
#24481=ORIENTED_EDGE('',*,*,#17424,.T.);
#24482=ORIENTED_EDGE('',*,*,#17425,.F.);
#24483=ORIENTED_EDGE('',*,*,#17190,.F.);
#24484=ORIENTED_EDGE('',*,*,#17426,.F.);
#24485=ORIENTED_EDGE('',*,*,#17427,.T.);
#24486=ORIENTED_EDGE('',*,*,#17428,.F.);
#24487=ORIENTED_EDGE('',*,*,#17193,.F.);
#24488=ORIENTED_EDGE('',*,*,#17429,.F.);
#24489=ORIENTED_EDGE('',*,*,#17430,.T.);
#24490=ORIENTED_EDGE('',*,*,#17431,.F.);
#24491=ORIENTED_EDGE('',*,*,#17196,.F.);
#24492=ORIENTED_EDGE('',*,*,#17432,.F.);
#24493=ORIENTED_EDGE('',*,*,#17433,.T.);
#24494=ORIENTED_EDGE('',*,*,#17434,.F.);
#24495=ORIENTED_EDGE('',*,*,#17199,.F.);
#24496=ORIENTED_EDGE('',*,*,#17435,.F.);
#24497=ORIENTED_EDGE('',*,*,#17436,.T.);
#24498=ORIENTED_EDGE('',*,*,#17437,.F.);
#24499=ORIENTED_EDGE('',*,*,#17202,.F.);
#24500=ORIENTED_EDGE('',*,*,#17438,.F.);
#24501=ORIENTED_EDGE('',*,*,#17439,.T.);
#24502=ORIENTED_EDGE('',*,*,#17440,.F.);
#24503=ORIENTED_EDGE('',*,*,#17205,.F.);
#24504=ORIENTED_EDGE('',*,*,#17441,.F.);
#24505=ORIENTED_EDGE('',*,*,#17442,.T.);
#24506=ORIENTED_EDGE('',*,*,#17443,.F.);
#24507=ORIENTED_EDGE('',*,*,#17208,.F.);
#24508=ORIENTED_EDGE('',*,*,#17444,.F.);
#24509=ORIENTED_EDGE('',*,*,#17445,.T.);
#24510=ORIENTED_EDGE('',*,*,#17446,.F.);
#24511=ORIENTED_EDGE('',*,*,#17211,.F.);
#24512=ORIENTED_EDGE('',*,*,#17447,.F.);
#24513=ORIENTED_EDGE('',*,*,#17448,.T.);
#24514=ORIENTED_EDGE('',*,*,#17449,.F.);
#24515=ORIENTED_EDGE('',*,*,#17214,.F.);
#24516=ORIENTED_EDGE('',*,*,#17450,.F.);
#24517=ORIENTED_EDGE('',*,*,#17451,.T.);
#24518=ORIENTED_EDGE('',*,*,#17452,.F.);
#24519=ORIENTED_EDGE('',*,*,#17217,.F.);
#24520=ORIENTED_EDGE('',*,*,#17453,.F.);
#24521=ORIENTED_EDGE('',*,*,#17454,.T.);
#24522=ORIENTED_EDGE('',*,*,#17455,.F.);
#24523=ORIENTED_EDGE('',*,*,#17220,.F.);
#24524=ORIENTED_EDGE('',*,*,#17456,.F.);
#24525=ORIENTED_EDGE('',*,*,#17457,.T.);
#24526=ORIENTED_EDGE('',*,*,#17458,.F.);
#24527=ORIENTED_EDGE('',*,*,#17223,.F.);
#24528=ORIENTED_EDGE('',*,*,#17459,.F.);
#24529=ORIENTED_EDGE('',*,*,#17460,.T.);
#24530=ORIENTED_EDGE('',*,*,#17461,.F.);
#24531=ORIENTED_EDGE('',*,*,#17226,.F.);
#24532=ORIENTED_EDGE('',*,*,#17462,.F.);
#24533=ORIENTED_EDGE('',*,*,#17463,.T.);
#24534=ORIENTED_EDGE('',*,*,#17464,.F.);
#24535=ORIENTED_EDGE('',*,*,#17229,.F.);
#24536=ORIENTED_EDGE('',*,*,#17465,.F.);
#24537=ORIENTED_EDGE('',*,*,#17466,.T.);
#24538=ORIENTED_EDGE('',*,*,#17467,.F.);
#24539=ORIENTED_EDGE('',*,*,#17232,.F.);
#24540=ORIENTED_EDGE('',*,*,#17468,.F.);
#24541=ORIENTED_EDGE('',*,*,#17469,.T.);
#24542=ORIENTED_EDGE('',*,*,#17470,.F.);
#24543=ORIENTED_EDGE('',*,*,#17235,.F.);
#24544=ORIENTED_EDGE('',*,*,#17471,.F.);
#24545=ORIENTED_EDGE('',*,*,#17472,.T.);
#24546=ORIENTED_EDGE('',*,*,#17473,.F.);
#24547=ORIENTED_EDGE('',*,*,#17238,.F.);
#24548=ORIENTED_EDGE('',*,*,#17474,.F.);
#24549=ORIENTED_EDGE('',*,*,#17475,.T.);
#24550=ORIENTED_EDGE('',*,*,#17476,.F.);
#24551=ORIENTED_EDGE('',*,*,#17241,.F.);
#24552=ORIENTED_EDGE('',*,*,#17477,.F.);
#24553=ORIENTED_EDGE('',*,*,#17478,.T.);
#24554=ORIENTED_EDGE('',*,*,#17479,.F.);
#24555=ORIENTED_EDGE('',*,*,#17244,.F.);
#24556=ORIENTED_EDGE('',*,*,#17480,.F.);
#24557=ORIENTED_EDGE('',*,*,#17481,.T.);
#24558=ORIENTED_EDGE('',*,*,#17482,.F.);
#24559=ORIENTED_EDGE('',*,*,#17247,.F.);
#24560=ORIENTED_EDGE('',*,*,#17483,.F.);
#24561=ORIENTED_EDGE('',*,*,#17484,.T.);
#24562=ORIENTED_EDGE('',*,*,#17485,.F.);
#24563=ORIENTED_EDGE('',*,*,#17250,.F.);
#24564=ORIENTED_EDGE('',*,*,#17486,.F.);
#24565=ORIENTED_EDGE('',*,*,#17487,.T.);
#24566=ORIENTED_EDGE('',*,*,#17488,.F.);
#24567=ORIENTED_EDGE('',*,*,#17253,.F.);
#24568=ORIENTED_EDGE('',*,*,#17489,.F.);
#24569=ORIENTED_EDGE('',*,*,#17490,.T.);
#24570=ORIENTED_EDGE('',*,*,#17491,.F.);
#24571=ORIENTED_EDGE('',*,*,#17256,.F.);
#24572=ORIENTED_EDGE('',*,*,#17492,.F.);
#24573=ORIENTED_EDGE('',*,*,#17493,.T.);
#24574=ORIENTED_EDGE('',*,*,#17494,.F.);
#24575=ORIENTED_EDGE('',*,*,#17259,.F.);
#24576=ORIENTED_EDGE('',*,*,#17495,.F.);
#24577=ORIENTED_EDGE('',*,*,#17496,.T.);
#24578=ORIENTED_EDGE('',*,*,#17497,.F.);
#24579=ORIENTED_EDGE('',*,*,#17262,.F.);
#24580=ORIENTED_EDGE('',*,*,#17498,.F.);
#24581=ORIENTED_EDGE('',*,*,#17499,.T.);
#24582=ORIENTED_EDGE('',*,*,#17500,.F.);
#24583=ORIENTED_EDGE('',*,*,#17265,.F.);
#24584=ORIENTED_EDGE('',*,*,#17501,.F.);
#24585=ORIENTED_EDGE('',*,*,#17502,.T.);
#24586=ORIENTED_EDGE('',*,*,#17503,.F.);
#24587=ORIENTED_EDGE('',*,*,#17268,.F.);
#24588=ORIENTED_EDGE('',*,*,#17504,.F.);
#24589=ORIENTED_EDGE('',*,*,#17505,.T.);
#24590=ORIENTED_EDGE('',*,*,#17506,.F.);
#24591=ORIENTED_EDGE('',*,*,#17271,.F.);
#24592=ORIENTED_EDGE('',*,*,#17507,.F.);
#24593=ORIENTED_EDGE('',*,*,#17508,.T.);
#24594=ORIENTED_EDGE('',*,*,#17509,.F.);
#24595=ORIENTED_EDGE('',*,*,#17274,.F.);
#24596=ORIENTED_EDGE('',*,*,#17510,.F.);
#24597=ORIENTED_EDGE('',*,*,#17511,.T.);
#24598=ORIENTED_EDGE('',*,*,#17512,.F.);
#24599=ORIENTED_EDGE('',*,*,#17277,.F.);
#24600=ORIENTED_EDGE('',*,*,#17513,.F.);
#24601=ORIENTED_EDGE('',*,*,#17514,.T.);
#24602=ORIENTED_EDGE('',*,*,#17515,.F.);
#24603=ORIENTED_EDGE('',*,*,#17280,.F.);
#24604=ORIENTED_EDGE('',*,*,#17516,.F.);
#24605=ORIENTED_EDGE('',*,*,#17517,.T.);
#24606=ORIENTED_EDGE('',*,*,#17518,.F.);
#24607=ORIENTED_EDGE('',*,*,#17283,.F.);
#24608=ORIENTED_EDGE('',*,*,#17519,.F.);
#24609=ORIENTED_EDGE('',*,*,#17520,.T.);
#24610=ORIENTED_EDGE('',*,*,#17521,.F.);
#24611=ORIENTED_EDGE('',*,*,#17286,.F.);
#24612=ORIENTED_EDGE('',*,*,#17522,.F.);
#24613=ORIENTED_EDGE('',*,*,#17523,.T.);
#24614=ORIENTED_EDGE('',*,*,#17524,.F.);
#24615=ORIENTED_EDGE('',*,*,#17289,.F.);
#24616=ORIENTED_EDGE('',*,*,#17525,.F.);
#24617=ORIENTED_EDGE('',*,*,#17526,.T.);
#24618=ORIENTED_EDGE('',*,*,#17527,.F.);
#24619=ORIENTED_EDGE('',*,*,#17292,.F.);
#24620=ORIENTED_EDGE('',*,*,#17528,.F.);
#24621=ORIENTED_EDGE('',*,*,#17529,.T.);
#24622=ORIENTED_EDGE('',*,*,#17530,.F.);
#24623=ORIENTED_EDGE('',*,*,#17295,.F.);
#24624=ORIENTED_EDGE('',*,*,#17531,.F.);
#24625=ORIENTED_EDGE('',*,*,#17532,.T.);
#24626=ORIENTED_EDGE('',*,*,#17533,.F.);
#24627=ORIENTED_EDGE('',*,*,#17298,.F.);
#24628=ORIENTED_EDGE('',*,*,#17534,.F.);
#24629=ORIENTED_EDGE('',*,*,#17535,.T.);
#24630=ORIENTED_EDGE('',*,*,#17536,.F.);
#24631=ORIENTED_EDGE('',*,*,#17301,.F.);
#24632=ORIENTED_EDGE('',*,*,#17537,.F.);
#24633=ORIENTED_EDGE('',*,*,#17538,.T.);
#24634=ORIENTED_EDGE('',*,*,#17539,.F.);
#24635=ORIENTED_EDGE('',*,*,#17304,.F.);
#24636=ORIENTED_EDGE('',*,*,#17540,.F.);
#24637=ORIENTED_EDGE('',*,*,#17541,.T.);
#24638=ORIENTED_EDGE('',*,*,#17542,.F.);
#24639=ORIENTED_EDGE('',*,*,#17307,.F.);
#24640=ORIENTED_EDGE('',*,*,#17543,.F.);
#24641=ORIENTED_EDGE('',*,*,#17544,.T.);
#24642=ORIENTED_EDGE('',*,*,#17545,.F.);
#24643=ORIENTED_EDGE('',*,*,#17310,.F.);
#24644=ORIENTED_EDGE('',*,*,#17546,.F.);
#24645=ORIENTED_EDGE('',*,*,#17547,.T.);
#24646=ORIENTED_EDGE('',*,*,#17548,.F.);
#24647=ORIENTED_EDGE('',*,*,#17313,.F.);
#24648=ORIENTED_EDGE('',*,*,#17549,.F.);
#24649=ORIENTED_EDGE('',*,*,#17550,.T.);
#24650=ORIENTED_EDGE('',*,*,#17551,.F.);
#24651=ORIENTED_EDGE('',*,*,#17316,.F.);
#24652=ORIENTED_EDGE('',*,*,#17552,.F.);
#24653=ORIENTED_EDGE('',*,*,#17553,.T.);
#24654=ORIENTED_EDGE('',*,*,#17554,.F.);
#24655=ORIENTED_EDGE('',*,*,#17555,.T.);
#24656=ORIENTED_EDGE('',*,*,#17556,.F.);
#24657=ORIENTED_EDGE('',*,*,#17318,.F.);
#24658=ORIENTED_EDGE('',*,*,#17557,.F.);
#24659=ORIENTED_EDGE('',*,*,#17558,.T.);
#24660=ORIENTED_EDGE('',*,*,#17559,.F.);
#24661=ORIENTED_EDGE('',*,*,#17321,.F.);
#24662=ORIENTED_EDGE('',*,*,#17560,.F.);
#24663=ORIENTED_EDGE('',*,*,#17561,.T.);
#24664=ORIENTED_EDGE('',*,*,#17562,.F.);
#24665=ORIENTED_EDGE('',*,*,#17324,.F.);
#24666=ORIENTED_EDGE('',*,*,#17563,.F.);
#24667=ORIENTED_EDGE('',*,*,#17564,.T.);
#24668=ORIENTED_EDGE('',*,*,#17565,.F.);
#24669=ORIENTED_EDGE('',*,*,#17327,.F.);
#24670=ORIENTED_EDGE('',*,*,#17566,.F.);
#24671=ORIENTED_EDGE('',*,*,#17567,.T.);
#24672=ORIENTED_EDGE('',*,*,#17568,.F.);
#24673=ORIENTED_EDGE('',*,*,#17330,.F.);
#24674=ORIENTED_EDGE('',*,*,#17569,.F.);
#24675=ORIENTED_EDGE('',*,*,#17570,.T.);
#24676=ORIENTED_EDGE('',*,*,#17571,.F.);
#24677=ORIENTED_EDGE('',*,*,#17333,.F.);
#24678=ORIENTED_EDGE('',*,*,#17572,.F.);
#24679=ORIENTED_EDGE('',*,*,#17573,.T.);
#24680=ORIENTED_EDGE('',*,*,#17574,.F.);
#24681=ORIENTED_EDGE('',*,*,#17336,.F.);
#24682=ORIENTED_EDGE('',*,*,#17575,.F.);
#24683=ORIENTED_EDGE('',*,*,#17576,.T.);
#24684=ORIENTED_EDGE('',*,*,#17577,.F.);
#24685=ORIENTED_EDGE('',*,*,#17339,.F.);
#24686=ORIENTED_EDGE('',*,*,#17578,.F.);
#24687=ORIENTED_EDGE('',*,*,#17579,.T.);
#24688=ORIENTED_EDGE('',*,*,#17580,.F.);
#24689=ORIENTED_EDGE('',*,*,#17342,.F.);
#24690=ORIENTED_EDGE('',*,*,#17581,.F.);
#24691=ORIENTED_EDGE('',*,*,#17582,.T.);
#24692=ORIENTED_EDGE('',*,*,#17583,.F.);
#24693=ORIENTED_EDGE('',*,*,#17345,.F.);
#24694=ORIENTED_EDGE('',*,*,#17584,.F.);
#24695=ORIENTED_EDGE('',*,*,#17585,.T.);
#24696=ORIENTED_EDGE('',*,*,#17586,.F.);
#24697=ORIENTED_EDGE('',*,*,#17348,.F.);
#24698=ORIENTED_EDGE('',*,*,#17587,.F.);
#24699=ORIENTED_EDGE('',*,*,#17588,.T.);
#24700=ORIENTED_EDGE('',*,*,#17589,.F.);
#24701=ORIENTED_EDGE('',*,*,#17351,.F.);
#24702=ORIENTED_EDGE('',*,*,#17590,.F.);
#24703=ORIENTED_EDGE('',*,*,#17591,.T.);
#24704=ORIENTED_EDGE('',*,*,#17592,.F.);
#24705=ORIENTED_EDGE('',*,*,#17354,.F.);
#24706=ORIENTED_EDGE('',*,*,#17593,.F.);
#24707=ORIENTED_EDGE('',*,*,#17594,.T.);
#24708=ORIENTED_EDGE('',*,*,#17595,.F.);
#24709=ORIENTED_EDGE('',*,*,#17357,.F.);
#24710=ORIENTED_EDGE('',*,*,#17596,.F.);
#24711=ORIENTED_EDGE('',*,*,#17361,.F.);
#24712=ORIENTED_EDGE('',*,*,#17597,.F.);
#24713=ORIENTED_EDGE('',*,*,#17598,.T.);
#24714=ORIENTED_EDGE('',*,*,#17599,.F.);
#24715=ORIENTED_EDGE('',*,*,#16710,.T.);
#24716=ORIENTED_EDGE('',*,*,#17600,.F.);
#24717=ORIENTED_EDGE('',*,*,#17363,.F.);
#24718=ORIENTED_EDGE('',*,*,#17601,.F.);
#24719=ORIENTED_EDGE('',*,*,#17367,.F.);
#24720=ORIENTED_EDGE('',*,*,#17602,.F.);
#24721=ORIENTED_EDGE('',*,*,#16713,.T.);
#24722=ORIENTED_EDGE('',*,*,#17603,.F.);
#24723=ORIENTED_EDGE('',*,*,#17370,.F.);
#24724=ORIENTED_EDGE('',*,*,#17604,.F.);
#24725=ORIENTED_EDGE('',*,*,#16716,.T.);
#24726=ORIENTED_EDGE('',*,*,#17605,.F.);
#24727=ORIENTED_EDGE('',*,*,#17373,.F.);
#24728=ORIENTED_EDGE('',*,*,#17606,.F.);
#24729=ORIENTED_EDGE('',*,*,#16719,.T.);
#24730=ORIENTED_EDGE('',*,*,#17607,.F.);
#24731=ORIENTED_EDGE('',*,*,#17376,.F.);
#24732=ORIENTED_EDGE('',*,*,#17608,.F.);
#24733=ORIENTED_EDGE('',*,*,#16722,.T.);
#24734=ORIENTED_EDGE('',*,*,#17609,.F.);
#24735=ORIENTED_EDGE('',*,*,#17379,.F.);
#24736=ORIENTED_EDGE('',*,*,#17610,.F.);
#24737=ORIENTED_EDGE('',*,*,#16725,.T.);
#24738=ORIENTED_EDGE('',*,*,#17611,.F.);
#24739=ORIENTED_EDGE('',*,*,#17382,.F.);
#24740=ORIENTED_EDGE('',*,*,#17612,.F.);
#24741=ORIENTED_EDGE('',*,*,#16728,.T.);
#24742=ORIENTED_EDGE('',*,*,#17613,.F.);
#24743=ORIENTED_EDGE('',*,*,#17385,.F.);
#24744=ORIENTED_EDGE('',*,*,#17614,.F.);
#24745=ORIENTED_EDGE('',*,*,#16732,.T.);
#24746=ORIENTED_EDGE('',*,*,#17615,.F.);
#24747=ORIENTED_EDGE('',*,*,#17388,.F.);
#24748=ORIENTED_EDGE('',*,*,#17616,.F.);
#24749=ORIENTED_EDGE('',*,*,#16736,.T.);
#24750=ORIENTED_EDGE('',*,*,#17617,.F.);
#24751=ORIENTED_EDGE('',*,*,#17391,.F.);
#24752=ORIENTED_EDGE('',*,*,#17618,.F.);
#24753=ORIENTED_EDGE('',*,*,#16740,.T.);
#24754=ORIENTED_EDGE('',*,*,#17619,.F.);
#24755=ORIENTED_EDGE('',*,*,#17394,.F.);
#24756=ORIENTED_EDGE('',*,*,#17620,.F.);
#24757=ORIENTED_EDGE('',*,*,#16744,.T.);
#24758=ORIENTED_EDGE('',*,*,#17621,.F.);
#24759=ORIENTED_EDGE('',*,*,#17397,.F.);
#24760=ORIENTED_EDGE('',*,*,#17622,.F.);
#24761=ORIENTED_EDGE('',*,*,#16748,.T.);
#24762=ORIENTED_EDGE('',*,*,#17623,.F.);
#24763=ORIENTED_EDGE('',*,*,#17400,.F.);
#24764=ORIENTED_EDGE('',*,*,#17624,.F.);
#24765=ORIENTED_EDGE('',*,*,#16752,.T.);
#24766=ORIENTED_EDGE('',*,*,#17625,.F.);
#24767=ORIENTED_EDGE('',*,*,#17403,.F.);
#24768=ORIENTED_EDGE('',*,*,#17626,.F.);
#24769=ORIENTED_EDGE('',*,*,#16756,.T.);
#24770=ORIENTED_EDGE('',*,*,#17627,.F.);
#24771=ORIENTED_EDGE('',*,*,#17406,.F.);
#24772=ORIENTED_EDGE('',*,*,#17628,.F.);
#24773=ORIENTED_EDGE('',*,*,#16760,.T.);
#24774=ORIENTED_EDGE('',*,*,#17629,.F.);
#24775=ORIENTED_EDGE('',*,*,#17409,.F.);
#24776=ORIENTED_EDGE('',*,*,#17630,.F.);
#24777=ORIENTED_EDGE('',*,*,#16764,.T.);
#24778=ORIENTED_EDGE('',*,*,#17631,.F.);
#24779=ORIENTED_EDGE('',*,*,#17412,.F.);
#24780=ORIENTED_EDGE('',*,*,#17632,.F.);
#24781=ORIENTED_EDGE('',*,*,#16768,.T.);
#24782=ORIENTED_EDGE('',*,*,#17633,.F.);
#24783=ORIENTED_EDGE('',*,*,#17415,.F.);
#24784=ORIENTED_EDGE('',*,*,#17634,.F.);
#24785=ORIENTED_EDGE('',*,*,#16772,.T.);
#24786=ORIENTED_EDGE('',*,*,#17635,.F.);
#24787=ORIENTED_EDGE('',*,*,#17418,.F.);
#24788=ORIENTED_EDGE('',*,*,#17636,.F.);
#24789=ORIENTED_EDGE('',*,*,#16776,.T.);
#24790=ORIENTED_EDGE('',*,*,#17637,.F.);
#24791=ORIENTED_EDGE('',*,*,#17421,.F.);
#24792=ORIENTED_EDGE('',*,*,#17638,.F.);
#24793=ORIENTED_EDGE('',*,*,#16780,.T.);
#24794=ORIENTED_EDGE('',*,*,#17639,.F.);
#24795=ORIENTED_EDGE('',*,*,#17424,.F.);
#24796=ORIENTED_EDGE('',*,*,#17640,.F.);
#24797=ORIENTED_EDGE('',*,*,#16784,.T.);
#24798=ORIENTED_EDGE('',*,*,#17641,.F.);
#24799=ORIENTED_EDGE('',*,*,#17427,.F.);
#24800=ORIENTED_EDGE('',*,*,#17642,.F.);
#24801=ORIENTED_EDGE('',*,*,#16788,.T.);
#24802=ORIENTED_EDGE('',*,*,#17643,.F.);
#24803=ORIENTED_EDGE('',*,*,#17430,.F.);
#24804=ORIENTED_EDGE('',*,*,#17644,.F.);
#24805=ORIENTED_EDGE('',*,*,#16792,.T.);
#24806=ORIENTED_EDGE('',*,*,#17645,.F.);
#24807=ORIENTED_EDGE('',*,*,#17433,.F.);
#24808=ORIENTED_EDGE('',*,*,#17646,.F.);
#24809=ORIENTED_EDGE('',*,*,#16796,.T.);
#24810=ORIENTED_EDGE('',*,*,#17647,.F.);
#24811=ORIENTED_EDGE('',*,*,#17436,.F.);
#24812=ORIENTED_EDGE('',*,*,#17648,.F.);
#24813=ORIENTED_EDGE('',*,*,#16800,.T.);
#24814=ORIENTED_EDGE('',*,*,#17649,.F.);
#24815=ORIENTED_EDGE('',*,*,#17439,.F.);
#24816=ORIENTED_EDGE('',*,*,#17650,.F.);
#24817=ORIENTED_EDGE('',*,*,#16804,.T.);
#24818=ORIENTED_EDGE('',*,*,#17651,.F.);
#24819=ORIENTED_EDGE('',*,*,#17442,.F.);
#24820=ORIENTED_EDGE('',*,*,#17652,.F.);
#24821=ORIENTED_EDGE('',*,*,#16503,.T.);
#24822=ORIENTED_EDGE('',*,*,#17653,.F.);
#24823=ORIENTED_EDGE('',*,*,#17445,.F.);
#24824=ORIENTED_EDGE('',*,*,#17654,.F.);
#24825=ORIENTED_EDGE('',*,*,#16507,.T.);
#24826=ORIENTED_EDGE('',*,*,#17655,.F.);
#24827=ORIENTED_EDGE('',*,*,#17448,.F.);
#24828=ORIENTED_EDGE('',*,*,#17656,.F.);
#24829=ORIENTED_EDGE('',*,*,#16511,.T.);
#24830=ORIENTED_EDGE('',*,*,#17657,.F.);
#24831=ORIENTED_EDGE('',*,*,#17451,.F.);
#24832=ORIENTED_EDGE('',*,*,#17658,.F.);
#24833=ORIENTED_EDGE('',*,*,#16515,.T.);
#24834=ORIENTED_EDGE('',*,*,#17659,.F.);
#24835=ORIENTED_EDGE('',*,*,#17454,.F.);
#24836=ORIENTED_EDGE('',*,*,#17660,.F.);
#24837=ORIENTED_EDGE('',*,*,#16519,.T.);
#24838=ORIENTED_EDGE('',*,*,#17661,.F.);
#24839=ORIENTED_EDGE('',*,*,#17457,.F.);
#24840=ORIENTED_EDGE('',*,*,#17662,.F.);
#24841=ORIENTED_EDGE('',*,*,#16523,.T.);
#24842=ORIENTED_EDGE('',*,*,#17663,.F.);
#24843=ORIENTED_EDGE('',*,*,#17460,.F.);
#24844=ORIENTED_EDGE('',*,*,#17664,.F.);
#24845=ORIENTED_EDGE('',*,*,#16527,.T.);
#24846=ORIENTED_EDGE('',*,*,#17665,.F.);
#24847=ORIENTED_EDGE('',*,*,#17463,.F.);
#24848=ORIENTED_EDGE('',*,*,#17666,.F.);
#24849=ORIENTED_EDGE('',*,*,#16531,.T.);
#24850=ORIENTED_EDGE('',*,*,#17667,.F.);
#24851=ORIENTED_EDGE('',*,*,#17466,.F.);
#24852=ORIENTED_EDGE('',*,*,#17668,.F.);
#24853=ORIENTED_EDGE('',*,*,#16535,.T.);
#24854=ORIENTED_EDGE('',*,*,#17669,.F.);
#24855=ORIENTED_EDGE('',*,*,#17469,.F.);
#24856=ORIENTED_EDGE('',*,*,#17670,.F.);
#24857=ORIENTED_EDGE('',*,*,#16539,.T.);
#24858=ORIENTED_EDGE('',*,*,#17671,.F.);
#24859=ORIENTED_EDGE('',*,*,#17472,.F.);
#24860=ORIENTED_EDGE('',*,*,#17672,.F.);
#24861=ORIENTED_EDGE('',*,*,#16543,.T.);
#24862=ORIENTED_EDGE('',*,*,#17673,.F.);
#24863=ORIENTED_EDGE('',*,*,#17475,.F.);
#24864=ORIENTED_EDGE('',*,*,#17674,.F.);
#24865=ORIENTED_EDGE('',*,*,#16547,.T.);
#24866=ORIENTED_EDGE('',*,*,#17675,.F.);
#24867=ORIENTED_EDGE('',*,*,#17478,.F.);
#24868=ORIENTED_EDGE('',*,*,#17676,.F.);
#24869=ORIENTED_EDGE('',*,*,#16551,.T.);
#24870=ORIENTED_EDGE('',*,*,#17677,.F.);
#24871=ORIENTED_EDGE('',*,*,#17481,.F.);
#24872=ORIENTED_EDGE('',*,*,#17678,.F.);
#24873=ORIENTED_EDGE('',*,*,#16555,.T.);
#24874=ORIENTED_EDGE('',*,*,#17679,.F.);
#24875=ORIENTED_EDGE('',*,*,#17484,.F.);
#24876=ORIENTED_EDGE('',*,*,#17680,.F.);
#24877=ORIENTED_EDGE('',*,*,#16559,.T.);
#24878=ORIENTED_EDGE('',*,*,#17681,.F.);
#24879=ORIENTED_EDGE('',*,*,#17487,.F.);
#24880=ORIENTED_EDGE('',*,*,#17682,.F.);
#24881=ORIENTED_EDGE('',*,*,#16563,.T.);
#24882=ORIENTED_EDGE('',*,*,#17683,.F.);
#24883=ORIENTED_EDGE('',*,*,#17490,.F.);
#24884=ORIENTED_EDGE('',*,*,#17684,.F.);
#24885=ORIENTED_EDGE('',*,*,#16567,.T.);
#24886=ORIENTED_EDGE('',*,*,#17685,.F.);
#24887=ORIENTED_EDGE('',*,*,#17493,.F.);
#24888=ORIENTED_EDGE('',*,*,#17686,.F.);
#24889=ORIENTED_EDGE('',*,*,#16571,.T.);
#24890=ORIENTED_EDGE('',*,*,#17687,.F.);
#24891=ORIENTED_EDGE('',*,*,#17496,.F.);
#24892=ORIENTED_EDGE('',*,*,#17688,.F.);
#24893=ORIENTED_EDGE('',*,*,#16575,.T.);
#24894=ORIENTED_EDGE('',*,*,#17689,.F.);
#24895=ORIENTED_EDGE('',*,*,#17499,.F.);
#24896=ORIENTED_EDGE('',*,*,#17690,.F.);
#24897=ORIENTED_EDGE('',*,*,#16579,.T.);
#24898=ORIENTED_EDGE('',*,*,#17691,.F.);
#24899=ORIENTED_EDGE('',*,*,#17502,.F.);
#24900=ORIENTED_EDGE('',*,*,#17692,.F.);
#24901=ORIENTED_EDGE('',*,*,#16583,.T.);
#24902=ORIENTED_EDGE('',*,*,#17693,.F.);
#24903=ORIENTED_EDGE('',*,*,#17505,.F.);
#24904=ORIENTED_EDGE('',*,*,#17694,.F.);
#24905=ORIENTED_EDGE('',*,*,#16587,.T.);
#24906=ORIENTED_EDGE('',*,*,#17695,.F.);
#24907=ORIENTED_EDGE('',*,*,#17508,.F.);
#24908=ORIENTED_EDGE('',*,*,#17696,.F.);
#24909=ORIENTED_EDGE('',*,*,#16591,.T.);
#24910=ORIENTED_EDGE('',*,*,#17697,.F.);
#24911=ORIENTED_EDGE('',*,*,#17511,.F.);
#24912=ORIENTED_EDGE('',*,*,#17698,.F.);
#24913=ORIENTED_EDGE('',*,*,#16595,.T.);
#24914=ORIENTED_EDGE('',*,*,#17699,.F.);
#24915=ORIENTED_EDGE('',*,*,#17514,.F.);
#24916=ORIENTED_EDGE('',*,*,#17700,.F.);
#24917=ORIENTED_EDGE('',*,*,#16599,.T.);
#24918=ORIENTED_EDGE('',*,*,#17701,.F.);
#24919=ORIENTED_EDGE('',*,*,#17517,.F.);
#24920=ORIENTED_EDGE('',*,*,#17702,.F.);
#24921=ORIENTED_EDGE('',*,*,#16603,.T.);
#24922=ORIENTED_EDGE('',*,*,#17703,.F.);
#24923=ORIENTED_EDGE('',*,*,#17520,.F.);
#24924=ORIENTED_EDGE('',*,*,#17704,.F.);
#24925=ORIENTED_EDGE('',*,*,#16607,.T.);
#24926=ORIENTED_EDGE('',*,*,#17705,.F.);
#24927=ORIENTED_EDGE('',*,*,#17523,.F.);
#24928=ORIENTED_EDGE('',*,*,#17706,.F.);
#24929=ORIENTED_EDGE('',*,*,#16611,.T.);
#24930=ORIENTED_EDGE('',*,*,#17707,.F.);
#24931=ORIENTED_EDGE('',*,*,#17526,.F.);
#24932=ORIENTED_EDGE('',*,*,#17708,.F.);
#24933=ORIENTED_EDGE('',*,*,#16615,.T.);
#24934=ORIENTED_EDGE('',*,*,#17709,.F.);
#24935=ORIENTED_EDGE('',*,*,#17529,.F.);
#24936=ORIENTED_EDGE('',*,*,#17710,.F.);
#24937=ORIENTED_EDGE('',*,*,#16619,.T.);
#24938=ORIENTED_EDGE('',*,*,#17711,.F.);
#24939=ORIENTED_EDGE('',*,*,#17532,.F.);
#24940=ORIENTED_EDGE('',*,*,#17712,.F.);
#24941=ORIENTED_EDGE('',*,*,#16623,.T.);
#24942=ORIENTED_EDGE('',*,*,#17713,.F.);
#24943=ORIENTED_EDGE('',*,*,#17535,.F.);
#24944=ORIENTED_EDGE('',*,*,#17714,.F.);
#24945=ORIENTED_EDGE('',*,*,#16627,.T.);
#24946=ORIENTED_EDGE('',*,*,#17715,.F.);
#24947=ORIENTED_EDGE('',*,*,#17538,.F.);
#24948=ORIENTED_EDGE('',*,*,#17716,.F.);
#24949=ORIENTED_EDGE('',*,*,#16631,.T.);
#24950=ORIENTED_EDGE('',*,*,#17717,.F.);
#24951=ORIENTED_EDGE('',*,*,#17541,.F.);
#24952=ORIENTED_EDGE('',*,*,#17718,.F.);
#24953=ORIENTED_EDGE('',*,*,#16635,.T.);
#24954=ORIENTED_EDGE('',*,*,#17719,.F.);
#24955=ORIENTED_EDGE('',*,*,#17544,.F.);
#24956=ORIENTED_EDGE('',*,*,#17720,.F.);
#24957=ORIENTED_EDGE('',*,*,#16639,.T.);
#24958=ORIENTED_EDGE('',*,*,#17721,.F.);
#24959=ORIENTED_EDGE('',*,*,#17547,.F.);
#24960=ORIENTED_EDGE('',*,*,#17722,.F.);
#24961=ORIENTED_EDGE('',*,*,#16643,.T.);
#24962=ORIENTED_EDGE('',*,*,#17723,.F.);
#24963=ORIENTED_EDGE('',*,*,#17550,.F.);
#24964=ORIENTED_EDGE('',*,*,#17724,.F.);
#24965=ORIENTED_EDGE('',*,*,#16647,.T.);
#24966=ORIENTED_EDGE('',*,*,#17725,.F.);
#24967=ORIENTED_EDGE('',*,*,#17553,.F.);
#24968=ORIENTED_EDGE('',*,*,#17726,.F.);
#24969=ORIENTED_EDGE('',*,*,#16651,.T.);
#24970=ORIENTED_EDGE('',*,*,#17727,.F.);
#24971=ORIENTED_EDGE('',*,*,#16707,.T.);
#24972=ORIENTED_EDGE('',*,*,#17728,.F.);
#24973=ORIENTED_EDGE('',*,*,#17555,.F.);
#24974=ORIENTED_EDGE('',*,*,#17729,.F.);
#24975=ORIENTED_EDGE('',*,*,#16704,.T.);
#24976=ORIENTED_EDGE('',*,*,#17730,.F.);
#24977=ORIENTED_EDGE('',*,*,#17558,.F.);
#24978=ORIENTED_EDGE('',*,*,#17731,.F.);
#24979=ORIENTED_EDGE('',*,*,#16701,.T.);
#24980=ORIENTED_EDGE('',*,*,#17732,.F.);
#24981=ORIENTED_EDGE('',*,*,#17561,.F.);
#24982=ORIENTED_EDGE('',*,*,#17733,.F.);
#24983=ORIENTED_EDGE('',*,*,#16698,.T.);
#24984=ORIENTED_EDGE('',*,*,#17734,.F.);
#24985=ORIENTED_EDGE('',*,*,#17564,.F.);
#24986=ORIENTED_EDGE('',*,*,#17735,.F.);
#24987=ORIENTED_EDGE('',*,*,#16695,.T.);
#24988=ORIENTED_EDGE('',*,*,#17736,.F.);
#24989=ORIENTED_EDGE('',*,*,#17567,.F.);
#24990=ORIENTED_EDGE('',*,*,#17737,.F.);
#24991=ORIENTED_EDGE('',*,*,#16692,.T.);
#24992=ORIENTED_EDGE('',*,*,#17738,.F.);
#24993=ORIENTED_EDGE('',*,*,#17570,.F.);
#24994=ORIENTED_EDGE('',*,*,#17739,.F.);
#24995=ORIENTED_EDGE('',*,*,#16689,.T.);
#24996=ORIENTED_EDGE('',*,*,#17740,.F.);
#24997=ORIENTED_EDGE('',*,*,#17573,.F.);
#24998=ORIENTED_EDGE('',*,*,#17741,.F.);
#24999=ORIENTED_EDGE('',*,*,#16686,.T.);
#25000=ORIENTED_EDGE('',*,*,#17742,.F.);
#25001=ORIENTED_EDGE('',*,*,#17576,.F.);
#25002=ORIENTED_EDGE('',*,*,#17743,.F.);
#25003=ORIENTED_EDGE('',*,*,#16683,.T.);
#25004=ORIENTED_EDGE('',*,*,#17744,.F.);
#25005=ORIENTED_EDGE('',*,*,#17579,.F.);
#25006=ORIENTED_EDGE('',*,*,#17745,.F.);
#25007=ORIENTED_EDGE('',*,*,#16679,.T.);
#25008=ORIENTED_EDGE('',*,*,#17746,.F.);
#25009=ORIENTED_EDGE('',*,*,#17582,.F.);
#25010=ORIENTED_EDGE('',*,*,#17747,.F.);
#25011=ORIENTED_EDGE('',*,*,#16675,.T.);
#25012=ORIENTED_EDGE('',*,*,#17748,.F.);
#25013=ORIENTED_EDGE('',*,*,#17585,.F.);
#25014=ORIENTED_EDGE('',*,*,#17749,.F.);
#25015=ORIENTED_EDGE('',*,*,#16671,.T.);
#25016=ORIENTED_EDGE('',*,*,#17750,.F.);
#25017=ORIENTED_EDGE('',*,*,#17588,.F.);
#25018=ORIENTED_EDGE('',*,*,#17751,.F.);
#25019=ORIENTED_EDGE('',*,*,#16667,.T.);
#25020=ORIENTED_EDGE('',*,*,#17752,.F.);
#25021=ORIENTED_EDGE('',*,*,#17591,.F.);
#25022=ORIENTED_EDGE('',*,*,#17753,.F.);
#25023=ORIENTED_EDGE('',*,*,#16663,.T.);
#25024=ORIENTED_EDGE('',*,*,#17754,.F.);
#25025=ORIENTED_EDGE('',*,*,#17594,.F.);
#25026=ORIENTED_EDGE('',*,*,#17755,.F.);
#25027=ORIENTED_EDGE('',*,*,#17598,.F.);
#25028=ORIENTED_EDGE('',*,*,#17756,.F.);
#25029=ORIENTED_EDGE('',*,*,#16655,.T.);
#25030=ORIENTED_EDGE('',*,*,#16333,.T.);
#25031=ORIENTED_EDGE('',*,*,#16423,.T.);
#25032=ORIENTED_EDGE('',*,*,#16330,.T.);
#25033=ORIENTED_EDGE('',*,*,#17121,.T.);
#25034=ORIENTED_EDGE('',*,*,#17124,.F.);
#25035=ORIENTED_EDGE('',*,*,#17757,.F.);
#25036=ORIENTED_EDGE('',*,*,#16810,.F.);
#25037=ORIENTED_EDGE('',*,*,#17758,.F.);
#25038=ORIENTED_EDGE('',*,*,#17759,.T.);
#25039=ORIENTED_EDGE('',*,*,#17760,.F.);
#25040=ORIENTED_EDGE('',*,*,#17759,.F.);
#25041=ORIENTED_EDGE('',*,*,#17761,.F.);
#25042=ORIENTED_EDGE('',*,*,#17762,.T.);
#25043=ORIENTED_EDGE('',*,*,#17763,.F.);
#25044=ORIENTED_EDGE('',*,*,#17762,.F.);
#25045=ORIENTED_EDGE('',*,*,#17764,.F.);
#25046=ORIENTED_EDGE('',*,*,#16659,.T.);
#25047=ORIENTED_EDGE('',*,*,#16500,.F.);
#25048=ORIENTED_EDGE('',*,*,#16497,.F.);
#25049=ORIENTED_EDGE('',*,*,#17765,.T.);
#25050=ORIENTED_EDGE('',*,*,#17766,.T.);
#25051=ORIENTED_EDGE('',*,*,#17767,.T.);
#25052=ORIENTED_EDGE('',*,*,#17768,.T.);
#25053=ORIENTED_EDGE('',*,*,#17769,.T.);
#25054=ORIENTED_EDGE('',*,*,#17770,.T.);
#25055=ORIENTED_EDGE('',*,*,#17771,.T.);
#25056=ORIENTED_EDGE('',*,*,#16492,.T.);
#25057=ORIENTED_EDGE('',*,*,#17772,.F.);
#25058=ORIENTED_EDGE('',*,*,#17766,.F.);
#25059=ORIENTED_EDGE('',*,*,#17772,.T.);
#25060=ORIENTED_EDGE('',*,*,#16491,.T.);
#25061=ORIENTED_EDGE('',*,*,#17773,.F.);
#25062=ORIENTED_EDGE('',*,*,#17767,.F.);
#25063=ORIENTED_EDGE('',*,*,#17773,.T.);
#25064=ORIENTED_EDGE('',*,*,#16490,.T.);
#25065=ORIENTED_EDGE('',*,*,#17774,.F.);
#25066=ORIENTED_EDGE('',*,*,#17768,.F.);
#25067=ORIENTED_EDGE('',*,*,#17774,.T.);
#25068=ORIENTED_EDGE('',*,*,#16489,.T.);
#25069=ORIENTED_EDGE('',*,*,#16495,.T.);
#25070=ORIENTED_EDGE('',*,*,#17775,.F.);
#25071=ORIENTED_EDGE('',*,*,#17769,.F.);
#25072=ORIENTED_EDGE('',*,*,#17775,.T.);
#25073=ORIENTED_EDGE('',*,*,#16494,.T.);
#25074=ORIENTED_EDGE('',*,*,#17776,.F.);
#25075=ORIENTED_EDGE('',*,*,#17770,.F.);
#25076=ORIENTED_EDGE('',*,*,#17776,.T.);
#25077=ORIENTED_EDGE('',*,*,#16493,.T.);
#25078=ORIENTED_EDGE('',*,*,#17771,.F.);
#25079=ORIENTED_EDGE('',*,*,#17765,.F.);
#25080=ORIENTED_EDGE('',*,*,#17777,.F.);
#25081=ORIENTED_EDGE('',*,*,#16421,.F.);
#25082=ORIENTED_EDGE('',*,*,#16420,.F.);
#25083=ORIENTED_EDGE('',*,*,#16417,.F.);
#25084=ORIENTED_EDGE('',*,*,#16414,.F.);
#25085=ORIENTED_EDGE('',*,*,#16411,.F.);
#25086=ORIENTED_EDGE('',*,*,#16408,.F.);
#25087=ORIENTED_EDGE('',*,*,#16405,.F.);
#25088=ORIENTED_EDGE('',*,*,#16402,.F.);
#25089=ORIENTED_EDGE('',*,*,#16399,.F.);
#25090=ORIENTED_EDGE('',*,*,#16396,.F.);
#25091=ORIENTED_EDGE('',*,*,#16393,.F.);
#25092=ORIENTED_EDGE('',*,*,#16390,.F.);
#25093=ORIENTED_EDGE('',*,*,#16387,.F.);
#25094=ORIENTED_EDGE('',*,*,#16384,.F.);
#25095=ORIENTED_EDGE('',*,*,#16381,.F.);
#25096=ORIENTED_EDGE('',*,*,#16378,.F.);
#25097=ORIENTED_EDGE('',*,*,#16375,.F.);
#25098=ORIENTED_EDGE('',*,*,#16372,.F.);
#25099=ORIENTED_EDGE('',*,*,#16369,.F.);
#25100=ORIENTED_EDGE('',*,*,#16366,.F.);
#25101=ORIENTED_EDGE('',*,*,#16363,.F.);
#25102=ORIENTED_EDGE('',*,*,#16360,.F.);
#25103=ORIENTED_EDGE('',*,*,#16357,.F.);
#25104=ORIENTED_EDGE('',*,*,#16354,.F.);
#25105=ORIENTED_EDGE('',*,*,#16351,.F.);
#25106=ORIENTED_EDGE('',*,*,#16348,.F.);
#25107=ORIENTED_EDGE('',*,*,#16345,.F.);
#25108=ORIENTED_EDGE('',*,*,#16342,.F.);
#25109=ORIENTED_EDGE('',*,*,#16339,.F.);
#25110=ORIENTED_EDGE('',*,*,#16336,.F.);
#25111=ORIENTED_EDGE('',*,*,#16329,.F.);
#25112=ORIENTED_EDGE('',*,*,#16426,.F.);
#25113=ORIENTED_EDGE('',*,*,#16427,.T.);
#25114=ORIENTED_EDGE('',*,*,#16327,.T.);
#25115=ORIENTED_EDGE('',*,*,#16324,.T.);
#25116=ORIENTED_EDGE('',*,*,#16321,.T.);
#25117=ORIENTED_EDGE('',*,*,#16318,.T.);
#25118=ORIENTED_EDGE('',*,*,#16315,.T.);
#25119=ORIENTED_EDGE('',*,*,#16312,.T.);
#25120=ORIENTED_EDGE('',*,*,#16309,.T.);
#25121=ORIENTED_EDGE('',*,*,#16306,.T.);
#25122=ORIENTED_EDGE('',*,*,#16303,.T.);
#25123=ORIENTED_EDGE('',*,*,#16300,.T.);
#25124=ORIENTED_EDGE('',*,*,#16297,.T.);
#25125=ORIENTED_EDGE('',*,*,#16294,.T.);
#25126=ORIENTED_EDGE('',*,*,#16291,.T.);
#25127=ORIENTED_EDGE('',*,*,#16288,.T.);
#25128=ORIENTED_EDGE('',*,*,#16285,.T.);
#25129=ORIENTED_EDGE('',*,*,#16282,.T.);
#25130=ORIENTED_EDGE('',*,*,#16279,.T.);
#25131=ORIENTED_EDGE('',*,*,#16276,.T.);
#25132=ORIENTED_EDGE('',*,*,#16273,.T.);
#25133=ORIENTED_EDGE('',*,*,#16270,.T.);
#25134=ORIENTED_EDGE('',*,*,#16267,.T.);
#25135=ORIENTED_EDGE('',*,*,#16264,.T.);
#25136=ORIENTED_EDGE('',*,*,#16261,.T.);
#25137=ORIENTED_EDGE('',*,*,#16258,.T.);
#25138=ORIENTED_EDGE('',*,*,#16255,.T.);
#25139=ORIENTED_EDGE('',*,*,#16252,.T.);
#25140=ORIENTED_EDGE('',*,*,#16249,.T.);
#25141=ORIENTED_EDGE('',*,*,#16246,.T.);
#25142=ORIENTED_EDGE('',*,*,#17778,.F.);
#25143=ORIENTED_EDGE('',*,*,#16242,.T.);
#25144=ORIENTED_EDGE('',*,*,#16248,.T.);
#25145=ORIENTED_EDGE('',*,*,#16251,.T.);
#25146=ORIENTED_EDGE('',*,*,#16254,.T.);
#25147=ORIENTED_EDGE('',*,*,#16257,.T.);
#25148=ORIENTED_EDGE('',*,*,#16260,.T.);
#25149=ORIENTED_EDGE('',*,*,#16263,.T.);
#25150=ORIENTED_EDGE('',*,*,#16266,.T.);
#25151=ORIENTED_EDGE('',*,*,#16269,.T.);
#25152=ORIENTED_EDGE('',*,*,#16272,.T.);
#25153=ORIENTED_EDGE('',*,*,#16275,.T.);
#25154=ORIENTED_EDGE('',*,*,#16278,.T.);
#25155=ORIENTED_EDGE('',*,*,#16281,.T.);
#25156=ORIENTED_EDGE('',*,*,#16284,.T.);
#25157=ORIENTED_EDGE('',*,*,#16287,.T.);
#25158=ORIENTED_EDGE('',*,*,#16290,.T.);
#25159=ORIENTED_EDGE('',*,*,#16293,.T.);
#25160=ORIENTED_EDGE('',*,*,#16296,.T.);
#25161=ORIENTED_EDGE('',*,*,#16299,.T.);
#25162=ORIENTED_EDGE('',*,*,#16302,.T.);
#25163=ORIENTED_EDGE('',*,*,#16305,.T.);
#25164=ORIENTED_EDGE('',*,*,#16308,.T.);
#25165=ORIENTED_EDGE('',*,*,#16311,.T.);
#25166=ORIENTED_EDGE('',*,*,#16314,.T.);
#25167=ORIENTED_EDGE('',*,*,#16317,.T.);
#25168=ORIENTED_EDGE('',*,*,#16320,.T.);
#25169=ORIENTED_EDGE('',*,*,#16323,.T.);
#25170=ORIENTED_EDGE('',*,*,#16326,.T.);
#25171=ORIENTED_EDGE('',*,*,#16428,.T.);
#25172=ORIENTED_EDGE('',*,*,#16424,.F.);
#25173=ORIENTED_EDGE('',*,*,#16332,.T.);
#25174=ORIENTED_EDGE('',*,*,#16335,.T.);
#25175=ORIENTED_EDGE('',*,*,#16338,.T.);
#25176=ORIENTED_EDGE('',*,*,#16341,.T.);
#25177=ORIENTED_EDGE('',*,*,#16344,.T.);
#25178=ORIENTED_EDGE('',*,*,#16347,.T.);
#25179=ORIENTED_EDGE('',*,*,#16350,.T.);
#25180=ORIENTED_EDGE('',*,*,#16353,.T.);
#25181=ORIENTED_EDGE('',*,*,#16356,.T.);
#25182=ORIENTED_EDGE('',*,*,#16359,.T.);
#25183=ORIENTED_EDGE('',*,*,#16362,.T.);
#25184=ORIENTED_EDGE('',*,*,#16365,.T.);
#25185=ORIENTED_EDGE('',*,*,#16368,.T.);
#25186=ORIENTED_EDGE('',*,*,#16371,.T.);
#25187=ORIENTED_EDGE('',*,*,#16374,.T.);
#25188=ORIENTED_EDGE('',*,*,#16377,.T.);
#25189=ORIENTED_EDGE('',*,*,#16380,.T.);
#25190=ORIENTED_EDGE('',*,*,#16383,.T.);
#25191=ORIENTED_EDGE('',*,*,#16386,.T.);
#25192=ORIENTED_EDGE('',*,*,#16389,.T.);
#25193=ORIENTED_EDGE('',*,*,#16392,.T.);
#25194=ORIENTED_EDGE('',*,*,#16395,.T.);
#25195=ORIENTED_EDGE('',*,*,#16398,.T.);
#25196=ORIENTED_EDGE('',*,*,#16401,.T.);
#25197=ORIENTED_EDGE('',*,*,#16404,.T.);
#25198=ORIENTED_EDGE('',*,*,#16407,.T.);
#25199=ORIENTED_EDGE('',*,*,#16410,.T.);
#25200=ORIENTED_EDGE('',*,*,#16413,.T.);
#25201=ORIENTED_EDGE('',*,*,#16416,.T.);
#25202=ORIENTED_EDGE('',*,*,#16419,.T.);
#25203=ORIENTED_EDGE('',*,*,#16422,.T.);
#25204=ORIENTED_EDGE('',*,*,#17777,.T.);
#25205=ORIENTED_EDGE('',*,*,#16245,.T.);
#25206=ORIENTED_EDGE('',*,*,#17778,.T.);
#25207=ORIENTED_EDGE('',*,*,#16809,.T.);
#25208=ORIENTED_EDGE('',*,*,#17779,.T.);
#25209=ORIENTED_EDGE('',*,*,#16660,.T.);
#25210=ORIENTED_EDGE('',*,*,#17764,.T.);
#25211=ORIENTED_EDGE('',*,*,#17761,.T.);
#25212=ORIENTED_EDGE('',*,*,#17758,.T.);
#25213=ORIENTED_EDGE('',*,*,#16808,.T.);
#25214=ORIENTED_EDGE('',*,*,#17113,.T.);
#25215=ORIENTED_EDGE('',*,*,#17780,.T.);
#25216=ORIENTED_EDGE('',*,*,#16661,.T.);
#25217=ORIENTED_EDGE('',*,*,#17779,.F.);
#25218=ORIENTED_EDGE('',*,*,#17112,.T.);
#25219=ORIENTED_EDGE('',*,*,#17358,.T.);
#25220=ORIENTED_EDGE('',*,*,#17595,.T.);
#25221=ORIENTED_EDGE('',*,*,#17754,.T.);
#25222=ORIENTED_EDGE('',*,*,#16662,.T.);
#25223=ORIENTED_EDGE('',*,*,#17780,.F.);
#25224=ORIENTED_EDGE('',*,*,#16813,.T.);
#25225=ORIENTED_EDGE('',*,*,#17781,.T.);
#25226=ORIENTED_EDGE('',*,*,#16656,.T.);
#25227=ORIENTED_EDGE('',*,*,#17756,.T.);
#25228=ORIENTED_EDGE('',*,*,#17597,.T.);
#25229=ORIENTED_EDGE('',*,*,#17360,.T.);
#25230=ORIENTED_EDGE('',*,*,#16812,.T.);
#25231=ORIENTED_EDGE('',*,*,#17782,.T.);
#25232=ORIENTED_EDGE('',*,*,#16657,.T.);
#25233=ORIENTED_EDGE('',*,*,#17781,.F.);
#25234=ORIENTED_EDGE('',*,*,#16811,.T.);
#25235=ORIENTED_EDGE('',*,*,#17757,.T.);
#25236=ORIENTED_EDGE('',*,*,#17760,.T.);
#25237=ORIENTED_EDGE('',*,*,#17763,.T.);
#25238=ORIENTED_EDGE('',*,*,#16658,.T.);
#25239=ORIENTED_EDGE('',*,*,#17782,.F.);
#25240=ORIENTED_EDGE('',*,*,#17110,.T.);
#25241=ORIENTED_EDGE('',*,*,#17783,.T.);
#25242=ORIENTED_EDGE('',*,*,#16664,.T.);
#25243=ORIENTED_EDGE('',*,*,#17753,.T.);
#25244=ORIENTED_EDGE('',*,*,#17593,.T.);
#25245=ORIENTED_EDGE('',*,*,#17356,.T.);
#25246=ORIENTED_EDGE('',*,*,#17109,.T.);
#25247=ORIENTED_EDGE('',*,*,#17784,.T.);
#25248=ORIENTED_EDGE('',*,*,#16665,.T.);
#25249=ORIENTED_EDGE('',*,*,#17783,.F.);
#25250=ORIENTED_EDGE('',*,*,#17108,.T.);
#25251=ORIENTED_EDGE('',*,*,#17355,.T.);
#25252=ORIENTED_EDGE('',*,*,#17592,.T.);
#25253=ORIENTED_EDGE('',*,*,#17752,.T.);
#25254=ORIENTED_EDGE('',*,*,#16666,.T.);
#25255=ORIENTED_EDGE('',*,*,#17784,.F.);
#25256=ORIENTED_EDGE('',*,*,#17106,.T.);
#25257=ORIENTED_EDGE('',*,*,#17785,.T.);
#25258=ORIENTED_EDGE('',*,*,#16668,.T.);
#25259=ORIENTED_EDGE('',*,*,#17751,.T.);
#25260=ORIENTED_EDGE('',*,*,#17590,.T.);
#25261=ORIENTED_EDGE('',*,*,#17353,.T.);
#25262=ORIENTED_EDGE('',*,*,#17105,.T.);
#25263=ORIENTED_EDGE('',*,*,#17786,.T.);
#25264=ORIENTED_EDGE('',*,*,#16669,.T.);
#25265=ORIENTED_EDGE('',*,*,#17785,.F.);
#25266=ORIENTED_EDGE('',*,*,#17104,.T.);
#25267=ORIENTED_EDGE('',*,*,#17352,.T.);
#25268=ORIENTED_EDGE('',*,*,#17589,.T.);
#25269=ORIENTED_EDGE('',*,*,#17750,.T.);
#25270=ORIENTED_EDGE('',*,*,#16670,.T.);
#25271=ORIENTED_EDGE('',*,*,#17786,.F.);
#25272=ORIENTED_EDGE('',*,*,#17102,.T.);
#25273=ORIENTED_EDGE('',*,*,#17787,.T.);
#25274=ORIENTED_EDGE('',*,*,#16672,.T.);
#25275=ORIENTED_EDGE('',*,*,#17749,.T.);
#25276=ORIENTED_EDGE('',*,*,#17587,.T.);
#25277=ORIENTED_EDGE('',*,*,#17350,.T.);
#25278=ORIENTED_EDGE('',*,*,#17101,.T.);
#25279=ORIENTED_EDGE('',*,*,#17788,.T.);
#25280=ORIENTED_EDGE('',*,*,#16673,.T.);
#25281=ORIENTED_EDGE('',*,*,#17787,.F.);
#25282=ORIENTED_EDGE('',*,*,#17100,.T.);
#25283=ORIENTED_EDGE('',*,*,#17349,.T.);
#25284=ORIENTED_EDGE('',*,*,#17586,.T.);
#25285=ORIENTED_EDGE('',*,*,#17748,.T.);
#25286=ORIENTED_EDGE('',*,*,#16674,.T.);
#25287=ORIENTED_EDGE('',*,*,#17788,.F.);
#25288=ORIENTED_EDGE('',*,*,#17098,.T.);
#25289=ORIENTED_EDGE('',*,*,#17789,.T.);
#25290=ORIENTED_EDGE('',*,*,#16676,.T.);
#25291=ORIENTED_EDGE('',*,*,#17747,.T.);
#25292=ORIENTED_EDGE('',*,*,#17584,.T.);
#25293=ORIENTED_EDGE('',*,*,#17347,.T.);
#25294=ORIENTED_EDGE('',*,*,#17097,.T.);
#25295=ORIENTED_EDGE('',*,*,#17790,.T.);
#25296=ORIENTED_EDGE('',*,*,#16677,.T.);
#25297=ORIENTED_EDGE('',*,*,#17789,.F.);
#25298=ORIENTED_EDGE('',*,*,#17096,.T.);
#25299=ORIENTED_EDGE('',*,*,#17346,.T.);
#25300=ORIENTED_EDGE('',*,*,#17583,.T.);
#25301=ORIENTED_EDGE('',*,*,#17746,.T.);
#25302=ORIENTED_EDGE('',*,*,#16678,.T.);
#25303=ORIENTED_EDGE('',*,*,#17790,.F.);
#25304=ORIENTED_EDGE('',*,*,#17094,.T.);
#25305=ORIENTED_EDGE('',*,*,#17791,.T.);
#25306=ORIENTED_EDGE('',*,*,#16680,.T.);
#25307=ORIENTED_EDGE('',*,*,#17745,.T.);
#25308=ORIENTED_EDGE('',*,*,#17581,.T.);
#25309=ORIENTED_EDGE('',*,*,#17344,.T.);
#25310=ORIENTED_EDGE('',*,*,#17093,.T.);
#25311=ORIENTED_EDGE('',*,*,#17792,.T.);
#25312=ORIENTED_EDGE('',*,*,#16681,.T.);
#25313=ORIENTED_EDGE('',*,*,#17791,.F.);
#25314=ORIENTED_EDGE('',*,*,#17092,.T.);
#25315=ORIENTED_EDGE('',*,*,#17343,.T.);
#25316=ORIENTED_EDGE('',*,*,#17580,.T.);
#25317=ORIENTED_EDGE('',*,*,#17744,.T.);
#25318=ORIENTED_EDGE('',*,*,#16682,.T.);
#25319=ORIENTED_EDGE('',*,*,#17792,.F.);
#25320=ORIENTED_EDGE('',*,*,#17090,.T.);
#25321=ORIENTED_EDGE('',*,*,#16488,.T.);
#25322=ORIENTED_EDGE('',*,*,#16684,.T.);
#25323=ORIENTED_EDGE('',*,*,#17743,.T.);
#25324=ORIENTED_EDGE('',*,*,#17578,.T.);
#25325=ORIENTED_EDGE('',*,*,#17341,.T.);
#25326=ORIENTED_EDGE('',*,*,#17089,.T.);
#25327=ORIENTED_EDGE('',*,*,#17340,.T.);
#25328=ORIENTED_EDGE('',*,*,#17577,.T.);
#25329=ORIENTED_EDGE('',*,*,#17742,.T.);
#25330=ORIENTED_EDGE('',*,*,#16685,.T.);
#25331=ORIENTED_EDGE('',*,*,#16486,.F.);
#25332=ORIENTED_EDGE('',*,*,#17087,.T.);
#25333=ORIENTED_EDGE('',*,*,#16484,.T.);
#25334=ORIENTED_EDGE('',*,*,#16687,.T.);
#25335=ORIENTED_EDGE('',*,*,#17741,.T.);
#25336=ORIENTED_EDGE('',*,*,#17575,.T.);
#25337=ORIENTED_EDGE('',*,*,#17338,.T.);
#25338=ORIENTED_EDGE('',*,*,#17086,.T.);
#25339=ORIENTED_EDGE('',*,*,#17337,.T.);
#25340=ORIENTED_EDGE('',*,*,#17574,.T.);
#25341=ORIENTED_EDGE('',*,*,#17740,.T.);
#25342=ORIENTED_EDGE('',*,*,#16688,.T.);
#25343=ORIENTED_EDGE('',*,*,#16482,.F.);
#25344=ORIENTED_EDGE('',*,*,#17084,.T.);
#25345=ORIENTED_EDGE('',*,*,#16480,.T.);
#25346=ORIENTED_EDGE('',*,*,#16690,.T.);
#25347=ORIENTED_EDGE('',*,*,#17739,.T.);
#25348=ORIENTED_EDGE('',*,*,#17572,.T.);
#25349=ORIENTED_EDGE('',*,*,#17335,.T.);
#25350=ORIENTED_EDGE('',*,*,#17083,.T.);
#25351=ORIENTED_EDGE('',*,*,#17334,.T.);
#25352=ORIENTED_EDGE('',*,*,#17571,.T.);
#25353=ORIENTED_EDGE('',*,*,#17738,.T.);
#25354=ORIENTED_EDGE('',*,*,#16691,.T.);
#25355=ORIENTED_EDGE('',*,*,#16478,.F.);
#25356=ORIENTED_EDGE('',*,*,#17081,.T.);
#25357=ORIENTED_EDGE('',*,*,#16476,.T.);
#25358=ORIENTED_EDGE('',*,*,#16693,.T.);
#25359=ORIENTED_EDGE('',*,*,#17737,.T.);
#25360=ORIENTED_EDGE('',*,*,#17569,.T.);
#25361=ORIENTED_EDGE('',*,*,#17332,.T.);
#25362=ORIENTED_EDGE('',*,*,#17080,.T.);
#25363=ORIENTED_EDGE('',*,*,#17331,.T.);
#25364=ORIENTED_EDGE('',*,*,#17568,.T.);
#25365=ORIENTED_EDGE('',*,*,#17736,.T.);
#25366=ORIENTED_EDGE('',*,*,#16694,.T.);
#25367=ORIENTED_EDGE('',*,*,#16474,.F.);
#25368=ORIENTED_EDGE('',*,*,#17078,.T.);
#25369=ORIENTED_EDGE('',*,*,#16472,.T.);
#25370=ORIENTED_EDGE('',*,*,#16696,.T.);
#25371=ORIENTED_EDGE('',*,*,#17735,.T.);
#25372=ORIENTED_EDGE('',*,*,#17566,.T.);
#25373=ORIENTED_EDGE('',*,*,#17329,.T.);
#25374=ORIENTED_EDGE('',*,*,#17077,.T.);
#25375=ORIENTED_EDGE('',*,*,#17328,.T.);
#25376=ORIENTED_EDGE('',*,*,#17565,.T.);
#25377=ORIENTED_EDGE('',*,*,#17734,.T.);
#25378=ORIENTED_EDGE('',*,*,#16697,.T.);
#25379=ORIENTED_EDGE('',*,*,#16470,.F.);
#25380=ORIENTED_EDGE('',*,*,#17075,.T.);
#25381=ORIENTED_EDGE('',*,*,#16468,.T.);
#25382=ORIENTED_EDGE('',*,*,#16699,.T.);
#25383=ORIENTED_EDGE('',*,*,#17733,.T.);
#25384=ORIENTED_EDGE('',*,*,#17563,.T.);
#25385=ORIENTED_EDGE('',*,*,#17326,.T.);
#25386=ORIENTED_EDGE('',*,*,#17074,.T.);
#25387=ORIENTED_EDGE('',*,*,#17325,.T.);
#25388=ORIENTED_EDGE('',*,*,#17562,.T.);
#25389=ORIENTED_EDGE('',*,*,#17732,.T.);
#25390=ORIENTED_EDGE('',*,*,#16700,.T.);
#25391=ORIENTED_EDGE('',*,*,#16466,.F.);
#25392=ORIENTED_EDGE('',*,*,#17072,.T.);
#25393=ORIENTED_EDGE('',*,*,#16464,.T.);
#25394=ORIENTED_EDGE('',*,*,#16702,.T.);
#25395=ORIENTED_EDGE('',*,*,#17731,.T.);
#25396=ORIENTED_EDGE('',*,*,#17560,.T.);
#25397=ORIENTED_EDGE('',*,*,#17323,.T.);
#25398=ORIENTED_EDGE('',*,*,#17071,.T.);
#25399=ORIENTED_EDGE('',*,*,#17322,.T.);
#25400=ORIENTED_EDGE('',*,*,#17559,.T.);
#25401=ORIENTED_EDGE('',*,*,#17730,.T.);
#25402=ORIENTED_EDGE('',*,*,#16703,.T.);
#25403=ORIENTED_EDGE('',*,*,#16462,.F.);
#25404=ORIENTED_EDGE('',*,*,#17069,.T.);
#25405=ORIENTED_EDGE('',*,*,#16460,.T.);
#25406=ORIENTED_EDGE('',*,*,#16705,.T.);
#25407=ORIENTED_EDGE('',*,*,#17729,.T.);
#25408=ORIENTED_EDGE('',*,*,#17557,.T.);
#25409=ORIENTED_EDGE('',*,*,#17320,.T.);
#25410=ORIENTED_EDGE('',*,*,#17068,.T.);
#25411=ORIENTED_EDGE('',*,*,#17319,.T.);
#25412=ORIENTED_EDGE('',*,*,#17556,.T.);
#25413=ORIENTED_EDGE('',*,*,#17728,.T.);
#25414=ORIENTED_EDGE('',*,*,#16706,.T.);
#25415=ORIENTED_EDGE('',*,*,#16458,.F.);
#25416=ORIENTED_EDGE('',*,*,#17066,.T.);
#25417=ORIENTED_EDGE('',*,*,#16456,.T.);
#25418=ORIENTED_EDGE('',*,*,#16708,.T.);
#25419=ORIENTED_EDGE('',*,*,#17727,.T.);
#25420=ORIENTED_EDGE('',*,*,#17554,.T.);
#25421=ORIENTED_EDGE('',*,*,#17317,.T.);
#25422=ORIENTED_EDGE('',*,*,#17065,.T.);
#25423=ORIENTED_EDGE('',*,*,#17127,.T.);
#25424=ORIENTED_EDGE('',*,*,#17364,.T.);
#25425=ORIENTED_EDGE('',*,*,#17600,.T.);
#25426=ORIENTED_EDGE('',*,*,#16709,.T.);
#25427=ORIENTED_EDGE('',*,*,#16454,.F.);
#25428=ORIENTED_EDGE('',*,*,#16817,.T.);
#25429=ORIENTED_EDGE('',*,*,#17793,.T.);
#25430=ORIENTED_EDGE('',*,*,#16652,.T.);
#25431=ORIENTED_EDGE('',*,*,#17726,.T.);
#25432=ORIENTED_EDGE('',*,*,#17552,.T.);
#25433=ORIENTED_EDGE('',*,*,#17315,.T.);
#25434=ORIENTED_EDGE('',*,*,#16816,.T.);
#25435=ORIENTED_EDGE('',*,*,#17794,.T.);
#25436=ORIENTED_EDGE('',*,*,#16653,.T.);
#25437=ORIENTED_EDGE('',*,*,#17793,.F.);
#25438=ORIENTED_EDGE('',*,*,#16815,.T.);
#25439=ORIENTED_EDGE('',*,*,#17359,.T.);
#25440=ORIENTED_EDGE('',*,*,#17596,.T.);
#25441=ORIENTED_EDGE('',*,*,#17755,.T.);
#25442=ORIENTED_EDGE('',*,*,#16654,.T.);
#25443=ORIENTED_EDGE('',*,*,#17794,.F.);
#25444=ORIENTED_EDGE('',*,*,#16821,.T.);
#25445=ORIENTED_EDGE('',*,*,#17795,.T.);
#25446=ORIENTED_EDGE('',*,*,#16648,.T.);
#25447=ORIENTED_EDGE('',*,*,#17724,.T.);
#25448=ORIENTED_EDGE('',*,*,#17549,.T.);
#25449=ORIENTED_EDGE('',*,*,#17312,.T.);
#25450=ORIENTED_EDGE('',*,*,#16820,.T.);
#25451=ORIENTED_EDGE('',*,*,#17796,.T.);
#25452=ORIENTED_EDGE('',*,*,#16649,.T.);
#25453=ORIENTED_EDGE('',*,*,#17795,.F.);
#25454=ORIENTED_EDGE('',*,*,#16819,.T.);
#25455=ORIENTED_EDGE('',*,*,#17314,.T.);
#25456=ORIENTED_EDGE('',*,*,#17551,.T.);
#25457=ORIENTED_EDGE('',*,*,#17725,.T.);
#25458=ORIENTED_EDGE('',*,*,#16650,.T.);
#25459=ORIENTED_EDGE('',*,*,#17796,.F.);
#25460=ORIENTED_EDGE('',*,*,#16825,.T.);
#25461=ORIENTED_EDGE('',*,*,#17797,.T.);
#25462=ORIENTED_EDGE('',*,*,#16644,.T.);
#25463=ORIENTED_EDGE('',*,*,#17722,.T.);
#25464=ORIENTED_EDGE('',*,*,#17546,.T.);
#25465=ORIENTED_EDGE('',*,*,#17309,.T.);
#25466=ORIENTED_EDGE('',*,*,#16824,.T.);
#25467=ORIENTED_EDGE('',*,*,#17798,.T.);
#25468=ORIENTED_EDGE('',*,*,#16645,.T.);
#25469=ORIENTED_EDGE('',*,*,#17797,.F.);
#25470=ORIENTED_EDGE('',*,*,#16823,.T.);
#25471=ORIENTED_EDGE('',*,*,#17311,.T.);
#25472=ORIENTED_EDGE('',*,*,#17548,.T.);
#25473=ORIENTED_EDGE('',*,*,#17723,.T.);
#25474=ORIENTED_EDGE('',*,*,#16646,.T.);
#25475=ORIENTED_EDGE('',*,*,#17798,.F.);
#25476=ORIENTED_EDGE('',*,*,#16829,.T.);
#25477=ORIENTED_EDGE('',*,*,#17799,.T.);
#25478=ORIENTED_EDGE('',*,*,#16640,.T.);
#25479=ORIENTED_EDGE('',*,*,#17720,.T.);
#25480=ORIENTED_EDGE('',*,*,#17543,.T.);
#25481=ORIENTED_EDGE('',*,*,#17306,.T.);
#25482=ORIENTED_EDGE('',*,*,#16828,.T.);
#25483=ORIENTED_EDGE('',*,*,#17800,.T.);
#25484=ORIENTED_EDGE('',*,*,#16641,.T.);
#25485=ORIENTED_EDGE('',*,*,#17799,.F.);
#25486=ORIENTED_EDGE('',*,*,#16827,.T.);
#25487=ORIENTED_EDGE('',*,*,#17308,.T.);
#25488=ORIENTED_EDGE('',*,*,#17545,.T.);
#25489=ORIENTED_EDGE('',*,*,#17721,.T.);
#25490=ORIENTED_EDGE('',*,*,#16642,.T.);
#25491=ORIENTED_EDGE('',*,*,#17800,.F.);
#25492=ORIENTED_EDGE('',*,*,#16833,.T.);
#25493=ORIENTED_EDGE('',*,*,#17801,.T.);
#25494=ORIENTED_EDGE('',*,*,#16636,.T.);
#25495=ORIENTED_EDGE('',*,*,#17718,.T.);
#25496=ORIENTED_EDGE('',*,*,#17540,.T.);
#25497=ORIENTED_EDGE('',*,*,#17303,.T.);
#25498=ORIENTED_EDGE('',*,*,#16832,.T.);
#25499=ORIENTED_EDGE('',*,*,#17802,.T.);
#25500=ORIENTED_EDGE('',*,*,#16637,.T.);
#25501=ORIENTED_EDGE('',*,*,#17801,.F.);
#25502=ORIENTED_EDGE('',*,*,#16831,.T.);
#25503=ORIENTED_EDGE('',*,*,#17305,.T.);
#25504=ORIENTED_EDGE('',*,*,#17542,.T.);
#25505=ORIENTED_EDGE('',*,*,#17719,.T.);
#25506=ORIENTED_EDGE('',*,*,#16638,.T.);
#25507=ORIENTED_EDGE('',*,*,#17802,.F.);
#25508=ORIENTED_EDGE('',*,*,#16837,.T.);
#25509=ORIENTED_EDGE('',*,*,#17803,.T.);
#25510=ORIENTED_EDGE('',*,*,#16632,.T.);
#25511=ORIENTED_EDGE('',*,*,#17716,.T.);
#25512=ORIENTED_EDGE('',*,*,#17537,.T.);
#25513=ORIENTED_EDGE('',*,*,#17300,.T.);
#25514=ORIENTED_EDGE('',*,*,#16836,.T.);
#25515=ORIENTED_EDGE('',*,*,#17804,.T.);
#25516=ORIENTED_EDGE('',*,*,#16633,.T.);
#25517=ORIENTED_EDGE('',*,*,#17803,.F.);
#25518=ORIENTED_EDGE('',*,*,#16835,.T.);
#25519=ORIENTED_EDGE('',*,*,#17302,.T.);
#25520=ORIENTED_EDGE('',*,*,#17539,.T.);
#25521=ORIENTED_EDGE('',*,*,#17717,.T.);
#25522=ORIENTED_EDGE('',*,*,#16634,.T.);
#25523=ORIENTED_EDGE('',*,*,#17804,.F.);
#25524=ORIENTED_EDGE('',*,*,#16841,.T.);
#25525=ORIENTED_EDGE('',*,*,#17805,.T.);
#25526=ORIENTED_EDGE('',*,*,#16628,.T.);
#25527=ORIENTED_EDGE('',*,*,#17714,.T.);
#25528=ORIENTED_EDGE('',*,*,#17534,.T.);
#25529=ORIENTED_EDGE('',*,*,#17297,.T.);
#25530=ORIENTED_EDGE('',*,*,#16840,.T.);
#25531=ORIENTED_EDGE('',*,*,#17806,.T.);
#25532=ORIENTED_EDGE('',*,*,#16629,.T.);
#25533=ORIENTED_EDGE('',*,*,#17805,.F.);
#25534=ORIENTED_EDGE('',*,*,#16839,.T.);
#25535=ORIENTED_EDGE('',*,*,#17299,.T.);
#25536=ORIENTED_EDGE('',*,*,#17536,.T.);
#25537=ORIENTED_EDGE('',*,*,#17715,.T.);
#25538=ORIENTED_EDGE('',*,*,#16630,.T.);
#25539=ORIENTED_EDGE('',*,*,#17806,.F.);
#25540=ORIENTED_EDGE('',*,*,#16845,.T.);
#25541=ORIENTED_EDGE('',*,*,#17807,.T.);
#25542=ORIENTED_EDGE('',*,*,#16624,.T.);
#25543=ORIENTED_EDGE('',*,*,#17712,.T.);
#25544=ORIENTED_EDGE('',*,*,#17531,.T.);
#25545=ORIENTED_EDGE('',*,*,#17294,.T.);
#25546=ORIENTED_EDGE('',*,*,#16844,.T.);
#25547=ORIENTED_EDGE('',*,*,#17808,.T.);
#25548=ORIENTED_EDGE('',*,*,#16625,.T.);
#25549=ORIENTED_EDGE('',*,*,#17807,.F.);
#25550=ORIENTED_EDGE('',*,*,#16843,.T.);
#25551=ORIENTED_EDGE('',*,*,#17296,.T.);
#25552=ORIENTED_EDGE('',*,*,#17533,.T.);
#25553=ORIENTED_EDGE('',*,*,#17713,.T.);
#25554=ORIENTED_EDGE('',*,*,#16626,.T.);
#25555=ORIENTED_EDGE('',*,*,#17808,.F.);
#25556=ORIENTED_EDGE('',*,*,#16849,.T.);
#25557=ORIENTED_EDGE('',*,*,#17809,.T.);
#25558=ORIENTED_EDGE('',*,*,#16620,.T.);
#25559=ORIENTED_EDGE('',*,*,#17710,.T.);
#25560=ORIENTED_EDGE('',*,*,#17528,.T.);
#25561=ORIENTED_EDGE('',*,*,#17291,.T.);
#25562=ORIENTED_EDGE('',*,*,#16848,.T.);
#25563=ORIENTED_EDGE('',*,*,#17810,.T.);
#25564=ORIENTED_EDGE('',*,*,#16621,.T.);
#25565=ORIENTED_EDGE('',*,*,#17809,.F.);
#25566=ORIENTED_EDGE('',*,*,#16847,.T.);
#25567=ORIENTED_EDGE('',*,*,#17293,.T.);
#25568=ORIENTED_EDGE('',*,*,#17530,.T.);
#25569=ORIENTED_EDGE('',*,*,#17711,.T.);
#25570=ORIENTED_EDGE('',*,*,#16622,.T.);
#25571=ORIENTED_EDGE('',*,*,#17810,.F.);
#25572=ORIENTED_EDGE('',*,*,#16853,.T.);
#25573=ORIENTED_EDGE('',*,*,#17811,.T.);
#25574=ORIENTED_EDGE('',*,*,#16616,.T.);
#25575=ORIENTED_EDGE('',*,*,#17708,.T.);
#25576=ORIENTED_EDGE('',*,*,#17525,.T.);
#25577=ORIENTED_EDGE('',*,*,#17288,.T.);
#25578=ORIENTED_EDGE('',*,*,#16852,.T.);
#25579=ORIENTED_EDGE('',*,*,#17812,.T.);
#25580=ORIENTED_EDGE('',*,*,#16617,.T.);
#25581=ORIENTED_EDGE('',*,*,#17811,.F.);
#25582=ORIENTED_EDGE('',*,*,#16851,.T.);
#25583=ORIENTED_EDGE('',*,*,#17290,.T.);
#25584=ORIENTED_EDGE('',*,*,#17527,.T.);
#25585=ORIENTED_EDGE('',*,*,#17709,.T.);
#25586=ORIENTED_EDGE('',*,*,#16618,.T.);
#25587=ORIENTED_EDGE('',*,*,#17812,.F.);
#25588=ORIENTED_EDGE('',*,*,#16857,.T.);
#25589=ORIENTED_EDGE('',*,*,#17813,.T.);
#25590=ORIENTED_EDGE('',*,*,#16612,.T.);
#25591=ORIENTED_EDGE('',*,*,#17706,.T.);
#25592=ORIENTED_EDGE('',*,*,#17522,.T.);
#25593=ORIENTED_EDGE('',*,*,#17285,.T.);
#25594=ORIENTED_EDGE('',*,*,#16856,.T.);
#25595=ORIENTED_EDGE('',*,*,#17814,.T.);
#25596=ORIENTED_EDGE('',*,*,#16613,.T.);
#25597=ORIENTED_EDGE('',*,*,#17813,.F.);
#25598=ORIENTED_EDGE('',*,*,#16855,.T.);
#25599=ORIENTED_EDGE('',*,*,#17287,.T.);
#25600=ORIENTED_EDGE('',*,*,#17524,.T.);
#25601=ORIENTED_EDGE('',*,*,#17707,.T.);
#25602=ORIENTED_EDGE('',*,*,#16614,.T.);
#25603=ORIENTED_EDGE('',*,*,#17814,.F.);
#25604=ORIENTED_EDGE('',*,*,#16861,.T.);
#25605=ORIENTED_EDGE('',*,*,#17815,.T.);
#25606=ORIENTED_EDGE('',*,*,#16608,.T.);
#25607=ORIENTED_EDGE('',*,*,#17704,.T.);
#25608=ORIENTED_EDGE('',*,*,#17519,.T.);
#25609=ORIENTED_EDGE('',*,*,#17282,.T.);
#25610=ORIENTED_EDGE('',*,*,#16860,.T.);
#25611=ORIENTED_EDGE('',*,*,#17816,.T.);
#25612=ORIENTED_EDGE('',*,*,#16609,.T.);
#25613=ORIENTED_EDGE('',*,*,#17815,.F.);
#25614=ORIENTED_EDGE('',*,*,#16859,.T.);
#25615=ORIENTED_EDGE('',*,*,#17284,.T.);
#25616=ORIENTED_EDGE('',*,*,#17521,.T.);
#25617=ORIENTED_EDGE('',*,*,#17705,.T.);
#25618=ORIENTED_EDGE('',*,*,#16610,.T.);
#25619=ORIENTED_EDGE('',*,*,#17816,.F.);
#25620=ORIENTED_EDGE('',*,*,#16865,.T.);
#25621=ORIENTED_EDGE('',*,*,#17817,.T.);
#25622=ORIENTED_EDGE('',*,*,#16604,.T.);
#25623=ORIENTED_EDGE('',*,*,#17702,.T.);
#25624=ORIENTED_EDGE('',*,*,#17516,.T.);
#25625=ORIENTED_EDGE('',*,*,#17279,.T.);
#25626=ORIENTED_EDGE('',*,*,#16864,.T.);
#25627=ORIENTED_EDGE('',*,*,#17818,.T.);
#25628=ORIENTED_EDGE('',*,*,#16605,.T.);
#25629=ORIENTED_EDGE('',*,*,#17817,.F.);
#25630=ORIENTED_EDGE('',*,*,#16863,.T.);
#25631=ORIENTED_EDGE('',*,*,#17281,.T.);
#25632=ORIENTED_EDGE('',*,*,#17518,.T.);
#25633=ORIENTED_EDGE('',*,*,#17703,.T.);
#25634=ORIENTED_EDGE('',*,*,#16606,.T.);
#25635=ORIENTED_EDGE('',*,*,#17818,.F.);
#25636=ORIENTED_EDGE('',*,*,#16869,.T.);
#25637=ORIENTED_EDGE('',*,*,#17819,.T.);
#25638=ORIENTED_EDGE('',*,*,#16600,.T.);
#25639=ORIENTED_EDGE('',*,*,#17700,.T.);
#25640=ORIENTED_EDGE('',*,*,#17513,.T.);
#25641=ORIENTED_EDGE('',*,*,#17276,.T.);
#25642=ORIENTED_EDGE('',*,*,#16868,.T.);
#25643=ORIENTED_EDGE('',*,*,#17820,.T.);
#25644=ORIENTED_EDGE('',*,*,#16601,.T.);
#25645=ORIENTED_EDGE('',*,*,#17819,.F.);
#25646=ORIENTED_EDGE('',*,*,#16867,.T.);
#25647=ORIENTED_EDGE('',*,*,#17278,.T.);
#25648=ORIENTED_EDGE('',*,*,#17515,.T.);
#25649=ORIENTED_EDGE('',*,*,#17701,.T.);
#25650=ORIENTED_EDGE('',*,*,#16602,.T.);
#25651=ORIENTED_EDGE('',*,*,#17820,.F.);
#25652=ORIENTED_EDGE('',*,*,#16873,.T.);
#25653=ORIENTED_EDGE('',*,*,#17821,.T.);
#25654=ORIENTED_EDGE('',*,*,#16596,.T.);
#25655=ORIENTED_EDGE('',*,*,#17698,.T.);
#25656=ORIENTED_EDGE('',*,*,#17510,.T.);
#25657=ORIENTED_EDGE('',*,*,#17273,.T.);
#25658=ORIENTED_EDGE('',*,*,#16872,.T.);
#25659=ORIENTED_EDGE('',*,*,#17822,.T.);
#25660=ORIENTED_EDGE('',*,*,#16597,.T.);
#25661=ORIENTED_EDGE('',*,*,#17821,.F.);
#25662=ORIENTED_EDGE('',*,*,#16871,.T.);
#25663=ORIENTED_EDGE('',*,*,#17275,.T.);
#25664=ORIENTED_EDGE('',*,*,#17512,.T.);
#25665=ORIENTED_EDGE('',*,*,#17699,.T.);
#25666=ORIENTED_EDGE('',*,*,#16598,.T.);
#25667=ORIENTED_EDGE('',*,*,#17822,.F.);
#25668=ORIENTED_EDGE('',*,*,#16877,.T.);
#25669=ORIENTED_EDGE('',*,*,#17823,.T.);
#25670=ORIENTED_EDGE('',*,*,#16592,.T.);
#25671=ORIENTED_EDGE('',*,*,#17696,.T.);
#25672=ORIENTED_EDGE('',*,*,#17507,.T.);
#25673=ORIENTED_EDGE('',*,*,#17270,.T.);
#25674=ORIENTED_EDGE('',*,*,#16876,.T.);
#25675=ORIENTED_EDGE('',*,*,#17824,.T.);
#25676=ORIENTED_EDGE('',*,*,#16593,.T.);
#25677=ORIENTED_EDGE('',*,*,#17823,.F.);
#25678=ORIENTED_EDGE('',*,*,#16875,.T.);
#25679=ORIENTED_EDGE('',*,*,#17272,.T.);
#25680=ORIENTED_EDGE('',*,*,#17509,.T.);
#25681=ORIENTED_EDGE('',*,*,#17697,.T.);
#25682=ORIENTED_EDGE('',*,*,#16594,.T.);
#25683=ORIENTED_EDGE('',*,*,#17824,.F.);
#25684=ORIENTED_EDGE('',*,*,#16881,.T.);
#25685=ORIENTED_EDGE('',*,*,#17825,.T.);
#25686=ORIENTED_EDGE('',*,*,#16588,.T.);
#25687=ORIENTED_EDGE('',*,*,#17694,.T.);
#25688=ORIENTED_EDGE('',*,*,#17504,.T.);
#25689=ORIENTED_EDGE('',*,*,#17267,.T.);
#25690=ORIENTED_EDGE('',*,*,#16880,.T.);
#25691=ORIENTED_EDGE('',*,*,#17826,.T.);
#25692=ORIENTED_EDGE('',*,*,#16589,.T.);
#25693=ORIENTED_EDGE('',*,*,#17825,.F.);
#25694=ORIENTED_EDGE('',*,*,#16879,.T.);
#25695=ORIENTED_EDGE('',*,*,#17269,.T.);
#25696=ORIENTED_EDGE('',*,*,#17506,.T.);
#25697=ORIENTED_EDGE('',*,*,#17695,.T.);
#25698=ORIENTED_EDGE('',*,*,#16590,.T.);
#25699=ORIENTED_EDGE('',*,*,#17826,.F.);
#25700=ORIENTED_EDGE('',*,*,#16885,.T.);
#25701=ORIENTED_EDGE('',*,*,#17827,.T.);
#25702=ORIENTED_EDGE('',*,*,#16584,.T.);
#25703=ORIENTED_EDGE('',*,*,#17692,.T.);
#25704=ORIENTED_EDGE('',*,*,#17501,.T.);
#25705=ORIENTED_EDGE('',*,*,#17264,.T.);
#25706=ORIENTED_EDGE('',*,*,#16884,.T.);
#25707=ORIENTED_EDGE('',*,*,#17828,.T.);
#25708=ORIENTED_EDGE('',*,*,#16585,.T.);
#25709=ORIENTED_EDGE('',*,*,#17827,.F.);
#25710=ORIENTED_EDGE('',*,*,#16883,.T.);
#25711=ORIENTED_EDGE('',*,*,#17266,.T.);
#25712=ORIENTED_EDGE('',*,*,#17503,.T.);
#25713=ORIENTED_EDGE('',*,*,#17693,.T.);
#25714=ORIENTED_EDGE('',*,*,#16586,.T.);
#25715=ORIENTED_EDGE('',*,*,#17828,.F.);
#25716=ORIENTED_EDGE('',*,*,#16889,.T.);
#25717=ORIENTED_EDGE('',*,*,#17829,.T.);
#25718=ORIENTED_EDGE('',*,*,#16580,.T.);
#25719=ORIENTED_EDGE('',*,*,#17690,.T.);
#25720=ORIENTED_EDGE('',*,*,#17498,.T.);
#25721=ORIENTED_EDGE('',*,*,#17261,.T.);
#25722=ORIENTED_EDGE('',*,*,#16888,.T.);
#25723=ORIENTED_EDGE('',*,*,#17830,.T.);
#25724=ORIENTED_EDGE('',*,*,#16581,.T.);
#25725=ORIENTED_EDGE('',*,*,#17829,.F.);
#25726=ORIENTED_EDGE('',*,*,#16887,.T.);
#25727=ORIENTED_EDGE('',*,*,#17263,.T.);
#25728=ORIENTED_EDGE('',*,*,#17500,.T.);
#25729=ORIENTED_EDGE('',*,*,#17691,.T.);
#25730=ORIENTED_EDGE('',*,*,#16582,.T.);
#25731=ORIENTED_EDGE('',*,*,#17830,.F.);
#25732=ORIENTED_EDGE('',*,*,#16893,.T.);
#25733=ORIENTED_EDGE('',*,*,#17831,.T.);
#25734=ORIENTED_EDGE('',*,*,#16576,.T.);
#25735=ORIENTED_EDGE('',*,*,#17688,.T.);
#25736=ORIENTED_EDGE('',*,*,#17495,.T.);
#25737=ORIENTED_EDGE('',*,*,#17258,.T.);
#25738=ORIENTED_EDGE('',*,*,#16892,.T.);
#25739=ORIENTED_EDGE('',*,*,#17832,.T.);
#25740=ORIENTED_EDGE('',*,*,#16577,.T.);
#25741=ORIENTED_EDGE('',*,*,#17831,.F.);
#25742=ORIENTED_EDGE('',*,*,#16891,.T.);
#25743=ORIENTED_EDGE('',*,*,#17260,.T.);
#25744=ORIENTED_EDGE('',*,*,#17497,.T.);
#25745=ORIENTED_EDGE('',*,*,#17689,.T.);
#25746=ORIENTED_EDGE('',*,*,#16578,.T.);
#25747=ORIENTED_EDGE('',*,*,#17832,.F.);
#25748=ORIENTED_EDGE('',*,*,#16897,.T.);
#25749=ORIENTED_EDGE('',*,*,#17833,.T.);
#25750=ORIENTED_EDGE('',*,*,#16572,.T.);
#25751=ORIENTED_EDGE('',*,*,#17686,.T.);
#25752=ORIENTED_EDGE('',*,*,#17492,.T.);
#25753=ORIENTED_EDGE('',*,*,#17255,.T.);
#25754=ORIENTED_EDGE('',*,*,#16896,.T.);
#25755=ORIENTED_EDGE('',*,*,#17834,.T.);
#25756=ORIENTED_EDGE('',*,*,#16573,.T.);
#25757=ORIENTED_EDGE('',*,*,#17833,.F.);
#25758=ORIENTED_EDGE('',*,*,#16895,.T.);
#25759=ORIENTED_EDGE('',*,*,#17257,.T.);
#25760=ORIENTED_EDGE('',*,*,#17494,.T.);
#25761=ORIENTED_EDGE('',*,*,#17687,.T.);
#25762=ORIENTED_EDGE('',*,*,#16574,.T.);
#25763=ORIENTED_EDGE('',*,*,#17834,.F.);
#25764=ORIENTED_EDGE('',*,*,#16901,.T.);
#25765=ORIENTED_EDGE('',*,*,#17835,.T.);
#25766=ORIENTED_EDGE('',*,*,#16568,.T.);
#25767=ORIENTED_EDGE('',*,*,#17684,.T.);
#25768=ORIENTED_EDGE('',*,*,#17489,.T.);
#25769=ORIENTED_EDGE('',*,*,#17252,.T.);
#25770=ORIENTED_EDGE('',*,*,#16900,.T.);
#25771=ORIENTED_EDGE('',*,*,#17836,.T.);
#25772=ORIENTED_EDGE('',*,*,#16569,.T.);
#25773=ORIENTED_EDGE('',*,*,#17835,.F.);
#25774=ORIENTED_EDGE('',*,*,#16899,.T.);
#25775=ORIENTED_EDGE('',*,*,#17254,.T.);
#25776=ORIENTED_EDGE('',*,*,#17491,.T.);
#25777=ORIENTED_EDGE('',*,*,#17685,.T.);
#25778=ORIENTED_EDGE('',*,*,#16570,.T.);
#25779=ORIENTED_EDGE('',*,*,#17836,.F.);
#25780=ORIENTED_EDGE('',*,*,#16905,.T.);
#25781=ORIENTED_EDGE('',*,*,#17837,.T.);
#25782=ORIENTED_EDGE('',*,*,#16564,.T.);
#25783=ORIENTED_EDGE('',*,*,#17682,.T.);
#25784=ORIENTED_EDGE('',*,*,#17486,.T.);
#25785=ORIENTED_EDGE('',*,*,#17249,.T.);
#25786=ORIENTED_EDGE('',*,*,#16904,.T.);
#25787=ORIENTED_EDGE('',*,*,#17838,.T.);
#25788=ORIENTED_EDGE('',*,*,#16565,.T.);
#25789=ORIENTED_EDGE('',*,*,#17837,.F.);
#25790=ORIENTED_EDGE('',*,*,#16903,.T.);
#25791=ORIENTED_EDGE('',*,*,#17251,.T.);
#25792=ORIENTED_EDGE('',*,*,#17488,.T.);
#25793=ORIENTED_EDGE('',*,*,#17683,.T.);
#25794=ORIENTED_EDGE('',*,*,#16566,.T.);
#25795=ORIENTED_EDGE('',*,*,#17838,.F.);
#25796=ORIENTED_EDGE('',*,*,#16909,.T.);
#25797=ORIENTED_EDGE('',*,*,#17839,.T.);
#25798=ORIENTED_EDGE('',*,*,#16560,.T.);
#25799=ORIENTED_EDGE('',*,*,#17680,.T.);
#25800=ORIENTED_EDGE('',*,*,#17483,.T.);
#25801=ORIENTED_EDGE('',*,*,#17246,.T.);
#25802=ORIENTED_EDGE('',*,*,#16908,.T.);
#25803=ORIENTED_EDGE('',*,*,#17840,.T.);
#25804=ORIENTED_EDGE('',*,*,#16561,.T.);
#25805=ORIENTED_EDGE('',*,*,#17839,.F.);
#25806=ORIENTED_EDGE('',*,*,#16907,.T.);
#25807=ORIENTED_EDGE('',*,*,#17248,.T.);
#25808=ORIENTED_EDGE('',*,*,#17485,.T.);
#25809=ORIENTED_EDGE('',*,*,#17681,.T.);
#25810=ORIENTED_EDGE('',*,*,#16562,.T.);
#25811=ORIENTED_EDGE('',*,*,#17840,.F.);
#25812=ORIENTED_EDGE('',*,*,#16913,.T.);
#25813=ORIENTED_EDGE('',*,*,#17841,.T.);
#25814=ORIENTED_EDGE('',*,*,#16556,.T.);
#25815=ORIENTED_EDGE('',*,*,#17678,.T.);
#25816=ORIENTED_EDGE('',*,*,#17480,.T.);
#25817=ORIENTED_EDGE('',*,*,#17243,.T.);
#25818=ORIENTED_EDGE('',*,*,#16912,.T.);
#25819=ORIENTED_EDGE('',*,*,#17842,.T.);
#25820=ORIENTED_EDGE('',*,*,#16557,.T.);
#25821=ORIENTED_EDGE('',*,*,#17841,.F.);
#25822=ORIENTED_EDGE('',*,*,#16911,.T.);
#25823=ORIENTED_EDGE('',*,*,#17245,.T.);
#25824=ORIENTED_EDGE('',*,*,#17482,.T.);
#25825=ORIENTED_EDGE('',*,*,#17679,.T.);
#25826=ORIENTED_EDGE('',*,*,#16558,.T.);
#25827=ORIENTED_EDGE('',*,*,#17842,.F.);
#25828=ORIENTED_EDGE('',*,*,#16917,.T.);
#25829=ORIENTED_EDGE('',*,*,#17843,.T.);
#25830=ORIENTED_EDGE('',*,*,#16552,.T.);
#25831=ORIENTED_EDGE('',*,*,#17676,.T.);
#25832=ORIENTED_EDGE('',*,*,#17477,.T.);
#25833=ORIENTED_EDGE('',*,*,#17240,.T.);
#25834=ORIENTED_EDGE('',*,*,#16916,.T.);
#25835=ORIENTED_EDGE('',*,*,#17844,.T.);
#25836=ORIENTED_EDGE('',*,*,#16553,.T.);
#25837=ORIENTED_EDGE('',*,*,#17843,.F.);
#25838=ORIENTED_EDGE('',*,*,#16915,.T.);
#25839=ORIENTED_EDGE('',*,*,#17242,.T.);
#25840=ORIENTED_EDGE('',*,*,#17479,.T.);
#25841=ORIENTED_EDGE('',*,*,#17677,.T.);
#25842=ORIENTED_EDGE('',*,*,#16554,.T.);
#25843=ORIENTED_EDGE('',*,*,#17844,.F.);
#25844=ORIENTED_EDGE('',*,*,#16921,.T.);
#25845=ORIENTED_EDGE('',*,*,#17845,.T.);
#25846=ORIENTED_EDGE('',*,*,#16548,.T.);
#25847=ORIENTED_EDGE('',*,*,#17674,.T.);
#25848=ORIENTED_EDGE('',*,*,#17474,.T.);
#25849=ORIENTED_EDGE('',*,*,#17237,.T.);
#25850=ORIENTED_EDGE('',*,*,#16920,.T.);
#25851=ORIENTED_EDGE('',*,*,#17846,.T.);
#25852=ORIENTED_EDGE('',*,*,#16549,.T.);
#25853=ORIENTED_EDGE('',*,*,#17845,.F.);
#25854=ORIENTED_EDGE('',*,*,#16919,.T.);
#25855=ORIENTED_EDGE('',*,*,#17239,.T.);
#25856=ORIENTED_EDGE('',*,*,#17476,.T.);
#25857=ORIENTED_EDGE('',*,*,#17675,.T.);
#25858=ORIENTED_EDGE('',*,*,#16550,.T.);
#25859=ORIENTED_EDGE('',*,*,#17846,.F.);
#25860=ORIENTED_EDGE('',*,*,#16925,.T.);
#25861=ORIENTED_EDGE('',*,*,#17847,.T.);
#25862=ORIENTED_EDGE('',*,*,#16544,.T.);
#25863=ORIENTED_EDGE('',*,*,#17672,.T.);
#25864=ORIENTED_EDGE('',*,*,#17471,.T.);
#25865=ORIENTED_EDGE('',*,*,#17234,.T.);
#25866=ORIENTED_EDGE('',*,*,#16924,.T.);
#25867=ORIENTED_EDGE('',*,*,#17848,.T.);
#25868=ORIENTED_EDGE('',*,*,#16545,.T.);
#25869=ORIENTED_EDGE('',*,*,#17847,.F.);
#25870=ORIENTED_EDGE('',*,*,#16923,.T.);
#25871=ORIENTED_EDGE('',*,*,#17236,.T.);
#25872=ORIENTED_EDGE('',*,*,#17473,.T.);
#25873=ORIENTED_EDGE('',*,*,#17673,.T.);
#25874=ORIENTED_EDGE('',*,*,#16546,.T.);
#25875=ORIENTED_EDGE('',*,*,#17848,.F.);
#25876=ORIENTED_EDGE('',*,*,#16929,.T.);
#25877=ORIENTED_EDGE('',*,*,#17849,.T.);
#25878=ORIENTED_EDGE('',*,*,#16540,.T.);
#25879=ORIENTED_EDGE('',*,*,#17670,.T.);
#25880=ORIENTED_EDGE('',*,*,#17468,.T.);
#25881=ORIENTED_EDGE('',*,*,#17231,.T.);
#25882=ORIENTED_EDGE('',*,*,#16928,.T.);
#25883=ORIENTED_EDGE('',*,*,#17850,.T.);
#25884=ORIENTED_EDGE('',*,*,#16541,.T.);
#25885=ORIENTED_EDGE('',*,*,#17849,.F.);
#25886=ORIENTED_EDGE('',*,*,#16927,.T.);
#25887=ORIENTED_EDGE('',*,*,#17233,.T.);
#25888=ORIENTED_EDGE('',*,*,#17470,.T.);
#25889=ORIENTED_EDGE('',*,*,#17671,.T.);
#25890=ORIENTED_EDGE('',*,*,#16542,.T.);
#25891=ORIENTED_EDGE('',*,*,#17850,.F.);
#25892=ORIENTED_EDGE('',*,*,#16933,.T.);
#25893=ORIENTED_EDGE('',*,*,#17851,.T.);
#25894=ORIENTED_EDGE('',*,*,#16536,.T.);
#25895=ORIENTED_EDGE('',*,*,#17668,.T.);
#25896=ORIENTED_EDGE('',*,*,#17465,.T.);
#25897=ORIENTED_EDGE('',*,*,#17228,.T.);
#25898=ORIENTED_EDGE('',*,*,#16932,.T.);
#25899=ORIENTED_EDGE('',*,*,#17852,.T.);
#25900=ORIENTED_EDGE('',*,*,#16537,.T.);
#25901=ORIENTED_EDGE('',*,*,#17851,.F.);
#25902=ORIENTED_EDGE('',*,*,#16931,.T.);
#25903=ORIENTED_EDGE('',*,*,#17230,.T.);
#25904=ORIENTED_EDGE('',*,*,#17467,.T.);
#25905=ORIENTED_EDGE('',*,*,#17669,.T.);
#25906=ORIENTED_EDGE('',*,*,#16538,.T.);
#25907=ORIENTED_EDGE('',*,*,#17852,.F.);
#25908=ORIENTED_EDGE('',*,*,#16937,.T.);
#25909=ORIENTED_EDGE('',*,*,#17853,.T.);
#25910=ORIENTED_EDGE('',*,*,#16532,.T.);
#25911=ORIENTED_EDGE('',*,*,#17666,.T.);
#25912=ORIENTED_EDGE('',*,*,#17462,.T.);
#25913=ORIENTED_EDGE('',*,*,#17225,.T.);
#25914=ORIENTED_EDGE('',*,*,#16936,.T.);
#25915=ORIENTED_EDGE('',*,*,#17854,.T.);
#25916=ORIENTED_EDGE('',*,*,#16533,.T.);
#25917=ORIENTED_EDGE('',*,*,#17853,.F.);
#25918=ORIENTED_EDGE('',*,*,#16935,.T.);
#25919=ORIENTED_EDGE('',*,*,#17227,.T.);
#25920=ORIENTED_EDGE('',*,*,#17464,.T.);
#25921=ORIENTED_EDGE('',*,*,#17667,.T.);
#25922=ORIENTED_EDGE('',*,*,#16534,.T.);
#25923=ORIENTED_EDGE('',*,*,#17854,.F.);
#25924=ORIENTED_EDGE('',*,*,#16941,.T.);
#25925=ORIENTED_EDGE('',*,*,#17855,.T.);
#25926=ORIENTED_EDGE('',*,*,#16528,.T.);
#25927=ORIENTED_EDGE('',*,*,#17664,.T.);
#25928=ORIENTED_EDGE('',*,*,#17459,.T.);
#25929=ORIENTED_EDGE('',*,*,#17222,.T.);
#25930=ORIENTED_EDGE('',*,*,#16940,.T.);
#25931=ORIENTED_EDGE('',*,*,#17856,.T.);
#25932=ORIENTED_EDGE('',*,*,#16529,.T.);
#25933=ORIENTED_EDGE('',*,*,#17855,.F.);
#25934=ORIENTED_EDGE('',*,*,#16939,.T.);
#25935=ORIENTED_EDGE('',*,*,#17224,.T.);
#25936=ORIENTED_EDGE('',*,*,#17461,.T.);
#25937=ORIENTED_EDGE('',*,*,#17665,.T.);
#25938=ORIENTED_EDGE('',*,*,#16530,.T.);
#25939=ORIENTED_EDGE('',*,*,#17856,.F.);
#25940=ORIENTED_EDGE('',*,*,#16945,.T.);
#25941=ORIENTED_EDGE('',*,*,#17857,.T.);
#25942=ORIENTED_EDGE('',*,*,#16524,.T.);
#25943=ORIENTED_EDGE('',*,*,#17662,.T.);
#25944=ORIENTED_EDGE('',*,*,#17456,.T.);
#25945=ORIENTED_EDGE('',*,*,#17219,.T.);
#25946=ORIENTED_EDGE('',*,*,#16944,.T.);
#25947=ORIENTED_EDGE('',*,*,#17858,.T.);
#25948=ORIENTED_EDGE('',*,*,#16525,.T.);
#25949=ORIENTED_EDGE('',*,*,#17857,.F.);
#25950=ORIENTED_EDGE('',*,*,#16943,.T.);
#25951=ORIENTED_EDGE('',*,*,#17221,.T.);
#25952=ORIENTED_EDGE('',*,*,#17458,.T.);
#25953=ORIENTED_EDGE('',*,*,#17663,.T.);
#25954=ORIENTED_EDGE('',*,*,#16526,.T.);
#25955=ORIENTED_EDGE('',*,*,#17858,.F.);
#25956=ORIENTED_EDGE('',*,*,#16949,.T.);
#25957=ORIENTED_EDGE('',*,*,#17859,.T.);
#25958=ORIENTED_EDGE('',*,*,#16520,.T.);
#25959=ORIENTED_EDGE('',*,*,#17660,.T.);
#25960=ORIENTED_EDGE('',*,*,#17453,.T.);
#25961=ORIENTED_EDGE('',*,*,#17216,.T.);
#25962=ORIENTED_EDGE('',*,*,#16948,.T.);
#25963=ORIENTED_EDGE('',*,*,#17860,.T.);
#25964=ORIENTED_EDGE('',*,*,#16521,.T.);
#25965=ORIENTED_EDGE('',*,*,#17859,.F.);
#25966=ORIENTED_EDGE('',*,*,#16947,.T.);
#25967=ORIENTED_EDGE('',*,*,#17218,.T.);
#25968=ORIENTED_EDGE('',*,*,#17455,.T.);
#25969=ORIENTED_EDGE('',*,*,#17661,.T.);
#25970=ORIENTED_EDGE('',*,*,#16522,.T.);
#25971=ORIENTED_EDGE('',*,*,#17860,.F.);
#25972=ORIENTED_EDGE('',*,*,#16953,.T.);
#25973=ORIENTED_EDGE('',*,*,#17861,.T.);
#25974=ORIENTED_EDGE('',*,*,#16516,.T.);
#25975=ORIENTED_EDGE('',*,*,#17658,.T.);
#25976=ORIENTED_EDGE('',*,*,#17450,.T.);
#25977=ORIENTED_EDGE('',*,*,#17213,.T.);
#25978=ORIENTED_EDGE('',*,*,#16952,.T.);
#25979=ORIENTED_EDGE('',*,*,#17862,.T.);
#25980=ORIENTED_EDGE('',*,*,#16517,.T.);
#25981=ORIENTED_EDGE('',*,*,#17861,.F.);
#25982=ORIENTED_EDGE('',*,*,#16951,.T.);
#25983=ORIENTED_EDGE('',*,*,#17215,.T.);
#25984=ORIENTED_EDGE('',*,*,#17452,.T.);
#25985=ORIENTED_EDGE('',*,*,#17659,.T.);
#25986=ORIENTED_EDGE('',*,*,#16518,.T.);
#25987=ORIENTED_EDGE('',*,*,#17862,.F.);
#25988=ORIENTED_EDGE('',*,*,#16957,.T.);
#25989=ORIENTED_EDGE('',*,*,#17863,.T.);
#25990=ORIENTED_EDGE('',*,*,#16512,.T.);
#25991=ORIENTED_EDGE('',*,*,#17656,.T.);
#25992=ORIENTED_EDGE('',*,*,#17447,.T.);
#25993=ORIENTED_EDGE('',*,*,#17210,.T.);
#25994=ORIENTED_EDGE('',*,*,#16956,.T.);
#25995=ORIENTED_EDGE('',*,*,#17864,.T.);
#25996=ORIENTED_EDGE('',*,*,#16513,.T.);
#25997=ORIENTED_EDGE('',*,*,#17863,.F.);
#25998=ORIENTED_EDGE('',*,*,#16955,.T.);
#25999=ORIENTED_EDGE('',*,*,#17212,.T.);
#26000=ORIENTED_EDGE('',*,*,#17449,.T.);
#26001=ORIENTED_EDGE('',*,*,#17657,.T.);
#26002=ORIENTED_EDGE('',*,*,#16514,.T.);
#26003=ORIENTED_EDGE('',*,*,#17864,.F.);
#26004=ORIENTED_EDGE('',*,*,#16961,.T.);
#26005=ORIENTED_EDGE('',*,*,#17865,.T.);
#26006=ORIENTED_EDGE('',*,*,#16508,.T.);
#26007=ORIENTED_EDGE('',*,*,#17654,.T.);
#26008=ORIENTED_EDGE('',*,*,#17444,.T.);
#26009=ORIENTED_EDGE('',*,*,#17207,.T.);
#26010=ORIENTED_EDGE('',*,*,#16960,.T.);
#26011=ORIENTED_EDGE('',*,*,#17866,.T.);
#26012=ORIENTED_EDGE('',*,*,#16509,.T.);
#26013=ORIENTED_EDGE('',*,*,#17865,.F.);
#26014=ORIENTED_EDGE('',*,*,#16959,.T.);
#26015=ORIENTED_EDGE('',*,*,#17209,.T.);
#26016=ORIENTED_EDGE('',*,*,#17446,.T.);
#26017=ORIENTED_EDGE('',*,*,#17655,.T.);
#26018=ORIENTED_EDGE('',*,*,#16510,.T.);
#26019=ORIENTED_EDGE('',*,*,#17866,.F.);
#26020=ORIENTED_EDGE('',*,*,#16965,.T.);
#26021=ORIENTED_EDGE('',*,*,#17867,.T.);
#26022=ORIENTED_EDGE('',*,*,#16504,.T.);
#26023=ORIENTED_EDGE('',*,*,#17652,.T.);
#26024=ORIENTED_EDGE('',*,*,#17441,.T.);
#26025=ORIENTED_EDGE('',*,*,#17204,.T.);
#26026=ORIENTED_EDGE('',*,*,#16964,.T.);
#26027=ORIENTED_EDGE('',*,*,#17868,.T.);
#26028=ORIENTED_EDGE('',*,*,#16505,.T.);
#26029=ORIENTED_EDGE('',*,*,#17867,.F.);
#26030=ORIENTED_EDGE('',*,*,#16963,.T.);
#26031=ORIENTED_EDGE('',*,*,#17206,.T.);
#26032=ORIENTED_EDGE('',*,*,#17443,.T.);
#26033=ORIENTED_EDGE('',*,*,#17653,.T.);
#26034=ORIENTED_EDGE('',*,*,#16506,.T.);
#26035=ORIENTED_EDGE('',*,*,#17868,.F.);
#26036=ORIENTED_EDGE('',*,*,#16969,.T.);
#26037=ORIENTED_EDGE('',*,*,#17869,.T.);
#26038=ORIENTED_EDGE('',*,*,#16805,.T.);
#26039=ORIENTED_EDGE('',*,*,#17650,.T.);
#26040=ORIENTED_EDGE('',*,*,#17438,.T.);
#26041=ORIENTED_EDGE('',*,*,#17201,.T.);
#26042=ORIENTED_EDGE('',*,*,#16968,.T.);
#26043=ORIENTED_EDGE('',*,*,#17870,.T.);
#26044=ORIENTED_EDGE('',*,*,#16501,.T.);
#26045=ORIENTED_EDGE('',*,*,#16806,.T.);
#26046=ORIENTED_EDGE('',*,*,#17869,.F.);
#26047=ORIENTED_EDGE('',*,*,#16967,.T.);
#26048=ORIENTED_EDGE('',*,*,#17203,.T.);
#26049=ORIENTED_EDGE('',*,*,#17440,.T.);
#26050=ORIENTED_EDGE('',*,*,#17651,.T.);
#26051=ORIENTED_EDGE('',*,*,#16502,.T.);
#26052=ORIENTED_EDGE('',*,*,#17870,.F.);
#26053=ORIENTED_EDGE('',*,*,#16973,.T.);
#26054=ORIENTED_EDGE('',*,*,#17871,.T.);
#26055=ORIENTED_EDGE('',*,*,#16801,.T.);
#26056=ORIENTED_EDGE('',*,*,#17648,.T.);
#26057=ORIENTED_EDGE('',*,*,#17435,.T.);
#26058=ORIENTED_EDGE('',*,*,#17198,.T.);
#26059=ORIENTED_EDGE('',*,*,#16972,.T.);
#26060=ORIENTED_EDGE('',*,*,#17872,.T.);
#26061=ORIENTED_EDGE('',*,*,#16802,.T.);
#26062=ORIENTED_EDGE('',*,*,#17871,.F.);
#26063=ORIENTED_EDGE('',*,*,#16971,.T.);
#26064=ORIENTED_EDGE('',*,*,#17200,.T.);
#26065=ORIENTED_EDGE('',*,*,#17437,.T.);
#26066=ORIENTED_EDGE('',*,*,#17649,.T.);
#26067=ORIENTED_EDGE('',*,*,#16803,.T.);
#26068=ORIENTED_EDGE('',*,*,#17872,.F.);
#26069=ORIENTED_EDGE('',*,*,#16977,.T.);
#26070=ORIENTED_EDGE('',*,*,#17873,.T.);
#26071=ORIENTED_EDGE('',*,*,#16797,.T.);
#26072=ORIENTED_EDGE('',*,*,#17646,.T.);
#26073=ORIENTED_EDGE('',*,*,#17432,.T.);
#26074=ORIENTED_EDGE('',*,*,#17195,.T.);
#26075=ORIENTED_EDGE('',*,*,#16976,.T.);
#26076=ORIENTED_EDGE('',*,*,#17874,.T.);
#26077=ORIENTED_EDGE('',*,*,#16798,.T.);
#26078=ORIENTED_EDGE('',*,*,#17873,.F.);
#26079=ORIENTED_EDGE('',*,*,#16975,.T.);
#26080=ORIENTED_EDGE('',*,*,#17197,.T.);
#26081=ORIENTED_EDGE('',*,*,#17434,.T.);
#26082=ORIENTED_EDGE('',*,*,#17647,.T.);
#26083=ORIENTED_EDGE('',*,*,#16799,.T.);
#26084=ORIENTED_EDGE('',*,*,#17874,.F.);
#26085=ORIENTED_EDGE('',*,*,#16981,.T.);
#26086=ORIENTED_EDGE('',*,*,#17875,.T.);
#26087=ORIENTED_EDGE('',*,*,#16793,.T.);
#26088=ORIENTED_EDGE('',*,*,#17644,.T.);
#26089=ORIENTED_EDGE('',*,*,#17429,.T.);
#26090=ORIENTED_EDGE('',*,*,#17192,.T.);
#26091=ORIENTED_EDGE('',*,*,#16980,.T.);
#26092=ORIENTED_EDGE('',*,*,#17876,.T.);
#26093=ORIENTED_EDGE('',*,*,#16794,.T.);
#26094=ORIENTED_EDGE('',*,*,#17875,.F.);
#26095=ORIENTED_EDGE('',*,*,#16979,.T.);
#26096=ORIENTED_EDGE('',*,*,#17194,.T.);
#26097=ORIENTED_EDGE('',*,*,#17431,.T.);
#26098=ORIENTED_EDGE('',*,*,#17645,.T.);
#26099=ORIENTED_EDGE('',*,*,#16795,.T.);
#26100=ORIENTED_EDGE('',*,*,#17876,.F.);
#26101=ORIENTED_EDGE('',*,*,#16985,.T.);
#26102=ORIENTED_EDGE('',*,*,#17877,.T.);
#26103=ORIENTED_EDGE('',*,*,#16789,.T.);
#26104=ORIENTED_EDGE('',*,*,#17642,.T.);
#26105=ORIENTED_EDGE('',*,*,#17426,.T.);
#26106=ORIENTED_EDGE('',*,*,#17189,.T.);
#26107=ORIENTED_EDGE('',*,*,#16984,.T.);
#26108=ORIENTED_EDGE('',*,*,#17878,.T.);
#26109=ORIENTED_EDGE('',*,*,#16790,.T.);
#26110=ORIENTED_EDGE('',*,*,#17877,.F.);
#26111=ORIENTED_EDGE('',*,*,#16983,.T.);
#26112=ORIENTED_EDGE('',*,*,#17191,.T.);
#26113=ORIENTED_EDGE('',*,*,#17428,.T.);
#26114=ORIENTED_EDGE('',*,*,#17643,.T.);
#26115=ORIENTED_EDGE('',*,*,#16791,.T.);
#26116=ORIENTED_EDGE('',*,*,#17878,.F.);
#26117=ORIENTED_EDGE('',*,*,#16989,.T.);
#26118=ORIENTED_EDGE('',*,*,#17879,.T.);
#26119=ORIENTED_EDGE('',*,*,#16785,.T.);
#26120=ORIENTED_EDGE('',*,*,#17640,.T.);
#26121=ORIENTED_EDGE('',*,*,#17423,.T.);
#26122=ORIENTED_EDGE('',*,*,#17186,.T.);
#26123=ORIENTED_EDGE('',*,*,#16988,.T.);
#26124=ORIENTED_EDGE('',*,*,#17880,.T.);
#26125=ORIENTED_EDGE('',*,*,#16786,.T.);
#26126=ORIENTED_EDGE('',*,*,#17879,.F.);
#26127=ORIENTED_EDGE('',*,*,#16987,.T.);
#26128=ORIENTED_EDGE('',*,*,#17188,.T.);
#26129=ORIENTED_EDGE('',*,*,#17425,.T.);
#26130=ORIENTED_EDGE('',*,*,#17641,.T.);
#26131=ORIENTED_EDGE('',*,*,#16787,.T.);
#26132=ORIENTED_EDGE('',*,*,#17880,.F.);
#26133=ORIENTED_EDGE('',*,*,#16993,.T.);
#26134=ORIENTED_EDGE('',*,*,#17881,.T.);
#26135=ORIENTED_EDGE('',*,*,#16781,.T.);
#26136=ORIENTED_EDGE('',*,*,#17638,.T.);
#26137=ORIENTED_EDGE('',*,*,#17420,.T.);
#26138=ORIENTED_EDGE('',*,*,#17183,.T.);
#26139=ORIENTED_EDGE('',*,*,#16992,.T.);
#26140=ORIENTED_EDGE('',*,*,#17882,.T.);
#26141=ORIENTED_EDGE('',*,*,#16782,.T.);
#26142=ORIENTED_EDGE('',*,*,#17881,.F.);
#26143=ORIENTED_EDGE('',*,*,#16991,.T.);
#26144=ORIENTED_EDGE('',*,*,#17185,.T.);
#26145=ORIENTED_EDGE('',*,*,#17422,.T.);
#26146=ORIENTED_EDGE('',*,*,#17639,.T.);
#26147=ORIENTED_EDGE('',*,*,#16783,.T.);
#26148=ORIENTED_EDGE('',*,*,#17882,.F.);
#26149=ORIENTED_EDGE('',*,*,#16997,.T.);
#26150=ORIENTED_EDGE('',*,*,#17883,.T.);
#26151=ORIENTED_EDGE('',*,*,#16777,.T.);
#26152=ORIENTED_EDGE('',*,*,#17636,.T.);
#26153=ORIENTED_EDGE('',*,*,#17417,.T.);
#26154=ORIENTED_EDGE('',*,*,#17180,.T.);
#26155=ORIENTED_EDGE('',*,*,#16996,.T.);
#26156=ORIENTED_EDGE('',*,*,#17884,.T.);
#26157=ORIENTED_EDGE('',*,*,#16778,.T.);
#26158=ORIENTED_EDGE('',*,*,#17883,.F.);
#26159=ORIENTED_EDGE('',*,*,#16995,.T.);
#26160=ORIENTED_EDGE('',*,*,#17182,.T.);
#26161=ORIENTED_EDGE('',*,*,#17419,.T.);
#26162=ORIENTED_EDGE('',*,*,#17637,.T.);
#26163=ORIENTED_EDGE('',*,*,#16779,.T.);
#26164=ORIENTED_EDGE('',*,*,#17884,.F.);
#26165=ORIENTED_EDGE('',*,*,#17001,.T.);
#26166=ORIENTED_EDGE('',*,*,#17885,.T.);
#26167=ORIENTED_EDGE('',*,*,#16773,.T.);
#26168=ORIENTED_EDGE('',*,*,#17634,.T.);
#26169=ORIENTED_EDGE('',*,*,#17414,.T.);
#26170=ORIENTED_EDGE('',*,*,#17177,.T.);
#26171=ORIENTED_EDGE('',*,*,#17000,.T.);
#26172=ORIENTED_EDGE('',*,*,#17886,.T.);
#26173=ORIENTED_EDGE('',*,*,#16774,.T.);
#26174=ORIENTED_EDGE('',*,*,#17885,.F.);
#26175=ORIENTED_EDGE('',*,*,#16999,.T.);
#26176=ORIENTED_EDGE('',*,*,#17179,.T.);
#26177=ORIENTED_EDGE('',*,*,#17416,.T.);
#26178=ORIENTED_EDGE('',*,*,#17635,.T.);
#26179=ORIENTED_EDGE('',*,*,#16775,.T.);
#26180=ORIENTED_EDGE('',*,*,#17886,.F.);
#26181=ORIENTED_EDGE('',*,*,#17005,.T.);
#26182=ORIENTED_EDGE('',*,*,#17887,.T.);
#26183=ORIENTED_EDGE('',*,*,#16769,.T.);
#26184=ORIENTED_EDGE('',*,*,#17632,.T.);
#26185=ORIENTED_EDGE('',*,*,#17411,.T.);
#26186=ORIENTED_EDGE('',*,*,#17174,.T.);
#26187=ORIENTED_EDGE('',*,*,#17004,.T.);
#26188=ORIENTED_EDGE('',*,*,#17888,.T.);
#26189=ORIENTED_EDGE('',*,*,#16770,.T.);
#26190=ORIENTED_EDGE('',*,*,#17887,.F.);
#26191=ORIENTED_EDGE('',*,*,#17003,.T.);
#26192=ORIENTED_EDGE('',*,*,#17176,.T.);
#26193=ORIENTED_EDGE('',*,*,#17413,.T.);
#26194=ORIENTED_EDGE('',*,*,#17633,.T.);
#26195=ORIENTED_EDGE('',*,*,#16771,.T.);
#26196=ORIENTED_EDGE('',*,*,#17888,.F.);
#26197=ORIENTED_EDGE('',*,*,#17009,.T.);
#26198=ORIENTED_EDGE('',*,*,#17889,.T.);
#26199=ORIENTED_EDGE('',*,*,#16765,.T.);
#26200=ORIENTED_EDGE('',*,*,#17630,.T.);
#26201=ORIENTED_EDGE('',*,*,#17408,.T.);
#26202=ORIENTED_EDGE('',*,*,#17171,.T.);
#26203=ORIENTED_EDGE('',*,*,#17008,.T.);
#26204=ORIENTED_EDGE('',*,*,#17890,.T.);
#26205=ORIENTED_EDGE('',*,*,#16766,.T.);
#26206=ORIENTED_EDGE('',*,*,#17889,.F.);
#26207=ORIENTED_EDGE('',*,*,#17007,.T.);
#26208=ORIENTED_EDGE('',*,*,#17173,.T.);
#26209=ORIENTED_EDGE('',*,*,#17410,.T.);
#26210=ORIENTED_EDGE('',*,*,#17631,.T.);
#26211=ORIENTED_EDGE('',*,*,#16767,.T.);
#26212=ORIENTED_EDGE('',*,*,#17890,.F.);
#26213=ORIENTED_EDGE('',*,*,#17013,.T.);
#26214=ORIENTED_EDGE('',*,*,#17891,.T.);
#26215=ORIENTED_EDGE('',*,*,#16761,.T.);
#26216=ORIENTED_EDGE('',*,*,#17628,.T.);
#26217=ORIENTED_EDGE('',*,*,#17405,.T.);
#26218=ORIENTED_EDGE('',*,*,#17168,.T.);
#26219=ORIENTED_EDGE('',*,*,#17012,.T.);
#26220=ORIENTED_EDGE('',*,*,#17892,.T.);
#26221=ORIENTED_EDGE('',*,*,#16762,.T.);
#26222=ORIENTED_EDGE('',*,*,#17891,.F.);
#26223=ORIENTED_EDGE('',*,*,#17011,.T.);
#26224=ORIENTED_EDGE('',*,*,#17170,.T.);
#26225=ORIENTED_EDGE('',*,*,#17407,.T.);
#26226=ORIENTED_EDGE('',*,*,#17629,.T.);
#26227=ORIENTED_EDGE('',*,*,#16763,.T.);
#26228=ORIENTED_EDGE('',*,*,#17892,.F.);
#26229=ORIENTED_EDGE('',*,*,#17017,.T.);
#26230=ORIENTED_EDGE('',*,*,#17893,.T.);
#26231=ORIENTED_EDGE('',*,*,#16757,.T.);
#26232=ORIENTED_EDGE('',*,*,#17626,.T.);
#26233=ORIENTED_EDGE('',*,*,#17402,.T.);
#26234=ORIENTED_EDGE('',*,*,#17165,.T.);
#26235=ORIENTED_EDGE('',*,*,#17016,.T.);
#26236=ORIENTED_EDGE('',*,*,#17894,.T.);
#26237=ORIENTED_EDGE('',*,*,#16758,.T.);
#26238=ORIENTED_EDGE('',*,*,#17893,.F.);
#26239=ORIENTED_EDGE('',*,*,#17015,.T.);
#26240=ORIENTED_EDGE('',*,*,#17167,.T.);
#26241=ORIENTED_EDGE('',*,*,#17404,.T.);
#26242=ORIENTED_EDGE('',*,*,#17627,.T.);
#26243=ORIENTED_EDGE('',*,*,#16759,.T.);
#26244=ORIENTED_EDGE('',*,*,#17894,.F.);
#26245=ORIENTED_EDGE('',*,*,#17021,.T.);
#26246=ORIENTED_EDGE('',*,*,#17895,.T.);
#26247=ORIENTED_EDGE('',*,*,#16753,.T.);
#26248=ORIENTED_EDGE('',*,*,#17624,.T.);
#26249=ORIENTED_EDGE('',*,*,#17399,.T.);
#26250=ORIENTED_EDGE('',*,*,#17162,.T.);
#26251=ORIENTED_EDGE('',*,*,#17020,.T.);
#26252=ORIENTED_EDGE('',*,*,#17896,.T.);
#26253=ORIENTED_EDGE('',*,*,#16754,.T.);
#26254=ORIENTED_EDGE('',*,*,#17895,.F.);
#26255=ORIENTED_EDGE('',*,*,#17019,.T.);
#26256=ORIENTED_EDGE('',*,*,#17164,.T.);
#26257=ORIENTED_EDGE('',*,*,#17401,.T.);
#26258=ORIENTED_EDGE('',*,*,#17625,.T.);
#26259=ORIENTED_EDGE('',*,*,#16755,.T.);
#26260=ORIENTED_EDGE('',*,*,#17896,.F.);
#26261=ORIENTED_EDGE('',*,*,#17025,.T.);
#26262=ORIENTED_EDGE('',*,*,#17897,.T.);
#26263=ORIENTED_EDGE('',*,*,#16749,.T.);
#26264=ORIENTED_EDGE('',*,*,#17622,.T.);
#26265=ORIENTED_EDGE('',*,*,#17396,.T.);
#26266=ORIENTED_EDGE('',*,*,#17159,.T.);
#26267=ORIENTED_EDGE('',*,*,#17024,.T.);
#26268=ORIENTED_EDGE('',*,*,#17898,.T.);
#26269=ORIENTED_EDGE('',*,*,#16750,.T.);
#26270=ORIENTED_EDGE('',*,*,#17897,.F.);
#26271=ORIENTED_EDGE('',*,*,#17023,.T.);
#26272=ORIENTED_EDGE('',*,*,#17161,.T.);
#26273=ORIENTED_EDGE('',*,*,#17398,.T.);
#26274=ORIENTED_EDGE('',*,*,#17623,.T.);
#26275=ORIENTED_EDGE('',*,*,#16751,.T.);
#26276=ORIENTED_EDGE('',*,*,#17898,.F.);
#26277=ORIENTED_EDGE('',*,*,#17029,.T.);
#26278=ORIENTED_EDGE('',*,*,#17899,.T.);
#26279=ORIENTED_EDGE('',*,*,#16745,.T.);
#26280=ORIENTED_EDGE('',*,*,#17620,.T.);
#26281=ORIENTED_EDGE('',*,*,#17393,.T.);
#26282=ORIENTED_EDGE('',*,*,#17156,.T.);
#26283=ORIENTED_EDGE('',*,*,#17028,.T.);
#26284=ORIENTED_EDGE('',*,*,#17900,.T.);
#26285=ORIENTED_EDGE('',*,*,#16746,.T.);
#26286=ORIENTED_EDGE('',*,*,#17899,.F.);
#26287=ORIENTED_EDGE('',*,*,#17027,.T.);
#26288=ORIENTED_EDGE('',*,*,#17158,.T.);
#26289=ORIENTED_EDGE('',*,*,#17395,.T.);
#26290=ORIENTED_EDGE('',*,*,#17621,.T.);
#26291=ORIENTED_EDGE('',*,*,#16747,.T.);
#26292=ORIENTED_EDGE('',*,*,#17900,.F.);
#26293=ORIENTED_EDGE('',*,*,#17033,.T.);
#26294=ORIENTED_EDGE('',*,*,#17901,.T.);
#26295=ORIENTED_EDGE('',*,*,#16741,.T.);
#26296=ORIENTED_EDGE('',*,*,#17618,.T.);
#26297=ORIENTED_EDGE('',*,*,#17390,.T.);
#26298=ORIENTED_EDGE('',*,*,#17153,.T.);
#26299=ORIENTED_EDGE('',*,*,#17032,.T.);
#26300=ORIENTED_EDGE('',*,*,#17902,.T.);
#26301=ORIENTED_EDGE('',*,*,#16742,.T.);
#26302=ORIENTED_EDGE('',*,*,#17901,.F.);
#26303=ORIENTED_EDGE('',*,*,#17031,.T.);
#26304=ORIENTED_EDGE('',*,*,#17155,.T.);
#26305=ORIENTED_EDGE('',*,*,#17392,.T.);
#26306=ORIENTED_EDGE('',*,*,#17619,.T.);
#26307=ORIENTED_EDGE('',*,*,#16743,.T.);
#26308=ORIENTED_EDGE('',*,*,#17902,.F.);
#26309=ORIENTED_EDGE('',*,*,#17037,.T.);
#26310=ORIENTED_EDGE('',*,*,#17903,.T.);
#26311=ORIENTED_EDGE('',*,*,#16737,.T.);
#26312=ORIENTED_EDGE('',*,*,#17616,.T.);
#26313=ORIENTED_EDGE('',*,*,#17387,.T.);
#26314=ORIENTED_EDGE('',*,*,#17150,.T.);
#26315=ORIENTED_EDGE('',*,*,#17036,.T.);
#26316=ORIENTED_EDGE('',*,*,#17904,.T.);
#26317=ORIENTED_EDGE('',*,*,#16738,.T.);
#26318=ORIENTED_EDGE('',*,*,#17903,.F.);
#26319=ORIENTED_EDGE('',*,*,#17035,.T.);
#26320=ORIENTED_EDGE('',*,*,#17152,.T.);
#26321=ORIENTED_EDGE('',*,*,#17389,.T.);
#26322=ORIENTED_EDGE('',*,*,#17617,.T.);
#26323=ORIENTED_EDGE('',*,*,#16739,.T.);
#26324=ORIENTED_EDGE('',*,*,#17904,.F.);
#26325=ORIENTED_EDGE('',*,*,#17041,.T.);
#26326=ORIENTED_EDGE('',*,*,#17905,.T.);
#26327=ORIENTED_EDGE('',*,*,#16733,.T.);
#26328=ORIENTED_EDGE('',*,*,#17614,.T.);
#26329=ORIENTED_EDGE('',*,*,#17384,.T.);
#26330=ORIENTED_EDGE('',*,*,#17147,.T.);
#26331=ORIENTED_EDGE('',*,*,#17040,.T.);
#26332=ORIENTED_EDGE('',*,*,#17906,.T.);
#26333=ORIENTED_EDGE('',*,*,#16734,.T.);
#26334=ORIENTED_EDGE('',*,*,#17905,.F.);
#26335=ORIENTED_EDGE('',*,*,#17039,.T.);
#26336=ORIENTED_EDGE('',*,*,#17149,.T.);
#26337=ORIENTED_EDGE('',*,*,#17386,.T.);
#26338=ORIENTED_EDGE('',*,*,#17615,.T.);
#26339=ORIENTED_EDGE('',*,*,#16735,.T.);
#26340=ORIENTED_EDGE('',*,*,#17906,.F.);
#26341=ORIENTED_EDGE('',*,*,#17045,.T.);
#26342=ORIENTED_EDGE('',*,*,#17907,.T.);
#26343=ORIENTED_EDGE('',*,*,#16729,.T.);
#26344=ORIENTED_EDGE('',*,*,#17612,.T.);
#26345=ORIENTED_EDGE('',*,*,#17381,.T.);
#26346=ORIENTED_EDGE('',*,*,#17144,.T.);
#26347=ORIENTED_EDGE('',*,*,#17044,.T.);
#26348=ORIENTED_EDGE('',*,*,#17908,.T.);
#26349=ORIENTED_EDGE('',*,*,#16730,.T.);
#26350=ORIENTED_EDGE('',*,*,#17907,.F.);
#26351=ORIENTED_EDGE('',*,*,#17043,.T.);
#26352=ORIENTED_EDGE('',*,*,#17146,.T.);
#26353=ORIENTED_EDGE('',*,*,#17383,.T.);
#26354=ORIENTED_EDGE('',*,*,#17613,.T.);
#26355=ORIENTED_EDGE('',*,*,#16731,.T.);
#26356=ORIENTED_EDGE('',*,*,#17908,.F.);
#26357=ORIENTED_EDGE('',*,*,#17048,.T.);
#26358=ORIENTED_EDGE('',*,*,#16452,.T.);
#26359=ORIENTED_EDGE('',*,*,#16726,.T.);
#26360=ORIENTED_EDGE('',*,*,#17610,.T.);
#26361=ORIENTED_EDGE('',*,*,#17378,.T.);
#26362=ORIENTED_EDGE('',*,*,#17141,.T.);
#26363=ORIENTED_EDGE('',*,*,#17047,.T.);
#26364=ORIENTED_EDGE('',*,*,#17143,.T.);
#26365=ORIENTED_EDGE('',*,*,#17380,.T.);
#26366=ORIENTED_EDGE('',*,*,#17611,.T.);
#26367=ORIENTED_EDGE('',*,*,#16727,.T.);
#26368=ORIENTED_EDGE('',*,*,#16450,.F.);
#26369=ORIENTED_EDGE('',*,*,#17051,.T.);
#26370=ORIENTED_EDGE('',*,*,#16448,.T.);
#26371=ORIENTED_EDGE('',*,*,#16723,.T.);
#26372=ORIENTED_EDGE('',*,*,#17608,.T.);
#26373=ORIENTED_EDGE('',*,*,#17375,.T.);
#26374=ORIENTED_EDGE('',*,*,#17138,.T.);
#26375=ORIENTED_EDGE('',*,*,#17050,.T.);
#26376=ORIENTED_EDGE('',*,*,#17140,.T.);
#26377=ORIENTED_EDGE('',*,*,#17377,.T.);
#26378=ORIENTED_EDGE('',*,*,#17609,.T.);
#26379=ORIENTED_EDGE('',*,*,#16724,.T.);
#26380=ORIENTED_EDGE('',*,*,#16446,.F.);
#26381=ORIENTED_EDGE('',*,*,#17054,.T.);
#26382=ORIENTED_EDGE('',*,*,#16444,.T.);
#26383=ORIENTED_EDGE('',*,*,#16720,.T.);
#26384=ORIENTED_EDGE('',*,*,#17606,.T.);
#26385=ORIENTED_EDGE('',*,*,#17372,.T.);
#26386=ORIENTED_EDGE('',*,*,#17135,.T.);
#26387=ORIENTED_EDGE('',*,*,#17053,.T.);
#26388=ORIENTED_EDGE('',*,*,#17137,.T.);
#26389=ORIENTED_EDGE('',*,*,#17374,.T.);
#26390=ORIENTED_EDGE('',*,*,#17607,.T.);
#26391=ORIENTED_EDGE('',*,*,#16721,.T.);
#26392=ORIENTED_EDGE('',*,*,#16442,.F.);
#26393=ORIENTED_EDGE('',*,*,#17057,.T.);
#26394=ORIENTED_EDGE('',*,*,#16440,.T.);
#26395=ORIENTED_EDGE('',*,*,#16717,.T.);
#26396=ORIENTED_EDGE('',*,*,#17604,.T.);
#26397=ORIENTED_EDGE('',*,*,#17369,.T.);
#26398=ORIENTED_EDGE('',*,*,#17132,.T.);
#26399=ORIENTED_EDGE('',*,*,#17056,.T.);
#26400=ORIENTED_EDGE('',*,*,#17134,.T.);
#26401=ORIENTED_EDGE('',*,*,#17371,.T.);
#26402=ORIENTED_EDGE('',*,*,#17605,.T.);
#26403=ORIENTED_EDGE('',*,*,#16718,.T.);
#26404=ORIENTED_EDGE('',*,*,#16438,.F.);
#26405=ORIENTED_EDGE('',*,*,#17060,.T.);
#26406=ORIENTED_EDGE('',*,*,#16436,.T.);
#26407=ORIENTED_EDGE('',*,*,#16714,.T.);
#26408=ORIENTED_EDGE('',*,*,#17602,.T.);
#26409=ORIENTED_EDGE('',*,*,#17366,.T.);
#26410=ORIENTED_EDGE('',*,*,#17129,.T.);
#26411=ORIENTED_EDGE('',*,*,#17059,.T.);
#26412=ORIENTED_EDGE('',*,*,#17131,.T.);
#26413=ORIENTED_EDGE('',*,*,#17368,.T.);
#26414=ORIENTED_EDGE('',*,*,#17603,.T.);
#26415=ORIENTED_EDGE('',*,*,#16715,.T.);
#26416=ORIENTED_EDGE('',*,*,#16434,.F.);
#26417=ORIENTED_EDGE('',*,*,#17063,.T.);
#26418=ORIENTED_EDGE('',*,*,#16432,.T.);
#26419=ORIENTED_EDGE('',*,*,#16711,.T.);
#26420=ORIENTED_EDGE('',*,*,#17599,.T.);
#26421=ORIENTED_EDGE('',*,*,#17362,.T.);
#26422=ORIENTED_EDGE('',*,*,#17125,.T.);
#26423=ORIENTED_EDGE('',*,*,#17062,.T.);
#26424=ORIENTED_EDGE('',*,*,#17128,.T.);
#26425=ORIENTED_EDGE('',*,*,#17365,.T.);
#26426=ORIENTED_EDGE('',*,*,#17601,.T.);
#26427=ORIENTED_EDGE('',*,*,#16712,.T.);
#26428=ORIENTED_EDGE('',*,*,#16430,.F.);
#26429=ORIENTED_EDGE('',*,*,#17909,.F.);
#26430=ORIENTED_EDGE('',*,*,#17910,.F.);
#26431=ORIENTED_EDGE('',*,*,#17911,.T.);
#26432=ORIENTED_EDGE('',*,*,#17912,.T.);
#26433=ORIENTED_EDGE('',*,*,#17911,.F.);
#26434=ORIENTED_EDGE('',*,*,#17913,.F.);
#26435=ORIENTED_EDGE('',*,*,#17914,.F.);
#26436=ORIENTED_EDGE('',*,*,#17915,.F.);
#26437=ORIENTED_EDGE('',*,*,#17916,.F.);
#26438=ORIENTED_EDGE('',*,*,#17909,.T.);
#26439=ORIENTED_EDGE('',*,*,#17917,.F.);
#26440=ORIENTED_EDGE('',*,*,#17918,.F.);
#26441=ORIENTED_EDGE('',*,*,#17919,.F.);
#26442=ORIENTED_EDGE('',*,*,#17915,.T.);
#26443=ORIENTED_EDGE('',*,*,#17920,.F.);
#26444=ORIENTED_EDGE('',*,*,#17921,.F.);
#26445=ORIENTED_EDGE('',*,*,#17922,.F.);
#26446=ORIENTED_EDGE('',*,*,#17918,.T.);
#26447=ORIENTED_EDGE('',*,*,#17923,.F.);
#26448=ORIENTED_EDGE('',*,*,#17924,.F.);
#26449=ORIENTED_EDGE('',*,*,#17925,.F.);
#26450=ORIENTED_EDGE('',*,*,#17921,.T.);
#26451=ORIENTED_EDGE('',*,*,#17926,.F.);
#26452=ORIENTED_EDGE('',*,*,#17927,.F.);
#26453=ORIENTED_EDGE('',*,*,#17928,.F.);
#26454=ORIENTED_EDGE('',*,*,#17924,.T.);
#26455=ORIENTED_EDGE('',*,*,#17929,.F.);
#26456=ORIENTED_EDGE('',*,*,#17930,.F.);
#26457=ORIENTED_EDGE('',*,*,#17931,.F.);
#26458=ORIENTED_EDGE('',*,*,#17927,.T.);
#26459=ORIENTED_EDGE('',*,*,#17932,.F.);
#26460=ORIENTED_EDGE('',*,*,#17933,.F.);
#26461=ORIENTED_EDGE('',*,*,#17934,.F.);
#26462=ORIENTED_EDGE('',*,*,#17930,.T.);
#26463=ORIENTED_EDGE('',*,*,#17935,.F.);
#26464=ORIENTED_EDGE('',*,*,#17936,.F.);
#26465=ORIENTED_EDGE('',*,*,#17937,.F.);
#26466=ORIENTED_EDGE('',*,*,#17933,.T.);
#26467=ORIENTED_EDGE('',*,*,#17938,.F.);
#26468=ORIENTED_EDGE('',*,*,#17939,.F.);
#26469=ORIENTED_EDGE('',*,*,#17940,.F.);
#26470=ORIENTED_EDGE('',*,*,#17936,.T.);
#26471=ORIENTED_EDGE('',*,*,#17941,.F.);
#26472=ORIENTED_EDGE('',*,*,#17942,.F.);
#26473=ORIENTED_EDGE('',*,*,#17943,.F.);
#26474=ORIENTED_EDGE('',*,*,#17939,.T.);
#26475=ORIENTED_EDGE('',*,*,#17944,.F.);
#26476=ORIENTED_EDGE('',*,*,#17945,.F.);
#26477=ORIENTED_EDGE('',*,*,#17946,.F.);
#26478=ORIENTED_EDGE('',*,*,#17942,.T.);
#26479=ORIENTED_EDGE('',*,*,#17947,.F.);
#26480=ORIENTED_EDGE('',*,*,#17948,.F.);
#26481=ORIENTED_EDGE('',*,*,#17949,.F.);
#26482=ORIENTED_EDGE('',*,*,#17945,.T.);
#26483=ORIENTED_EDGE('',*,*,#17950,.F.);
#26484=ORIENTED_EDGE('',*,*,#17951,.F.);
#26485=ORIENTED_EDGE('',*,*,#17952,.F.);
#26486=ORIENTED_EDGE('',*,*,#17948,.T.);
#26487=ORIENTED_EDGE('',*,*,#17953,.F.);
#26488=ORIENTED_EDGE('',*,*,#17954,.F.);
#26489=ORIENTED_EDGE('',*,*,#17955,.F.);
#26490=ORIENTED_EDGE('',*,*,#17951,.T.);
#26491=ORIENTED_EDGE('',*,*,#17956,.F.);
#26492=ORIENTED_EDGE('',*,*,#17957,.F.);
#26493=ORIENTED_EDGE('',*,*,#17958,.F.);
#26494=ORIENTED_EDGE('',*,*,#17954,.T.);
#26495=ORIENTED_EDGE('',*,*,#17959,.F.);
#26496=ORIENTED_EDGE('',*,*,#17960,.F.);
#26497=ORIENTED_EDGE('',*,*,#17961,.F.);
#26498=ORIENTED_EDGE('',*,*,#17957,.T.);
#26499=ORIENTED_EDGE('',*,*,#17962,.F.);
#26500=ORIENTED_EDGE('',*,*,#17963,.F.);
#26501=ORIENTED_EDGE('',*,*,#17964,.F.);
#26502=ORIENTED_EDGE('',*,*,#17960,.T.);
#26503=ORIENTED_EDGE('',*,*,#17965,.F.);
#26504=ORIENTED_EDGE('',*,*,#17966,.F.);
#26505=ORIENTED_EDGE('',*,*,#17967,.F.);
#26506=ORIENTED_EDGE('',*,*,#17963,.T.);
#26507=ORIENTED_EDGE('',*,*,#17968,.F.);
#26508=ORIENTED_EDGE('',*,*,#17969,.F.);
#26509=ORIENTED_EDGE('',*,*,#17970,.F.);
#26510=ORIENTED_EDGE('',*,*,#17966,.T.);
#26511=ORIENTED_EDGE('',*,*,#17971,.F.);
#26512=ORIENTED_EDGE('',*,*,#17972,.F.);
#26513=ORIENTED_EDGE('',*,*,#17973,.F.);
#26514=ORIENTED_EDGE('',*,*,#17969,.T.);
#26515=ORIENTED_EDGE('',*,*,#17974,.F.);
#26516=ORIENTED_EDGE('',*,*,#17975,.F.);
#26517=ORIENTED_EDGE('',*,*,#17976,.F.);
#26518=ORIENTED_EDGE('',*,*,#17972,.T.);
#26519=ORIENTED_EDGE('',*,*,#17977,.F.);
#26520=ORIENTED_EDGE('',*,*,#17978,.F.);
#26521=ORIENTED_EDGE('',*,*,#17979,.F.);
#26522=ORIENTED_EDGE('',*,*,#17975,.T.);
#26523=ORIENTED_EDGE('',*,*,#17980,.F.);
#26524=ORIENTED_EDGE('',*,*,#17981,.F.);
#26525=ORIENTED_EDGE('',*,*,#17982,.F.);
#26526=ORIENTED_EDGE('',*,*,#17978,.T.);
#26527=ORIENTED_EDGE('',*,*,#17983,.F.);
#26528=ORIENTED_EDGE('',*,*,#17984,.F.);
#26529=ORIENTED_EDGE('',*,*,#17985,.F.);
#26530=ORIENTED_EDGE('',*,*,#17981,.T.);
#26531=ORIENTED_EDGE('',*,*,#17986,.F.);
#26532=ORIENTED_EDGE('',*,*,#17987,.F.);
#26533=ORIENTED_EDGE('',*,*,#17988,.F.);
#26534=ORIENTED_EDGE('',*,*,#17984,.T.);
#26535=ORIENTED_EDGE('',*,*,#17989,.F.);
#26536=ORIENTED_EDGE('',*,*,#17990,.F.);
#26537=ORIENTED_EDGE('',*,*,#17991,.F.);
#26538=ORIENTED_EDGE('',*,*,#17987,.T.);
#26539=ORIENTED_EDGE('',*,*,#17992,.F.);
#26540=ORIENTED_EDGE('',*,*,#17993,.F.);
#26541=ORIENTED_EDGE('',*,*,#17994,.F.);
#26542=ORIENTED_EDGE('',*,*,#17990,.T.);
#26543=ORIENTED_EDGE('',*,*,#17995,.F.);
#26544=ORIENTED_EDGE('',*,*,#17996,.F.);
#26545=ORIENTED_EDGE('',*,*,#17997,.T.);
#26546=ORIENTED_EDGE('',*,*,#17998,.F.);
#26547=ORIENTED_EDGE('',*,*,#17999,.F.);
#26548=ORIENTED_EDGE('',*,*,#18000,.F.);
#26549=ORIENTED_EDGE('',*,*,#18001,.F.);
#26550=ORIENTED_EDGE('',*,*,#18002,.F.);
#26551=ORIENTED_EDGE('',*,*,#18003,.F.);
#26552=ORIENTED_EDGE('',*,*,#17999,.T.);
#26553=ORIENTED_EDGE('',*,*,#18004,.T.);
#26554=ORIENTED_EDGE('',*,*,#18005,.F.);
#26555=ORIENTED_EDGE('',*,*,#18006,.F.);
#26556=ORIENTED_EDGE('',*,*,#18002,.T.);
#26557=ORIENTED_EDGE('',*,*,#18007,.T.);
#26558=ORIENTED_EDGE('',*,*,#18008,.F.);
#26559=ORIENTED_EDGE('',*,*,#18009,.F.);
#26560=ORIENTED_EDGE('',*,*,#18005,.T.);
#26561=ORIENTED_EDGE('',*,*,#18010,.T.);
#26562=ORIENTED_EDGE('',*,*,#18011,.F.);
#26563=ORIENTED_EDGE('',*,*,#18012,.F.);
#26564=ORIENTED_EDGE('',*,*,#18008,.T.);
#26565=ORIENTED_EDGE('',*,*,#18013,.T.);
#26566=ORIENTED_EDGE('',*,*,#18014,.F.);
#26567=ORIENTED_EDGE('',*,*,#18015,.F.);
#26568=ORIENTED_EDGE('',*,*,#18011,.T.);
#26569=ORIENTED_EDGE('',*,*,#18016,.T.);
#26570=ORIENTED_EDGE('',*,*,#18017,.F.);
#26571=ORIENTED_EDGE('',*,*,#18018,.F.);
#26572=ORIENTED_EDGE('',*,*,#18014,.T.);
#26573=ORIENTED_EDGE('',*,*,#18019,.T.);
#26574=ORIENTED_EDGE('',*,*,#18020,.F.);
#26575=ORIENTED_EDGE('',*,*,#18021,.F.);
#26576=ORIENTED_EDGE('',*,*,#18017,.T.);
#26577=ORIENTED_EDGE('',*,*,#18022,.T.);
#26578=ORIENTED_EDGE('',*,*,#18023,.F.);
#26579=ORIENTED_EDGE('',*,*,#18024,.F.);
#26580=ORIENTED_EDGE('',*,*,#18020,.T.);
#26581=ORIENTED_EDGE('',*,*,#18025,.T.);
#26582=ORIENTED_EDGE('',*,*,#18026,.F.);
#26583=ORIENTED_EDGE('',*,*,#18027,.F.);
#26584=ORIENTED_EDGE('',*,*,#18023,.T.);
#26585=ORIENTED_EDGE('',*,*,#18028,.T.);
#26586=ORIENTED_EDGE('',*,*,#18029,.F.);
#26587=ORIENTED_EDGE('',*,*,#18030,.F.);
#26588=ORIENTED_EDGE('',*,*,#18026,.T.);
#26589=ORIENTED_EDGE('',*,*,#18031,.T.);
#26590=ORIENTED_EDGE('',*,*,#18032,.F.);
#26591=ORIENTED_EDGE('',*,*,#18033,.F.);
#26592=ORIENTED_EDGE('',*,*,#18029,.T.);
#26593=ORIENTED_EDGE('',*,*,#18034,.T.);
#26594=ORIENTED_EDGE('',*,*,#18035,.F.);
#26595=ORIENTED_EDGE('',*,*,#18036,.F.);
#26596=ORIENTED_EDGE('',*,*,#18032,.T.);
#26597=ORIENTED_EDGE('',*,*,#18037,.T.);
#26598=ORIENTED_EDGE('',*,*,#18038,.F.);
#26599=ORIENTED_EDGE('',*,*,#18039,.F.);
#26600=ORIENTED_EDGE('',*,*,#18035,.T.);
#26601=ORIENTED_EDGE('',*,*,#18040,.T.);
#26602=ORIENTED_EDGE('',*,*,#18041,.F.);
#26603=ORIENTED_EDGE('',*,*,#18042,.F.);
#26604=ORIENTED_EDGE('',*,*,#18038,.T.);
#26605=ORIENTED_EDGE('',*,*,#18043,.T.);
#26606=ORIENTED_EDGE('',*,*,#18044,.F.);
#26607=ORIENTED_EDGE('',*,*,#18045,.F.);
#26608=ORIENTED_EDGE('',*,*,#18041,.T.);
#26609=ORIENTED_EDGE('',*,*,#18046,.T.);
#26610=ORIENTED_EDGE('',*,*,#18047,.F.);
#26611=ORIENTED_EDGE('',*,*,#18048,.F.);
#26612=ORIENTED_EDGE('',*,*,#18044,.T.);
#26613=ORIENTED_EDGE('',*,*,#18049,.T.);
#26614=ORIENTED_EDGE('',*,*,#18050,.F.);
#26615=ORIENTED_EDGE('',*,*,#18051,.F.);
#26616=ORIENTED_EDGE('',*,*,#18047,.T.);
#26617=ORIENTED_EDGE('',*,*,#18052,.T.);
#26618=ORIENTED_EDGE('',*,*,#18053,.F.);
#26619=ORIENTED_EDGE('',*,*,#18054,.F.);
#26620=ORIENTED_EDGE('',*,*,#18050,.T.);
#26621=ORIENTED_EDGE('',*,*,#18055,.T.);
#26622=ORIENTED_EDGE('',*,*,#18056,.F.);
#26623=ORIENTED_EDGE('',*,*,#18057,.F.);
#26624=ORIENTED_EDGE('',*,*,#18053,.T.);
#26625=ORIENTED_EDGE('',*,*,#18058,.T.);
#26626=ORIENTED_EDGE('',*,*,#18059,.F.);
#26627=ORIENTED_EDGE('',*,*,#18060,.F.);
#26628=ORIENTED_EDGE('',*,*,#18056,.T.);
#26629=ORIENTED_EDGE('',*,*,#18061,.T.);
#26630=ORIENTED_EDGE('',*,*,#18062,.F.);
#26631=ORIENTED_EDGE('',*,*,#18063,.F.);
#26632=ORIENTED_EDGE('',*,*,#18059,.T.);
#26633=ORIENTED_EDGE('',*,*,#18064,.T.);
#26634=ORIENTED_EDGE('',*,*,#18065,.F.);
#26635=ORIENTED_EDGE('',*,*,#18066,.F.);
#26636=ORIENTED_EDGE('',*,*,#18062,.T.);
#26637=ORIENTED_EDGE('',*,*,#18067,.T.);
#26638=ORIENTED_EDGE('',*,*,#18068,.F.);
#26639=ORIENTED_EDGE('',*,*,#18069,.F.);
#26640=ORIENTED_EDGE('',*,*,#18065,.T.);
#26641=ORIENTED_EDGE('',*,*,#18070,.T.);
#26642=ORIENTED_EDGE('',*,*,#18071,.F.);
#26643=ORIENTED_EDGE('',*,*,#18072,.F.);
#26644=ORIENTED_EDGE('',*,*,#18068,.T.);
#26645=ORIENTED_EDGE('',*,*,#18073,.T.);
#26646=ORIENTED_EDGE('',*,*,#18074,.F.);
#26647=ORIENTED_EDGE('',*,*,#18075,.F.);
#26648=ORIENTED_EDGE('',*,*,#18071,.T.);
#26649=ORIENTED_EDGE('',*,*,#18076,.T.);
#26650=ORIENTED_EDGE('',*,*,#18077,.F.);
#26651=ORIENTED_EDGE('',*,*,#18078,.F.);
#26652=ORIENTED_EDGE('',*,*,#18074,.T.);
#26653=ORIENTED_EDGE('',*,*,#18079,.T.);
#26654=ORIENTED_EDGE('',*,*,#18080,.F.);
#26655=ORIENTED_EDGE('',*,*,#18081,.F.);
#26656=ORIENTED_EDGE('',*,*,#18077,.T.);
#26657=ORIENTED_EDGE('',*,*,#18082,.T.);
#26658=ORIENTED_EDGE('',*,*,#18083,.F.);
#26659=ORIENTED_EDGE('',*,*,#18084,.F.);
#26660=ORIENTED_EDGE('',*,*,#18080,.T.);
#26661=ORIENTED_EDGE('',*,*,#18085,.T.);
#26662=ORIENTED_EDGE('',*,*,#18086,.F.);
#26663=ORIENTED_EDGE('',*,*,#18087,.F.);
#26664=ORIENTED_EDGE('',*,*,#18083,.T.);
#26665=ORIENTED_EDGE('',*,*,#18088,.T.);
#26666=ORIENTED_EDGE('',*,*,#18086,.T.);
#26667=ORIENTED_EDGE('',*,*,#18089,.T.);
#26668=ORIENTED_EDGE('',*,*,#18090,.F.);
#26669=ORIENTED_EDGE('',*,*,#17996,.T.);
#26670=ORIENTED_EDGE('',*,*,#18091,.F.);
#26671=ORIENTED_EDGE('',*,*,#18092,.T.);
#26672=ORIENTED_EDGE('',*,*,#18093,.T.);
#26673=ORIENTED_EDGE('',*,*,#18094,.T.);
#26674=ORIENTED_EDGE('',*,*,#17993,.T.);
#26675=ORIENTED_EDGE('',*,*,#18095,.F.);
#26676=ORIENTED_EDGE('',*,*,#18093,.F.);
#26677=ORIENTED_EDGE('',*,*,#18096,.F.);
#26678=ORIENTED_EDGE('',*,*,#18097,.T.);
#26679=ORIENTED_EDGE('',*,*,#18098,.T.);
#26680=ORIENTED_EDGE('',*,*,#18099,.T.);
#26681=ORIENTED_EDGE('',*,*,#18100,.F.);
#26682=ORIENTED_EDGE('',*,*,#18101,.T.);
#26683=ORIENTED_EDGE('',*,*,#18102,.T.);
#26684=ORIENTED_EDGE('',*,*,#18103,.T.);
#26685=ORIENTED_EDGE('',*,*,#18104,.F.);
#26686=ORIENTED_EDGE('',*,*,#18105,.T.);
#26687=ORIENTED_EDGE('',*,*,#18106,.T.);
#26688=ORIENTED_EDGE('',*,*,#18107,.T.);
#26689=ORIENTED_EDGE('',*,*,#18108,.F.);
#26690=ORIENTED_EDGE('',*,*,#18109,.T.);
#26691=ORIENTED_EDGE('',*,*,#18110,.T.);
#26692=ORIENTED_EDGE('',*,*,#18111,.T.);
#26693=ORIENTED_EDGE('',*,*,#18112,.F.);
#26694=ORIENTED_EDGE('',*,*,#18113,.T.);
#26695=ORIENTED_EDGE('',*,*,#18114,.T.);
#26696=ORIENTED_EDGE('',*,*,#18115,.T.);
#26697=ORIENTED_EDGE('',*,*,#18116,.F.);
#26698=ORIENTED_EDGE('',*,*,#18117,.T.);
#26699=ORIENTED_EDGE('',*,*,#18118,.T.);
#26700=ORIENTED_EDGE('',*,*,#18119,.T.);
#26701=ORIENTED_EDGE('',*,*,#18120,.F.);
#26702=ORIENTED_EDGE('',*,*,#18121,.T.);
#26703=ORIENTED_EDGE('',*,*,#18122,.T.);
#26704=ORIENTED_EDGE('',*,*,#18123,.T.);
#26705=ORIENTED_EDGE('',*,*,#18124,.F.);
#26706=ORIENTED_EDGE('',*,*,#18125,.T.);
#26707=ORIENTED_EDGE('',*,*,#18126,.T.);
#26708=ORIENTED_EDGE('',*,*,#18127,.T.);
#26709=ORIENTED_EDGE('',*,*,#18128,.F.);
#26710=ORIENTED_EDGE('',*,*,#18129,.T.);
#26711=ORIENTED_EDGE('',*,*,#18130,.T.);
#26712=ORIENTED_EDGE('',*,*,#18131,.T.);
#26713=ORIENTED_EDGE('',*,*,#18132,.F.);
#26714=ORIENTED_EDGE('',*,*,#18133,.T.);
#26715=ORIENTED_EDGE('',*,*,#18134,.T.);
#26716=ORIENTED_EDGE('',*,*,#18135,.T.);
#26717=ORIENTED_EDGE('',*,*,#18136,.F.);
#26718=ORIENTED_EDGE('',*,*,#18137,.T.);
#26719=ORIENTED_EDGE('',*,*,#18138,.T.);
#26720=ORIENTED_EDGE('',*,*,#18139,.T.);
#26721=ORIENTED_EDGE('',*,*,#18140,.F.);
#26722=ORIENTED_EDGE('',*,*,#18141,.T.);
#26723=ORIENTED_EDGE('',*,*,#18142,.T.);
#26724=ORIENTED_EDGE('',*,*,#18143,.T.);
#26725=ORIENTED_EDGE('',*,*,#18144,.F.);
#26726=ORIENTED_EDGE('',*,*,#18145,.T.);
#26727=ORIENTED_EDGE('',*,*,#18146,.T.);
#26728=ORIENTED_EDGE('',*,*,#18147,.T.);
#26729=ORIENTED_EDGE('',*,*,#18148,.F.);
#26730=ORIENTED_EDGE('',*,*,#18149,.T.);
#26731=ORIENTED_EDGE('',*,*,#18150,.T.);
#26732=ORIENTED_EDGE('',*,*,#18151,.T.);
#26733=ORIENTED_EDGE('',*,*,#18152,.F.);
#26734=ORIENTED_EDGE('',*,*,#18153,.T.);
#26735=ORIENTED_EDGE('',*,*,#18154,.T.);
#26736=ORIENTED_EDGE('',*,*,#18155,.T.);
#26737=ORIENTED_EDGE('',*,*,#18156,.F.);
#26738=ORIENTED_EDGE('',*,*,#18157,.F.);
#26739=ORIENTED_EDGE('',*,*,#18158,.F.);
#26740=ORIENTED_EDGE('',*,*,#18159,.F.);
#26741=ORIENTED_EDGE('',*,*,#18160,.F.);
#26742=ORIENTED_EDGE('',*,*,#18161,.F.);
#26743=ORIENTED_EDGE('',*,*,#18162,.F.);
#26744=ORIENTED_EDGE('',*,*,#18163,.F.);
#26745=ORIENTED_EDGE('',*,*,#18164,.T.);
#26746=ORIENTED_EDGE('',*,*,#18165,.T.);
#26747=ORIENTED_EDGE('',*,*,#18164,.F.);
#26748=ORIENTED_EDGE('',*,*,#18166,.F.);
#26749=ORIENTED_EDGE('',*,*,#18167,.T.);
#26750=ORIENTED_EDGE('',*,*,#18168,.T.);
#26751=ORIENTED_EDGE('',*,*,#18167,.F.);
#26752=ORIENTED_EDGE('',*,*,#18169,.F.);
#26753=ORIENTED_EDGE('',*,*,#18170,.F.);
#26754=ORIENTED_EDGE('',*,*,#18171,.F.);
#26755=ORIENTED_EDGE('',*,*,#18172,.F.);
#26756=ORIENTED_EDGE('',*,*,#18173,.F.);
#26757=ORIENTED_EDGE('',*,*,#18174,.F.);
#26758=ORIENTED_EDGE('',*,*,#18175,.F.);
#26759=ORIENTED_EDGE('',*,*,#18176,.F.);
#26760=ORIENTED_EDGE('',*,*,#18177,.F.);
#26761=ORIENTED_EDGE('',*,*,#18178,.F.);
#26762=ORIENTED_EDGE('',*,*,#18179,.F.);
#26763=ORIENTED_EDGE('',*,*,#18180,.F.);
#26764=ORIENTED_EDGE('',*,*,#18181,.F.);
#26765=ORIENTED_EDGE('',*,*,#18182,.F.);
#26766=ORIENTED_EDGE('',*,*,#18183,.F.);
#26767=ORIENTED_EDGE('',*,*,#18184,.F.);
#26768=ORIENTED_EDGE('',*,*,#18185,.F.);
#26769=ORIENTED_EDGE('',*,*,#18186,.F.);
#26770=ORIENTED_EDGE('',*,*,#18187,.F.);
#26771=ORIENTED_EDGE('',*,*,#18188,.F.);
#26772=ORIENTED_EDGE('',*,*,#18189,.F.);
#26773=ORIENTED_EDGE('',*,*,#18190,.F.);
#26774=ORIENTED_EDGE('',*,*,#18191,.F.);
#26775=ORIENTED_EDGE('',*,*,#18192,.F.);
#26776=ORIENTED_EDGE('',*,*,#18193,.F.);
#26777=ORIENTED_EDGE('',*,*,#18194,.F.);
#26778=ORIENTED_EDGE('',*,*,#18195,.F.);
#26779=ORIENTED_EDGE('',*,*,#18196,.F.);
#26780=ORIENTED_EDGE('',*,*,#18197,.F.);
#26781=ORIENTED_EDGE('',*,*,#18198,.F.);
#26782=ORIENTED_EDGE('',*,*,#18199,.F.);
#26783=ORIENTED_EDGE('',*,*,#18200,.F.);
#26784=ORIENTED_EDGE('',*,*,#18201,.F.);
#26785=ORIENTED_EDGE('',*,*,#18202,.F.);
#26786=ORIENTED_EDGE('',*,*,#18203,.F.);
#26787=ORIENTED_EDGE('',*,*,#18204,.F.);
#26788=ORIENTED_EDGE('',*,*,#18205,.F.);
#26789=ORIENTED_EDGE('',*,*,#18206,.F.);
#26790=ORIENTED_EDGE('',*,*,#18207,.F.);
#26791=ORIENTED_EDGE('',*,*,#18208,.F.);
#26792=ORIENTED_EDGE('',*,*,#18209,.F.);
#26793=ORIENTED_EDGE('',*,*,#18210,.F.);
#26794=ORIENTED_EDGE('',*,*,#18211,.F.);
#26795=ORIENTED_EDGE('',*,*,#18212,.F.);
#26796=ORIENTED_EDGE('',*,*,#18213,.F.);
#26797=ORIENTED_EDGE('',*,*,#18214,.F.);
#26798=ORIENTED_EDGE('',*,*,#18215,.F.);
#26799=ORIENTED_EDGE('',*,*,#18216,.F.);
#26800=ORIENTED_EDGE('',*,*,#18217,.F.);
#26801=ORIENTED_EDGE('',*,*,#18218,.F.);
#26802=ORIENTED_EDGE('',*,*,#18219,.F.);
#26803=ORIENTED_EDGE('',*,*,#18220,.F.);
#26804=ORIENTED_EDGE('',*,*,#18221,.F.);
#26805=ORIENTED_EDGE('',*,*,#18222,.F.);
#26806=ORIENTED_EDGE('',*,*,#18223,.F.);
#26807=ORIENTED_EDGE('',*,*,#18224,.F.);
#26808=ORIENTED_EDGE('',*,*,#18225,.F.);
#26809=ORIENTED_EDGE('',*,*,#18226,.F.);
#26810=ORIENTED_EDGE('',*,*,#18227,.F.);
#26811=ORIENTED_EDGE('',*,*,#18228,.F.);
#26812=ORIENTED_EDGE('',*,*,#18229,.F.);
#26813=ORIENTED_EDGE('',*,*,#18230,.F.);
#26814=ORIENTED_EDGE('',*,*,#18231,.F.);
#26815=ORIENTED_EDGE('',*,*,#18232,.F.);
#26816=ORIENTED_EDGE('',*,*,#18233,.F.);
#26817=ORIENTED_EDGE('',*,*,#18234,.F.);
#26818=ORIENTED_EDGE('',*,*,#18235,.F.);
#26819=ORIENTED_EDGE('',*,*,#18236,.F.);
#26820=ORIENTED_EDGE('',*,*,#18237,.F.);
#26821=ORIENTED_EDGE('',*,*,#18238,.F.);
#26822=ORIENTED_EDGE('',*,*,#18239,.F.);
#26823=ORIENTED_EDGE('',*,*,#18240,.F.);
#26824=ORIENTED_EDGE('',*,*,#18241,.F.);
#26825=ORIENTED_EDGE('',*,*,#18242,.F.);
#26826=ORIENTED_EDGE('',*,*,#18243,.F.);
#26827=ORIENTED_EDGE('',*,*,#18244,.F.);
#26828=ORIENTED_EDGE('',*,*,#18245,.F.);
#26829=ORIENTED_EDGE('',*,*,#18246,.F.);
#26830=ORIENTED_EDGE('',*,*,#18247,.F.);
#26831=ORIENTED_EDGE('',*,*,#18248,.F.);
#26832=ORIENTED_EDGE('',*,*,#18249,.F.);
#26833=ORIENTED_EDGE('',*,*,#18250,.F.);
#26834=ORIENTED_EDGE('',*,*,#18251,.F.);
#26835=ORIENTED_EDGE('',*,*,#18252,.F.);
#26836=ORIENTED_EDGE('',*,*,#18253,.F.);
#26837=ORIENTED_EDGE('',*,*,#18254,.F.);
#26838=ORIENTED_EDGE('',*,*,#18255,.F.);
#26839=ORIENTED_EDGE('',*,*,#18256,.F.);
#26840=ORIENTED_EDGE('',*,*,#18257,.F.);
#26841=ORIENTED_EDGE('',*,*,#18258,.F.);
#26842=ORIENTED_EDGE('',*,*,#18259,.F.);
#26843=ORIENTED_EDGE('',*,*,#18260,.F.);
#26844=ORIENTED_EDGE('',*,*,#18261,.F.);
#26845=ORIENTED_EDGE('',*,*,#18262,.F.);
#26846=ORIENTED_EDGE('',*,*,#18263,.F.);
#26847=ORIENTED_EDGE('',*,*,#18264,.F.);
#26848=ORIENTED_EDGE('',*,*,#18265,.F.);
#26849=ORIENTED_EDGE('',*,*,#18266,.F.);
#26850=ORIENTED_EDGE('',*,*,#18267,.F.);
#26851=ORIENTED_EDGE('',*,*,#18268,.F.);
#26852=ORIENTED_EDGE('',*,*,#18269,.F.);
#26853=ORIENTED_EDGE('',*,*,#18270,.F.);
#26854=ORIENTED_EDGE('',*,*,#18271,.F.);
#26855=ORIENTED_EDGE('',*,*,#18272,.F.);
#26856=ORIENTED_EDGE('',*,*,#18273,.F.);
#26857=ORIENTED_EDGE('',*,*,#18274,.F.);
#26858=ORIENTED_EDGE('',*,*,#18275,.F.);
#26859=ORIENTED_EDGE('',*,*,#18276,.F.);
#26860=ORIENTED_EDGE('',*,*,#18277,.F.);
#26861=ORIENTED_EDGE('',*,*,#18278,.F.);
#26862=ORIENTED_EDGE('',*,*,#18279,.F.);
#26863=ORIENTED_EDGE('',*,*,#18280,.F.);
#26864=ORIENTED_EDGE('',*,*,#18281,.F.);
#26865=ORIENTED_EDGE('',*,*,#18282,.F.);
#26866=ORIENTED_EDGE('',*,*,#18283,.F.);
#26867=ORIENTED_EDGE('',*,*,#18284,.F.);
#26868=ORIENTED_EDGE('',*,*,#18285,.F.);
#26869=ORIENTED_EDGE('',*,*,#18286,.F.);
#26870=ORIENTED_EDGE('',*,*,#18287,.F.);
#26871=ORIENTED_EDGE('',*,*,#18288,.F.);
#26872=ORIENTED_EDGE('',*,*,#18289,.F.);
#26873=ORIENTED_EDGE('',*,*,#18290,.F.);
#26874=ORIENTED_EDGE('',*,*,#18291,.F.);
#26875=ORIENTED_EDGE('',*,*,#18292,.F.);
#26876=ORIENTED_EDGE('',*,*,#18293,.F.);
#26877=ORIENTED_EDGE('',*,*,#18294,.F.);
#26878=ORIENTED_EDGE('',*,*,#18295,.F.);
#26879=ORIENTED_EDGE('',*,*,#18296,.F.);
#26880=ORIENTED_EDGE('',*,*,#18297,.F.);
#26881=ORIENTED_EDGE('',*,*,#18298,.F.);
#26882=ORIENTED_EDGE('',*,*,#18299,.F.);
#26883=ORIENTED_EDGE('',*,*,#18300,.F.);
#26884=ORIENTED_EDGE('',*,*,#18301,.F.);
#26885=ORIENTED_EDGE('',*,*,#18302,.F.);
#26886=ORIENTED_EDGE('',*,*,#18303,.F.);
#26887=ORIENTED_EDGE('',*,*,#18304,.F.);
#26888=ORIENTED_EDGE('',*,*,#18305,.F.);
#26889=ORIENTED_EDGE('',*,*,#18306,.F.);
#26890=ORIENTED_EDGE('',*,*,#18307,.F.);
#26891=ORIENTED_EDGE('',*,*,#18308,.F.);
#26892=ORIENTED_EDGE('',*,*,#18309,.F.);
#26893=ORIENTED_EDGE('',*,*,#18310,.F.);
#26894=ORIENTED_EDGE('',*,*,#18311,.F.);
#26895=ORIENTED_EDGE('',*,*,#18312,.F.);
#26896=ORIENTED_EDGE('',*,*,#18313,.F.);
#26897=ORIENTED_EDGE('',*,*,#18314,.F.);
#26898=ORIENTED_EDGE('',*,*,#18315,.F.);
#26899=ORIENTED_EDGE('',*,*,#18316,.F.);
#26900=ORIENTED_EDGE('',*,*,#18317,.F.);
#26901=ORIENTED_EDGE('',*,*,#18318,.F.);
#26902=ORIENTED_EDGE('',*,*,#18319,.F.);
#26903=ORIENTED_EDGE('',*,*,#18320,.F.);
#26904=ORIENTED_EDGE('',*,*,#18321,.F.);
#26905=ORIENTED_EDGE('',*,*,#18322,.F.);
#26906=ORIENTED_EDGE('',*,*,#18323,.F.);
#26907=ORIENTED_EDGE('',*,*,#18324,.F.);
#26908=ORIENTED_EDGE('',*,*,#18325,.F.);
#26909=ORIENTED_EDGE('',*,*,#18326,.F.);
#26910=ORIENTED_EDGE('',*,*,#18327,.F.);
#26911=ORIENTED_EDGE('',*,*,#18328,.F.);
#26912=ORIENTED_EDGE('',*,*,#18329,.F.);
#26913=ORIENTED_EDGE('',*,*,#18330,.F.);
#26914=ORIENTED_EDGE('',*,*,#18331,.F.);
#26915=ORIENTED_EDGE('',*,*,#18332,.F.);
#26916=ORIENTED_EDGE('',*,*,#18333,.F.);
#26917=ORIENTED_EDGE('',*,*,#18334,.F.);
#26918=ORIENTED_EDGE('',*,*,#18335,.F.);
#26919=ORIENTED_EDGE('',*,*,#18336,.F.);
#26920=ORIENTED_EDGE('',*,*,#18337,.F.);
#26921=ORIENTED_EDGE('',*,*,#18338,.F.);
#26922=ORIENTED_EDGE('',*,*,#18339,.F.);
#26923=ORIENTED_EDGE('',*,*,#18340,.F.);
#26924=ORIENTED_EDGE('',*,*,#18341,.F.);
#26925=ORIENTED_EDGE('',*,*,#18342,.F.);
#26926=ORIENTED_EDGE('',*,*,#18343,.F.);
#26927=ORIENTED_EDGE('',*,*,#18344,.F.);
#26928=ORIENTED_EDGE('',*,*,#18345,.F.);
#26929=ORIENTED_EDGE('',*,*,#18346,.F.);
#26930=ORIENTED_EDGE('',*,*,#18347,.F.);
#26931=ORIENTED_EDGE('',*,*,#18348,.F.);
#26932=ORIENTED_EDGE('',*,*,#18349,.F.);
#26933=ORIENTED_EDGE('',*,*,#18350,.F.);
#26934=ORIENTED_EDGE('',*,*,#18351,.F.);
#26935=ORIENTED_EDGE('',*,*,#18352,.F.);
#26936=ORIENTED_EDGE('',*,*,#18155,.F.);
#26937=ORIENTED_EDGE('',*,*,#18353,.F.);
#26938=ORIENTED_EDGE('',*,*,#18354,.F.);
#26939=ORIENTED_EDGE('',*,*,#18355,.F.);
#26940=ORIENTED_EDGE('',*,*,#18151,.F.);
#26941=ORIENTED_EDGE('',*,*,#18356,.F.);
#26942=ORIENTED_EDGE('',*,*,#18357,.F.);
#26943=ORIENTED_EDGE('',*,*,#18358,.F.);
#26944=ORIENTED_EDGE('',*,*,#18147,.F.);
#26945=ORIENTED_EDGE('',*,*,#18359,.F.);
#26946=ORIENTED_EDGE('',*,*,#18360,.F.);
#26947=ORIENTED_EDGE('',*,*,#18361,.F.);
#26948=ORIENTED_EDGE('',*,*,#18143,.F.);
#26949=ORIENTED_EDGE('',*,*,#18362,.F.);
#26950=ORIENTED_EDGE('',*,*,#18363,.F.);
#26951=ORIENTED_EDGE('',*,*,#18364,.F.);
#26952=ORIENTED_EDGE('',*,*,#18139,.F.);
#26953=ORIENTED_EDGE('',*,*,#18365,.F.);
#26954=ORIENTED_EDGE('',*,*,#18366,.F.);
#26955=ORIENTED_EDGE('',*,*,#18367,.F.);
#26956=ORIENTED_EDGE('',*,*,#18135,.F.);
#26957=ORIENTED_EDGE('',*,*,#18368,.F.);
#26958=ORIENTED_EDGE('',*,*,#18369,.F.);
#26959=ORIENTED_EDGE('',*,*,#18370,.F.);
#26960=ORIENTED_EDGE('',*,*,#18131,.F.);
#26961=ORIENTED_EDGE('',*,*,#18371,.F.);
#26962=ORIENTED_EDGE('',*,*,#18372,.F.);
#26963=ORIENTED_EDGE('',*,*,#18373,.F.);
#26964=ORIENTED_EDGE('',*,*,#18127,.F.);
#26965=ORIENTED_EDGE('',*,*,#18374,.F.);
#26966=ORIENTED_EDGE('',*,*,#18375,.F.);
#26967=ORIENTED_EDGE('',*,*,#18376,.F.);
#26968=ORIENTED_EDGE('',*,*,#18123,.F.);
#26969=ORIENTED_EDGE('',*,*,#18377,.F.);
#26970=ORIENTED_EDGE('',*,*,#18378,.F.);
#26971=ORIENTED_EDGE('',*,*,#18379,.F.);
#26972=ORIENTED_EDGE('',*,*,#18099,.F.);
#26973=ORIENTED_EDGE('',*,*,#18380,.F.);
#26974=ORIENTED_EDGE('',*,*,#18381,.F.);
#26975=ORIENTED_EDGE('',*,*,#18382,.F.);
#26976=ORIENTED_EDGE('',*,*,#18103,.F.);
#26977=ORIENTED_EDGE('',*,*,#18383,.F.);
#26978=ORIENTED_EDGE('',*,*,#18384,.F.);
#26979=ORIENTED_EDGE('',*,*,#18385,.F.);
#26980=ORIENTED_EDGE('',*,*,#18107,.F.);
#26981=ORIENTED_EDGE('',*,*,#18386,.F.);
#26982=ORIENTED_EDGE('',*,*,#18387,.F.);
#26983=ORIENTED_EDGE('',*,*,#18388,.F.);
#26984=ORIENTED_EDGE('',*,*,#18111,.F.);
#26985=ORIENTED_EDGE('',*,*,#18389,.F.);
#26986=ORIENTED_EDGE('',*,*,#18390,.F.);
#26987=ORIENTED_EDGE('',*,*,#18391,.F.);
#26988=ORIENTED_EDGE('',*,*,#18115,.F.);
#26989=ORIENTED_EDGE('',*,*,#18392,.F.);
#26990=ORIENTED_EDGE('',*,*,#18393,.F.);
#26991=ORIENTED_EDGE('',*,*,#18394,.F.);
#26992=ORIENTED_EDGE('',*,*,#18119,.F.);
#26993=ORIENTED_EDGE('',*,*,#18395,.F.);
#26994=ORIENTED_EDGE('',*,*,#18396,.F.);
#26995=ORIENTED_EDGE('',*,*,#18397,.F.);
#26996=ORIENTED_EDGE('',*,*,#18398,.F.);
#26997=ORIENTED_EDGE('',*,*,#18399,.F.);
#26998=ORIENTED_EDGE('',*,*,#18400,.F.);
#26999=ORIENTED_EDGE('',*,*,#18401,.F.);
#27000=ORIENTED_EDGE('',*,*,#18402,.F.);
#27001=ORIENTED_EDGE('',*,*,#18403,.F.);
#27002=ORIENTED_EDGE('',*,*,#18404,.F.);
#27003=ORIENTED_EDGE('',*,*,#18405,.F.);
#27004=ORIENTED_EDGE('',*,*,#18406,.F.);
#27005=ORIENTED_EDGE('',*,*,#18407,.F.);
#27006=ORIENTED_EDGE('',*,*,#18408,.F.);
#27007=ORIENTED_EDGE('',*,*,#18409,.F.);
#27008=ORIENTED_EDGE('',*,*,#18410,.F.);
#27009=ORIENTED_EDGE('',*,*,#18411,.F.);
#27010=ORIENTED_EDGE('',*,*,#18412,.F.);
#27011=ORIENTED_EDGE('',*,*,#18413,.F.);
#27012=ORIENTED_EDGE('',*,*,#18414,.F.);
#27013=ORIENTED_EDGE('',*,*,#18415,.F.);
#27014=ORIENTED_EDGE('',*,*,#18416,.F.);
#27015=ORIENTED_EDGE('',*,*,#18417,.F.);
#27016=ORIENTED_EDGE('',*,*,#18418,.F.);
#27017=ORIENTED_EDGE('',*,*,#18419,.F.);
#27018=ORIENTED_EDGE('',*,*,#18420,.F.);
#27019=ORIENTED_EDGE('',*,*,#18421,.F.);
#27020=ORIENTED_EDGE('',*,*,#18422,.F.);
#27021=ORIENTED_EDGE('',*,*,#18423,.F.);
#27022=ORIENTED_EDGE('',*,*,#18424,.F.);
#27023=ORIENTED_EDGE('',*,*,#18425,.F.);
#27024=ORIENTED_EDGE('',*,*,#18426,.F.);
#27025=ORIENTED_EDGE('',*,*,#18427,.F.);
#27026=ORIENTED_EDGE('',*,*,#18428,.F.);
#27027=ORIENTED_EDGE('',*,*,#18429,.F.);
#27028=ORIENTED_EDGE('',*,*,#18430,.F.);
#27029=ORIENTED_EDGE('',*,*,#18431,.F.);
#27030=ORIENTED_EDGE('',*,*,#18432,.F.);
#27031=ORIENTED_EDGE('',*,*,#18433,.F.);
#27032=ORIENTED_EDGE('',*,*,#18434,.F.);
#27033=ORIENTED_EDGE('',*,*,#18435,.F.);
#27034=ORIENTED_EDGE('',*,*,#18436,.F.);
#27035=ORIENTED_EDGE('',*,*,#18437,.F.);
#27036=ORIENTED_EDGE('',*,*,#18438,.F.);
#27037=ORIENTED_EDGE('',*,*,#18439,.F.);
#27038=ORIENTED_EDGE('',*,*,#18440,.F.);
#27039=ORIENTED_EDGE('',*,*,#18441,.F.);
#27040=ORIENTED_EDGE('',*,*,#18442,.F.);
#27041=ORIENTED_EDGE('',*,*,#18443,.F.);
#27042=ORIENTED_EDGE('',*,*,#18444,.F.);
#27043=ORIENTED_EDGE('',*,*,#18445,.F.);
#27044=ORIENTED_EDGE('',*,*,#18446,.F.);
#27045=ORIENTED_EDGE('',*,*,#18447,.F.);
#27046=ORIENTED_EDGE('',*,*,#18448,.F.);
#27047=ORIENTED_EDGE('',*,*,#18449,.F.);
#27048=ORIENTED_EDGE('',*,*,#18450,.F.);
#27049=ORIENTED_EDGE('',*,*,#18451,.F.);
#27050=ORIENTED_EDGE('',*,*,#18452,.F.);
#27051=ORIENTED_EDGE('',*,*,#18453,.F.);
#27052=ORIENTED_EDGE('',*,*,#18454,.F.);
#27053=ORIENTED_EDGE('',*,*,#18455,.F.);
#27054=ORIENTED_EDGE('',*,*,#18456,.F.);
#27055=ORIENTED_EDGE('',*,*,#18457,.F.);
#27056=ORIENTED_EDGE('',*,*,#18458,.F.);
#27057=ORIENTED_EDGE('',*,*,#18459,.F.);
#27058=ORIENTED_EDGE('',*,*,#18460,.F.);
#27059=ORIENTED_EDGE('',*,*,#18461,.F.);
#27060=ORIENTED_EDGE('',*,*,#18462,.F.);
#27061=ORIENTED_EDGE('',*,*,#18463,.F.);
#27062=ORIENTED_EDGE('',*,*,#18464,.F.);
#27063=ORIENTED_EDGE('',*,*,#18465,.F.);
#27064=ORIENTED_EDGE('',*,*,#18466,.F.);
#27065=ORIENTED_EDGE('',*,*,#18467,.F.);
#27066=ORIENTED_EDGE('',*,*,#18468,.F.);
#27067=ORIENTED_EDGE('',*,*,#18469,.F.);
#27068=ORIENTED_EDGE('',*,*,#18470,.F.);
#27069=ORIENTED_EDGE('',*,*,#18471,.F.);
#27070=ORIENTED_EDGE('',*,*,#18472,.F.);
#27071=ORIENTED_EDGE('',*,*,#18473,.F.);
#27072=ORIENTED_EDGE('',*,*,#18474,.F.);
#27073=ORIENTED_EDGE('',*,*,#18475,.T.);
#27074=ORIENTED_EDGE('',*,*,#18166,.T.);
#27075=ORIENTED_EDGE('',*,*,#18475,.F.);
#27076=ORIENTED_EDGE('',*,*,#18476,.F.);
#27077=ORIENTED_EDGE('',*,*,#18477,.F.);
#27078=ORIENTED_EDGE('',*,*,#18478,.T.);
#27079=ORIENTED_EDGE('',*,*,#18479,.F.);
#27080=ORIENTED_EDGE('',*,*,#18480,.F.);
#27081=ORIENTED_EDGE('',*,*,#18481,.F.);
#27082=ORIENTED_EDGE('',*,*,#18482,.T.);
#27083=ORIENTED_EDGE('',*,*,#18483,.F.);
#27084=ORIENTED_EDGE('',*,*,#18484,.F.);
#27085=ORIENTED_EDGE('',*,*,#18485,.F.);
#27086=ORIENTED_EDGE('',*,*,#18486,.T.);
#27087=ORIENTED_EDGE('',*,*,#18487,.F.);
#27088=ORIENTED_EDGE('',*,*,#18488,.F.);
#27089=ORIENTED_EDGE('',*,*,#18489,.F.);
#27090=ORIENTED_EDGE('',*,*,#18490,.T.);
#27091=ORIENTED_EDGE('',*,*,#18491,.F.);
#27092=ORIENTED_EDGE('',*,*,#18492,.F.);
#27093=ORIENTED_EDGE('',*,*,#18493,.F.);
#27094=ORIENTED_EDGE('',*,*,#18494,.T.);
#27095=ORIENTED_EDGE('',*,*,#18495,.F.);
#27096=ORIENTED_EDGE('',*,*,#18496,.F.);
#27097=ORIENTED_EDGE('',*,*,#18497,.F.);
#27098=ORIENTED_EDGE('',*,*,#18498,.T.);
#27099=ORIENTED_EDGE('',*,*,#18499,.F.);
#27100=ORIENTED_EDGE('',*,*,#18500,.F.);
#27101=ORIENTED_EDGE('',*,*,#18501,.F.);
#27102=ORIENTED_EDGE('',*,*,#18502,.T.);
#27103=ORIENTED_EDGE('',*,*,#18503,.F.);
#27104=ORIENTED_EDGE('',*,*,#18504,.F.);
#27105=ORIENTED_EDGE('',*,*,#18505,.F.);
#27106=ORIENTED_EDGE('',*,*,#18506,.T.);
#27107=ORIENTED_EDGE('',*,*,#18507,.F.);
#27108=ORIENTED_EDGE('',*,*,#18508,.F.);
#27109=ORIENTED_EDGE('',*,*,#18509,.F.);
#27110=ORIENTED_EDGE('',*,*,#18510,.T.);
#27111=ORIENTED_EDGE('',*,*,#18511,.F.);
#27112=ORIENTED_EDGE('',*,*,#18512,.F.);
#27113=ORIENTED_EDGE('',*,*,#18513,.F.);
#27114=ORIENTED_EDGE('',*,*,#18514,.T.);
#27115=ORIENTED_EDGE('',*,*,#18515,.F.);
#27116=ORIENTED_EDGE('',*,*,#18516,.F.);
#27117=ORIENTED_EDGE('',*,*,#18517,.F.);
#27118=ORIENTED_EDGE('',*,*,#18518,.T.);
#27119=ORIENTED_EDGE('',*,*,#18519,.F.);
#27120=ORIENTED_EDGE('',*,*,#18520,.F.);
#27121=ORIENTED_EDGE('',*,*,#18521,.F.);
#27122=ORIENTED_EDGE('',*,*,#18522,.T.);
#27123=ORIENTED_EDGE('',*,*,#18523,.F.);
#27124=ORIENTED_EDGE('',*,*,#18524,.F.);
#27125=ORIENTED_EDGE('',*,*,#18525,.F.);
#27126=ORIENTED_EDGE('',*,*,#18526,.T.);
#27127=ORIENTED_EDGE('',*,*,#18527,.F.);
#27128=ORIENTED_EDGE('',*,*,#18528,.F.);
#27129=ORIENTED_EDGE('',*,*,#18529,.F.);
#27130=ORIENTED_EDGE('',*,*,#18530,.T.);
#27131=ORIENTED_EDGE('',*,*,#18531,.F.);
#27132=ORIENTED_EDGE('',*,*,#18532,.F.);
#27133=ORIENTED_EDGE('',*,*,#18533,.F.);
#27134=ORIENTED_EDGE('',*,*,#18534,.T.);
#27135=ORIENTED_EDGE('',*,*,#18535,.F.);
#27136=ORIENTED_EDGE('',*,*,#18536,.F.);
#27137=ORIENTED_EDGE('',*,*,#18537,.F.);
#27138=ORIENTED_EDGE('',*,*,#18538,.T.);
#27139=ORIENTED_EDGE('',*,*,#18539,.F.);
#27140=ORIENTED_EDGE('',*,*,#18540,.F.);
#27141=ORIENTED_EDGE('',*,*,#18541,.F.);
#27142=ORIENTED_EDGE('',*,*,#18542,.T.);
#27143=ORIENTED_EDGE('',*,*,#18543,.F.);
#27144=ORIENTED_EDGE('',*,*,#18544,.F.);
#27145=ORIENTED_EDGE('',*,*,#18545,.F.);
#27146=ORIENTED_EDGE('',*,*,#18546,.T.);
#27147=ORIENTED_EDGE('',*,*,#18547,.F.);
#27148=ORIENTED_EDGE('',*,*,#18548,.F.);
#27149=ORIENTED_EDGE('',*,*,#18549,.F.);
#27150=ORIENTED_EDGE('',*,*,#18550,.T.);
#27151=ORIENTED_EDGE('',*,*,#18551,.F.);
#27152=ORIENTED_EDGE('',*,*,#18552,.F.);
#27153=ORIENTED_EDGE('',*,*,#18553,.F.);
#27154=ORIENTED_EDGE('',*,*,#18554,.T.);
#27155=ORIENTED_EDGE('',*,*,#18555,.F.);
#27156=ORIENTED_EDGE('',*,*,#18556,.F.);
#27157=ORIENTED_EDGE('',*,*,#18557,.F.);
#27158=ORIENTED_EDGE('',*,*,#18558,.T.);
#27159=ORIENTED_EDGE('',*,*,#18559,.F.);
#27160=ORIENTED_EDGE('',*,*,#18560,.F.);
#27161=ORIENTED_EDGE('',*,*,#18561,.F.);
#27162=ORIENTED_EDGE('',*,*,#18562,.T.);
#27163=ORIENTED_EDGE('',*,*,#18563,.F.);
#27164=ORIENTED_EDGE('',*,*,#18564,.F.);
#27165=ORIENTED_EDGE('',*,*,#18565,.F.);
#27166=ORIENTED_EDGE('',*,*,#18566,.T.);
#27167=ORIENTED_EDGE('',*,*,#18567,.F.);
#27168=ORIENTED_EDGE('',*,*,#18568,.F.);
#27169=ORIENTED_EDGE('',*,*,#18569,.F.);
#27170=ORIENTED_EDGE('',*,*,#18570,.T.);
#27171=ORIENTED_EDGE('',*,*,#18571,.F.);
#27172=ORIENTED_EDGE('',*,*,#18572,.F.);
#27173=ORIENTED_EDGE('',*,*,#18573,.F.);
#27174=ORIENTED_EDGE('',*,*,#18574,.T.);
#27175=ORIENTED_EDGE('',*,*,#18575,.F.);
#27176=ORIENTED_EDGE('',*,*,#18576,.F.);
#27177=ORIENTED_EDGE('',*,*,#18577,.F.);
#27178=ORIENTED_EDGE('',*,*,#18578,.T.);
#27179=ORIENTED_EDGE('',*,*,#18579,.F.);
#27180=ORIENTED_EDGE('',*,*,#18580,.F.);
#27181=ORIENTED_EDGE('',*,*,#18581,.F.);
#27182=ORIENTED_EDGE('',*,*,#18582,.T.);
#27183=ORIENTED_EDGE('',*,*,#18583,.F.);
#27184=ORIENTED_EDGE('',*,*,#18584,.F.);
#27185=ORIENTED_EDGE('',*,*,#18585,.F.);
#27186=ORIENTED_EDGE('',*,*,#18586,.T.);
#27187=ORIENTED_EDGE('',*,*,#18587,.F.);
#27188=ORIENTED_EDGE('',*,*,#18588,.F.);
#27189=ORIENTED_EDGE('',*,*,#18589,.F.);
#27190=ORIENTED_EDGE('',*,*,#18590,.T.);
#27191=ORIENTED_EDGE('',*,*,#18591,.F.);
#27192=ORIENTED_EDGE('',*,*,#18592,.F.);
#27193=ORIENTED_EDGE('',*,*,#18593,.F.);
#27194=ORIENTED_EDGE('',*,*,#18594,.T.);
#27195=ORIENTED_EDGE('',*,*,#18595,.F.);
#27196=ORIENTED_EDGE('',*,*,#18596,.F.);
#27197=ORIENTED_EDGE('',*,*,#18597,.F.);
#27198=ORIENTED_EDGE('',*,*,#18598,.T.);
#27199=ORIENTED_EDGE('',*,*,#18599,.F.);
#27200=ORIENTED_EDGE('',*,*,#18600,.F.);
#27201=ORIENTED_EDGE('',*,*,#18601,.F.);
#27202=ORIENTED_EDGE('',*,*,#18602,.T.);
#27203=ORIENTED_EDGE('',*,*,#18603,.F.);
#27204=ORIENTED_EDGE('',*,*,#18604,.F.);
#27205=ORIENTED_EDGE('',*,*,#18605,.F.);
#27206=ORIENTED_EDGE('',*,*,#18606,.T.);
#27207=ORIENTED_EDGE('',*,*,#18607,.F.);
#27208=ORIENTED_EDGE('',*,*,#18608,.F.);
#27209=ORIENTED_EDGE('',*,*,#18609,.F.);
#27210=ORIENTED_EDGE('',*,*,#18610,.T.);
#27211=ORIENTED_EDGE('',*,*,#18611,.F.);
#27212=ORIENTED_EDGE('',*,*,#18612,.F.);
#27213=ORIENTED_EDGE('',*,*,#18613,.F.);
#27214=ORIENTED_EDGE('',*,*,#18614,.T.);
#27215=ORIENTED_EDGE('',*,*,#18615,.F.);
#27216=ORIENTED_EDGE('',*,*,#18616,.F.);
#27217=ORIENTED_EDGE('',*,*,#18617,.F.);
#27218=ORIENTED_EDGE('',*,*,#18618,.T.);
#27219=ORIENTED_EDGE('',*,*,#18619,.F.);
#27220=ORIENTED_EDGE('',*,*,#18620,.F.);
#27221=ORIENTED_EDGE('',*,*,#18621,.F.);
#27222=ORIENTED_EDGE('',*,*,#18622,.T.);
#27223=ORIENTED_EDGE('',*,*,#18623,.F.);
#27224=ORIENTED_EDGE('',*,*,#18624,.F.);
#27225=ORIENTED_EDGE('',*,*,#18625,.F.);
#27226=ORIENTED_EDGE('',*,*,#18626,.T.);
#27227=ORIENTED_EDGE('',*,*,#18627,.F.);
#27228=ORIENTED_EDGE('',*,*,#18628,.F.);
#27229=ORIENTED_EDGE('',*,*,#18629,.F.);
#27230=ORIENTED_EDGE('',*,*,#18630,.T.);
#27231=ORIENTED_EDGE('',*,*,#18631,.F.);
#27232=ORIENTED_EDGE('',*,*,#18632,.F.);
#27233=ORIENTED_EDGE('',*,*,#18633,.F.);
#27234=ORIENTED_EDGE('',*,*,#18634,.T.);
#27235=ORIENTED_EDGE('',*,*,#18635,.F.);
#27236=ORIENTED_EDGE('',*,*,#18636,.F.);
#27237=ORIENTED_EDGE('',*,*,#18637,.F.);
#27238=ORIENTED_EDGE('',*,*,#18638,.T.);
#27239=ORIENTED_EDGE('',*,*,#18639,.F.);
#27240=ORIENTED_EDGE('',*,*,#18640,.F.);
#27241=ORIENTED_EDGE('',*,*,#18641,.F.);
#27242=ORIENTED_EDGE('',*,*,#18642,.T.);
#27243=ORIENTED_EDGE('',*,*,#18643,.F.);
#27244=ORIENTED_EDGE('',*,*,#18644,.F.);
#27245=ORIENTED_EDGE('',*,*,#18645,.F.);
#27246=ORIENTED_EDGE('',*,*,#18646,.T.);
#27247=ORIENTED_EDGE('',*,*,#18647,.F.);
#27248=ORIENTED_EDGE('',*,*,#18648,.F.);
#27249=ORIENTED_EDGE('',*,*,#18649,.F.);
#27250=ORIENTED_EDGE('',*,*,#18650,.T.);
#27251=ORIENTED_EDGE('',*,*,#18651,.F.);
#27252=ORIENTED_EDGE('',*,*,#18652,.F.);
#27253=ORIENTED_EDGE('',*,*,#18653,.F.);
#27254=ORIENTED_EDGE('',*,*,#18654,.T.);
#27255=ORIENTED_EDGE('',*,*,#18655,.F.);
#27256=ORIENTED_EDGE('',*,*,#18656,.F.);
#27257=ORIENTED_EDGE('',*,*,#18657,.F.);
#27258=ORIENTED_EDGE('',*,*,#18658,.T.);
#27259=ORIENTED_EDGE('',*,*,#18659,.F.);
#27260=ORIENTED_EDGE('',*,*,#18660,.F.);
#27261=ORIENTED_EDGE('',*,*,#18661,.F.);
#27262=ORIENTED_EDGE('',*,*,#18662,.T.);
#27263=ORIENTED_EDGE('',*,*,#18663,.F.);
#27264=ORIENTED_EDGE('',*,*,#18664,.F.);
#27265=ORIENTED_EDGE('',*,*,#18665,.F.);
#27266=ORIENTED_EDGE('',*,*,#18666,.T.);
#27267=ORIENTED_EDGE('',*,*,#18667,.F.);
#27268=ORIENTED_EDGE('',*,*,#18668,.F.);
#27269=ORIENTED_EDGE('',*,*,#18669,.F.);
#27270=ORIENTED_EDGE('',*,*,#18670,.T.);
#27271=ORIENTED_EDGE('',*,*,#18671,.F.);
#27272=ORIENTED_EDGE('',*,*,#18672,.F.);
#27273=ORIENTED_EDGE('',*,*,#18673,.F.);
#27274=ORIENTED_EDGE('',*,*,#18674,.T.);
#27275=ORIENTED_EDGE('',*,*,#18675,.F.);
#27276=ORIENTED_EDGE('',*,*,#18676,.F.);
#27277=ORIENTED_EDGE('',*,*,#18677,.F.);
#27278=ORIENTED_EDGE('',*,*,#18678,.T.);
#27279=ORIENTED_EDGE('',*,*,#18679,.F.);
#27280=ORIENTED_EDGE('',*,*,#18680,.F.);
#27281=ORIENTED_EDGE('',*,*,#18681,.F.);
#27282=ORIENTED_EDGE('',*,*,#18682,.T.);
#27283=ORIENTED_EDGE('',*,*,#18683,.F.);
#27284=ORIENTED_EDGE('',*,*,#18684,.F.);
#27285=ORIENTED_EDGE('',*,*,#18685,.F.);
#27286=ORIENTED_EDGE('',*,*,#18686,.T.);
#27287=ORIENTED_EDGE('',*,*,#18687,.F.);
#27288=ORIENTED_EDGE('',*,*,#18688,.F.);
#27289=ORIENTED_EDGE('',*,*,#18689,.F.);
#27290=ORIENTED_EDGE('',*,*,#18690,.T.);
#27291=ORIENTED_EDGE('',*,*,#18691,.F.);
#27292=ORIENTED_EDGE('',*,*,#18692,.F.);
#27293=ORIENTED_EDGE('',*,*,#18693,.F.);
#27294=ORIENTED_EDGE('',*,*,#18694,.T.);
#27295=ORIENTED_EDGE('',*,*,#18695,.F.);
#27296=ORIENTED_EDGE('',*,*,#18696,.F.);
#27297=ORIENTED_EDGE('',*,*,#18697,.F.);
#27298=ORIENTED_EDGE('',*,*,#18698,.T.);
#27299=ORIENTED_EDGE('',*,*,#18699,.F.);
#27300=ORIENTED_EDGE('',*,*,#18700,.F.);
#27301=ORIENTED_EDGE('',*,*,#18701,.F.);
#27302=ORIENTED_EDGE('',*,*,#18702,.T.);
#27303=ORIENTED_EDGE('',*,*,#18703,.F.);
#27304=ORIENTED_EDGE('',*,*,#18704,.F.);
#27305=ORIENTED_EDGE('',*,*,#18705,.F.);
#27306=ORIENTED_EDGE('',*,*,#18706,.T.);
#27307=ORIENTED_EDGE('',*,*,#18707,.F.);
#27308=ORIENTED_EDGE('',*,*,#18708,.F.);
#27309=ORIENTED_EDGE('',*,*,#18709,.F.);
#27310=ORIENTED_EDGE('',*,*,#18710,.T.);
#27311=ORIENTED_EDGE('',*,*,#18711,.F.);
#27312=ORIENTED_EDGE('',*,*,#18712,.F.);
#27313=ORIENTED_EDGE('',*,*,#18713,.F.);
#27314=ORIENTED_EDGE('',*,*,#18714,.T.);
#27315=ORIENTED_EDGE('',*,*,#18715,.F.);
#27316=ORIENTED_EDGE('',*,*,#18117,.F.);
#27317=ORIENTED_EDGE('',*,*,#18716,.F.);
#27318=ORIENTED_EDGE('',*,*,#18717,.T.);
#27319=ORIENTED_EDGE('',*,*,#18718,.F.);
#27320=ORIENTED_EDGE('',*,*,#18113,.F.);
#27321=ORIENTED_EDGE('',*,*,#18719,.F.);
#27322=ORIENTED_EDGE('',*,*,#18720,.T.);
#27323=ORIENTED_EDGE('',*,*,#18721,.F.);
#27324=ORIENTED_EDGE('',*,*,#18109,.F.);
#27325=ORIENTED_EDGE('',*,*,#18722,.F.);
#27326=ORIENTED_EDGE('',*,*,#18723,.T.);
#27327=ORIENTED_EDGE('',*,*,#18724,.F.);
#27328=ORIENTED_EDGE('',*,*,#18105,.F.);
#27329=ORIENTED_EDGE('',*,*,#18725,.F.);
#27330=ORIENTED_EDGE('',*,*,#18726,.T.);
#27331=ORIENTED_EDGE('',*,*,#18727,.F.);
#27332=ORIENTED_EDGE('',*,*,#18101,.F.);
#27333=ORIENTED_EDGE('',*,*,#18728,.F.);
#27334=ORIENTED_EDGE('',*,*,#18729,.T.);
#27335=ORIENTED_EDGE('',*,*,#18730,.F.);
#27336=ORIENTED_EDGE('',*,*,#18097,.F.);
#27337=ORIENTED_EDGE('',*,*,#18731,.F.);
#27338=ORIENTED_EDGE('',*,*,#18732,.T.);
#27339=ORIENTED_EDGE('',*,*,#18733,.F.);
#27340=ORIENTED_EDGE('',*,*,#18121,.F.);
#27341=ORIENTED_EDGE('',*,*,#18734,.F.);
#27342=ORIENTED_EDGE('',*,*,#18735,.T.);
#27343=ORIENTED_EDGE('',*,*,#18736,.F.);
#27344=ORIENTED_EDGE('',*,*,#18125,.F.);
#27345=ORIENTED_EDGE('',*,*,#18737,.F.);
#27346=ORIENTED_EDGE('',*,*,#18738,.T.);
#27347=ORIENTED_EDGE('',*,*,#18739,.F.);
#27348=ORIENTED_EDGE('',*,*,#18129,.F.);
#27349=ORIENTED_EDGE('',*,*,#18740,.F.);
#27350=ORIENTED_EDGE('',*,*,#18741,.T.);
#27351=ORIENTED_EDGE('',*,*,#18742,.F.);
#27352=ORIENTED_EDGE('',*,*,#18133,.F.);
#27353=ORIENTED_EDGE('',*,*,#18743,.F.);
#27354=ORIENTED_EDGE('',*,*,#18744,.T.);
#27355=ORIENTED_EDGE('',*,*,#18745,.F.);
#27356=ORIENTED_EDGE('',*,*,#18137,.F.);
#27357=ORIENTED_EDGE('',*,*,#18746,.F.);
#27358=ORIENTED_EDGE('',*,*,#18747,.T.);
#27359=ORIENTED_EDGE('',*,*,#18748,.F.);
#27360=ORIENTED_EDGE('',*,*,#18141,.F.);
#27361=ORIENTED_EDGE('',*,*,#18749,.F.);
#27362=ORIENTED_EDGE('',*,*,#18750,.T.);
#27363=ORIENTED_EDGE('',*,*,#18751,.F.);
#27364=ORIENTED_EDGE('',*,*,#18145,.F.);
#27365=ORIENTED_EDGE('',*,*,#18752,.F.);
#27366=ORIENTED_EDGE('',*,*,#18753,.T.);
#27367=ORIENTED_EDGE('',*,*,#18754,.F.);
#27368=ORIENTED_EDGE('',*,*,#18149,.F.);
#27369=ORIENTED_EDGE('',*,*,#18755,.F.);
#27370=ORIENTED_EDGE('',*,*,#18756,.T.);
#27371=ORIENTED_EDGE('',*,*,#18757,.F.);
#27372=ORIENTED_EDGE('',*,*,#18153,.F.);
#27373=ORIENTED_EDGE('',*,*,#18758,.F.);
#27374=ORIENTED_EDGE('',*,*,#18759,.T.);
#27375=ORIENTED_EDGE('',*,*,#18760,.F.);
#27376=ORIENTED_EDGE('',*,*,#18761,.F.);
#27377=ORIENTED_EDGE('',*,*,#18762,.F.);
#27378=ORIENTED_EDGE('',*,*,#18763,.T.);
#27379=ORIENTED_EDGE('',*,*,#18764,.F.);
#27380=ORIENTED_EDGE('',*,*,#18765,.F.);
#27381=ORIENTED_EDGE('',*,*,#18766,.F.);
#27382=ORIENTED_EDGE('',*,*,#18767,.T.);
#27383=ORIENTED_EDGE('',*,*,#18768,.F.);
#27384=ORIENTED_EDGE('',*,*,#18769,.F.);
#27385=ORIENTED_EDGE('',*,*,#18770,.F.);
#27386=ORIENTED_EDGE('',*,*,#18771,.T.);
#27387=ORIENTED_EDGE('',*,*,#18772,.F.);
#27388=ORIENTED_EDGE('',*,*,#18773,.F.);
#27389=ORIENTED_EDGE('',*,*,#18774,.F.);
#27390=ORIENTED_EDGE('',*,*,#18775,.T.);
#27391=ORIENTED_EDGE('',*,*,#18776,.F.);
#27392=ORIENTED_EDGE('',*,*,#18777,.F.);
#27393=ORIENTED_EDGE('',*,*,#18778,.F.);
#27394=ORIENTED_EDGE('',*,*,#18779,.T.);
#27395=ORIENTED_EDGE('',*,*,#18780,.F.);
#27396=ORIENTED_EDGE('',*,*,#18781,.F.);
#27397=ORIENTED_EDGE('',*,*,#18782,.T.);
#27398=ORIENTED_EDGE('',*,*,#18783,.F.);
#27399=ORIENTED_EDGE('',*,*,#18784,.F.);
#27400=ORIENTED_EDGE('',*,*,#18782,.F.);
#27401=ORIENTED_EDGE('',*,*,#18785,.F.);
#27402=ORIENTED_EDGE('',*,*,#18786,.T.);
#27403=ORIENTED_EDGE('',*,*,#18783,.T.);
#27404=ORIENTED_EDGE('',*,*,#18784,.T.);
#27405=ORIENTED_EDGE('',*,*,#18786,.F.);
#27406=ORIENTED_EDGE('',*,*,#18787,.F.);
#27407=ORIENTED_EDGE('',*,*,#18788,.T.);
#27408=ORIENTED_EDGE('',*,*,#18785,.T.);
#27409=ORIENTED_EDGE('',*,*,#18788,.F.);
#27410=ORIENTED_EDGE('',*,*,#18789,.F.);
#27411=ORIENTED_EDGE('',*,*,#18790,.T.);
#27412=ORIENTED_EDGE('',*,*,#18787,.T.);
#27413=ORIENTED_EDGE('',*,*,#18790,.F.);
#27414=ORIENTED_EDGE('',*,*,#17912,.F.);
#27415=ORIENTED_EDGE('',*,*,#18791,.T.);
#27416=ORIENTED_EDGE('',*,*,#18792,.T.);
#27417=ORIENTED_EDGE('',*,*,#18791,.F.);
#27418=ORIENTED_EDGE('',*,*,#18793,.F.);
#27419=ORIENTED_EDGE('',*,*,#18794,.T.);
#27420=ORIENTED_EDGE('',*,*,#18795,.F.);
#27421=ORIENTED_EDGE('',*,*,#18732,.F.);
#27422=ORIENTED_EDGE('',*,*,#18796,.F.);
#27423=ORIENTED_EDGE('',*,*,#18729,.F.);
#27424=ORIENTED_EDGE('',*,*,#18797,.F.);
#27425=ORIENTED_EDGE('',*,*,#18798,.T.);
#27426=ORIENTED_EDGE('',*,*,#18799,.F.);
#27427=ORIENTED_EDGE('',*,*,#18726,.F.);
#27428=ORIENTED_EDGE('',*,*,#18800,.F.);
#27429=ORIENTED_EDGE('',*,*,#18801,.T.);
#27430=ORIENTED_EDGE('',*,*,#18802,.F.);
#27431=ORIENTED_EDGE('',*,*,#18723,.F.);
#27432=ORIENTED_EDGE('',*,*,#18803,.F.);
#27433=ORIENTED_EDGE('',*,*,#18804,.T.);
#27434=ORIENTED_EDGE('',*,*,#18805,.F.);
#27435=ORIENTED_EDGE('',*,*,#18720,.F.);
#27436=ORIENTED_EDGE('',*,*,#18806,.F.);
#27437=ORIENTED_EDGE('',*,*,#18807,.T.);
#27438=ORIENTED_EDGE('',*,*,#18808,.F.);
#27439=ORIENTED_EDGE('',*,*,#18717,.F.);
#27440=ORIENTED_EDGE('',*,*,#18809,.F.);
#27441=ORIENTED_EDGE('',*,*,#18810,.T.);
#27442=ORIENTED_EDGE('',*,*,#18811,.F.);
#27443=ORIENTED_EDGE('',*,*,#18714,.F.);
#27444=ORIENTED_EDGE('',*,*,#18812,.F.);
#27445=ORIENTED_EDGE('',*,*,#18813,.T.);
#27446=ORIENTED_EDGE('',*,*,#18814,.F.);
#27447=ORIENTED_EDGE('',*,*,#18710,.F.);
#27448=ORIENTED_EDGE('',*,*,#18815,.F.);
#27449=ORIENTED_EDGE('',*,*,#18816,.T.);
#27450=ORIENTED_EDGE('',*,*,#18817,.F.);
#27451=ORIENTED_EDGE('',*,*,#18706,.F.);
#27452=ORIENTED_EDGE('',*,*,#18818,.F.);
#27453=ORIENTED_EDGE('',*,*,#18819,.T.);
#27454=ORIENTED_EDGE('',*,*,#18820,.F.);
#27455=ORIENTED_EDGE('',*,*,#18702,.F.);
#27456=ORIENTED_EDGE('',*,*,#18821,.F.);
#27457=ORIENTED_EDGE('',*,*,#18822,.T.);
#27458=ORIENTED_EDGE('',*,*,#18823,.F.);
#27459=ORIENTED_EDGE('',*,*,#18698,.F.);
#27460=ORIENTED_EDGE('',*,*,#18824,.F.);
#27461=ORIENTED_EDGE('',*,*,#18825,.T.);
#27462=ORIENTED_EDGE('',*,*,#18826,.F.);
#27463=ORIENTED_EDGE('',*,*,#18694,.F.);
#27464=ORIENTED_EDGE('',*,*,#18827,.F.);
#27465=ORIENTED_EDGE('',*,*,#18828,.T.);
#27466=ORIENTED_EDGE('',*,*,#18829,.F.);
#27467=ORIENTED_EDGE('',*,*,#18690,.F.);
#27468=ORIENTED_EDGE('',*,*,#18830,.F.);
#27469=ORIENTED_EDGE('',*,*,#18831,.T.);
#27470=ORIENTED_EDGE('',*,*,#18832,.F.);
#27471=ORIENTED_EDGE('',*,*,#18686,.F.);
#27472=ORIENTED_EDGE('',*,*,#18833,.F.);
#27473=ORIENTED_EDGE('',*,*,#18834,.T.);
#27474=ORIENTED_EDGE('',*,*,#18835,.F.);
#27475=ORIENTED_EDGE('',*,*,#18682,.F.);
#27476=ORIENTED_EDGE('',*,*,#18836,.F.);
#27477=ORIENTED_EDGE('',*,*,#18837,.T.);
#27478=ORIENTED_EDGE('',*,*,#18838,.F.);
#27479=ORIENTED_EDGE('',*,*,#18678,.F.);
#27480=ORIENTED_EDGE('',*,*,#18839,.F.);
#27481=ORIENTED_EDGE('',*,*,#18840,.T.);
#27482=ORIENTED_EDGE('',*,*,#18841,.F.);
#27483=ORIENTED_EDGE('',*,*,#18674,.F.);
#27484=ORIENTED_EDGE('',*,*,#18842,.F.);
#27485=ORIENTED_EDGE('',*,*,#18843,.T.);
#27486=ORIENTED_EDGE('',*,*,#18844,.F.);
#27487=ORIENTED_EDGE('',*,*,#18670,.F.);
#27488=ORIENTED_EDGE('',*,*,#18845,.F.);
#27489=ORIENTED_EDGE('',*,*,#18846,.T.);
#27490=ORIENTED_EDGE('',*,*,#18847,.F.);
#27491=ORIENTED_EDGE('',*,*,#18666,.F.);
#27492=ORIENTED_EDGE('',*,*,#18848,.F.);
#27493=ORIENTED_EDGE('',*,*,#18849,.T.);
#27494=ORIENTED_EDGE('',*,*,#18850,.F.);
#27495=ORIENTED_EDGE('',*,*,#18662,.F.);
#27496=ORIENTED_EDGE('',*,*,#18851,.F.);
#27497=ORIENTED_EDGE('',*,*,#18852,.T.);
#27498=ORIENTED_EDGE('',*,*,#18853,.F.);
#27499=ORIENTED_EDGE('',*,*,#18658,.F.);
#27500=ORIENTED_EDGE('',*,*,#18854,.F.);
#27501=ORIENTED_EDGE('',*,*,#18855,.T.);
#27502=ORIENTED_EDGE('',*,*,#18856,.F.);
#27503=ORIENTED_EDGE('',*,*,#18654,.F.);
#27504=ORIENTED_EDGE('',*,*,#18857,.F.);
#27505=ORIENTED_EDGE('',*,*,#18858,.T.);
#27506=ORIENTED_EDGE('',*,*,#18859,.F.);
#27507=ORIENTED_EDGE('',*,*,#18650,.F.);
#27508=ORIENTED_EDGE('',*,*,#18860,.F.);
#27509=ORIENTED_EDGE('',*,*,#18861,.T.);
#27510=ORIENTED_EDGE('',*,*,#18862,.F.);
#27511=ORIENTED_EDGE('',*,*,#18646,.F.);
#27512=ORIENTED_EDGE('',*,*,#18863,.F.);
#27513=ORIENTED_EDGE('',*,*,#18864,.T.);
#27514=ORIENTED_EDGE('',*,*,#18865,.F.);
#27515=ORIENTED_EDGE('',*,*,#18642,.F.);
#27516=ORIENTED_EDGE('',*,*,#18866,.F.);
#27517=ORIENTED_EDGE('',*,*,#18867,.T.);
#27518=ORIENTED_EDGE('',*,*,#18868,.F.);
#27519=ORIENTED_EDGE('',*,*,#18638,.F.);
#27520=ORIENTED_EDGE('',*,*,#18869,.F.);
#27521=ORIENTED_EDGE('',*,*,#18870,.T.);
#27522=ORIENTED_EDGE('',*,*,#18871,.F.);
#27523=ORIENTED_EDGE('',*,*,#18634,.F.);
#27524=ORIENTED_EDGE('',*,*,#18872,.F.);
#27525=ORIENTED_EDGE('',*,*,#18873,.T.);
#27526=ORIENTED_EDGE('',*,*,#18874,.F.);
#27527=ORIENTED_EDGE('',*,*,#18630,.F.);
#27528=ORIENTED_EDGE('',*,*,#18875,.F.);
#27529=ORIENTED_EDGE('',*,*,#18876,.T.);
#27530=ORIENTED_EDGE('',*,*,#18877,.F.);
#27531=ORIENTED_EDGE('',*,*,#18626,.F.);
#27532=ORIENTED_EDGE('',*,*,#18878,.F.);
#27533=ORIENTED_EDGE('',*,*,#18879,.T.);
#27534=ORIENTED_EDGE('',*,*,#18880,.F.);
#27535=ORIENTED_EDGE('',*,*,#18622,.F.);
#27536=ORIENTED_EDGE('',*,*,#18881,.F.);
#27537=ORIENTED_EDGE('',*,*,#18882,.T.);
#27538=ORIENTED_EDGE('',*,*,#18883,.F.);
#27539=ORIENTED_EDGE('',*,*,#18618,.F.);
#27540=ORIENTED_EDGE('',*,*,#18884,.F.);
#27541=ORIENTED_EDGE('',*,*,#18885,.T.);
#27542=ORIENTED_EDGE('',*,*,#18886,.F.);
#27543=ORIENTED_EDGE('',*,*,#18614,.F.);
#27544=ORIENTED_EDGE('',*,*,#18887,.F.);
#27545=ORIENTED_EDGE('',*,*,#18888,.T.);
#27546=ORIENTED_EDGE('',*,*,#18889,.F.);
#27547=ORIENTED_EDGE('',*,*,#18610,.F.);
#27548=ORIENTED_EDGE('',*,*,#18890,.F.);
#27549=ORIENTED_EDGE('',*,*,#18891,.T.);
#27550=ORIENTED_EDGE('',*,*,#18892,.F.);
#27551=ORIENTED_EDGE('',*,*,#18606,.F.);
#27552=ORIENTED_EDGE('',*,*,#18893,.F.);
#27553=ORIENTED_EDGE('',*,*,#18894,.T.);
#27554=ORIENTED_EDGE('',*,*,#18895,.F.);
#27555=ORIENTED_EDGE('',*,*,#18602,.F.);
#27556=ORIENTED_EDGE('',*,*,#18896,.F.);
#27557=ORIENTED_EDGE('',*,*,#18897,.T.);
#27558=ORIENTED_EDGE('',*,*,#18898,.F.);
#27559=ORIENTED_EDGE('',*,*,#18598,.F.);
#27560=ORIENTED_EDGE('',*,*,#18899,.F.);
#27561=ORIENTED_EDGE('',*,*,#18900,.T.);
#27562=ORIENTED_EDGE('',*,*,#18901,.F.);
#27563=ORIENTED_EDGE('',*,*,#18594,.F.);
#27564=ORIENTED_EDGE('',*,*,#18902,.F.);
#27565=ORIENTED_EDGE('',*,*,#18903,.T.);
#27566=ORIENTED_EDGE('',*,*,#18904,.F.);
#27567=ORIENTED_EDGE('',*,*,#18590,.F.);
#27568=ORIENTED_EDGE('',*,*,#18905,.F.);
#27569=ORIENTED_EDGE('',*,*,#18906,.T.);
#27570=ORIENTED_EDGE('',*,*,#18907,.F.);
#27571=ORIENTED_EDGE('',*,*,#18586,.F.);
#27572=ORIENTED_EDGE('',*,*,#18908,.F.);
#27573=ORIENTED_EDGE('',*,*,#18909,.T.);
#27574=ORIENTED_EDGE('',*,*,#18910,.F.);
#27575=ORIENTED_EDGE('',*,*,#18582,.F.);
#27576=ORIENTED_EDGE('',*,*,#18911,.F.);
#27577=ORIENTED_EDGE('',*,*,#18912,.T.);
#27578=ORIENTED_EDGE('',*,*,#18913,.F.);
#27579=ORIENTED_EDGE('',*,*,#18578,.F.);
#27580=ORIENTED_EDGE('',*,*,#18914,.F.);
#27581=ORIENTED_EDGE('',*,*,#18915,.T.);
#27582=ORIENTED_EDGE('',*,*,#18916,.F.);
#27583=ORIENTED_EDGE('',*,*,#18574,.F.);
#27584=ORIENTED_EDGE('',*,*,#18917,.F.);
#27585=ORIENTED_EDGE('',*,*,#18918,.T.);
#27586=ORIENTED_EDGE('',*,*,#18919,.F.);
#27587=ORIENTED_EDGE('',*,*,#18570,.F.);
#27588=ORIENTED_EDGE('',*,*,#18920,.F.);
#27589=ORIENTED_EDGE('',*,*,#18921,.T.);
#27590=ORIENTED_EDGE('',*,*,#18922,.F.);
#27591=ORIENTED_EDGE('',*,*,#18566,.F.);
#27592=ORIENTED_EDGE('',*,*,#18923,.F.);
#27593=ORIENTED_EDGE('',*,*,#18924,.T.);
#27594=ORIENTED_EDGE('',*,*,#18925,.F.);
#27595=ORIENTED_EDGE('',*,*,#18562,.F.);
#27596=ORIENTED_EDGE('',*,*,#18926,.F.);
#27597=ORIENTED_EDGE('',*,*,#18927,.T.);
#27598=ORIENTED_EDGE('',*,*,#18928,.F.);
#27599=ORIENTED_EDGE('',*,*,#18558,.F.);
#27600=ORIENTED_EDGE('',*,*,#18929,.F.);
#27601=ORIENTED_EDGE('',*,*,#18930,.T.);
#27602=ORIENTED_EDGE('',*,*,#18931,.F.);
#27603=ORIENTED_EDGE('',*,*,#18554,.F.);
#27604=ORIENTED_EDGE('',*,*,#18932,.F.);
#27605=ORIENTED_EDGE('',*,*,#18933,.T.);
#27606=ORIENTED_EDGE('',*,*,#18934,.F.);
#27607=ORIENTED_EDGE('',*,*,#18550,.F.);
#27608=ORIENTED_EDGE('',*,*,#18935,.F.);
#27609=ORIENTED_EDGE('',*,*,#18936,.T.);
#27610=ORIENTED_EDGE('',*,*,#18937,.F.);
#27611=ORIENTED_EDGE('',*,*,#18546,.F.);
#27612=ORIENTED_EDGE('',*,*,#18938,.F.);
#27613=ORIENTED_EDGE('',*,*,#18939,.T.);
#27614=ORIENTED_EDGE('',*,*,#18940,.F.);
#27615=ORIENTED_EDGE('',*,*,#18542,.F.);
#27616=ORIENTED_EDGE('',*,*,#18941,.F.);
#27617=ORIENTED_EDGE('',*,*,#18942,.T.);
#27618=ORIENTED_EDGE('',*,*,#18943,.F.);
#27619=ORIENTED_EDGE('',*,*,#18538,.F.);
#27620=ORIENTED_EDGE('',*,*,#18944,.F.);
#27621=ORIENTED_EDGE('',*,*,#18945,.T.);
#27622=ORIENTED_EDGE('',*,*,#18946,.F.);
#27623=ORIENTED_EDGE('',*,*,#18534,.F.);
#27624=ORIENTED_EDGE('',*,*,#18947,.F.);
#27625=ORIENTED_EDGE('',*,*,#18948,.T.);
#27626=ORIENTED_EDGE('',*,*,#18949,.F.);
#27627=ORIENTED_EDGE('',*,*,#18530,.F.);
#27628=ORIENTED_EDGE('',*,*,#18950,.F.);
#27629=ORIENTED_EDGE('',*,*,#18951,.T.);
#27630=ORIENTED_EDGE('',*,*,#18952,.F.);
#27631=ORIENTED_EDGE('',*,*,#18526,.F.);
#27632=ORIENTED_EDGE('',*,*,#18953,.F.);
#27633=ORIENTED_EDGE('',*,*,#18954,.T.);
#27634=ORIENTED_EDGE('',*,*,#18955,.F.);
#27635=ORIENTED_EDGE('',*,*,#18522,.F.);
#27636=ORIENTED_EDGE('',*,*,#18956,.F.);
#27637=ORIENTED_EDGE('',*,*,#18957,.T.);
#27638=ORIENTED_EDGE('',*,*,#18958,.F.);
#27639=ORIENTED_EDGE('',*,*,#18518,.F.);
#27640=ORIENTED_EDGE('',*,*,#18959,.F.);
#27641=ORIENTED_EDGE('',*,*,#18960,.T.);
#27642=ORIENTED_EDGE('',*,*,#18961,.F.);
#27643=ORIENTED_EDGE('',*,*,#18514,.F.);
#27644=ORIENTED_EDGE('',*,*,#18962,.F.);
#27645=ORIENTED_EDGE('',*,*,#18963,.T.);
#27646=ORIENTED_EDGE('',*,*,#18964,.F.);
#27647=ORIENTED_EDGE('',*,*,#18510,.F.);
#27648=ORIENTED_EDGE('',*,*,#18965,.F.);
#27649=ORIENTED_EDGE('',*,*,#18966,.T.);
#27650=ORIENTED_EDGE('',*,*,#18967,.F.);
#27651=ORIENTED_EDGE('',*,*,#18506,.F.);
#27652=ORIENTED_EDGE('',*,*,#18968,.F.);
#27653=ORIENTED_EDGE('',*,*,#18969,.T.);
#27654=ORIENTED_EDGE('',*,*,#18970,.F.);
#27655=ORIENTED_EDGE('',*,*,#18502,.F.);
#27656=ORIENTED_EDGE('',*,*,#18971,.F.);
#27657=ORIENTED_EDGE('',*,*,#18972,.T.);
#27658=ORIENTED_EDGE('',*,*,#18973,.F.);
#27659=ORIENTED_EDGE('',*,*,#18498,.F.);
#27660=ORIENTED_EDGE('',*,*,#18974,.F.);
#27661=ORIENTED_EDGE('',*,*,#18975,.T.);
#27662=ORIENTED_EDGE('',*,*,#18976,.F.);
#27663=ORIENTED_EDGE('',*,*,#18494,.F.);
#27664=ORIENTED_EDGE('',*,*,#18977,.F.);
#27665=ORIENTED_EDGE('',*,*,#18978,.T.);
#27666=ORIENTED_EDGE('',*,*,#18979,.F.);
#27667=ORIENTED_EDGE('',*,*,#18490,.F.);
#27668=ORIENTED_EDGE('',*,*,#18980,.F.);
#27669=ORIENTED_EDGE('',*,*,#18981,.T.);
#27670=ORIENTED_EDGE('',*,*,#18982,.F.);
#27671=ORIENTED_EDGE('',*,*,#18486,.F.);
#27672=ORIENTED_EDGE('',*,*,#18983,.F.);
#27673=ORIENTED_EDGE('',*,*,#18984,.T.);
#27674=ORIENTED_EDGE('',*,*,#18985,.F.);
#27675=ORIENTED_EDGE('',*,*,#18986,.T.);
#27676=ORIENTED_EDGE('',*,*,#18987,.F.);
#27677=ORIENTED_EDGE('',*,*,#18735,.F.);
#27678=ORIENTED_EDGE('',*,*,#18988,.F.);
#27679=ORIENTED_EDGE('',*,*,#18989,.T.);
#27680=ORIENTED_EDGE('',*,*,#18990,.F.);
#27681=ORIENTED_EDGE('',*,*,#18738,.F.);
#27682=ORIENTED_EDGE('',*,*,#18991,.F.);
#27683=ORIENTED_EDGE('',*,*,#18992,.T.);
#27684=ORIENTED_EDGE('',*,*,#18993,.F.);
#27685=ORIENTED_EDGE('',*,*,#18741,.F.);
#27686=ORIENTED_EDGE('',*,*,#18994,.F.);
#27687=ORIENTED_EDGE('',*,*,#18995,.T.);
#27688=ORIENTED_EDGE('',*,*,#18996,.F.);
#27689=ORIENTED_EDGE('',*,*,#18744,.F.);
#27690=ORIENTED_EDGE('',*,*,#18997,.F.);
#27691=ORIENTED_EDGE('',*,*,#18998,.T.);
#27692=ORIENTED_EDGE('',*,*,#18999,.F.);
#27693=ORIENTED_EDGE('',*,*,#18747,.F.);
#27694=ORIENTED_EDGE('',*,*,#19000,.F.);
#27695=ORIENTED_EDGE('',*,*,#19001,.T.);
#27696=ORIENTED_EDGE('',*,*,#19002,.F.);
#27697=ORIENTED_EDGE('',*,*,#18750,.F.);
#27698=ORIENTED_EDGE('',*,*,#19003,.F.);
#27699=ORIENTED_EDGE('',*,*,#19004,.T.);
#27700=ORIENTED_EDGE('',*,*,#19005,.F.);
#27701=ORIENTED_EDGE('',*,*,#18753,.F.);
#27702=ORIENTED_EDGE('',*,*,#19006,.F.);
#27703=ORIENTED_EDGE('',*,*,#19007,.T.);
#27704=ORIENTED_EDGE('',*,*,#19008,.F.);
#27705=ORIENTED_EDGE('',*,*,#18756,.F.);
#27706=ORIENTED_EDGE('',*,*,#19009,.F.);
#27707=ORIENTED_EDGE('',*,*,#19010,.T.);
#27708=ORIENTED_EDGE('',*,*,#19011,.F.);
#27709=ORIENTED_EDGE('',*,*,#18759,.F.);
#27710=ORIENTED_EDGE('',*,*,#19012,.F.);
#27711=ORIENTED_EDGE('',*,*,#19013,.T.);
#27712=ORIENTED_EDGE('',*,*,#19014,.F.);
#27713=ORIENTED_EDGE('',*,*,#18763,.F.);
#27714=ORIENTED_EDGE('',*,*,#19015,.F.);
#27715=ORIENTED_EDGE('',*,*,#19016,.T.);
#27716=ORIENTED_EDGE('',*,*,#19017,.F.);
#27717=ORIENTED_EDGE('',*,*,#18767,.F.);
#27718=ORIENTED_EDGE('',*,*,#19018,.F.);
#27719=ORIENTED_EDGE('',*,*,#19019,.T.);
#27720=ORIENTED_EDGE('',*,*,#19020,.F.);
#27721=ORIENTED_EDGE('',*,*,#18771,.F.);
#27722=ORIENTED_EDGE('',*,*,#19021,.F.);
#27723=ORIENTED_EDGE('',*,*,#19022,.T.);
#27724=ORIENTED_EDGE('',*,*,#19023,.F.);
#27725=ORIENTED_EDGE('',*,*,#18775,.F.);
#27726=ORIENTED_EDGE('',*,*,#19024,.F.);
#27727=ORIENTED_EDGE('',*,*,#19025,.T.);
#27728=ORIENTED_EDGE('',*,*,#19026,.F.);
#27729=ORIENTED_EDGE('',*,*,#18779,.F.);
#27730=ORIENTED_EDGE('',*,*,#19027,.F.);
#27731=ORIENTED_EDGE('',*,*,#18482,.F.);
#27732=ORIENTED_EDGE('',*,*,#19028,.F.);
#27733=ORIENTED_EDGE('',*,*,#19029,.T.);
#27734=ORIENTED_EDGE('',*,*,#19030,.F.);
#27735=ORIENTED_EDGE('',*,*,#19031,.T.);
#27736=ORIENTED_EDGE('',*,*,#19032,.F.);
#27737=ORIENTED_EDGE('',*,*,#18794,.F.);
#27738=ORIENTED_EDGE('',*,*,#19033,.F.);
#27739=ORIENTED_EDGE('',*,*,#18798,.F.);
#27740=ORIENTED_EDGE('',*,*,#19034,.F.);
#27741=ORIENTED_EDGE('',*,*,#19035,.T.);
#27742=ORIENTED_EDGE('',*,*,#19036,.F.);
#27743=ORIENTED_EDGE('',*,*,#18801,.F.);
#27744=ORIENTED_EDGE('',*,*,#19037,.F.);
#27745=ORIENTED_EDGE('',*,*,#19038,.T.);
#27746=ORIENTED_EDGE('',*,*,#19039,.F.);
#27747=ORIENTED_EDGE('',*,*,#18804,.F.);
#27748=ORIENTED_EDGE('',*,*,#19040,.F.);
#27749=ORIENTED_EDGE('',*,*,#19041,.T.);
#27750=ORIENTED_EDGE('',*,*,#19042,.F.);
#27751=ORIENTED_EDGE('',*,*,#18807,.F.);
#27752=ORIENTED_EDGE('',*,*,#19043,.F.);
#27753=ORIENTED_EDGE('',*,*,#19044,.T.);
#27754=ORIENTED_EDGE('',*,*,#19045,.F.);
#27755=ORIENTED_EDGE('',*,*,#18810,.F.);
#27756=ORIENTED_EDGE('',*,*,#19046,.F.);
#27757=ORIENTED_EDGE('',*,*,#19047,.T.);
#27758=ORIENTED_EDGE('',*,*,#19048,.F.);
#27759=ORIENTED_EDGE('',*,*,#18813,.F.);
#27760=ORIENTED_EDGE('',*,*,#19049,.F.);
#27761=ORIENTED_EDGE('',*,*,#19050,.T.);
#27762=ORIENTED_EDGE('',*,*,#19051,.F.);
#27763=ORIENTED_EDGE('',*,*,#18816,.F.);
#27764=ORIENTED_EDGE('',*,*,#19052,.F.);
#27765=ORIENTED_EDGE('',*,*,#19053,.T.);
#27766=ORIENTED_EDGE('',*,*,#19054,.F.);
#27767=ORIENTED_EDGE('',*,*,#18819,.F.);
#27768=ORIENTED_EDGE('',*,*,#19055,.F.);
#27769=ORIENTED_EDGE('',*,*,#19056,.T.);
#27770=ORIENTED_EDGE('',*,*,#19057,.F.);
#27771=ORIENTED_EDGE('',*,*,#18822,.F.);
#27772=ORIENTED_EDGE('',*,*,#19058,.F.);
#27773=ORIENTED_EDGE('',*,*,#19059,.T.);
#27774=ORIENTED_EDGE('',*,*,#19060,.F.);
#27775=ORIENTED_EDGE('',*,*,#18825,.F.);
#27776=ORIENTED_EDGE('',*,*,#19061,.F.);
#27777=ORIENTED_EDGE('',*,*,#19062,.T.);
#27778=ORIENTED_EDGE('',*,*,#19063,.F.);
#27779=ORIENTED_EDGE('',*,*,#18828,.F.);
#27780=ORIENTED_EDGE('',*,*,#19064,.F.);
#27781=ORIENTED_EDGE('',*,*,#19065,.T.);
#27782=ORIENTED_EDGE('',*,*,#19066,.F.);
#27783=ORIENTED_EDGE('',*,*,#18831,.F.);
#27784=ORIENTED_EDGE('',*,*,#19067,.F.);
#27785=ORIENTED_EDGE('',*,*,#19068,.T.);
#27786=ORIENTED_EDGE('',*,*,#19069,.F.);
#27787=ORIENTED_EDGE('',*,*,#18834,.F.);
#27788=ORIENTED_EDGE('',*,*,#19070,.F.);
#27789=ORIENTED_EDGE('',*,*,#19071,.T.);
#27790=ORIENTED_EDGE('',*,*,#19072,.F.);
#27791=ORIENTED_EDGE('',*,*,#18837,.F.);
#27792=ORIENTED_EDGE('',*,*,#19073,.F.);
#27793=ORIENTED_EDGE('',*,*,#19074,.T.);
#27794=ORIENTED_EDGE('',*,*,#19075,.F.);
#27795=ORIENTED_EDGE('',*,*,#18840,.F.);
#27796=ORIENTED_EDGE('',*,*,#19076,.F.);
#27797=ORIENTED_EDGE('',*,*,#19077,.T.);
#27798=ORIENTED_EDGE('',*,*,#19078,.F.);
#27799=ORIENTED_EDGE('',*,*,#18843,.F.);
#27800=ORIENTED_EDGE('',*,*,#19079,.F.);
#27801=ORIENTED_EDGE('',*,*,#19080,.T.);
#27802=ORIENTED_EDGE('',*,*,#19081,.F.);
#27803=ORIENTED_EDGE('',*,*,#18846,.F.);
#27804=ORIENTED_EDGE('',*,*,#19082,.F.);
#27805=ORIENTED_EDGE('',*,*,#19083,.T.);
#27806=ORIENTED_EDGE('',*,*,#19084,.F.);
#27807=ORIENTED_EDGE('',*,*,#18849,.F.);
#27808=ORIENTED_EDGE('',*,*,#19085,.F.);
#27809=ORIENTED_EDGE('',*,*,#19086,.T.);
#27810=ORIENTED_EDGE('',*,*,#19087,.F.);
#27811=ORIENTED_EDGE('',*,*,#18852,.F.);
#27812=ORIENTED_EDGE('',*,*,#19088,.F.);
#27813=ORIENTED_EDGE('',*,*,#19089,.T.);
#27814=ORIENTED_EDGE('',*,*,#19090,.F.);
#27815=ORIENTED_EDGE('',*,*,#18855,.F.);
#27816=ORIENTED_EDGE('',*,*,#19091,.F.);
#27817=ORIENTED_EDGE('',*,*,#19092,.T.);
#27818=ORIENTED_EDGE('',*,*,#19093,.F.);
#27819=ORIENTED_EDGE('',*,*,#18858,.F.);
#27820=ORIENTED_EDGE('',*,*,#19094,.F.);
#27821=ORIENTED_EDGE('',*,*,#19095,.T.);
#27822=ORIENTED_EDGE('',*,*,#19096,.F.);
#27823=ORIENTED_EDGE('',*,*,#18861,.F.);
#27824=ORIENTED_EDGE('',*,*,#19097,.F.);
#27825=ORIENTED_EDGE('',*,*,#19098,.T.);
#27826=ORIENTED_EDGE('',*,*,#19099,.F.);
#27827=ORIENTED_EDGE('',*,*,#18864,.F.);
#27828=ORIENTED_EDGE('',*,*,#19100,.F.);
#27829=ORIENTED_EDGE('',*,*,#19101,.T.);
#27830=ORIENTED_EDGE('',*,*,#19102,.F.);
#27831=ORIENTED_EDGE('',*,*,#18867,.F.);
#27832=ORIENTED_EDGE('',*,*,#19103,.F.);
#27833=ORIENTED_EDGE('',*,*,#19104,.T.);
#27834=ORIENTED_EDGE('',*,*,#19105,.F.);
#27835=ORIENTED_EDGE('',*,*,#18870,.F.);
#27836=ORIENTED_EDGE('',*,*,#19106,.F.);
#27837=ORIENTED_EDGE('',*,*,#19107,.T.);
#27838=ORIENTED_EDGE('',*,*,#19108,.F.);
#27839=ORIENTED_EDGE('',*,*,#18873,.F.);
#27840=ORIENTED_EDGE('',*,*,#19109,.F.);
#27841=ORIENTED_EDGE('',*,*,#19110,.T.);
#27842=ORIENTED_EDGE('',*,*,#19111,.F.);
#27843=ORIENTED_EDGE('',*,*,#18876,.F.);
#27844=ORIENTED_EDGE('',*,*,#19112,.F.);
#27845=ORIENTED_EDGE('',*,*,#19113,.T.);
#27846=ORIENTED_EDGE('',*,*,#19114,.F.);
#27847=ORIENTED_EDGE('',*,*,#18879,.F.);
#27848=ORIENTED_EDGE('',*,*,#19115,.F.);
#27849=ORIENTED_EDGE('',*,*,#19116,.T.);
#27850=ORIENTED_EDGE('',*,*,#19117,.F.);
#27851=ORIENTED_EDGE('',*,*,#18882,.F.);
#27852=ORIENTED_EDGE('',*,*,#19118,.F.);
#27853=ORIENTED_EDGE('',*,*,#19119,.T.);
#27854=ORIENTED_EDGE('',*,*,#19120,.F.);
#27855=ORIENTED_EDGE('',*,*,#18885,.F.);
#27856=ORIENTED_EDGE('',*,*,#19121,.F.);
#27857=ORIENTED_EDGE('',*,*,#19122,.T.);
#27858=ORIENTED_EDGE('',*,*,#19123,.F.);
#27859=ORIENTED_EDGE('',*,*,#18888,.F.);
#27860=ORIENTED_EDGE('',*,*,#19124,.F.);
#27861=ORIENTED_EDGE('',*,*,#19125,.T.);
#27862=ORIENTED_EDGE('',*,*,#19126,.F.);
#27863=ORIENTED_EDGE('',*,*,#18891,.F.);
#27864=ORIENTED_EDGE('',*,*,#19127,.F.);
#27865=ORIENTED_EDGE('',*,*,#19128,.T.);
#27866=ORIENTED_EDGE('',*,*,#19129,.F.);
#27867=ORIENTED_EDGE('',*,*,#18894,.F.);
#27868=ORIENTED_EDGE('',*,*,#19130,.F.);
#27869=ORIENTED_EDGE('',*,*,#19131,.T.);
#27870=ORIENTED_EDGE('',*,*,#19132,.F.);
#27871=ORIENTED_EDGE('',*,*,#18897,.F.);
#27872=ORIENTED_EDGE('',*,*,#19133,.F.);
#27873=ORIENTED_EDGE('',*,*,#19134,.T.);
#27874=ORIENTED_EDGE('',*,*,#19135,.F.);
#27875=ORIENTED_EDGE('',*,*,#18900,.F.);
#27876=ORIENTED_EDGE('',*,*,#19136,.F.);
#27877=ORIENTED_EDGE('',*,*,#19137,.T.);
#27878=ORIENTED_EDGE('',*,*,#19138,.F.);
#27879=ORIENTED_EDGE('',*,*,#18903,.F.);
#27880=ORIENTED_EDGE('',*,*,#19139,.F.);
#27881=ORIENTED_EDGE('',*,*,#19140,.T.);
#27882=ORIENTED_EDGE('',*,*,#19141,.F.);
#27883=ORIENTED_EDGE('',*,*,#18906,.F.);
#27884=ORIENTED_EDGE('',*,*,#19142,.F.);
#27885=ORIENTED_EDGE('',*,*,#19143,.T.);
#27886=ORIENTED_EDGE('',*,*,#19144,.F.);
#27887=ORIENTED_EDGE('',*,*,#18909,.F.);
#27888=ORIENTED_EDGE('',*,*,#19145,.F.);
#27889=ORIENTED_EDGE('',*,*,#19146,.T.);
#27890=ORIENTED_EDGE('',*,*,#19147,.F.);
#27891=ORIENTED_EDGE('',*,*,#18912,.F.);
#27892=ORIENTED_EDGE('',*,*,#19148,.F.);
#27893=ORIENTED_EDGE('',*,*,#19149,.T.);
#27894=ORIENTED_EDGE('',*,*,#19150,.F.);
#27895=ORIENTED_EDGE('',*,*,#18915,.F.);
#27896=ORIENTED_EDGE('',*,*,#19151,.F.);
#27897=ORIENTED_EDGE('',*,*,#19152,.T.);
#27898=ORIENTED_EDGE('',*,*,#19153,.F.);
#27899=ORIENTED_EDGE('',*,*,#18918,.F.);
#27900=ORIENTED_EDGE('',*,*,#19154,.F.);
#27901=ORIENTED_EDGE('',*,*,#19155,.T.);
#27902=ORIENTED_EDGE('',*,*,#19156,.F.);
#27903=ORIENTED_EDGE('',*,*,#18921,.F.);
#27904=ORIENTED_EDGE('',*,*,#19157,.F.);
#27905=ORIENTED_EDGE('',*,*,#19158,.T.);
#27906=ORIENTED_EDGE('',*,*,#19159,.F.);
#27907=ORIENTED_EDGE('',*,*,#18924,.F.);
#27908=ORIENTED_EDGE('',*,*,#19160,.F.);
#27909=ORIENTED_EDGE('',*,*,#19161,.T.);
#27910=ORIENTED_EDGE('',*,*,#19162,.F.);
#27911=ORIENTED_EDGE('',*,*,#18927,.F.);
#27912=ORIENTED_EDGE('',*,*,#19163,.F.);
#27913=ORIENTED_EDGE('',*,*,#19164,.T.);
#27914=ORIENTED_EDGE('',*,*,#19165,.F.);
#27915=ORIENTED_EDGE('',*,*,#18930,.F.);
#27916=ORIENTED_EDGE('',*,*,#19166,.F.);
#27917=ORIENTED_EDGE('',*,*,#19167,.T.);
#27918=ORIENTED_EDGE('',*,*,#19168,.F.);
#27919=ORIENTED_EDGE('',*,*,#18933,.F.);
#27920=ORIENTED_EDGE('',*,*,#19169,.F.);
#27921=ORIENTED_EDGE('',*,*,#19170,.T.);
#27922=ORIENTED_EDGE('',*,*,#19171,.F.);
#27923=ORIENTED_EDGE('',*,*,#18936,.F.);
#27924=ORIENTED_EDGE('',*,*,#19172,.F.);
#27925=ORIENTED_EDGE('',*,*,#19173,.T.);
#27926=ORIENTED_EDGE('',*,*,#19174,.F.);
#27927=ORIENTED_EDGE('',*,*,#18939,.F.);
#27928=ORIENTED_EDGE('',*,*,#19175,.F.);
#27929=ORIENTED_EDGE('',*,*,#19176,.T.);
#27930=ORIENTED_EDGE('',*,*,#19177,.F.);
#27931=ORIENTED_EDGE('',*,*,#18942,.F.);
#27932=ORIENTED_EDGE('',*,*,#19178,.F.);
#27933=ORIENTED_EDGE('',*,*,#19179,.T.);
#27934=ORIENTED_EDGE('',*,*,#19180,.F.);
#27935=ORIENTED_EDGE('',*,*,#18945,.F.);
#27936=ORIENTED_EDGE('',*,*,#19181,.F.);
#27937=ORIENTED_EDGE('',*,*,#19182,.T.);
#27938=ORIENTED_EDGE('',*,*,#19183,.F.);
#27939=ORIENTED_EDGE('',*,*,#18948,.F.);
#27940=ORIENTED_EDGE('',*,*,#19184,.F.);
#27941=ORIENTED_EDGE('',*,*,#19185,.T.);
#27942=ORIENTED_EDGE('',*,*,#19186,.F.);
#27943=ORIENTED_EDGE('',*,*,#18951,.F.);
#27944=ORIENTED_EDGE('',*,*,#19187,.F.);
#27945=ORIENTED_EDGE('',*,*,#19188,.T.);
#27946=ORIENTED_EDGE('',*,*,#19189,.F.);
#27947=ORIENTED_EDGE('',*,*,#18954,.F.);
#27948=ORIENTED_EDGE('',*,*,#19190,.F.);
#27949=ORIENTED_EDGE('',*,*,#19191,.T.);
#27950=ORIENTED_EDGE('',*,*,#19192,.F.);
#27951=ORIENTED_EDGE('',*,*,#18957,.F.);
#27952=ORIENTED_EDGE('',*,*,#19193,.F.);
#27953=ORIENTED_EDGE('',*,*,#19194,.T.);
#27954=ORIENTED_EDGE('',*,*,#19195,.F.);
#27955=ORIENTED_EDGE('',*,*,#18960,.F.);
#27956=ORIENTED_EDGE('',*,*,#19196,.F.);
#27957=ORIENTED_EDGE('',*,*,#19197,.T.);
#27958=ORIENTED_EDGE('',*,*,#19198,.F.);
#27959=ORIENTED_EDGE('',*,*,#18963,.F.);
#27960=ORIENTED_EDGE('',*,*,#19199,.F.);
#27961=ORIENTED_EDGE('',*,*,#19200,.T.);
#27962=ORIENTED_EDGE('',*,*,#19201,.F.);
#27963=ORIENTED_EDGE('',*,*,#18966,.F.);
#27964=ORIENTED_EDGE('',*,*,#19202,.F.);
#27965=ORIENTED_EDGE('',*,*,#19203,.T.);
#27966=ORIENTED_EDGE('',*,*,#19204,.F.);
#27967=ORIENTED_EDGE('',*,*,#18969,.F.);
#27968=ORIENTED_EDGE('',*,*,#19205,.F.);
#27969=ORIENTED_EDGE('',*,*,#19206,.T.);
#27970=ORIENTED_EDGE('',*,*,#19207,.F.);
#27971=ORIENTED_EDGE('',*,*,#18972,.F.);
#27972=ORIENTED_EDGE('',*,*,#19208,.F.);
#27973=ORIENTED_EDGE('',*,*,#19209,.T.);
#27974=ORIENTED_EDGE('',*,*,#19210,.F.);
#27975=ORIENTED_EDGE('',*,*,#18975,.F.);
#27976=ORIENTED_EDGE('',*,*,#19211,.F.);
#27977=ORIENTED_EDGE('',*,*,#19212,.T.);
#27978=ORIENTED_EDGE('',*,*,#19213,.F.);
#27979=ORIENTED_EDGE('',*,*,#18978,.F.);
#27980=ORIENTED_EDGE('',*,*,#19214,.F.);
#27981=ORIENTED_EDGE('',*,*,#19215,.T.);
#27982=ORIENTED_EDGE('',*,*,#19216,.F.);
#27983=ORIENTED_EDGE('',*,*,#18981,.F.);
#27984=ORIENTED_EDGE('',*,*,#19217,.F.);
#27985=ORIENTED_EDGE('',*,*,#19218,.T.);
#27986=ORIENTED_EDGE('',*,*,#19219,.F.);
#27987=ORIENTED_EDGE('',*,*,#18984,.F.);
#27988=ORIENTED_EDGE('',*,*,#19220,.F.);
#27989=ORIENTED_EDGE('',*,*,#19221,.T.);
#27990=ORIENTED_EDGE('',*,*,#19222,.F.);
#27991=ORIENTED_EDGE('',*,*,#19223,.T.);
#27992=ORIENTED_EDGE('',*,*,#19224,.F.);
#27993=ORIENTED_EDGE('',*,*,#18986,.F.);
#27994=ORIENTED_EDGE('',*,*,#19225,.F.);
#27995=ORIENTED_EDGE('',*,*,#19226,.T.);
#27996=ORIENTED_EDGE('',*,*,#19227,.F.);
#27997=ORIENTED_EDGE('',*,*,#18989,.F.);
#27998=ORIENTED_EDGE('',*,*,#19228,.F.);
#27999=ORIENTED_EDGE('',*,*,#19229,.T.);
#28000=ORIENTED_EDGE('',*,*,#19230,.F.);
#28001=ORIENTED_EDGE('',*,*,#18992,.F.);
#28002=ORIENTED_EDGE('',*,*,#19231,.F.);
#28003=ORIENTED_EDGE('',*,*,#19232,.T.);
#28004=ORIENTED_EDGE('',*,*,#19233,.F.);
#28005=ORIENTED_EDGE('',*,*,#18995,.F.);
#28006=ORIENTED_EDGE('',*,*,#19234,.F.);
#28007=ORIENTED_EDGE('',*,*,#19235,.T.);
#28008=ORIENTED_EDGE('',*,*,#19236,.F.);
#28009=ORIENTED_EDGE('',*,*,#18998,.F.);
#28010=ORIENTED_EDGE('',*,*,#19237,.F.);
#28011=ORIENTED_EDGE('',*,*,#19238,.T.);
#28012=ORIENTED_EDGE('',*,*,#19239,.F.);
#28013=ORIENTED_EDGE('',*,*,#19001,.F.);
#28014=ORIENTED_EDGE('',*,*,#19240,.F.);
#28015=ORIENTED_EDGE('',*,*,#19241,.T.);
#28016=ORIENTED_EDGE('',*,*,#19242,.F.);
#28017=ORIENTED_EDGE('',*,*,#19004,.F.);
#28018=ORIENTED_EDGE('',*,*,#19243,.F.);
#28019=ORIENTED_EDGE('',*,*,#19244,.T.);
#28020=ORIENTED_EDGE('',*,*,#19245,.F.);
#28021=ORIENTED_EDGE('',*,*,#19007,.F.);
#28022=ORIENTED_EDGE('',*,*,#19246,.F.);
#28023=ORIENTED_EDGE('',*,*,#19247,.T.);
#28024=ORIENTED_EDGE('',*,*,#19248,.F.);
#28025=ORIENTED_EDGE('',*,*,#19010,.F.);
#28026=ORIENTED_EDGE('',*,*,#19249,.F.);
#28027=ORIENTED_EDGE('',*,*,#19250,.T.);
#28028=ORIENTED_EDGE('',*,*,#19251,.F.);
#28029=ORIENTED_EDGE('',*,*,#19013,.F.);
#28030=ORIENTED_EDGE('',*,*,#19252,.F.);
#28031=ORIENTED_EDGE('',*,*,#19253,.T.);
#28032=ORIENTED_EDGE('',*,*,#19254,.F.);
#28033=ORIENTED_EDGE('',*,*,#19016,.F.);
#28034=ORIENTED_EDGE('',*,*,#19255,.F.);
#28035=ORIENTED_EDGE('',*,*,#19256,.T.);
#28036=ORIENTED_EDGE('',*,*,#19257,.F.);
#28037=ORIENTED_EDGE('',*,*,#19019,.F.);
#28038=ORIENTED_EDGE('',*,*,#19258,.F.);
#28039=ORIENTED_EDGE('',*,*,#19259,.T.);
#28040=ORIENTED_EDGE('',*,*,#19260,.F.);
#28041=ORIENTED_EDGE('',*,*,#19022,.F.);
#28042=ORIENTED_EDGE('',*,*,#19261,.F.);
#28043=ORIENTED_EDGE('',*,*,#19262,.T.);
#28044=ORIENTED_EDGE('',*,*,#19263,.F.);
#28045=ORIENTED_EDGE('',*,*,#19025,.F.);
#28046=ORIENTED_EDGE('',*,*,#19264,.F.);
#28047=ORIENTED_EDGE('',*,*,#19029,.F.);
#28048=ORIENTED_EDGE('',*,*,#19265,.F.);
#28049=ORIENTED_EDGE('',*,*,#19266,.T.);
#28050=ORIENTED_EDGE('',*,*,#19267,.F.);
#28051=ORIENTED_EDGE('',*,*,#18378,.T.);
#28052=ORIENTED_EDGE('',*,*,#19268,.F.);
#28053=ORIENTED_EDGE('',*,*,#19031,.F.);
#28054=ORIENTED_EDGE('',*,*,#19269,.F.);
#28055=ORIENTED_EDGE('',*,*,#19035,.F.);
#28056=ORIENTED_EDGE('',*,*,#19270,.F.);
#28057=ORIENTED_EDGE('',*,*,#18381,.T.);
#28058=ORIENTED_EDGE('',*,*,#19271,.F.);
#28059=ORIENTED_EDGE('',*,*,#19038,.F.);
#28060=ORIENTED_EDGE('',*,*,#19272,.F.);
#28061=ORIENTED_EDGE('',*,*,#18384,.T.);
#28062=ORIENTED_EDGE('',*,*,#19273,.F.);
#28063=ORIENTED_EDGE('',*,*,#19041,.F.);
#28064=ORIENTED_EDGE('',*,*,#19274,.F.);
#28065=ORIENTED_EDGE('',*,*,#18387,.T.);
#28066=ORIENTED_EDGE('',*,*,#19275,.F.);
#28067=ORIENTED_EDGE('',*,*,#19044,.F.);
#28068=ORIENTED_EDGE('',*,*,#19276,.F.);
#28069=ORIENTED_EDGE('',*,*,#18390,.T.);
#28070=ORIENTED_EDGE('',*,*,#19277,.F.);
#28071=ORIENTED_EDGE('',*,*,#19047,.F.);
#28072=ORIENTED_EDGE('',*,*,#19278,.F.);
#28073=ORIENTED_EDGE('',*,*,#18393,.T.);
#28074=ORIENTED_EDGE('',*,*,#19279,.F.);
#28075=ORIENTED_EDGE('',*,*,#19050,.F.);
#28076=ORIENTED_EDGE('',*,*,#19280,.F.);
#28077=ORIENTED_EDGE('',*,*,#18396,.T.);
#28078=ORIENTED_EDGE('',*,*,#19281,.F.);
#28079=ORIENTED_EDGE('',*,*,#19053,.F.);
#28080=ORIENTED_EDGE('',*,*,#19282,.F.);
#28081=ORIENTED_EDGE('',*,*,#18400,.T.);
#28082=ORIENTED_EDGE('',*,*,#19283,.F.);
#28083=ORIENTED_EDGE('',*,*,#19056,.F.);
#28084=ORIENTED_EDGE('',*,*,#19284,.F.);
#28085=ORIENTED_EDGE('',*,*,#18404,.T.);
#28086=ORIENTED_EDGE('',*,*,#19285,.F.);
#28087=ORIENTED_EDGE('',*,*,#19059,.F.);
#28088=ORIENTED_EDGE('',*,*,#19286,.F.);
#28089=ORIENTED_EDGE('',*,*,#18408,.T.);
#28090=ORIENTED_EDGE('',*,*,#19287,.F.);
#28091=ORIENTED_EDGE('',*,*,#19062,.F.);
#28092=ORIENTED_EDGE('',*,*,#19288,.F.);
#28093=ORIENTED_EDGE('',*,*,#18412,.T.);
#28094=ORIENTED_EDGE('',*,*,#19289,.F.);
#28095=ORIENTED_EDGE('',*,*,#19065,.F.);
#28096=ORIENTED_EDGE('',*,*,#19290,.F.);
#28097=ORIENTED_EDGE('',*,*,#18416,.T.);
#28098=ORIENTED_EDGE('',*,*,#19291,.F.);
#28099=ORIENTED_EDGE('',*,*,#19068,.F.);
#28100=ORIENTED_EDGE('',*,*,#19292,.F.);
#28101=ORIENTED_EDGE('',*,*,#18420,.T.);
#28102=ORIENTED_EDGE('',*,*,#19293,.F.);
#28103=ORIENTED_EDGE('',*,*,#19071,.F.);
#28104=ORIENTED_EDGE('',*,*,#19294,.F.);
#28105=ORIENTED_EDGE('',*,*,#18424,.T.);
#28106=ORIENTED_EDGE('',*,*,#19295,.F.);
#28107=ORIENTED_EDGE('',*,*,#19074,.F.);
#28108=ORIENTED_EDGE('',*,*,#19296,.F.);
#28109=ORIENTED_EDGE('',*,*,#18428,.T.);
#28110=ORIENTED_EDGE('',*,*,#19297,.F.);
#28111=ORIENTED_EDGE('',*,*,#19077,.F.);
#28112=ORIENTED_EDGE('',*,*,#19298,.F.);
#28113=ORIENTED_EDGE('',*,*,#18432,.T.);
#28114=ORIENTED_EDGE('',*,*,#19299,.F.);
#28115=ORIENTED_EDGE('',*,*,#19080,.F.);
#28116=ORIENTED_EDGE('',*,*,#19300,.F.);
#28117=ORIENTED_EDGE('',*,*,#18436,.T.);
#28118=ORIENTED_EDGE('',*,*,#19301,.F.);
#28119=ORIENTED_EDGE('',*,*,#19083,.F.);
#28120=ORIENTED_EDGE('',*,*,#19302,.F.);
#28121=ORIENTED_EDGE('',*,*,#18440,.T.);
#28122=ORIENTED_EDGE('',*,*,#19303,.F.);
#28123=ORIENTED_EDGE('',*,*,#19086,.F.);
#28124=ORIENTED_EDGE('',*,*,#19304,.F.);
#28125=ORIENTED_EDGE('',*,*,#18444,.T.);
#28126=ORIENTED_EDGE('',*,*,#19305,.F.);
#28127=ORIENTED_EDGE('',*,*,#19089,.F.);
#28128=ORIENTED_EDGE('',*,*,#19306,.F.);
#28129=ORIENTED_EDGE('',*,*,#18448,.T.);
#28130=ORIENTED_EDGE('',*,*,#19307,.F.);
#28131=ORIENTED_EDGE('',*,*,#19092,.F.);
#28132=ORIENTED_EDGE('',*,*,#19308,.F.);
#28133=ORIENTED_EDGE('',*,*,#18452,.T.);
#28134=ORIENTED_EDGE('',*,*,#19309,.F.);
#28135=ORIENTED_EDGE('',*,*,#19095,.F.);
#28136=ORIENTED_EDGE('',*,*,#19310,.F.);
#28137=ORIENTED_EDGE('',*,*,#18456,.T.);
#28138=ORIENTED_EDGE('',*,*,#19311,.F.);
#28139=ORIENTED_EDGE('',*,*,#19098,.F.);
#28140=ORIENTED_EDGE('',*,*,#19312,.F.);
#28141=ORIENTED_EDGE('',*,*,#18460,.T.);
#28142=ORIENTED_EDGE('',*,*,#19313,.F.);
#28143=ORIENTED_EDGE('',*,*,#19101,.F.);
#28144=ORIENTED_EDGE('',*,*,#19314,.F.);
#28145=ORIENTED_EDGE('',*,*,#18464,.T.);
#28146=ORIENTED_EDGE('',*,*,#19315,.F.);
#28147=ORIENTED_EDGE('',*,*,#19104,.F.);
#28148=ORIENTED_EDGE('',*,*,#19316,.F.);
#28149=ORIENTED_EDGE('',*,*,#18468,.T.);
#28150=ORIENTED_EDGE('',*,*,#19317,.F.);
#28151=ORIENTED_EDGE('',*,*,#19107,.F.);
#28152=ORIENTED_EDGE('',*,*,#19318,.F.);
#28153=ORIENTED_EDGE('',*,*,#18472,.T.);
#28154=ORIENTED_EDGE('',*,*,#19319,.F.);
#28155=ORIENTED_EDGE('',*,*,#19110,.F.);
#28156=ORIENTED_EDGE('',*,*,#19320,.F.);
#28157=ORIENTED_EDGE('',*,*,#18171,.T.);
#28158=ORIENTED_EDGE('',*,*,#19321,.F.);
#28159=ORIENTED_EDGE('',*,*,#19113,.F.);
#28160=ORIENTED_EDGE('',*,*,#19322,.F.);
#28161=ORIENTED_EDGE('',*,*,#18175,.T.);
#28162=ORIENTED_EDGE('',*,*,#19323,.F.);
#28163=ORIENTED_EDGE('',*,*,#19116,.F.);
#28164=ORIENTED_EDGE('',*,*,#19324,.F.);
#28165=ORIENTED_EDGE('',*,*,#18179,.T.);
#28166=ORIENTED_EDGE('',*,*,#19325,.F.);
#28167=ORIENTED_EDGE('',*,*,#19119,.F.);
#28168=ORIENTED_EDGE('',*,*,#19326,.F.);
#28169=ORIENTED_EDGE('',*,*,#18183,.T.);
#28170=ORIENTED_EDGE('',*,*,#19327,.F.);
#28171=ORIENTED_EDGE('',*,*,#19122,.F.);
#28172=ORIENTED_EDGE('',*,*,#19328,.F.);
#28173=ORIENTED_EDGE('',*,*,#18187,.T.);
#28174=ORIENTED_EDGE('',*,*,#19329,.F.);
#28175=ORIENTED_EDGE('',*,*,#19125,.F.);
#28176=ORIENTED_EDGE('',*,*,#19330,.F.);
#28177=ORIENTED_EDGE('',*,*,#18191,.T.);
#28178=ORIENTED_EDGE('',*,*,#19331,.F.);
#28179=ORIENTED_EDGE('',*,*,#19128,.F.);
#28180=ORIENTED_EDGE('',*,*,#19332,.F.);
#28181=ORIENTED_EDGE('',*,*,#18195,.T.);
#28182=ORIENTED_EDGE('',*,*,#19333,.F.);
#28183=ORIENTED_EDGE('',*,*,#19131,.F.);
#28184=ORIENTED_EDGE('',*,*,#19334,.F.);
#28185=ORIENTED_EDGE('',*,*,#18199,.T.);
#28186=ORIENTED_EDGE('',*,*,#19335,.F.);
#28187=ORIENTED_EDGE('',*,*,#19134,.F.);
#28188=ORIENTED_EDGE('',*,*,#19336,.F.);
#28189=ORIENTED_EDGE('',*,*,#18203,.T.);
#28190=ORIENTED_EDGE('',*,*,#19337,.F.);
#28191=ORIENTED_EDGE('',*,*,#19137,.F.);
#28192=ORIENTED_EDGE('',*,*,#19338,.F.);
#28193=ORIENTED_EDGE('',*,*,#18207,.T.);
#28194=ORIENTED_EDGE('',*,*,#19339,.F.);
#28195=ORIENTED_EDGE('',*,*,#19140,.F.);
#28196=ORIENTED_EDGE('',*,*,#19340,.F.);
#28197=ORIENTED_EDGE('',*,*,#18211,.T.);
#28198=ORIENTED_EDGE('',*,*,#19341,.F.);
#28199=ORIENTED_EDGE('',*,*,#19143,.F.);
#28200=ORIENTED_EDGE('',*,*,#19342,.F.);
#28201=ORIENTED_EDGE('',*,*,#18215,.T.);
#28202=ORIENTED_EDGE('',*,*,#19343,.F.);
#28203=ORIENTED_EDGE('',*,*,#19146,.F.);
#28204=ORIENTED_EDGE('',*,*,#19344,.F.);
#28205=ORIENTED_EDGE('',*,*,#18219,.T.);
#28206=ORIENTED_EDGE('',*,*,#19345,.F.);
#28207=ORIENTED_EDGE('',*,*,#19149,.F.);
#28208=ORIENTED_EDGE('',*,*,#19346,.F.);
#28209=ORIENTED_EDGE('',*,*,#18223,.T.);
#28210=ORIENTED_EDGE('',*,*,#19347,.F.);
#28211=ORIENTED_EDGE('',*,*,#19152,.F.);
#28212=ORIENTED_EDGE('',*,*,#19348,.F.);
#28213=ORIENTED_EDGE('',*,*,#18227,.T.);
#28214=ORIENTED_EDGE('',*,*,#19349,.F.);
#28215=ORIENTED_EDGE('',*,*,#19155,.F.);
#28216=ORIENTED_EDGE('',*,*,#19350,.F.);
#28217=ORIENTED_EDGE('',*,*,#18231,.T.);
#28218=ORIENTED_EDGE('',*,*,#19351,.F.);
#28219=ORIENTED_EDGE('',*,*,#19158,.F.);
#28220=ORIENTED_EDGE('',*,*,#19352,.F.);
#28221=ORIENTED_EDGE('',*,*,#18235,.T.);
#28222=ORIENTED_EDGE('',*,*,#19353,.F.);
#28223=ORIENTED_EDGE('',*,*,#19161,.F.);
#28224=ORIENTED_EDGE('',*,*,#19354,.F.);
#28225=ORIENTED_EDGE('',*,*,#18239,.T.);
#28226=ORIENTED_EDGE('',*,*,#19355,.F.);
#28227=ORIENTED_EDGE('',*,*,#19164,.F.);
#28228=ORIENTED_EDGE('',*,*,#19356,.F.);
#28229=ORIENTED_EDGE('',*,*,#18243,.T.);
#28230=ORIENTED_EDGE('',*,*,#19357,.F.);
#28231=ORIENTED_EDGE('',*,*,#19167,.F.);
#28232=ORIENTED_EDGE('',*,*,#19358,.F.);
#28233=ORIENTED_EDGE('',*,*,#18247,.T.);
#28234=ORIENTED_EDGE('',*,*,#19359,.F.);
#28235=ORIENTED_EDGE('',*,*,#19170,.F.);
#28236=ORIENTED_EDGE('',*,*,#19360,.F.);
#28237=ORIENTED_EDGE('',*,*,#18251,.T.);
#28238=ORIENTED_EDGE('',*,*,#19361,.F.);
#28239=ORIENTED_EDGE('',*,*,#19173,.F.);
#28240=ORIENTED_EDGE('',*,*,#19362,.F.);
#28241=ORIENTED_EDGE('',*,*,#18255,.T.);
#28242=ORIENTED_EDGE('',*,*,#19363,.F.);
#28243=ORIENTED_EDGE('',*,*,#19176,.F.);
#28244=ORIENTED_EDGE('',*,*,#19364,.F.);
#28245=ORIENTED_EDGE('',*,*,#18259,.T.);
#28246=ORIENTED_EDGE('',*,*,#19365,.F.);
#28247=ORIENTED_EDGE('',*,*,#19179,.F.);
#28248=ORIENTED_EDGE('',*,*,#19366,.F.);
#28249=ORIENTED_EDGE('',*,*,#18263,.T.);
#28250=ORIENTED_EDGE('',*,*,#19367,.F.);
#28251=ORIENTED_EDGE('',*,*,#19182,.F.);
#28252=ORIENTED_EDGE('',*,*,#19368,.F.);
#28253=ORIENTED_EDGE('',*,*,#18267,.T.);
#28254=ORIENTED_EDGE('',*,*,#19369,.F.);
#28255=ORIENTED_EDGE('',*,*,#19185,.F.);
#28256=ORIENTED_EDGE('',*,*,#19370,.F.);
#28257=ORIENTED_EDGE('',*,*,#18271,.T.);
#28258=ORIENTED_EDGE('',*,*,#19371,.F.);
#28259=ORIENTED_EDGE('',*,*,#19188,.F.);
#28260=ORIENTED_EDGE('',*,*,#19372,.F.);
#28261=ORIENTED_EDGE('',*,*,#18275,.T.);
#28262=ORIENTED_EDGE('',*,*,#19373,.F.);
#28263=ORIENTED_EDGE('',*,*,#19191,.F.);
#28264=ORIENTED_EDGE('',*,*,#19374,.F.);
#28265=ORIENTED_EDGE('',*,*,#18279,.T.);
#28266=ORIENTED_EDGE('',*,*,#19375,.F.);
#28267=ORIENTED_EDGE('',*,*,#19194,.F.);
#28268=ORIENTED_EDGE('',*,*,#19376,.F.);
#28269=ORIENTED_EDGE('',*,*,#18283,.T.);
#28270=ORIENTED_EDGE('',*,*,#19377,.F.);
#28271=ORIENTED_EDGE('',*,*,#19197,.F.);
#28272=ORIENTED_EDGE('',*,*,#19378,.F.);
#28273=ORIENTED_EDGE('',*,*,#18287,.T.);
#28274=ORIENTED_EDGE('',*,*,#19379,.F.);
#28275=ORIENTED_EDGE('',*,*,#19200,.F.);
#28276=ORIENTED_EDGE('',*,*,#19380,.F.);
#28277=ORIENTED_EDGE('',*,*,#18291,.T.);
#28278=ORIENTED_EDGE('',*,*,#19381,.F.);
#28279=ORIENTED_EDGE('',*,*,#19203,.F.);
#28280=ORIENTED_EDGE('',*,*,#19382,.F.);
#28281=ORIENTED_EDGE('',*,*,#18295,.T.);
#28282=ORIENTED_EDGE('',*,*,#19383,.F.);
#28283=ORIENTED_EDGE('',*,*,#19206,.F.);
#28284=ORIENTED_EDGE('',*,*,#19384,.F.);
#28285=ORIENTED_EDGE('',*,*,#18299,.T.);
#28286=ORIENTED_EDGE('',*,*,#19385,.F.);
#28287=ORIENTED_EDGE('',*,*,#19209,.F.);
#28288=ORIENTED_EDGE('',*,*,#19386,.F.);
#28289=ORIENTED_EDGE('',*,*,#18303,.T.);
#28290=ORIENTED_EDGE('',*,*,#19387,.F.);
#28291=ORIENTED_EDGE('',*,*,#19212,.F.);
#28292=ORIENTED_EDGE('',*,*,#19388,.F.);
#28293=ORIENTED_EDGE('',*,*,#18307,.T.);
#28294=ORIENTED_EDGE('',*,*,#19389,.F.);
#28295=ORIENTED_EDGE('',*,*,#19215,.F.);
#28296=ORIENTED_EDGE('',*,*,#19390,.F.);
#28297=ORIENTED_EDGE('',*,*,#18311,.T.);
#28298=ORIENTED_EDGE('',*,*,#19391,.F.);
#28299=ORIENTED_EDGE('',*,*,#19218,.F.);
#28300=ORIENTED_EDGE('',*,*,#19392,.F.);
#28301=ORIENTED_EDGE('',*,*,#18315,.T.);
#28302=ORIENTED_EDGE('',*,*,#19393,.F.);
#28303=ORIENTED_EDGE('',*,*,#19221,.F.);
#28304=ORIENTED_EDGE('',*,*,#19394,.F.);
#28305=ORIENTED_EDGE('',*,*,#18319,.T.);
#28306=ORIENTED_EDGE('',*,*,#19395,.F.);
#28307=ORIENTED_EDGE('',*,*,#18375,.T.);
#28308=ORIENTED_EDGE('',*,*,#19396,.F.);
#28309=ORIENTED_EDGE('',*,*,#19223,.F.);
#28310=ORIENTED_EDGE('',*,*,#19397,.F.);
#28311=ORIENTED_EDGE('',*,*,#18372,.T.);
#28312=ORIENTED_EDGE('',*,*,#19398,.F.);
#28313=ORIENTED_EDGE('',*,*,#19226,.F.);
#28314=ORIENTED_EDGE('',*,*,#19399,.F.);
#28315=ORIENTED_EDGE('',*,*,#18369,.T.);
#28316=ORIENTED_EDGE('',*,*,#19400,.F.);
#28317=ORIENTED_EDGE('',*,*,#19229,.F.);
#28318=ORIENTED_EDGE('',*,*,#19401,.F.);
#28319=ORIENTED_EDGE('',*,*,#18366,.T.);
#28320=ORIENTED_EDGE('',*,*,#19402,.F.);
#28321=ORIENTED_EDGE('',*,*,#19232,.F.);
#28322=ORIENTED_EDGE('',*,*,#19403,.F.);
#28323=ORIENTED_EDGE('',*,*,#18363,.T.);
#28324=ORIENTED_EDGE('',*,*,#19404,.F.);
#28325=ORIENTED_EDGE('',*,*,#19235,.F.);
#28326=ORIENTED_EDGE('',*,*,#19405,.F.);
#28327=ORIENTED_EDGE('',*,*,#18360,.T.);
#28328=ORIENTED_EDGE('',*,*,#19406,.F.);
#28329=ORIENTED_EDGE('',*,*,#19238,.F.);
#28330=ORIENTED_EDGE('',*,*,#19407,.F.);
#28331=ORIENTED_EDGE('',*,*,#18357,.T.);
#28332=ORIENTED_EDGE('',*,*,#19408,.F.);
#28333=ORIENTED_EDGE('',*,*,#19241,.F.);
#28334=ORIENTED_EDGE('',*,*,#19409,.F.);
#28335=ORIENTED_EDGE('',*,*,#18354,.T.);
#28336=ORIENTED_EDGE('',*,*,#19410,.F.);
#28337=ORIENTED_EDGE('',*,*,#19244,.F.);
#28338=ORIENTED_EDGE('',*,*,#19411,.F.);
#28339=ORIENTED_EDGE('',*,*,#18351,.T.);
#28340=ORIENTED_EDGE('',*,*,#19412,.F.);
#28341=ORIENTED_EDGE('',*,*,#19247,.F.);
#28342=ORIENTED_EDGE('',*,*,#19413,.F.);
#28343=ORIENTED_EDGE('',*,*,#18347,.T.);
#28344=ORIENTED_EDGE('',*,*,#19414,.F.);
#28345=ORIENTED_EDGE('',*,*,#19250,.F.);
#28346=ORIENTED_EDGE('',*,*,#19415,.F.);
#28347=ORIENTED_EDGE('',*,*,#18343,.T.);
#28348=ORIENTED_EDGE('',*,*,#19416,.F.);
#28349=ORIENTED_EDGE('',*,*,#19253,.F.);
#28350=ORIENTED_EDGE('',*,*,#19417,.F.);
#28351=ORIENTED_EDGE('',*,*,#18339,.T.);
#28352=ORIENTED_EDGE('',*,*,#19418,.F.);
#28353=ORIENTED_EDGE('',*,*,#19256,.F.);
#28354=ORIENTED_EDGE('',*,*,#19419,.F.);
#28355=ORIENTED_EDGE('',*,*,#18335,.T.);
#28356=ORIENTED_EDGE('',*,*,#19420,.F.);
#28357=ORIENTED_EDGE('',*,*,#19259,.F.);
#28358=ORIENTED_EDGE('',*,*,#19421,.F.);
#28359=ORIENTED_EDGE('',*,*,#18331,.T.);
#28360=ORIENTED_EDGE('',*,*,#19422,.F.);
#28361=ORIENTED_EDGE('',*,*,#19262,.F.);
#28362=ORIENTED_EDGE('',*,*,#19423,.F.);
#28363=ORIENTED_EDGE('',*,*,#19266,.F.);
#28364=ORIENTED_EDGE('',*,*,#19424,.F.);
#28365=ORIENTED_EDGE('',*,*,#18323,.T.);
#28366=ORIENTED_EDGE('',*,*,#18001,.T.);
#28367=ORIENTED_EDGE('',*,*,#18091,.T.);
#28368=ORIENTED_EDGE('',*,*,#17998,.T.);
#28369=ORIENTED_EDGE('',*,*,#18789,.T.);
#28370=ORIENTED_EDGE('',*,*,#18792,.F.);
#28371=ORIENTED_EDGE('',*,*,#19425,.F.);
#28372=ORIENTED_EDGE('',*,*,#18478,.F.);
#28373=ORIENTED_EDGE('',*,*,#19426,.F.);
#28374=ORIENTED_EDGE('',*,*,#19427,.T.);
#28375=ORIENTED_EDGE('',*,*,#19428,.F.);
#28376=ORIENTED_EDGE('',*,*,#19427,.F.);
#28377=ORIENTED_EDGE('',*,*,#19429,.F.);
#28378=ORIENTED_EDGE('',*,*,#19430,.T.);
#28379=ORIENTED_EDGE('',*,*,#19431,.F.);
#28380=ORIENTED_EDGE('',*,*,#19430,.F.);
#28381=ORIENTED_EDGE('',*,*,#19432,.F.);
#28382=ORIENTED_EDGE('',*,*,#18327,.T.);
#28383=ORIENTED_EDGE('',*,*,#18168,.F.);
#28384=ORIENTED_EDGE('',*,*,#18165,.F.);
#28385=ORIENTED_EDGE('',*,*,#19433,.T.);
#28386=ORIENTED_EDGE('',*,*,#19434,.T.);
#28387=ORIENTED_EDGE('',*,*,#19435,.T.);
#28388=ORIENTED_EDGE('',*,*,#19436,.T.);
#28389=ORIENTED_EDGE('',*,*,#19437,.T.);
#28390=ORIENTED_EDGE('',*,*,#19438,.T.);
#28391=ORIENTED_EDGE('',*,*,#19439,.T.);
#28392=ORIENTED_EDGE('',*,*,#18160,.T.);
#28393=ORIENTED_EDGE('',*,*,#19440,.F.);
#28394=ORIENTED_EDGE('',*,*,#19434,.F.);
#28395=ORIENTED_EDGE('',*,*,#19440,.T.);
#28396=ORIENTED_EDGE('',*,*,#18159,.T.);
#28397=ORIENTED_EDGE('',*,*,#19441,.F.);
#28398=ORIENTED_EDGE('',*,*,#19435,.F.);
#28399=ORIENTED_EDGE('',*,*,#19441,.T.);
#28400=ORIENTED_EDGE('',*,*,#18158,.T.);
#28401=ORIENTED_EDGE('',*,*,#19442,.F.);
#28402=ORIENTED_EDGE('',*,*,#19436,.F.);
#28403=ORIENTED_EDGE('',*,*,#19442,.T.);
#28404=ORIENTED_EDGE('',*,*,#18157,.T.);
#28405=ORIENTED_EDGE('',*,*,#18163,.T.);
#28406=ORIENTED_EDGE('',*,*,#19443,.F.);
#28407=ORIENTED_EDGE('',*,*,#19437,.F.);
#28408=ORIENTED_EDGE('',*,*,#19443,.T.);
#28409=ORIENTED_EDGE('',*,*,#18162,.T.);
#28410=ORIENTED_EDGE('',*,*,#19444,.F.);
#28411=ORIENTED_EDGE('',*,*,#19438,.F.);
#28412=ORIENTED_EDGE('',*,*,#19444,.T.);
#28413=ORIENTED_EDGE('',*,*,#18161,.T.);
#28414=ORIENTED_EDGE('',*,*,#19439,.F.);
#28415=ORIENTED_EDGE('',*,*,#19433,.F.);
#28416=ORIENTED_EDGE('',*,*,#19445,.F.);
#28417=ORIENTED_EDGE('',*,*,#18089,.F.);
#28418=ORIENTED_EDGE('',*,*,#18088,.F.);
#28419=ORIENTED_EDGE('',*,*,#18085,.F.);
#28420=ORIENTED_EDGE('',*,*,#18082,.F.);
#28421=ORIENTED_EDGE('',*,*,#18079,.F.);
#28422=ORIENTED_EDGE('',*,*,#18076,.F.);
#28423=ORIENTED_EDGE('',*,*,#18073,.F.);
#28424=ORIENTED_EDGE('',*,*,#18070,.F.);
#28425=ORIENTED_EDGE('',*,*,#18067,.F.);
#28426=ORIENTED_EDGE('',*,*,#18064,.F.);
#28427=ORIENTED_EDGE('',*,*,#18061,.F.);
#28428=ORIENTED_EDGE('',*,*,#18058,.F.);
#28429=ORIENTED_EDGE('',*,*,#18055,.F.);
#28430=ORIENTED_EDGE('',*,*,#18052,.F.);
#28431=ORIENTED_EDGE('',*,*,#18049,.F.);
#28432=ORIENTED_EDGE('',*,*,#18046,.F.);
#28433=ORIENTED_EDGE('',*,*,#18043,.F.);
#28434=ORIENTED_EDGE('',*,*,#18040,.F.);
#28435=ORIENTED_EDGE('',*,*,#18037,.F.);
#28436=ORIENTED_EDGE('',*,*,#18034,.F.);
#28437=ORIENTED_EDGE('',*,*,#18031,.F.);
#28438=ORIENTED_EDGE('',*,*,#18028,.F.);
#28439=ORIENTED_EDGE('',*,*,#18025,.F.);
#28440=ORIENTED_EDGE('',*,*,#18022,.F.);
#28441=ORIENTED_EDGE('',*,*,#18019,.F.);
#28442=ORIENTED_EDGE('',*,*,#18016,.F.);
#28443=ORIENTED_EDGE('',*,*,#18013,.F.);
#28444=ORIENTED_EDGE('',*,*,#18010,.F.);
#28445=ORIENTED_EDGE('',*,*,#18007,.F.);
#28446=ORIENTED_EDGE('',*,*,#18004,.F.);
#28447=ORIENTED_EDGE('',*,*,#17997,.F.);
#28448=ORIENTED_EDGE('',*,*,#18094,.F.);
#28449=ORIENTED_EDGE('',*,*,#18095,.T.);
#28450=ORIENTED_EDGE('',*,*,#17995,.T.);
#28451=ORIENTED_EDGE('',*,*,#17992,.T.);
#28452=ORIENTED_EDGE('',*,*,#17989,.T.);
#28453=ORIENTED_EDGE('',*,*,#17986,.T.);
#28454=ORIENTED_EDGE('',*,*,#17983,.T.);
#28455=ORIENTED_EDGE('',*,*,#17980,.T.);
#28456=ORIENTED_EDGE('',*,*,#17977,.T.);
#28457=ORIENTED_EDGE('',*,*,#17974,.T.);
#28458=ORIENTED_EDGE('',*,*,#17971,.T.);
#28459=ORIENTED_EDGE('',*,*,#17968,.T.);
#28460=ORIENTED_EDGE('',*,*,#17965,.T.);
#28461=ORIENTED_EDGE('',*,*,#17962,.T.);
#28462=ORIENTED_EDGE('',*,*,#17959,.T.);
#28463=ORIENTED_EDGE('',*,*,#17956,.T.);
#28464=ORIENTED_EDGE('',*,*,#17953,.T.);
#28465=ORIENTED_EDGE('',*,*,#17950,.T.);
#28466=ORIENTED_EDGE('',*,*,#17947,.T.);
#28467=ORIENTED_EDGE('',*,*,#17944,.T.);
#28468=ORIENTED_EDGE('',*,*,#17941,.T.);
#28469=ORIENTED_EDGE('',*,*,#17938,.T.);
#28470=ORIENTED_EDGE('',*,*,#17935,.T.);
#28471=ORIENTED_EDGE('',*,*,#17932,.T.);
#28472=ORIENTED_EDGE('',*,*,#17929,.T.);
#28473=ORIENTED_EDGE('',*,*,#17926,.T.);
#28474=ORIENTED_EDGE('',*,*,#17923,.T.);
#28475=ORIENTED_EDGE('',*,*,#17920,.T.);
#28476=ORIENTED_EDGE('',*,*,#17917,.T.);
#28477=ORIENTED_EDGE('',*,*,#17914,.T.);
#28478=ORIENTED_EDGE('',*,*,#19446,.F.);
#28479=ORIENTED_EDGE('',*,*,#17910,.T.);
#28480=ORIENTED_EDGE('',*,*,#17916,.T.);
#28481=ORIENTED_EDGE('',*,*,#17919,.T.);
#28482=ORIENTED_EDGE('',*,*,#17922,.T.);
#28483=ORIENTED_EDGE('',*,*,#17925,.T.);
#28484=ORIENTED_EDGE('',*,*,#17928,.T.);
#28485=ORIENTED_EDGE('',*,*,#17931,.T.);
#28486=ORIENTED_EDGE('',*,*,#17934,.T.);
#28487=ORIENTED_EDGE('',*,*,#17937,.T.);
#28488=ORIENTED_EDGE('',*,*,#17940,.T.);
#28489=ORIENTED_EDGE('',*,*,#17943,.T.);
#28490=ORIENTED_EDGE('',*,*,#17946,.T.);
#28491=ORIENTED_EDGE('',*,*,#17949,.T.);
#28492=ORIENTED_EDGE('',*,*,#17952,.T.);
#28493=ORIENTED_EDGE('',*,*,#17955,.T.);
#28494=ORIENTED_EDGE('',*,*,#17958,.T.);
#28495=ORIENTED_EDGE('',*,*,#17961,.T.);
#28496=ORIENTED_EDGE('',*,*,#17964,.T.);
#28497=ORIENTED_EDGE('',*,*,#17967,.T.);
#28498=ORIENTED_EDGE('',*,*,#17970,.T.);
#28499=ORIENTED_EDGE('',*,*,#17973,.T.);
#28500=ORIENTED_EDGE('',*,*,#17976,.T.);
#28501=ORIENTED_EDGE('',*,*,#17979,.T.);
#28502=ORIENTED_EDGE('',*,*,#17982,.T.);
#28503=ORIENTED_EDGE('',*,*,#17985,.T.);
#28504=ORIENTED_EDGE('',*,*,#17988,.T.);
#28505=ORIENTED_EDGE('',*,*,#17991,.T.);
#28506=ORIENTED_EDGE('',*,*,#17994,.T.);
#28507=ORIENTED_EDGE('',*,*,#18096,.T.);
#28508=ORIENTED_EDGE('',*,*,#18092,.F.);
#28509=ORIENTED_EDGE('',*,*,#18000,.T.);
#28510=ORIENTED_EDGE('',*,*,#18003,.T.);
#28511=ORIENTED_EDGE('',*,*,#18006,.T.);
#28512=ORIENTED_EDGE('',*,*,#18009,.T.);
#28513=ORIENTED_EDGE('',*,*,#18012,.T.);
#28514=ORIENTED_EDGE('',*,*,#18015,.T.);
#28515=ORIENTED_EDGE('',*,*,#18018,.T.);
#28516=ORIENTED_EDGE('',*,*,#18021,.T.);
#28517=ORIENTED_EDGE('',*,*,#18024,.T.);
#28518=ORIENTED_EDGE('',*,*,#18027,.T.);
#28519=ORIENTED_EDGE('',*,*,#18030,.T.);
#28520=ORIENTED_EDGE('',*,*,#18033,.T.);
#28521=ORIENTED_EDGE('',*,*,#18036,.T.);
#28522=ORIENTED_EDGE('',*,*,#18039,.T.);
#28523=ORIENTED_EDGE('',*,*,#18042,.T.);
#28524=ORIENTED_EDGE('',*,*,#18045,.T.);
#28525=ORIENTED_EDGE('',*,*,#18048,.T.);
#28526=ORIENTED_EDGE('',*,*,#18051,.T.);
#28527=ORIENTED_EDGE('',*,*,#18054,.T.);
#28528=ORIENTED_EDGE('',*,*,#18057,.T.);
#28529=ORIENTED_EDGE('',*,*,#18060,.T.);
#28530=ORIENTED_EDGE('',*,*,#18063,.T.);
#28531=ORIENTED_EDGE('',*,*,#18066,.T.);
#28532=ORIENTED_EDGE('',*,*,#18069,.T.);
#28533=ORIENTED_EDGE('',*,*,#18072,.T.);
#28534=ORIENTED_EDGE('',*,*,#18075,.T.);
#28535=ORIENTED_EDGE('',*,*,#18078,.T.);
#28536=ORIENTED_EDGE('',*,*,#18081,.T.);
#28537=ORIENTED_EDGE('',*,*,#18084,.T.);
#28538=ORIENTED_EDGE('',*,*,#18087,.T.);
#28539=ORIENTED_EDGE('',*,*,#18090,.T.);
#28540=ORIENTED_EDGE('',*,*,#19445,.T.);
#28541=ORIENTED_EDGE('',*,*,#17913,.T.);
#28542=ORIENTED_EDGE('',*,*,#19446,.T.);
#28543=ORIENTED_EDGE('',*,*,#18477,.T.);
#28544=ORIENTED_EDGE('',*,*,#19447,.T.);
#28545=ORIENTED_EDGE('',*,*,#18328,.T.);
#28546=ORIENTED_EDGE('',*,*,#19432,.T.);
#28547=ORIENTED_EDGE('',*,*,#19429,.T.);
#28548=ORIENTED_EDGE('',*,*,#19426,.T.);
#28549=ORIENTED_EDGE('',*,*,#18476,.T.);
#28550=ORIENTED_EDGE('',*,*,#18781,.T.);
#28551=ORIENTED_EDGE('',*,*,#19448,.T.);
#28552=ORIENTED_EDGE('',*,*,#18329,.T.);
#28553=ORIENTED_EDGE('',*,*,#19447,.F.);
#28554=ORIENTED_EDGE('',*,*,#18780,.T.);
#28555=ORIENTED_EDGE('',*,*,#19026,.T.);
#28556=ORIENTED_EDGE('',*,*,#19263,.T.);
#28557=ORIENTED_EDGE('',*,*,#19422,.T.);
#28558=ORIENTED_EDGE('',*,*,#18330,.T.);
#28559=ORIENTED_EDGE('',*,*,#19448,.F.);
#28560=ORIENTED_EDGE('',*,*,#18481,.T.);
#28561=ORIENTED_EDGE('',*,*,#19449,.T.);
#28562=ORIENTED_EDGE('',*,*,#18324,.T.);
#28563=ORIENTED_EDGE('',*,*,#19424,.T.);
#28564=ORIENTED_EDGE('',*,*,#19265,.T.);
#28565=ORIENTED_EDGE('',*,*,#19028,.T.);
#28566=ORIENTED_EDGE('',*,*,#18480,.T.);
#28567=ORIENTED_EDGE('',*,*,#19450,.T.);
#28568=ORIENTED_EDGE('',*,*,#18325,.T.);
#28569=ORIENTED_EDGE('',*,*,#19449,.F.);
#28570=ORIENTED_EDGE('',*,*,#18479,.T.);
#28571=ORIENTED_EDGE('',*,*,#19425,.T.);
#28572=ORIENTED_EDGE('',*,*,#19428,.T.);
#28573=ORIENTED_EDGE('',*,*,#19431,.T.);
#28574=ORIENTED_EDGE('',*,*,#18326,.T.);
#28575=ORIENTED_EDGE('',*,*,#19450,.F.);
#28576=ORIENTED_EDGE('',*,*,#18778,.T.);
#28577=ORIENTED_EDGE('',*,*,#19451,.T.);
#28578=ORIENTED_EDGE('',*,*,#18332,.T.);
#28579=ORIENTED_EDGE('',*,*,#19421,.T.);
#28580=ORIENTED_EDGE('',*,*,#19261,.T.);
#28581=ORIENTED_EDGE('',*,*,#19024,.T.);
#28582=ORIENTED_EDGE('',*,*,#18777,.T.);
#28583=ORIENTED_EDGE('',*,*,#19452,.T.);
#28584=ORIENTED_EDGE('',*,*,#18333,.T.);
#28585=ORIENTED_EDGE('',*,*,#19451,.F.);
#28586=ORIENTED_EDGE('',*,*,#18776,.T.);
#28587=ORIENTED_EDGE('',*,*,#19023,.T.);
#28588=ORIENTED_EDGE('',*,*,#19260,.T.);
#28589=ORIENTED_EDGE('',*,*,#19420,.T.);
#28590=ORIENTED_EDGE('',*,*,#18334,.T.);
#28591=ORIENTED_EDGE('',*,*,#19452,.F.);
#28592=ORIENTED_EDGE('',*,*,#18774,.T.);
#28593=ORIENTED_EDGE('',*,*,#19453,.T.);
#28594=ORIENTED_EDGE('',*,*,#18336,.T.);
#28595=ORIENTED_EDGE('',*,*,#19419,.T.);
#28596=ORIENTED_EDGE('',*,*,#19258,.T.);
#28597=ORIENTED_EDGE('',*,*,#19021,.T.);
#28598=ORIENTED_EDGE('',*,*,#18773,.T.);
#28599=ORIENTED_EDGE('',*,*,#19454,.T.);
#28600=ORIENTED_EDGE('',*,*,#18337,.T.);
#28601=ORIENTED_EDGE('',*,*,#19453,.F.);
#28602=ORIENTED_EDGE('',*,*,#18772,.T.);
#28603=ORIENTED_EDGE('',*,*,#19020,.T.);
#28604=ORIENTED_EDGE('',*,*,#19257,.T.);
#28605=ORIENTED_EDGE('',*,*,#19418,.T.);
#28606=ORIENTED_EDGE('',*,*,#18338,.T.);
#28607=ORIENTED_EDGE('',*,*,#19454,.F.);
#28608=ORIENTED_EDGE('',*,*,#18770,.T.);
#28609=ORIENTED_EDGE('',*,*,#19455,.T.);
#28610=ORIENTED_EDGE('',*,*,#18340,.T.);
#28611=ORIENTED_EDGE('',*,*,#19417,.T.);
#28612=ORIENTED_EDGE('',*,*,#19255,.T.);
#28613=ORIENTED_EDGE('',*,*,#19018,.T.);
#28614=ORIENTED_EDGE('',*,*,#18769,.T.);
#28615=ORIENTED_EDGE('',*,*,#19456,.T.);
#28616=ORIENTED_EDGE('',*,*,#18341,.T.);
#28617=ORIENTED_EDGE('',*,*,#19455,.F.);
#28618=ORIENTED_EDGE('',*,*,#18768,.T.);
#28619=ORIENTED_EDGE('',*,*,#19017,.T.);
#28620=ORIENTED_EDGE('',*,*,#19254,.T.);
#28621=ORIENTED_EDGE('',*,*,#19416,.T.);
#28622=ORIENTED_EDGE('',*,*,#18342,.T.);
#28623=ORIENTED_EDGE('',*,*,#19456,.F.);
#28624=ORIENTED_EDGE('',*,*,#18766,.T.);
#28625=ORIENTED_EDGE('',*,*,#19457,.T.);
#28626=ORIENTED_EDGE('',*,*,#18344,.T.);
#28627=ORIENTED_EDGE('',*,*,#19415,.T.);
#28628=ORIENTED_EDGE('',*,*,#19252,.T.);
#28629=ORIENTED_EDGE('',*,*,#19015,.T.);
#28630=ORIENTED_EDGE('',*,*,#18765,.T.);
#28631=ORIENTED_EDGE('',*,*,#19458,.T.);
#28632=ORIENTED_EDGE('',*,*,#18345,.T.);
#28633=ORIENTED_EDGE('',*,*,#19457,.F.);
#28634=ORIENTED_EDGE('',*,*,#18764,.T.);
#28635=ORIENTED_EDGE('',*,*,#19014,.T.);
#28636=ORIENTED_EDGE('',*,*,#19251,.T.);
#28637=ORIENTED_EDGE('',*,*,#19414,.T.);
#28638=ORIENTED_EDGE('',*,*,#18346,.T.);
#28639=ORIENTED_EDGE('',*,*,#19458,.F.);
#28640=ORIENTED_EDGE('',*,*,#18762,.T.);
#28641=ORIENTED_EDGE('',*,*,#19459,.T.);
#28642=ORIENTED_EDGE('',*,*,#18348,.T.);
#28643=ORIENTED_EDGE('',*,*,#19413,.T.);
#28644=ORIENTED_EDGE('',*,*,#19249,.T.);
#28645=ORIENTED_EDGE('',*,*,#19012,.T.);
#28646=ORIENTED_EDGE('',*,*,#18761,.T.);
#28647=ORIENTED_EDGE('',*,*,#19460,.T.);
#28648=ORIENTED_EDGE('',*,*,#18349,.T.);
#28649=ORIENTED_EDGE('',*,*,#19459,.F.);
#28650=ORIENTED_EDGE('',*,*,#18760,.T.);
#28651=ORIENTED_EDGE('',*,*,#19011,.T.);
#28652=ORIENTED_EDGE('',*,*,#19248,.T.);
#28653=ORIENTED_EDGE('',*,*,#19412,.T.);
#28654=ORIENTED_EDGE('',*,*,#18350,.T.);
#28655=ORIENTED_EDGE('',*,*,#19460,.F.);
#28656=ORIENTED_EDGE('',*,*,#18758,.T.);
#28657=ORIENTED_EDGE('',*,*,#18156,.T.);
#28658=ORIENTED_EDGE('',*,*,#18352,.T.);
#28659=ORIENTED_EDGE('',*,*,#19411,.T.);
#28660=ORIENTED_EDGE('',*,*,#19246,.T.);
#28661=ORIENTED_EDGE('',*,*,#19009,.T.);
#28662=ORIENTED_EDGE('',*,*,#18757,.T.);
#28663=ORIENTED_EDGE('',*,*,#19008,.T.);
#28664=ORIENTED_EDGE('',*,*,#19245,.T.);
#28665=ORIENTED_EDGE('',*,*,#19410,.T.);
#28666=ORIENTED_EDGE('',*,*,#18353,.T.);
#28667=ORIENTED_EDGE('',*,*,#18154,.F.);
#28668=ORIENTED_EDGE('',*,*,#18755,.T.);
#28669=ORIENTED_EDGE('',*,*,#18152,.T.);
#28670=ORIENTED_EDGE('',*,*,#18355,.T.);
#28671=ORIENTED_EDGE('',*,*,#19409,.T.);
#28672=ORIENTED_EDGE('',*,*,#19243,.T.);
#28673=ORIENTED_EDGE('',*,*,#19006,.T.);
#28674=ORIENTED_EDGE('',*,*,#18754,.T.);
#28675=ORIENTED_EDGE('',*,*,#19005,.T.);
#28676=ORIENTED_EDGE('',*,*,#19242,.T.);
#28677=ORIENTED_EDGE('',*,*,#19408,.T.);
#28678=ORIENTED_EDGE('',*,*,#18356,.T.);
#28679=ORIENTED_EDGE('',*,*,#18150,.F.);
#28680=ORIENTED_EDGE('',*,*,#18752,.T.);
#28681=ORIENTED_EDGE('',*,*,#18148,.T.);
#28682=ORIENTED_EDGE('',*,*,#18358,.T.);
#28683=ORIENTED_EDGE('',*,*,#19407,.T.);
#28684=ORIENTED_EDGE('',*,*,#19240,.T.);
#28685=ORIENTED_EDGE('',*,*,#19003,.T.);
#28686=ORIENTED_EDGE('',*,*,#18751,.T.);
#28687=ORIENTED_EDGE('',*,*,#19002,.T.);
#28688=ORIENTED_EDGE('',*,*,#19239,.T.);
#28689=ORIENTED_EDGE('',*,*,#19406,.T.);
#28690=ORIENTED_EDGE('',*,*,#18359,.T.);
#28691=ORIENTED_EDGE('',*,*,#18146,.F.);
#28692=ORIENTED_EDGE('',*,*,#18749,.T.);
#28693=ORIENTED_EDGE('',*,*,#18144,.T.);
#28694=ORIENTED_EDGE('',*,*,#18361,.T.);
#28695=ORIENTED_EDGE('',*,*,#19405,.T.);
#28696=ORIENTED_EDGE('',*,*,#19237,.T.);
#28697=ORIENTED_EDGE('',*,*,#19000,.T.);
#28698=ORIENTED_EDGE('',*,*,#18748,.T.);
#28699=ORIENTED_EDGE('',*,*,#18999,.T.);
#28700=ORIENTED_EDGE('',*,*,#19236,.T.);
#28701=ORIENTED_EDGE('',*,*,#19404,.T.);
#28702=ORIENTED_EDGE('',*,*,#18362,.T.);
#28703=ORIENTED_EDGE('',*,*,#18142,.F.);
#28704=ORIENTED_EDGE('',*,*,#18746,.T.);
#28705=ORIENTED_EDGE('',*,*,#18140,.T.);
#28706=ORIENTED_EDGE('',*,*,#18364,.T.);
#28707=ORIENTED_EDGE('',*,*,#19403,.T.);
#28708=ORIENTED_EDGE('',*,*,#19234,.T.);
#28709=ORIENTED_EDGE('',*,*,#18997,.T.);
#28710=ORIENTED_EDGE('',*,*,#18745,.T.);
#28711=ORIENTED_EDGE('',*,*,#18996,.T.);
#28712=ORIENTED_EDGE('',*,*,#19233,.T.);
#28713=ORIENTED_EDGE('',*,*,#19402,.T.);
#28714=ORIENTED_EDGE('',*,*,#18365,.T.);
#28715=ORIENTED_EDGE('',*,*,#18138,.F.);
#28716=ORIENTED_EDGE('',*,*,#18743,.T.);
#28717=ORIENTED_EDGE('',*,*,#18136,.T.);
#28718=ORIENTED_EDGE('',*,*,#18367,.T.);
#28719=ORIENTED_EDGE('',*,*,#19401,.T.);
#28720=ORIENTED_EDGE('',*,*,#19231,.T.);
#28721=ORIENTED_EDGE('',*,*,#18994,.T.);
#28722=ORIENTED_EDGE('',*,*,#18742,.T.);
#28723=ORIENTED_EDGE('',*,*,#18993,.T.);
#28724=ORIENTED_EDGE('',*,*,#19230,.T.);
#28725=ORIENTED_EDGE('',*,*,#19400,.T.);
#28726=ORIENTED_EDGE('',*,*,#18368,.T.);
#28727=ORIENTED_EDGE('',*,*,#18134,.F.);
#28728=ORIENTED_EDGE('',*,*,#18740,.T.);
#28729=ORIENTED_EDGE('',*,*,#18132,.T.);
#28730=ORIENTED_EDGE('',*,*,#18370,.T.);
#28731=ORIENTED_EDGE('',*,*,#19399,.T.);
#28732=ORIENTED_EDGE('',*,*,#19228,.T.);
#28733=ORIENTED_EDGE('',*,*,#18991,.T.);
#28734=ORIENTED_EDGE('',*,*,#18739,.T.);
#28735=ORIENTED_EDGE('',*,*,#18990,.T.);
#28736=ORIENTED_EDGE('',*,*,#19227,.T.);
#28737=ORIENTED_EDGE('',*,*,#19398,.T.);
#28738=ORIENTED_EDGE('',*,*,#18371,.T.);
#28739=ORIENTED_EDGE('',*,*,#18130,.F.);
#28740=ORIENTED_EDGE('',*,*,#18737,.T.);
#28741=ORIENTED_EDGE('',*,*,#18128,.T.);
#28742=ORIENTED_EDGE('',*,*,#18373,.T.);
#28743=ORIENTED_EDGE('',*,*,#19397,.T.);
#28744=ORIENTED_EDGE('',*,*,#19225,.T.);
#28745=ORIENTED_EDGE('',*,*,#18988,.T.);
#28746=ORIENTED_EDGE('',*,*,#18736,.T.);
#28747=ORIENTED_EDGE('',*,*,#18987,.T.);
#28748=ORIENTED_EDGE('',*,*,#19224,.T.);
#28749=ORIENTED_EDGE('',*,*,#19396,.T.);
#28750=ORIENTED_EDGE('',*,*,#18374,.T.);
#28751=ORIENTED_EDGE('',*,*,#18126,.F.);
#28752=ORIENTED_EDGE('',*,*,#18734,.T.);
#28753=ORIENTED_EDGE('',*,*,#18124,.T.);
#28754=ORIENTED_EDGE('',*,*,#18376,.T.);
#28755=ORIENTED_EDGE('',*,*,#19395,.T.);
#28756=ORIENTED_EDGE('',*,*,#19222,.T.);
#28757=ORIENTED_EDGE('',*,*,#18985,.T.);
#28758=ORIENTED_EDGE('',*,*,#18733,.T.);
#28759=ORIENTED_EDGE('',*,*,#18795,.T.);
#28760=ORIENTED_EDGE('',*,*,#19032,.T.);
#28761=ORIENTED_EDGE('',*,*,#19268,.T.);
#28762=ORIENTED_EDGE('',*,*,#18377,.T.);
#28763=ORIENTED_EDGE('',*,*,#18122,.F.);
#28764=ORIENTED_EDGE('',*,*,#18485,.T.);
#28765=ORIENTED_EDGE('',*,*,#19461,.T.);
#28766=ORIENTED_EDGE('',*,*,#18320,.T.);
#28767=ORIENTED_EDGE('',*,*,#19394,.T.);
#28768=ORIENTED_EDGE('',*,*,#19220,.T.);
#28769=ORIENTED_EDGE('',*,*,#18983,.T.);
#28770=ORIENTED_EDGE('',*,*,#18484,.T.);
#28771=ORIENTED_EDGE('',*,*,#19462,.T.);
#28772=ORIENTED_EDGE('',*,*,#18321,.T.);
#28773=ORIENTED_EDGE('',*,*,#19461,.F.);
#28774=ORIENTED_EDGE('',*,*,#18483,.T.);
#28775=ORIENTED_EDGE('',*,*,#19027,.T.);
#28776=ORIENTED_EDGE('',*,*,#19264,.T.);
#28777=ORIENTED_EDGE('',*,*,#19423,.T.);
#28778=ORIENTED_EDGE('',*,*,#18322,.T.);
#28779=ORIENTED_EDGE('',*,*,#19462,.F.);
#28780=ORIENTED_EDGE('',*,*,#18489,.T.);
#28781=ORIENTED_EDGE('',*,*,#19463,.T.);
#28782=ORIENTED_EDGE('',*,*,#18316,.T.);
#28783=ORIENTED_EDGE('',*,*,#19392,.T.);
#28784=ORIENTED_EDGE('',*,*,#19217,.T.);
#28785=ORIENTED_EDGE('',*,*,#18980,.T.);
#28786=ORIENTED_EDGE('',*,*,#18488,.T.);
#28787=ORIENTED_EDGE('',*,*,#19464,.T.);
#28788=ORIENTED_EDGE('',*,*,#18317,.T.);
#28789=ORIENTED_EDGE('',*,*,#19463,.F.);
#28790=ORIENTED_EDGE('',*,*,#18487,.T.);
#28791=ORIENTED_EDGE('',*,*,#18982,.T.);
#28792=ORIENTED_EDGE('',*,*,#19219,.T.);
#28793=ORIENTED_EDGE('',*,*,#19393,.T.);
#28794=ORIENTED_EDGE('',*,*,#18318,.T.);
#28795=ORIENTED_EDGE('',*,*,#19464,.F.);
#28796=ORIENTED_EDGE('',*,*,#18493,.T.);
#28797=ORIENTED_EDGE('',*,*,#19465,.T.);
#28798=ORIENTED_EDGE('',*,*,#18312,.T.);
#28799=ORIENTED_EDGE('',*,*,#19390,.T.);
#28800=ORIENTED_EDGE('',*,*,#19214,.T.);
#28801=ORIENTED_EDGE('',*,*,#18977,.T.);
#28802=ORIENTED_EDGE('',*,*,#18492,.T.);
#28803=ORIENTED_EDGE('',*,*,#19466,.T.);
#28804=ORIENTED_EDGE('',*,*,#18313,.T.);
#28805=ORIENTED_EDGE('',*,*,#19465,.F.);
#28806=ORIENTED_EDGE('',*,*,#18491,.T.);
#28807=ORIENTED_EDGE('',*,*,#18979,.T.);
#28808=ORIENTED_EDGE('',*,*,#19216,.T.);
#28809=ORIENTED_EDGE('',*,*,#19391,.T.);
#28810=ORIENTED_EDGE('',*,*,#18314,.T.);
#28811=ORIENTED_EDGE('',*,*,#19466,.F.);
#28812=ORIENTED_EDGE('',*,*,#18497,.T.);
#28813=ORIENTED_EDGE('',*,*,#19467,.T.);
#28814=ORIENTED_EDGE('',*,*,#18308,.T.);
#28815=ORIENTED_EDGE('',*,*,#19388,.T.);
#28816=ORIENTED_EDGE('',*,*,#19211,.T.);
#28817=ORIENTED_EDGE('',*,*,#18974,.T.);
#28818=ORIENTED_EDGE('',*,*,#18496,.T.);
#28819=ORIENTED_EDGE('',*,*,#19468,.T.);
#28820=ORIENTED_EDGE('',*,*,#18309,.T.);
#28821=ORIENTED_EDGE('',*,*,#19467,.F.);
#28822=ORIENTED_EDGE('',*,*,#18495,.T.);
#28823=ORIENTED_EDGE('',*,*,#18976,.T.);
#28824=ORIENTED_EDGE('',*,*,#19213,.T.);
#28825=ORIENTED_EDGE('',*,*,#19389,.T.);
#28826=ORIENTED_EDGE('',*,*,#18310,.T.);
#28827=ORIENTED_EDGE('',*,*,#19468,.F.);
#28828=ORIENTED_EDGE('',*,*,#18501,.T.);
#28829=ORIENTED_EDGE('',*,*,#19469,.T.);
#28830=ORIENTED_EDGE('',*,*,#18304,.T.);
#28831=ORIENTED_EDGE('',*,*,#19386,.T.);
#28832=ORIENTED_EDGE('',*,*,#19208,.T.);
#28833=ORIENTED_EDGE('',*,*,#18971,.T.);
#28834=ORIENTED_EDGE('',*,*,#18500,.T.);
#28835=ORIENTED_EDGE('',*,*,#19470,.T.);
#28836=ORIENTED_EDGE('',*,*,#18305,.T.);
#28837=ORIENTED_EDGE('',*,*,#19469,.F.);
#28838=ORIENTED_EDGE('',*,*,#18499,.T.);
#28839=ORIENTED_EDGE('',*,*,#18973,.T.);
#28840=ORIENTED_EDGE('',*,*,#19210,.T.);
#28841=ORIENTED_EDGE('',*,*,#19387,.T.);
#28842=ORIENTED_EDGE('',*,*,#18306,.T.);
#28843=ORIENTED_EDGE('',*,*,#19470,.F.);
#28844=ORIENTED_EDGE('',*,*,#18505,.T.);
#28845=ORIENTED_EDGE('',*,*,#19471,.T.);
#28846=ORIENTED_EDGE('',*,*,#18300,.T.);
#28847=ORIENTED_EDGE('',*,*,#19384,.T.);
#28848=ORIENTED_EDGE('',*,*,#19205,.T.);
#28849=ORIENTED_EDGE('',*,*,#18968,.T.);
#28850=ORIENTED_EDGE('',*,*,#18504,.T.);
#28851=ORIENTED_EDGE('',*,*,#19472,.T.);
#28852=ORIENTED_EDGE('',*,*,#18301,.T.);
#28853=ORIENTED_EDGE('',*,*,#19471,.F.);
#28854=ORIENTED_EDGE('',*,*,#18503,.T.);
#28855=ORIENTED_EDGE('',*,*,#18970,.T.);
#28856=ORIENTED_EDGE('',*,*,#19207,.T.);
#28857=ORIENTED_EDGE('',*,*,#19385,.T.);
#28858=ORIENTED_EDGE('',*,*,#18302,.T.);
#28859=ORIENTED_EDGE('',*,*,#19472,.F.);
#28860=ORIENTED_EDGE('',*,*,#18509,.T.);
#28861=ORIENTED_EDGE('',*,*,#19473,.T.);
#28862=ORIENTED_EDGE('',*,*,#18296,.T.);
#28863=ORIENTED_EDGE('',*,*,#19382,.T.);
#28864=ORIENTED_EDGE('',*,*,#19202,.T.);
#28865=ORIENTED_EDGE('',*,*,#18965,.T.);
#28866=ORIENTED_EDGE('',*,*,#18508,.T.);
#28867=ORIENTED_EDGE('',*,*,#19474,.T.);
#28868=ORIENTED_EDGE('',*,*,#18297,.T.);
#28869=ORIENTED_EDGE('',*,*,#19473,.F.);
#28870=ORIENTED_EDGE('',*,*,#18507,.T.);
#28871=ORIENTED_EDGE('',*,*,#18967,.T.);
#28872=ORIENTED_EDGE('',*,*,#19204,.T.);
#28873=ORIENTED_EDGE('',*,*,#19383,.T.);
#28874=ORIENTED_EDGE('',*,*,#18298,.T.);
#28875=ORIENTED_EDGE('',*,*,#19474,.F.);
#28876=ORIENTED_EDGE('',*,*,#18513,.T.);
#28877=ORIENTED_EDGE('',*,*,#19475,.T.);
#28878=ORIENTED_EDGE('',*,*,#18292,.T.);
#28879=ORIENTED_EDGE('',*,*,#19380,.T.);
#28880=ORIENTED_EDGE('',*,*,#19199,.T.);
#28881=ORIENTED_EDGE('',*,*,#18962,.T.);
#28882=ORIENTED_EDGE('',*,*,#18512,.T.);
#28883=ORIENTED_EDGE('',*,*,#19476,.T.);
#28884=ORIENTED_EDGE('',*,*,#18293,.T.);
#28885=ORIENTED_EDGE('',*,*,#19475,.F.);
#28886=ORIENTED_EDGE('',*,*,#18511,.T.);
#28887=ORIENTED_EDGE('',*,*,#18964,.T.);
#28888=ORIENTED_EDGE('',*,*,#19201,.T.);
#28889=ORIENTED_EDGE('',*,*,#19381,.T.);
#28890=ORIENTED_EDGE('',*,*,#18294,.T.);
#28891=ORIENTED_EDGE('',*,*,#19476,.F.);
#28892=ORIENTED_EDGE('',*,*,#18517,.T.);
#28893=ORIENTED_EDGE('',*,*,#19477,.T.);
#28894=ORIENTED_EDGE('',*,*,#18288,.T.);
#28895=ORIENTED_EDGE('',*,*,#19378,.T.);
#28896=ORIENTED_EDGE('',*,*,#19196,.T.);
#28897=ORIENTED_EDGE('',*,*,#18959,.T.);
#28898=ORIENTED_EDGE('',*,*,#18516,.T.);
#28899=ORIENTED_EDGE('',*,*,#19478,.T.);
#28900=ORIENTED_EDGE('',*,*,#18289,.T.);
#28901=ORIENTED_EDGE('',*,*,#19477,.F.);
#28902=ORIENTED_EDGE('',*,*,#18515,.T.);
#28903=ORIENTED_EDGE('',*,*,#18961,.T.);
#28904=ORIENTED_EDGE('',*,*,#19198,.T.);
#28905=ORIENTED_EDGE('',*,*,#19379,.T.);
#28906=ORIENTED_EDGE('',*,*,#18290,.T.);
#28907=ORIENTED_EDGE('',*,*,#19478,.F.);
#28908=ORIENTED_EDGE('',*,*,#18521,.T.);
#28909=ORIENTED_EDGE('',*,*,#19479,.T.);
#28910=ORIENTED_EDGE('',*,*,#18284,.T.);
#28911=ORIENTED_EDGE('',*,*,#19376,.T.);
#28912=ORIENTED_EDGE('',*,*,#19193,.T.);
#28913=ORIENTED_EDGE('',*,*,#18956,.T.);
#28914=ORIENTED_EDGE('',*,*,#18520,.T.);
#28915=ORIENTED_EDGE('',*,*,#19480,.T.);
#28916=ORIENTED_EDGE('',*,*,#18285,.T.);
#28917=ORIENTED_EDGE('',*,*,#19479,.F.);
#28918=ORIENTED_EDGE('',*,*,#18519,.T.);
#28919=ORIENTED_EDGE('',*,*,#18958,.T.);
#28920=ORIENTED_EDGE('',*,*,#19195,.T.);
#28921=ORIENTED_EDGE('',*,*,#19377,.T.);
#28922=ORIENTED_EDGE('',*,*,#18286,.T.);
#28923=ORIENTED_EDGE('',*,*,#19480,.F.);
#28924=ORIENTED_EDGE('',*,*,#18525,.T.);
#28925=ORIENTED_EDGE('',*,*,#19481,.T.);
#28926=ORIENTED_EDGE('',*,*,#18280,.T.);
#28927=ORIENTED_EDGE('',*,*,#19374,.T.);
#28928=ORIENTED_EDGE('',*,*,#19190,.T.);
#28929=ORIENTED_EDGE('',*,*,#18953,.T.);
#28930=ORIENTED_EDGE('',*,*,#18524,.T.);
#28931=ORIENTED_EDGE('',*,*,#19482,.T.);
#28932=ORIENTED_EDGE('',*,*,#18281,.T.);
#28933=ORIENTED_EDGE('',*,*,#19481,.F.);
#28934=ORIENTED_EDGE('',*,*,#18523,.T.);
#28935=ORIENTED_EDGE('',*,*,#18955,.T.);
#28936=ORIENTED_EDGE('',*,*,#19192,.T.);
#28937=ORIENTED_EDGE('',*,*,#19375,.T.);
#28938=ORIENTED_EDGE('',*,*,#18282,.T.);
#28939=ORIENTED_EDGE('',*,*,#19482,.F.);
#28940=ORIENTED_EDGE('',*,*,#18529,.T.);
#28941=ORIENTED_EDGE('',*,*,#19483,.T.);
#28942=ORIENTED_EDGE('',*,*,#18276,.T.);
#28943=ORIENTED_EDGE('',*,*,#19372,.T.);
#28944=ORIENTED_EDGE('',*,*,#19187,.T.);
#28945=ORIENTED_EDGE('',*,*,#18950,.T.);
#28946=ORIENTED_EDGE('',*,*,#18528,.T.);
#28947=ORIENTED_EDGE('',*,*,#19484,.T.);
#28948=ORIENTED_EDGE('',*,*,#18277,.T.);
#28949=ORIENTED_EDGE('',*,*,#19483,.F.);
#28950=ORIENTED_EDGE('',*,*,#18527,.T.);
#28951=ORIENTED_EDGE('',*,*,#18952,.T.);
#28952=ORIENTED_EDGE('',*,*,#19189,.T.);
#28953=ORIENTED_EDGE('',*,*,#19373,.T.);
#28954=ORIENTED_EDGE('',*,*,#18278,.T.);
#28955=ORIENTED_EDGE('',*,*,#19484,.F.);
#28956=ORIENTED_EDGE('',*,*,#18533,.T.);
#28957=ORIENTED_EDGE('',*,*,#19485,.T.);
#28958=ORIENTED_EDGE('',*,*,#18272,.T.);
#28959=ORIENTED_EDGE('',*,*,#19370,.T.);
#28960=ORIENTED_EDGE('',*,*,#19184,.T.);
#28961=ORIENTED_EDGE('',*,*,#18947,.T.);
#28962=ORIENTED_EDGE('',*,*,#18532,.T.);
#28963=ORIENTED_EDGE('',*,*,#19486,.T.);
#28964=ORIENTED_EDGE('',*,*,#18273,.T.);
#28965=ORIENTED_EDGE('',*,*,#19485,.F.);
#28966=ORIENTED_EDGE('',*,*,#18531,.T.);
#28967=ORIENTED_EDGE('',*,*,#18949,.T.);
#28968=ORIENTED_EDGE('',*,*,#19186,.T.);
#28969=ORIENTED_EDGE('',*,*,#19371,.T.);
#28970=ORIENTED_EDGE('',*,*,#18274,.T.);
#28971=ORIENTED_EDGE('',*,*,#19486,.F.);
#28972=ORIENTED_EDGE('',*,*,#18537,.T.);
#28973=ORIENTED_EDGE('',*,*,#19487,.T.);
#28974=ORIENTED_EDGE('',*,*,#18268,.T.);
#28975=ORIENTED_EDGE('',*,*,#19368,.T.);
#28976=ORIENTED_EDGE('',*,*,#19181,.T.);
#28977=ORIENTED_EDGE('',*,*,#18944,.T.);
#28978=ORIENTED_EDGE('',*,*,#18536,.T.);
#28979=ORIENTED_EDGE('',*,*,#19488,.T.);
#28980=ORIENTED_EDGE('',*,*,#18269,.T.);
#28981=ORIENTED_EDGE('',*,*,#19487,.F.);
#28982=ORIENTED_EDGE('',*,*,#18535,.T.);
#28983=ORIENTED_EDGE('',*,*,#18946,.T.);
#28984=ORIENTED_EDGE('',*,*,#19183,.T.);
#28985=ORIENTED_EDGE('',*,*,#19369,.T.);
#28986=ORIENTED_EDGE('',*,*,#18270,.T.);
#28987=ORIENTED_EDGE('',*,*,#19488,.F.);
#28988=ORIENTED_EDGE('',*,*,#18541,.T.);
#28989=ORIENTED_EDGE('',*,*,#19489,.T.);
#28990=ORIENTED_EDGE('',*,*,#18264,.T.);
#28991=ORIENTED_EDGE('',*,*,#19366,.T.);
#28992=ORIENTED_EDGE('',*,*,#19178,.T.);
#28993=ORIENTED_EDGE('',*,*,#18941,.T.);
#28994=ORIENTED_EDGE('',*,*,#18540,.T.);
#28995=ORIENTED_EDGE('',*,*,#19490,.T.);
#28996=ORIENTED_EDGE('',*,*,#18265,.T.);
#28997=ORIENTED_EDGE('',*,*,#19489,.F.);
#28998=ORIENTED_EDGE('',*,*,#18539,.T.);
#28999=ORIENTED_EDGE('',*,*,#18943,.T.);
#29000=ORIENTED_EDGE('',*,*,#19180,.T.);
#29001=ORIENTED_EDGE('',*,*,#19367,.T.);
#29002=ORIENTED_EDGE('',*,*,#18266,.T.);
#29003=ORIENTED_EDGE('',*,*,#19490,.F.);
#29004=ORIENTED_EDGE('',*,*,#18545,.T.);
#29005=ORIENTED_EDGE('',*,*,#19491,.T.);
#29006=ORIENTED_EDGE('',*,*,#18260,.T.);
#29007=ORIENTED_EDGE('',*,*,#19364,.T.);
#29008=ORIENTED_EDGE('',*,*,#19175,.T.);
#29009=ORIENTED_EDGE('',*,*,#18938,.T.);
#29010=ORIENTED_EDGE('',*,*,#18544,.T.);
#29011=ORIENTED_EDGE('',*,*,#19492,.T.);
#29012=ORIENTED_EDGE('',*,*,#18261,.T.);
#29013=ORIENTED_EDGE('',*,*,#19491,.F.);
#29014=ORIENTED_EDGE('',*,*,#18543,.T.);
#29015=ORIENTED_EDGE('',*,*,#18940,.T.);
#29016=ORIENTED_EDGE('',*,*,#19177,.T.);
#29017=ORIENTED_EDGE('',*,*,#19365,.T.);
#29018=ORIENTED_EDGE('',*,*,#18262,.T.);
#29019=ORIENTED_EDGE('',*,*,#19492,.F.);
#29020=ORIENTED_EDGE('',*,*,#18549,.T.);
#29021=ORIENTED_EDGE('',*,*,#19493,.T.);
#29022=ORIENTED_EDGE('',*,*,#18256,.T.);
#29023=ORIENTED_EDGE('',*,*,#19362,.T.);
#29024=ORIENTED_EDGE('',*,*,#19172,.T.);
#29025=ORIENTED_EDGE('',*,*,#18935,.T.);
#29026=ORIENTED_EDGE('',*,*,#18548,.T.);
#29027=ORIENTED_EDGE('',*,*,#19494,.T.);
#29028=ORIENTED_EDGE('',*,*,#18257,.T.);
#29029=ORIENTED_EDGE('',*,*,#19493,.F.);
#29030=ORIENTED_EDGE('',*,*,#18547,.T.);
#29031=ORIENTED_EDGE('',*,*,#18937,.T.);
#29032=ORIENTED_EDGE('',*,*,#19174,.T.);
#29033=ORIENTED_EDGE('',*,*,#19363,.T.);
#29034=ORIENTED_EDGE('',*,*,#18258,.T.);
#29035=ORIENTED_EDGE('',*,*,#19494,.F.);
#29036=ORIENTED_EDGE('',*,*,#18553,.T.);
#29037=ORIENTED_EDGE('',*,*,#19495,.T.);
#29038=ORIENTED_EDGE('',*,*,#18252,.T.);
#29039=ORIENTED_EDGE('',*,*,#19360,.T.);
#29040=ORIENTED_EDGE('',*,*,#19169,.T.);
#29041=ORIENTED_EDGE('',*,*,#18932,.T.);
#29042=ORIENTED_EDGE('',*,*,#18552,.T.);
#29043=ORIENTED_EDGE('',*,*,#19496,.T.);
#29044=ORIENTED_EDGE('',*,*,#18253,.T.);
#29045=ORIENTED_EDGE('',*,*,#19495,.F.);
#29046=ORIENTED_EDGE('',*,*,#18551,.T.);
#29047=ORIENTED_EDGE('',*,*,#18934,.T.);
#29048=ORIENTED_EDGE('',*,*,#19171,.T.);
#29049=ORIENTED_EDGE('',*,*,#19361,.T.);
#29050=ORIENTED_EDGE('',*,*,#18254,.T.);
#29051=ORIENTED_EDGE('',*,*,#19496,.F.);
#29052=ORIENTED_EDGE('',*,*,#18557,.T.);
#29053=ORIENTED_EDGE('',*,*,#19497,.T.);
#29054=ORIENTED_EDGE('',*,*,#18248,.T.);
#29055=ORIENTED_EDGE('',*,*,#19358,.T.);
#29056=ORIENTED_EDGE('',*,*,#19166,.T.);
#29057=ORIENTED_EDGE('',*,*,#18929,.T.);
#29058=ORIENTED_EDGE('',*,*,#18556,.T.);
#29059=ORIENTED_EDGE('',*,*,#19498,.T.);
#29060=ORIENTED_EDGE('',*,*,#18249,.T.);
#29061=ORIENTED_EDGE('',*,*,#19497,.F.);
#29062=ORIENTED_EDGE('',*,*,#18555,.T.);
#29063=ORIENTED_EDGE('',*,*,#18931,.T.);
#29064=ORIENTED_EDGE('',*,*,#19168,.T.);
#29065=ORIENTED_EDGE('',*,*,#19359,.T.);
#29066=ORIENTED_EDGE('',*,*,#18250,.T.);
#29067=ORIENTED_EDGE('',*,*,#19498,.F.);
#29068=ORIENTED_EDGE('',*,*,#18561,.T.);
#29069=ORIENTED_EDGE('',*,*,#19499,.T.);
#29070=ORIENTED_EDGE('',*,*,#18244,.T.);
#29071=ORIENTED_EDGE('',*,*,#19356,.T.);
#29072=ORIENTED_EDGE('',*,*,#19163,.T.);
#29073=ORIENTED_EDGE('',*,*,#18926,.T.);
#29074=ORIENTED_EDGE('',*,*,#18560,.T.);
#29075=ORIENTED_EDGE('',*,*,#19500,.T.);
#29076=ORIENTED_EDGE('',*,*,#18245,.T.);
#29077=ORIENTED_EDGE('',*,*,#19499,.F.);
#29078=ORIENTED_EDGE('',*,*,#18559,.T.);
#29079=ORIENTED_EDGE('',*,*,#18928,.T.);
#29080=ORIENTED_EDGE('',*,*,#19165,.T.);
#29081=ORIENTED_EDGE('',*,*,#19357,.T.);
#29082=ORIENTED_EDGE('',*,*,#18246,.T.);
#29083=ORIENTED_EDGE('',*,*,#19500,.F.);
#29084=ORIENTED_EDGE('',*,*,#18565,.T.);
#29085=ORIENTED_EDGE('',*,*,#19501,.T.);
#29086=ORIENTED_EDGE('',*,*,#18240,.T.);
#29087=ORIENTED_EDGE('',*,*,#19354,.T.);
#29088=ORIENTED_EDGE('',*,*,#19160,.T.);
#29089=ORIENTED_EDGE('',*,*,#18923,.T.);
#29090=ORIENTED_EDGE('',*,*,#18564,.T.);
#29091=ORIENTED_EDGE('',*,*,#19502,.T.);
#29092=ORIENTED_EDGE('',*,*,#18241,.T.);
#29093=ORIENTED_EDGE('',*,*,#19501,.F.);
#29094=ORIENTED_EDGE('',*,*,#18563,.T.);
#29095=ORIENTED_EDGE('',*,*,#18925,.T.);
#29096=ORIENTED_EDGE('',*,*,#19162,.T.);
#29097=ORIENTED_EDGE('',*,*,#19355,.T.);
#29098=ORIENTED_EDGE('',*,*,#18242,.T.);
#29099=ORIENTED_EDGE('',*,*,#19502,.F.);
#29100=ORIENTED_EDGE('',*,*,#18569,.T.);
#29101=ORIENTED_EDGE('',*,*,#19503,.T.);
#29102=ORIENTED_EDGE('',*,*,#18236,.T.);
#29103=ORIENTED_EDGE('',*,*,#19352,.T.);
#29104=ORIENTED_EDGE('',*,*,#19157,.T.);
#29105=ORIENTED_EDGE('',*,*,#18920,.T.);
#29106=ORIENTED_EDGE('',*,*,#18568,.T.);
#29107=ORIENTED_EDGE('',*,*,#19504,.T.);
#29108=ORIENTED_EDGE('',*,*,#18237,.T.);
#29109=ORIENTED_EDGE('',*,*,#19503,.F.);
#29110=ORIENTED_EDGE('',*,*,#18567,.T.);
#29111=ORIENTED_EDGE('',*,*,#18922,.T.);
#29112=ORIENTED_EDGE('',*,*,#19159,.T.);
#29113=ORIENTED_EDGE('',*,*,#19353,.T.);
#29114=ORIENTED_EDGE('',*,*,#18238,.T.);
#29115=ORIENTED_EDGE('',*,*,#19504,.F.);
#29116=ORIENTED_EDGE('',*,*,#18573,.T.);
#29117=ORIENTED_EDGE('',*,*,#19505,.T.);
#29118=ORIENTED_EDGE('',*,*,#18232,.T.);
#29119=ORIENTED_EDGE('',*,*,#19350,.T.);
#29120=ORIENTED_EDGE('',*,*,#19154,.T.);
#29121=ORIENTED_EDGE('',*,*,#18917,.T.);
#29122=ORIENTED_EDGE('',*,*,#18572,.T.);
#29123=ORIENTED_EDGE('',*,*,#19506,.T.);
#29124=ORIENTED_EDGE('',*,*,#18233,.T.);
#29125=ORIENTED_EDGE('',*,*,#19505,.F.);
#29126=ORIENTED_EDGE('',*,*,#18571,.T.);
#29127=ORIENTED_EDGE('',*,*,#18919,.T.);
#29128=ORIENTED_EDGE('',*,*,#19156,.T.);
#29129=ORIENTED_EDGE('',*,*,#19351,.T.);
#29130=ORIENTED_EDGE('',*,*,#18234,.T.);
#29131=ORIENTED_EDGE('',*,*,#19506,.F.);
#29132=ORIENTED_EDGE('',*,*,#18577,.T.);
#29133=ORIENTED_EDGE('',*,*,#19507,.T.);
#29134=ORIENTED_EDGE('',*,*,#18228,.T.);
#29135=ORIENTED_EDGE('',*,*,#19348,.T.);
#29136=ORIENTED_EDGE('',*,*,#19151,.T.);
#29137=ORIENTED_EDGE('',*,*,#18914,.T.);
#29138=ORIENTED_EDGE('',*,*,#18576,.T.);
#29139=ORIENTED_EDGE('',*,*,#19508,.T.);
#29140=ORIENTED_EDGE('',*,*,#18229,.T.);
#29141=ORIENTED_EDGE('',*,*,#19507,.F.);
#29142=ORIENTED_EDGE('',*,*,#18575,.T.);
#29143=ORIENTED_EDGE('',*,*,#18916,.T.);
#29144=ORIENTED_EDGE('',*,*,#19153,.T.);
#29145=ORIENTED_EDGE('',*,*,#19349,.T.);
#29146=ORIENTED_EDGE('',*,*,#18230,.T.);
#29147=ORIENTED_EDGE('',*,*,#19508,.F.);
#29148=ORIENTED_EDGE('',*,*,#18581,.T.);
#29149=ORIENTED_EDGE('',*,*,#19509,.T.);
#29150=ORIENTED_EDGE('',*,*,#18224,.T.);
#29151=ORIENTED_EDGE('',*,*,#19346,.T.);
#29152=ORIENTED_EDGE('',*,*,#19148,.T.);
#29153=ORIENTED_EDGE('',*,*,#18911,.T.);
#29154=ORIENTED_EDGE('',*,*,#18580,.T.);
#29155=ORIENTED_EDGE('',*,*,#19510,.T.);
#29156=ORIENTED_EDGE('',*,*,#18225,.T.);
#29157=ORIENTED_EDGE('',*,*,#19509,.F.);
#29158=ORIENTED_EDGE('',*,*,#18579,.T.);
#29159=ORIENTED_EDGE('',*,*,#18913,.T.);
#29160=ORIENTED_EDGE('',*,*,#19150,.T.);
#29161=ORIENTED_EDGE('',*,*,#19347,.T.);
#29162=ORIENTED_EDGE('',*,*,#18226,.T.);
#29163=ORIENTED_EDGE('',*,*,#19510,.F.);
#29164=ORIENTED_EDGE('',*,*,#18585,.T.);
#29165=ORIENTED_EDGE('',*,*,#19511,.T.);
#29166=ORIENTED_EDGE('',*,*,#18220,.T.);
#29167=ORIENTED_EDGE('',*,*,#19344,.T.);
#29168=ORIENTED_EDGE('',*,*,#19145,.T.);
#29169=ORIENTED_EDGE('',*,*,#18908,.T.);
#29170=ORIENTED_EDGE('',*,*,#18584,.T.);
#29171=ORIENTED_EDGE('',*,*,#19512,.T.);
#29172=ORIENTED_EDGE('',*,*,#18221,.T.);
#29173=ORIENTED_EDGE('',*,*,#19511,.F.);
#29174=ORIENTED_EDGE('',*,*,#18583,.T.);
#29175=ORIENTED_EDGE('',*,*,#18910,.T.);
#29176=ORIENTED_EDGE('',*,*,#19147,.T.);
#29177=ORIENTED_EDGE('',*,*,#19345,.T.);
#29178=ORIENTED_EDGE('',*,*,#18222,.T.);
#29179=ORIENTED_EDGE('',*,*,#19512,.F.);
#29180=ORIENTED_EDGE('',*,*,#18589,.T.);
#29181=ORIENTED_EDGE('',*,*,#19513,.T.);
#29182=ORIENTED_EDGE('',*,*,#18216,.T.);
#29183=ORIENTED_EDGE('',*,*,#19342,.T.);
#29184=ORIENTED_EDGE('',*,*,#19142,.T.);
#29185=ORIENTED_EDGE('',*,*,#18905,.T.);
#29186=ORIENTED_EDGE('',*,*,#18588,.T.);
#29187=ORIENTED_EDGE('',*,*,#19514,.T.);
#29188=ORIENTED_EDGE('',*,*,#18217,.T.);
#29189=ORIENTED_EDGE('',*,*,#19513,.F.);
#29190=ORIENTED_EDGE('',*,*,#18587,.T.);
#29191=ORIENTED_EDGE('',*,*,#18907,.T.);
#29192=ORIENTED_EDGE('',*,*,#19144,.T.);
#29193=ORIENTED_EDGE('',*,*,#19343,.T.);
#29194=ORIENTED_EDGE('',*,*,#18218,.T.);
#29195=ORIENTED_EDGE('',*,*,#19514,.F.);
#29196=ORIENTED_EDGE('',*,*,#18593,.T.);
#29197=ORIENTED_EDGE('',*,*,#19515,.T.);
#29198=ORIENTED_EDGE('',*,*,#18212,.T.);
#29199=ORIENTED_EDGE('',*,*,#19340,.T.);
#29200=ORIENTED_EDGE('',*,*,#19139,.T.);
#29201=ORIENTED_EDGE('',*,*,#18902,.T.);
#29202=ORIENTED_EDGE('',*,*,#18592,.T.);
#29203=ORIENTED_EDGE('',*,*,#19516,.T.);
#29204=ORIENTED_EDGE('',*,*,#18213,.T.);
#29205=ORIENTED_EDGE('',*,*,#19515,.F.);
#29206=ORIENTED_EDGE('',*,*,#18591,.T.);
#29207=ORIENTED_EDGE('',*,*,#18904,.T.);
#29208=ORIENTED_EDGE('',*,*,#19141,.T.);
#29209=ORIENTED_EDGE('',*,*,#19341,.T.);
#29210=ORIENTED_EDGE('',*,*,#18214,.T.);
#29211=ORIENTED_EDGE('',*,*,#19516,.F.);
#29212=ORIENTED_EDGE('',*,*,#18597,.T.);
#29213=ORIENTED_EDGE('',*,*,#19517,.T.);
#29214=ORIENTED_EDGE('',*,*,#18208,.T.);
#29215=ORIENTED_EDGE('',*,*,#19338,.T.);
#29216=ORIENTED_EDGE('',*,*,#19136,.T.);
#29217=ORIENTED_EDGE('',*,*,#18899,.T.);
#29218=ORIENTED_EDGE('',*,*,#18596,.T.);
#29219=ORIENTED_EDGE('',*,*,#19518,.T.);
#29220=ORIENTED_EDGE('',*,*,#18209,.T.);
#29221=ORIENTED_EDGE('',*,*,#19517,.F.);
#29222=ORIENTED_EDGE('',*,*,#18595,.T.);
#29223=ORIENTED_EDGE('',*,*,#18901,.T.);
#29224=ORIENTED_EDGE('',*,*,#19138,.T.);
#29225=ORIENTED_EDGE('',*,*,#19339,.T.);
#29226=ORIENTED_EDGE('',*,*,#18210,.T.);
#29227=ORIENTED_EDGE('',*,*,#19518,.F.);
#29228=ORIENTED_EDGE('',*,*,#18601,.T.);
#29229=ORIENTED_EDGE('',*,*,#19519,.T.);
#29230=ORIENTED_EDGE('',*,*,#18204,.T.);
#29231=ORIENTED_EDGE('',*,*,#19336,.T.);
#29232=ORIENTED_EDGE('',*,*,#19133,.T.);
#29233=ORIENTED_EDGE('',*,*,#18896,.T.);
#29234=ORIENTED_EDGE('',*,*,#18600,.T.);
#29235=ORIENTED_EDGE('',*,*,#19520,.T.);
#29236=ORIENTED_EDGE('',*,*,#18205,.T.);
#29237=ORIENTED_EDGE('',*,*,#19519,.F.);
#29238=ORIENTED_EDGE('',*,*,#18599,.T.);
#29239=ORIENTED_EDGE('',*,*,#18898,.T.);
#29240=ORIENTED_EDGE('',*,*,#19135,.T.);
#29241=ORIENTED_EDGE('',*,*,#19337,.T.);
#29242=ORIENTED_EDGE('',*,*,#18206,.T.);
#29243=ORIENTED_EDGE('',*,*,#19520,.F.);
#29244=ORIENTED_EDGE('',*,*,#18605,.T.);
#29245=ORIENTED_EDGE('',*,*,#19521,.T.);
#29246=ORIENTED_EDGE('',*,*,#18200,.T.);
#29247=ORIENTED_EDGE('',*,*,#19334,.T.);
#29248=ORIENTED_EDGE('',*,*,#19130,.T.);
#29249=ORIENTED_EDGE('',*,*,#18893,.T.);
#29250=ORIENTED_EDGE('',*,*,#18604,.T.);
#29251=ORIENTED_EDGE('',*,*,#19522,.T.);
#29252=ORIENTED_EDGE('',*,*,#18201,.T.);
#29253=ORIENTED_EDGE('',*,*,#19521,.F.);
#29254=ORIENTED_EDGE('',*,*,#18603,.T.);
#29255=ORIENTED_EDGE('',*,*,#18895,.T.);
#29256=ORIENTED_EDGE('',*,*,#19132,.T.);
#29257=ORIENTED_EDGE('',*,*,#19335,.T.);
#29258=ORIENTED_EDGE('',*,*,#18202,.T.);
#29259=ORIENTED_EDGE('',*,*,#19522,.F.);
#29260=ORIENTED_EDGE('',*,*,#18609,.T.);
#29261=ORIENTED_EDGE('',*,*,#19523,.T.);
#29262=ORIENTED_EDGE('',*,*,#18196,.T.);
#29263=ORIENTED_EDGE('',*,*,#19332,.T.);
#29264=ORIENTED_EDGE('',*,*,#19127,.T.);
#29265=ORIENTED_EDGE('',*,*,#18890,.T.);
#29266=ORIENTED_EDGE('',*,*,#18608,.T.);
#29267=ORIENTED_EDGE('',*,*,#19524,.T.);
#29268=ORIENTED_EDGE('',*,*,#18197,.T.);
#29269=ORIENTED_EDGE('',*,*,#19523,.F.);
#29270=ORIENTED_EDGE('',*,*,#18607,.T.);
#29271=ORIENTED_EDGE('',*,*,#18892,.T.);
#29272=ORIENTED_EDGE('',*,*,#19129,.T.);
#29273=ORIENTED_EDGE('',*,*,#19333,.T.);
#29274=ORIENTED_EDGE('',*,*,#18198,.T.);
#29275=ORIENTED_EDGE('',*,*,#19524,.F.);
#29276=ORIENTED_EDGE('',*,*,#18613,.T.);
#29277=ORIENTED_EDGE('',*,*,#19525,.T.);
#29278=ORIENTED_EDGE('',*,*,#18192,.T.);
#29279=ORIENTED_EDGE('',*,*,#19330,.T.);
#29280=ORIENTED_EDGE('',*,*,#19124,.T.);
#29281=ORIENTED_EDGE('',*,*,#18887,.T.);
#29282=ORIENTED_EDGE('',*,*,#18612,.T.);
#29283=ORIENTED_EDGE('',*,*,#19526,.T.);
#29284=ORIENTED_EDGE('',*,*,#18193,.T.);
#29285=ORIENTED_EDGE('',*,*,#19525,.F.);
#29286=ORIENTED_EDGE('',*,*,#18611,.T.);
#29287=ORIENTED_EDGE('',*,*,#18889,.T.);
#29288=ORIENTED_EDGE('',*,*,#19126,.T.);
#29289=ORIENTED_EDGE('',*,*,#19331,.T.);
#29290=ORIENTED_EDGE('',*,*,#18194,.T.);
#29291=ORIENTED_EDGE('',*,*,#19526,.F.);
#29292=ORIENTED_EDGE('',*,*,#18617,.T.);
#29293=ORIENTED_EDGE('',*,*,#19527,.T.);
#29294=ORIENTED_EDGE('',*,*,#18188,.T.);
#29295=ORIENTED_EDGE('',*,*,#19328,.T.);
#29296=ORIENTED_EDGE('',*,*,#19121,.T.);
#29297=ORIENTED_EDGE('',*,*,#18884,.T.);
#29298=ORIENTED_EDGE('',*,*,#18616,.T.);
#29299=ORIENTED_EDGE('',*,*,#19528,.T.);
#29300=ORIENTED_EDGE('',*,*,#18189,.T.);
#29301=ORIENTED_EDGE('',*,*,#19527,.F.);
#29302=ORIENTED_EDGE('',*,*,#18615,.T.);
#29303=ORIENTED_EDGE('',*,*,#18886,.T.);
#29304=ORIENTED_EDGE('',*,*,#19123,.T.);
#29305=ORIENTED_EDGE('',*,*,#19329,.T.);
#29306=ORIENTED_EDGE('',*,*,#18190,.T.);
#29307=ORIENTED_EDGE('',*,*,#19528,.F.);
#29308=ORIENTED_EDGE('',*,*,#18621,.T.);
#29309=ORIENTED_EDGE('',*,*,#19529,.T.);
#29310=ORIENTED_EDGE('',*,*,#18184,.T.);
#29311=ORIENTED_EDGE('',*,*,#19326,.T.);
#29312=ORIENTED_EDGE('',*,*,#19118,.T.);
#29313=ORIENTED_EDGE('',*,*,#18881,.T.);
#29314=ORIENTED_EDGE('',*,*,#18620,.T.);
#29315=ORIENTED_EDGE('',*,*,#19530,.T.);
#29316=ORIENTED_EDGE('',*,*,#18185,.T.);
#29317=ORIENTED_EDGE('',*,*,#19529,.F.);
#29318=ORIENTED_EDGE('',*,*,#18619,.T.);
#29319=ORIENTED_EDGE('',*,*,#18883,.T.);
#29320=ORIENTED_EDGE('',*,*,#19120,.T.);
#29321=ORIENTED_EDGE('',*,*,#19327,.T.);
#29322=ORIENTED_EDGE('',*,*,#18186,.T.);
#29323=ORIENTED_EDGE('',*,*,#19530,.F.);
#29324=ORIENTED_EDGE('',*,*,#18625,.T.);
#29325=ORIENTED_EDGE('',*,*,#19531,.T.);
#29326=ORIENTED_EDGE('',*,*,#18180,.T.);
#29327=ORIENTED_EDGE('',*,*,#19324,.T.);
#29328=ORIENTED_EDGE('',*,*,#19115,.T.);
#29329=ORIENTED_EDGE('',*,*,#18878,.T.);
#29330=ORIENTED_EDGE('',*,*,#18624,.T.);
#29331=ORIENTED_EDGE('',*,*,#19532,.T.);
#29332=ORIENTED_EDGE('',*,*,#18181,.T.);
#29333=ORIENTED_EDGE('',*,*,#19531,.F.);
#29334=ORIENTED_EDGE('',*,*,#18623,.T.);
#29335=ORIENTED_EDGE('',*,*,#18880,.T.);
#29336=ORIENTED_EDGE('',*,*,#19117,.T.);
#29337=ORIENTED_EDGE('',*,*,#19325,.T.);
#29338=ORIENTED_EDGE('',*,*,#18182,.T.);
#29339=ORIENTED_EDGE('',*,*,#19532,.F.);
#29340=ORIENTED_EDGE('',*,*,#18629,.T.);
#29341=ORIENTED_EDGE('',*,*,#19533,.T.);
#29342=ORIENTED_EDGE('',*,*,#18176,.T.);
#29343=ORIENTED_EDGE('',*,*,#19322,.T.);
#29344=ORIENTED_EDGE('',*,*,#19112,.T.);
#29345=ORIENTED_EDGE('',*,*,#18875,.T.);
#29346=ORIENTED_EDGE('',*,*,#18628,.T.);
#29347=ORIENTED_EDGE('',*,*,#19534,.T.);
#29348=ORIENTED_EDGE('',*,*,#18177,.T.);
#29349=ORIENTED_EDGE('',*,*,#19533,.F.);
#29350=ORIENTED_EDGE('',*,*,#18627,.T.);
#29351=ORIENTED_EDGE('',*,*,#18877,.T.);
#29352=ORIENTED_EDGE('',*,*,#19114,.T.);
#29353=ORIENTED_EDGE('',*,*,#19323,.T.);
#29354=ORIENTED_EDGE('',*,*,#18178,.T.);
#29355=ORIENTED_EDGE('',*,*,#19534,.F.);
#29356=ORIENTED_EDGE('',*,*,#18633,.T.);
#29357=ORIENTED_EDGE('',*,*,#19535,.T.);
#29358=ORIENTED_EDGE('',*,*,#18172,.T.);
#29359=ORIENTED_EDGE('',*,*,#19320,.T.);
#29360=ORIENTED_EDGE('',*,*,#19109,.T.);
#29361=ORIENTED_EDGE('',*,*,#18872,.T.);
#29362=ORIENTED_EDGE('',*,*,#18632,.T.);
#29363=ORIENTED_EDGE('',*,*,#19536,.T.);
#29364=ORIENTED_EDGE('',*,*,#18173,.T.);
#29365=ORIENTED_EDGE('',*,*,#19535,.F.);
#29366=ORIENTED_EDGE('',*,*,#18631,.T.);
#29367=ORIENTED_EDGE('',*,*,#18874,.T.);
#29368=ORIENTED_EDGE('',*,*,#19111,.T.);
#29369=ORIENTED_EDGE('',*,*,#19321,.T.);
#29370=ORIENTED_EDGE('',*,*,#18174,.T.);
#29371=ORIENTED_EDGE('',*,*,#19536,.F.);
#29372=ORIENTED_EDGE('',*,*,#18637,.T.);
#29373=ORIENTED_EDGE('',*,*,#19537,.T.);
#29374=ORIENTED_EDGE('',*,*,#18473,.T.);
#29375=ORIENTED_EDGE('',*,*,#19318,.T.);
#29376=ORIENTED_EDGE('',*,*,#19106,.T.);
#29377=ORIENTED_EDGE('',*,*,#18869,.T.);
#29378=ORIENTED_EDGE('',*,*,#18636,.T.);
#29379=ORIENTED_EDGE('',*,*,#19538,.T.);
#29380=ORIENTED_EDGE('',*,*,#18169,.T.);
#29381=ORIENTED_EDGE('',*,*,#18474,.T.);
#29382=ORIENTED_EDGE('',*,*,#19537,.F.);
#29383=ORIENTED_EDGE('',*,*,#18635,.T.);
#29384=ORIENTED_EDGE('',*,*,#18871,.T.);
#29385=ORIENTED_EDGE('',*,*,#19108,.T.);
#29386=ORIENTED_EDGE('',*,*,#19319,.T.);
#29387=ORIENTED_EDGE('',*,*,#18170,.T.);
#29388=ORIENTED_EDGE('',*,*,#19538,.F.);
#29389=ORIENTED_EDGE('',*,*,#18641,.T.);
#29390=ORIENTED_EDGE('',*,*,#19539,.T.);
#29391=ORIENTED_EDGE('',*,*,#18469,.T.);
#29392=ORIENTED_EDGE('',*,*,#19316,.T.);
#29393=ORIENTED_EDGE('',*,*,#19103,.T.);
#29394=ORIENTED_EDGE('',*,*,#18866,.T.);
#29395=ORIENTED_EDGE('',*,*,#18640,.T.);
#29396=ORIENTED_EDGE('',*,*,#19540,.T.);
#29397=ORIENTED_EDGE('',*,*,#18470,.T.);
#29398=ORIENTED_EDGE('',*,*,#19539,.F.);
#29399=ORIENTED_EDGE('',*,*,#18639,.T.);
#29400=ORIENTED_EDGE('',*,*,#18868,.T.);
#29401=ORIENTED_EDGE('',*,*,#19105,.T.);
#29402=ORIENTED_EDGE('',*,*,#19317,.T.);
#29403=ORIENTED_EDGE('',*,*,#18471,.T.);
#29404=ORIENTED_EDGE('',*,*,#19540,.F.);
#29405=ORIENTED_EDGE('',*,*,#18645,.T.);
#29406=ORIENTED_EDGE('',*,*,#19541,.T.);
#29407=ORIENTED_EDGE('',*,*,#18465,.T.);
#29408=ORIENTED_EDGE('',*,*,#19314,.T.);
#29409=ORIENTED_EDGE('',*,*,#19100,.T.);
#29410=ORIENTED_EDGE('',*,*,#18863,.T.);
#29411=ORIENTED_EDGE('',*,*,#18644,.T.);
#29412=ORIENTED_EDGE('',*,*,#19542,.T.);
#29413=ORIENTED_EDGE('',*,*,#18466,.T.);
#29414=ORIENTED_EDGE('',*,*,#19541,.F.);
#29415=ORIENTED_EDGE('',*,*,#18643,.T.);
#29416=ORIENTED_EDGE('',*,*,#18865,.T.);
#29417=ORIENTED_EDGE('',*,*,#19102,.T.);
#29418=ORIENTED_EDGE('',*,*,#19315,.T.);
#29419=ORIENTED_EDGE('',*,*,#18467,.T.);
#29420=ORIENTED_EDGE('',*,*,#19542,.F.);
#29421=ORIENTED_EDGE('',*,*,#18649,.T.);
#29422=ORIENTED_EDGE('',*,*,#19543,.T.);
#29423=ORIENTED_EDGE('',*,*,#18461,.T.);
#29424=ORIENTED_EDGE('',*,*,#19312,.T.);
#29425=ORIENTED_EDGE('',*,*,#19097,.T.);
#29426=ORIENTED_EDGE('',*,*,#18860,.T.);
#29427=ORIENTED_EDGE('',*,*,#18648,.T.);
#29428=ORIENTED_EDGE('',*,*,#19544,.T.);
#29429=ORIENTED_EDGE('',*,*,#18462,.T.);
#29430=ORIENTED_EDGE('',*,*,#19543,.F.);
#29431=ORIENTED_EDGE('',*,*,#18647,.T.);
#29432=ORIENTED_EDGE('',*,*,#18862,.T.);
#29433=ORIENTED_EDGE('',*,*,#19099,.T.);
#29434=ORIENTED_EDGE('',*,*,#19313,.T.);
#29435=ORIENTED_EDGE('',*,*,#18463,.T.);
#29436=ORIENTED_EDGE('',*,*,#19544,.F.);
#29437=ORIENTED_EDGE('',*,*,#18653,.T.);
#29438=ORIENTED_EDGE('',*,*,#19545,.T.);
#29439=ORIENTED_EDGE('',*,*,#18457,.T.);
#29440=ORIENTED_EDGE('',*,*,#19310,.T.);
#29441=ORIENTED_EDGE('',*,*,#19094,.T.);
#29442=ORIENTED_EDGE('',*,*,#18857,.T.);
#29443=ORIENTED_EDGE('',*,*,#18652,.T.);
#29444=ORIENTED_EDGE('',*,*,#19546,.T.);
#29445=ORIENTED_EDGE('',*,*,#18458,.T.);
#29446=ORIENTED_EDGE('',*,*,#19545,.F.);
#29447=ORIENTED_EDGE('',*,*,#18651,.T.);
#29448=ORIENTED_EDGE('',*,*,#18859,.T.);
#29449=ORIENTED_EDGE('',*,*,#19096,.T.);
#29450=ORIENTED_EDGE('',*,*,#19311,.T.);
#29451=ORIENTED_EDGE('',*,*,#18459,.T.);
#29452=ORIENTED_EDGE('',*,*,#19546,.F.);
#29453=ORIENTED_EDGE('',*,*,#18657,.T.);
#29454=ORIENTED_EDGE('',*,*,#19547,.T.);
#29455=ORIENTED_EDGE('',*,*,#18453,.T.);
#29456=ORIENTED_EDGE('',*,*,#19308,.T.);
#29457=ORIENTED_EDGE('',*,*,#19091,.T.);
#29458=ORIENTED_EDGE('',*,*,#18854,.T.);
#29459=ORIENTED_EDGE('',*,*,#18656,.T.);
#29460=ORIENTED_EDGE('',*,*,#19548,.T.);
#29461=ORIENTED_EDGE('',*,*,#18454,.T.);
#29462=ORIENTED_EDGE('',*,*,#19547,.F.);
#29463=ORIENTED_EDGE('',*,*,#18655,.T.);
#29464=ORIENTED_EDGE('',*,*,#18856,.T.);
#29465=ORIENTED_EDGE('',*,*,#19093,.T.);
#29466=ORIENTED_EDGE('',*,*,#19309,.T.);
#29467=ORIENTED_EDGE('',*,*,#18455,.T.);
#29468=ORIENTED_EDGE('',*,*,#19548,.F.);
#29469=ORIENTED_EDGE('',*,*,#18661,.T.);
#29470=ORIENTED_EDGE('',*,*,#19549,.T.);
#29471=ORIENTED_EDGE('',*,*,#18449,.T.);
#29472=ORIENTED_EDGE('',*,*,#19306,.T.);
#29473=ORIENTED_EDGE('',*,*,#19088,.T.);
#29474=ORIENTED_EDGE('',*,*,#18851,.T.);
#29475=ORIENTED_EDGE('',*,*,#18660,.T.);
#29476=ORIENTED_EDGE('',*,*,#19550,.T.);
#29477=ORIENTED_EDGE('',*,*,#18450,.T.);
#29478=ORIENTED_EDGE('',*,*,#19549,.F.);
#29479=ORIENTED_EDGE('',*,*,#18659,.T.);
#29480=ORIENTED_EDGE('',*,*,#18853,.T.);
#29481=ORIENTED_EDGE('',*,*,#19090,.T.);
#29482=ORIENTED_EDGE('',*,*,#19307,.T.);
#29483=ORIENTED_EDGE('',*,*,#18451,.T.);
#29484=ORIENTED_EDGE('',*,*,#19550,.F.);
#29485=ORIENTED_EDGE('',*,*,#18665,.T.);
#29486=ORIENTED_EDGE('',*,*,#19551,.T.);
#29487=ORIENTED_EDGE('',*,*,#18445,.T.);
#29488=ORIENTED_EDGE('',*,*,#19304,.T.);
#29489=ORIENTED_EDGE('',*,*,#19085,.T.);
#29490=ORIENTED_EDGE('',*,*,#18848,.T.);
#29491=ORIENTED_EDGE('',*,*,#18664,.T.);
#29492=ORIENTED_EDGE('',*,*,#19552,.T.);
#29493=ORIENTED_EDGE('',*,*,#18446,.T.);
#29494=ORIENTED_EDGE('',*,*,#19551,.F.);
#29495=ORIENTED_EDGE('',*,*,#18663,.T.);
#29496=ORIENTED_EDGE('',*,*,#18850,.T.);
#29497=ORIENTED_EDGE('',*,*,#19087,.T.);
#29498=ORIENTED_EDGE('',*,*,#19305,.T.);
#29499=ORIENTED_EDGE('',*,*,#18447,.T.);
#29500=ORIENTED_EDGE('',*,*,#19552,.F.);
#29501=ORIENTED_EDGE('',*,*,#18669,.T.);
#29502=ORIENTED_EDGE('',*,*,#19553,.T.);
#29503=ORIENTED_EDGE('',*,*,#18441,.T.);
#29504=ORIENTED_EDGE('',*,*,#19302,.T.);
#29505=ORIENTED_EDGE('',*,*,#19082,.T.);
#29506=ORIENTED_EDGE('',*,*,#18845,.T.);
#29507=ORIENTED_EDGE('',*,*,#18668,.T.);
#29508=ORIENTED_EDGE('',*,*,#19554,.T.);
#29509=ORIENTED_EDGE('',*,*,#18442,.T.);
#29510=ORIENTED_EDGE('',*,*,#19553,.F.);
#29511=ORIENTED_EDGE('',*,*,#18667,.T.);
#29512=ORIENTED_EDGE('',*,*,#18847,.T.);
#29513=ORIENTED_EDGE('',*,*,#19084,.T.);
#29514=ORIENTED_EDGE('',*,*,#19303,.T.);
#29515=ORIENTED_EDGE('',*,*,#18443,.T.);
#29516=ORIENTED_EDGE('',*,*,#19554,.F.);
#29517=ORIENTED_EDGE('',*,*,#18673,.T.);
#29518=ORIENTED_EDGE('',*,*,#19555,.T.);
#29519=ORIENTED_EDGE('',*,*,#18437,.T.);
#29520=ORIENTED_EDGE('',*,*,#19300,.T.);
#29521=ORIENTED_EDGE('',*,*,#19079,.T.);
#29522=ORIENTED_EDGE('',*,*,#18842,.T.);
#29523=ORIENTED_EDGE('',*,*,#18672,.T.);
#29524=ORIENTED_EDGE('',*,*,#19556,.T.);
#29525=ORIENTED_EDGE('',*,*,#18438,.T.);
#29526=ORIENTED_EDGE('',*,*,#19555,.F.);
#29527=ORIENTED_EDGE('',*,*,#18671,.T.);
#29528=ORIENTED_EDGE('',*,*,#18844,.T.);
#29529=ORIENTED_EDGE('',*,*,#19081,.T.);
#29530=ORIENTED_EDGE('',*,*,#19301,.T.);
#29531=ORIENTED_EDGE('',*,*,#18439,.T.);
#29532=ORIENTED_EDGE('',*,*,#19556,.F.);
#29533=ORIENTED_EDGE('',*,*,#18677,.T.);
#29534=ORIENTED_EDGE('',*,*,#19557,.T.);
#29535=ORIENTED_EDGE('',*,*,#18433,.T.);
#29536=ORIENTED_EDGE('',*,*,#19298,.T.);
#29537=ORIENTED_EDGE('',*,*,#19076,.T.);
#29538=ORIENTED_EDGE('',*,*,#18839,.T.);
#29539=ORIENTED_EDGE('',*,*,#18676,.T.);
#29540=ORIENTED_EDGE('',*,*,#19558,.T.);
#29541=ORIENTED_EDGE('',*,*,#18434,.T.);
#29542=ORIENTED_EDGE('',*,*,#19557,.F.);
#29543=ORIENTED_EDGE('',*,*,#18675,.T.);
#29544=ORIENTED_EDGE('',*,*,#18841,.T.);
#29545=ORIENTED_EDGE('',*,*,#19078,.T.);
#29546=ORIENTED_EDGE('',*,*,#19299,.T.);
#29547=ORIENTED_EDGE('',*,*,#18435,.T.);
#29548=ORIENTED_EDGE('',*,*,#19558,.F.);
#29549=ORIENTED_EDGE('',*,*,#18681,.T.);
#29550=ORIENTED_EDGE('',*,*,#19559,.T.);
#29551=ORIENTED_EDGE('',*,*,#18429,.T.);
#29552=ORIENTED_EDGE('',*,*,#19296,.T.);
#29553=ORIENTED_EDGE('',*,*,#19073,.T.);
#29554=ORIENTED_EDGE('',*,*,#18836,.T.);
#29555=ORIENTED_EDGE('',*,*,#18680,.T.);
#29556=ORIENTED_EDGE('',*,*,#19560,.T.);
#29557=ORIENTED_EDGE('',*,*,#18430,.T.);
#29558=ORIENTED_EDGE('',*,*,#19559,.F.);
#29559=ORIENTED_EDGE('',*,*,#18679,.T.);
#29560=ORIENTED_EDGE('',*,*,#18838,.T.);
#29561=ORIENTED_EDGE('',*,*,#19075,.T.);
#29562=ORIENTED_EDGE('',*,*,#19297,.T.);
#29563=ORIENTED_EDGE('',*,*,#18431,.T.);
#29564=ORIENTED_EDGE('',*,*,#19560,.F.);
#29565=ORIENTED_EDGE('',*,*,#18685,.T.);
#29566=ORIENTED_EDGE('',*,*,#19561,.T.);
#29567=ORIENTED_EDGE('',*,*,#18425,.T.);
#29568=ORIENTED_EDGE('',*,*,#19294,.T.);
#29569=ORIENTED_EDGE('',*,*,#19070,.T.);
#29570=ORIENTED_EDGE('',*,*,#18833,.T.);
#29571=ORIENTED_EDGE('',*,*,#18684,.T.);
#29572=ORIENTED_EDGE('',*,*,#19562,.T.);
#29573=ORIENTED_EDGE('',*,*,#18426,.T.);
#29574=ORIENTED_EDGE('',*,*,#19561,.F.);
#29575=ORIENTED_EDGE('',*,*,#18683,.T.);
#29576=ORIENTED_EDGE('',*,*,#18835,.T.);
#29577=ORIENTED_EDGE('',*,*,#19072,.T.);
#29578=ORIENTED_EDGE('',*,*,#19295,.T.);
#29579=ORIENTED_EDGE('',*,*,#18427,.T.);
#29580=ORIENTED_EDGE('',*,*,#19562,.F.);
#29581=ORIENTED_EDGE('',*,*,#18689,.T.);
#29582=ORIENTED_EDGE('',*,*,#19563,.T.);
#29583=ORIENTED_EDGE('',*,*,#18421,.T.);
#29584=ORIENTED_EDGE('',*,*,#19292,.T.);
#29585=ORIENTED_EDGE('',*,*,#19067,.T.);
#29586=ORIENTED_EDGE('',*,*,#18830,.T.);
#29587=ORIENTED_EDGE('',*,*,#18688,.T.);
#29588=ORIENTED_EDGE('',*,*,#19564,.T.);
#29589=ORIENTED_EDGE('',*,*,#18422,.T.);
#29590=ORIENTED_EDGE('',*,*,#19563,.F.);
#29591=ORIENTED_EDGE('',*,*,#18687,.T.);
#29592=ORIENTED_EDGE('',*,*,#18832,.T.);
#29593=ORIENTED_EDGE('',*,*,#19069,.T.);
#29594=ORIENTED_EDGE('',*,*,#19293,.T.);
#29595=ORIENTED_EDGE('',*,*,#18423,.T.);
#29596=ORIENTED_EDGE('',*,*,#19564,.F.);
#29597=ORIENTED_EDGE('',*,*,#18693,.T.);
#29598=ORIENTED_EDGE('',*,*,#19565,.T.);
#29599=ORIENTED_EDGE('',*,*,#18417,.T.);
#29600=ORIENTED_EDGE('',*,*,#19290,.T.);
#29601=ORIENTED_EDGE('',*,*,#19064,.T.);
#29602=ORIENTED_EDGE('',*,*,#18827,.T.);
#29603=ORIENTED_EDGE('',*,*,#18692,.T.);
#29604=ORIENTED_EDGE('',*,*,#19566,.T.);
#29605=ORIENTED_EDGE('',*,*,#18418,.T.);
#29606=ORIENTED_EDGE('',*,*,#19565,.F.);
#29607=ORIENTED_EDGE('',*,*,#18691,.T.);
#29608=ORIENTED_EDGE('',*,*,#18829,.T.);
#29609=ORIENTED_EDGE('',*,*,#19066,.T.);
#29610=ORIENTED_EDGE('',*,*,#19291,.T.);
#29611=ORIENTED_EDGE('',*,*,#18419,.T.);
#29612=ORIENTED_EDGE('',*,*,#19566,.F.);
#29613=ORIENTED_EDGE('',*,*,#18697,.T.);
#29614=ORIENTED_EDGE('',*,*,#19567,.T.);
#29615=ORIENTED_EDGE('',*,*,#18413,.T.);
#29616=ORIENTED_EDGE('',*,*,#19288,.T.);
#29617=ORIENTED_EDGE('',*,*,#19061,.T.);
#29618=ORIENTED_EDGE('',*,*,#18824,.T.);
#29619=ORIENTED_EDGE('',*,*,#18696,.T.);
#29620=ORIENTED_EDGE('',*,*,#19568,.T.);
#29621=ORIENTED_EDGE('',*,*,#18414,.T.);
#29622=ORIENTED_EDGE('',*,*,#19567,.F.);
#29623=ORIENTED_EDGE('',*,*,#18695,.T.);
#29624=ORIENTED_EDGE('',*,*,#18826,.T.);
#29625=ORIENTED_EDGE('',*,*,#19063,.T.);
#29626=ORIENTED_EDGE('',*,*,#19289,.T.);
#29627=ORIENTED_EDGE('',*,*,#18415,.T.);
#29628=ORIENTED_EDGE('',*,*,#19568,.F.);
#29629=ORIENTED_EDGE('',*,*,#18701,.T.);
#29630=ORIENTED_EDGE('',*,*,#19569,.T.);
#29631=ORIENTED_EDGE('',*,*,#18409,.T.);
#29632=ORIENTED_EDGE('',*,*,#19286,.T.);
#29633=ORIENTED_EDGE('',*,*,#19058,.T.);
#29634=ORIENTED_EDGE('',*,*,#18821,.T.);
#29635=ORIENTED_EDGE('',*,*,#18700,.T.);
#29636=ORIENTED_EDGE('',*,*,#19570,.T.);
#29637=ORIENTED_EDGE('',*,*,#18410,.T.);
#29638=ORIENTED_EDGE('',*,*,#19569,.F.);
#29639=ORIENTED_EDGE('',*,*,#18699,.T.);
#29640=ORIENTED_EDGE('',*,*,#18823,.T.);
#29641=ORIENTED_EDGE('',*,*,#19060,.T.);
#29642=ORIENTED_EDGE('',*,*,#19287,.T.);
#29643=ORIENTED_EDGE('',*,*,#18411,.T.);
#29644=ORIENTED_EDGE('',*,*,#19570,.F.);
#29645=ORIENTED_EDGE('',*,*,#18705,.T.);
#29646=ORIENTED_EDGE('',*,*,#19571,.T.);
#29647=ORIENTED_EDGE('',*,*,#18405,.T.);
#29648=ORIENTED_EDGE('',*,*,#19284,.T.);
#29649=ORIENTED_EDGE('',*,*,#19055,.T.);
#29650=ORIENTED_EDGE('',*,*,#18818,.T.);
#29651=ORIENTED_EDGE('',*,*,#18704,.T.);
#29652=ORIENTED_EDGE('',*,*,#19572,.T.);
#29653=ORIENTED_EDGE('',*,*,#18406,.T.);
#29654=ORIENTED_EDGE('',*,*,#19571,.F.);
#29655=ORIENTED_EDGE('',*,*,#18703,.T.);
#29656=ORIENTED_EDGE('',*,*,#18820,.T.);
#29657=ORIENTED_EDGE('',*,*,#19057,.T.);
#29658=ORIENTED_EDGE('',*,*,#19285,.T.);
#29659=ORIENTED_EDGE('',*,*,#18407,.T.);
#29660=ORIENTED_EDGE('',*,*,#19572,.F.);
#29661=ORIENTED_EDGE('',*,*,#18709,.T.);
#29662=ORIENTED_EDGE('',*,*,#19573,.T.);
#29663=ORIENTED_EDGE('',*,*,#18401,.T.);
#29664=ORIENTED_EDGE('',*,*,#19282,.T.);
#29665=ORIENTED_EDGE('',*,*,#19052,.T.);
#29666=ORIENTED_EDGE('',*,*,#18815,.T.);
#29667=ORIENTED_EDGE('',*,*,#18708,.T.);
#29668=ORIENTED_EDGE('',*,*,#19574,.T.);
#29669=ORIENTED_EDGE('',*,*,#18402,.T.);
#29670=ORIENTED_EDGE('',*,*,#19573,.F.);
#29671=ORIENTED_EDGE('',*,*,#18707,.T.);
#29672=ORIENTED_EDGE('',*,*,#18817,.T.);
#29673=ORIENTED_EDGE('',*,*,#19054,.T.);
#29674=ORIENTED_EDGE('',*,*,#19283,.T.);
#29675=ORIENTED_EDGE('',*,*,#18403,.T.);
#29676=ORIENTED_EDGE('',*,*,#19574,.F.);
#29677=ORIENTED_EDGE('',*,*,#18713,.T.);
#29678=ORIENTED_EDGE('',*,*,#19575,.T.);
#29679=ORIENTED_EDGE('',*,*,#18397,.T.);
#29680=ORIENTED_EDGE('',*,*,#19280,.T.);
#29681=ORIENTED_EDGE('',*,*,#19049,.T.);
#29682=ORIENTED_EDGE('',*,*,#18812,.T.);
#29683=ORIENTED_EDGE('',*,*,#18712,.T.);
#29684=ORIENTED_EDGE('',*,*,#19576,.T.);
#29685=ORIENTED_EDGE('',*,*,#18398,.T.);
#29686=ORIENTED_EDGE('',*,*,#19575,.F.);
#29687=ORIENTED_EDGE('',*,*,#18711,.T.);
#29688=ORIENTED_EDGE('',*,*,#18814,.T.);
#29689=ORIENTED_EDGE('',*,*,#19051,.T.);
#29690=ORIENTED_EDGE('',*,*,#19281,.T.);
#29691=ORIENTED_EDGE('',*,*,#18399,.T.);
#29692=ORIENTED_EDGE('',*,*,#19576,.F.);
#29693=ORIENTED_EDGE('',*,*,#18716,.T.);
#29694=ORIENTED_EDGE('',*,*,#18120,.T.);
#29695=ORIENTED_EDGE('',*,*,#18394,.T.);
#29696=ORIENTED_EDGE('',*,*,#19278,.T.);
#29697=ORIENTED_EDGE('',*,*,#19046,.T.);
#29698=ORIENTED_EDGE('',*,*,#18809,.T.);
#29699=ORIENTED_EDGE('',*,*,#18715,.T.);
#29700=ORIENTED_EDGE('',*,*,#18811,.T.);
#29701=ORIENTED_EDGE('',*,*,#19048,.T.);
#29702=ORIENTED_EDGE('',*,*,#19279,.T.);
#29703=ORIENTED_EDGE('',*,*,#18395,.T.);
#29704=ORIENTED_EDGE('',*,*,#18118,.F.);
#29705=ORIENTED_EDGE('',*,*,#18719,.T.);
#29706=ORIENTED_EDGE('',*,*,#18116,.T.);
#29707=ORIENTED_EDGE('',*,*,#18391,.T.);
#29708=ORIENTED_EDGE('',*,*,#19276,.T.);
#29709=ORIENTED_EDGE('',*,*,#19043,.T.);
#29710=ORIENTED_EDGE('',*,*,#18806,.T.);
#29711=ORIENTED_EDGE('',*,*,#18718,.T.);
#29712=ORIENTED_EDGE('',*,*,#18808,.T.);
#29713=ORIENTED_EDGE('',*,*,#19045,.T.);
#29714=ORIENTED_EDGE('',*,*,#19277,.T.);
#29715=ORIENTED_EDGE('',*,*,#18392,.T.);
#29716=ORIENTED_EDGE('',*,*,#18114,.F.);
#29717=ORIENTED_EDGE('',*,*,#18722,.T.);
#29718=ORIENTED_EDGE('',*,*,#18112,.T.);
#29719=ORIENTED_EDGE('',*,*,#18388,.T.);
#29720=ORIENTED_EDGE('',*,*,#19274,.T.);
#29721=ORIENTED_EDGE('',*,*,#19040,.T.);
#29722=ORIENTED_EDGE('',*,*,#18803,.T.);
#29723=ORIENTED_EDGE('',*,*,#18721,.T.);
#29724=ORIENTED_EDGE('',*,*,#18805,.T.);
#29725=ORIENTED_EDGE('',*,*,#19042,.T.);
#29726=ORIENTED_EDGE('',*,*,#19275,.T.);
#29727=ORIENTED_EDGE('',*,*,#18389,.T.);
#29728=ORIENTED_EDGE('',*,*,#18110,.F.);
#29729=ORIENTED_EDGE('',*,*,#18725,.T.);
#29730=ORIENTED_EDGE('',*,*,#18108,.T.);
#29731=ORIENTED_EDGE('',*,*,#18385,.T.);
#29732=ORIENTED_EDGE('',*,*,#19272,.T.);
#29733=ORIENTED_EDGE('',*,*,#19037,.T.);
#29734=ORIENTED_EDGE('',*,*,#18800,.T.);
#29735=ORIENTED_EDGE('',*,*,#18724,.T.);
#29736=ORIENTED_EDGE('',*,*,#18802,.T.);
#29737=ORIENTED_EDGE('',*,*,#19039,.T.);
#29738=ORIENTED_EDGE('',*,*,#19273,.T.);
#29739=ORIENTED_EDGE('',*,*,#18386,.T.);
#29740=ORIENTED_EDGE('',*,*,#18106,.F.);
#29741=ORIENTED_EDGE('',*,*,#18728,.T.);
#29742=ORIENTED_EDGE('',*,*,#18104,.T.);
#29743=ORIENTED_EDGE('',*,*,#18382,.T.);
#29744=ORIENTED_EDGE('',*,*,#19270,.T.);
#29745=ORIENTED_EDGE('',*,*,#19034,.T.);
#29746=ORIENTED_EDGE('',*,*,#18797,.T.);
#29747=ORIENTED_EDGE('',*,*,#18727,.T.);
#29748=ORIENTED_EDGE('',*,*,#18799,.T.);
#29749=ORIENTED_EDGE('',*,*,#19036,.T.);
#29750=ORIENTED_EDGE('',*,*,#19271,.T.);
#29751=ORIENTED_EDGE('',*,*,#18383,.T.);
#29752=ORIENTED_EDGE('',*,*,#18102,.F.);
#29753=ORIENTED_EDGE('',*,*,#18731,.T.);
#29754=ORIENTED_EDGE('',*,*,#18100,.T.);
#29755=ORIENTED_EDGE('',*,*,#18379,.T.);
#29756=ORIENTED_EDGE('',*,*,#19267,.T.);
#29757=ORIENTED_EDGE('',*,*,#19030,.T.);
#29758=ORIENTED_EDGE('',*,*,#18793,.T.);
#29759=ORIENTED_EDGE('',*,*,#18730,.T.);
#29760=ORIENTED_EDGE('',*,*,#18796,.T.);
#29761=ORIENTED_EDGE('',*,*,#19033,.T.);
#29762=ORIENTED_EDGE('',*,*,#19269,.T.);
#29763=ORIENTED_EDGE('',*,*,#18380,.T.);
#29764=ORIENTED_EDGE('',*,*,#18098,.F.);
#29765=PLANE('',#32120);
#29766=PLANE('',#32121);
#29767=PLANE('',#32122);
#29768=PLANE('',#32123);
#29769=PLANE('',#32124);
#29770=PLANE('',#32125);
#29771=PLANE('',#32126);
#29772=PLANE('',#32127);
#29773=PLANE('',#32128);
#29774=PLANE('',#32132);
#29775=PLANE('',#32133);
#29776=PLANE('',#32156);
#29777=PLANE('',#32160);
#29778=PLANE('',#32164);
#29779=PLANE('',#32171);
#29780=PLANE('',#32191);
#29781=PLANE('',#32194);
#29782=PLANE('',#32195);
#29783=PLANE('',#32196);
#29784=PLANE('',#33332);
#29785=PLANE('',#33333);
#29786=PLANE('',#33343);
#29787=PLANE('',#33344);
#29788=PLANE('',#33345);
#29789=PLANE('',#33346);
#29790=PLANE('',#33347);
#29791=PLANE('',#33348);
#29792=PLANE('',#33349);
#29793=PLANE('',#33350);
#29794=PLANE('',#33352);
#29795=PLANE('',#33354);
#29796=PLANE('',#33355);
#29797=PLANE('',#33357);
#29798=PLANE('',#33358);
#29799=PLANE('',#33360);
#29800=PLANE('',#33361);
#29801=PLANE('',#33363);
#29802=PLANE('',#33364);
#29803=PLANE('',#33366);
#29804=PLANE('',#33367);
#29805=PLANE('',#33369);
#29806=PLANE('',#33370);
#29807=PLANE('',#33372);
#29808=PLANE('',#33373);
#29809=PLANE('',#33374);
#29810=PLANE('',#33375);
#29811=PLANE('',#33376);
#29812=PLANE('',#33377);
#29813=PLANE('',#33378);
#29814=PLANE('',#33379);
#29815=PLANE('',#33380);
#29816=PLANE('',#33381);
#29817=PLANE('',#33382);
#29818=PLANE('',#33383);
#29819=PLANE('',#33384);
#29820=PLANE('',#33385);
#29821=PLANE('',#33386);
#29822=PLANE('',#33387);
#29823=PLANE('',#33388);
#29824=PLANE('',#33389);
#29825=PLANE('',#33390);
#29826=PLANE('',#33391);
#29827=PLANE('',#33393);
#29828=PLANE('',#33394);
#29829=PLANE('',#33396);
#29830=PLANE('',#33397);
#29831=PLANE('',#33399);
#29832=PLANE('',#33400);
#29833=PLANE('',#33402);
#29834=PLANE('',#33403);
#29835=PLANE('',#33405);
#29836=PLANE('',#33406);
#29837=PLANE('',#33408);
#29838=PLANE('',#33409);
#29839=PLANE('',#33411);
#29840=PLANE('',#33412);
#29841=PLANE('',#33414);
#29842=PLANE('',#33415);
#29843=PLANE('',#33417);
#29844=PLANE('',#33418);
#29845=PLANE('',#33420);
#29846=PLANE('',#33421);
#29847=PLANE('',#33423);
#29848=PLANE('',#33424);
#29849=PLANE('',#33426);
#29850=PLANE('',#33427);
#29851=PLANE('',#33429);
#29852=PLANE('',#33430);
#29853=PLANE('',#33432);
#29854=PLANE('',#33433);
#29855=PLANE('',#33435);
#29856=PLANE('',#33436);
#29857=PLANE('',#33438);
#29858=PLANE('',#33439);
#29859=PLANE('',#33441);
#29860=PLANE('',#33442);
#29861=PLANE('',#33444);
#29862=PLANE('',#33445);
#29863=PLANE('',#33447);
#29864=PLANE('',#33448);
#29865=PLANE('',#33450);
#29866=PLANE('',#33451);
#29867=PLANE('',#33453);
#29868=PLANE('',#33454);
#29869=PLANE('',#33456);
#29870=PLANE('',#33457);
#29871=PLANE('',#33459);
#29872=PLANE('',#33460);
#29873=PLANE('',#33462);
#29874=PLANE('',#33463);
#29875=PLANE('',#33465);
#29876=PLANE('',#33466);
#29877=PLANE('',#33468);
#29878=PLANE('',#33469);
#29879=PLANE('',#33471);
#29880=PLANE('',#33472);
#29881=PLANE('',#33474);
#29882=PLANE('',#33475);
#29883=PLANE('',#33477);
#29884=PLANE('',#33478);
#29885=PLANE('',#33480);
#29886=PLANE('',#33481);
#29887=PLANE('',#33483);
#29888=PLANE('',#33484);
#29889=PLANE('',#33486);
#29890=PLANE('',#33487);
#29891=PLANE('',#33489);
#29892=PLANE('',#33490);
#29893=PLANE('',#33492);
#29894=PLANE('',#33493);
#29895=PLANE('',#33495);
#29896=PLANE('',#33496);
#29897=PLANE('',#33498);
#29898=PLANE('',#33499);
#29899=PLANE('',#33501);
#29900=PLANE('',#33502);
#29901=PLANE('',#33504);
#29902=PLANE('',#33505);
#29903=PLANE('',#33507);
#29904=PLANE('',#33508);
#29905=PLANE('',#33510);
#29906=PLANE('',#33511);
#29907=PLANE('',#33513);
#29908=PLANE('',#33514);
#29909=PLANE('',#33516);
#29910=PLANE('',#33517);
#29911=PLANE('',#33519);
#29912=PLANE('',#33520);
#29913=PLANE('',#33522);
#29914=PLANE('',#33523);
#29915=PLANE('',#33525);
#29916=PLANE('',#33526);
#29917=PLANE('',#33528);
#29918=PLANE('',#33529);
#29919=PLANE('',#33531);
#29920=PLANE('',#33532);
#29921=PLANE('',#33534);
#29922=PLANE('',#33535);
#29923=PLANE('',#33537);
#29924=PLANE('',#33538);
#29925=PLANE('',#33540);
#29926=PLANE('',#33541);
#29927=PLANE('',#33543);
#29928=PLANE('',#33544);
#29929=PLANE('',#33546);
#29930=PLANE('',#33547);
#29931=PLANE('',#33549);
#29932=PLANE('',#33550);
#29933=PLANE('',#33552);
#29934=PLANE('',#33553);
#29935=PLANE('',#33555);
#29936=PLANE('',#33556);
#29937=PLANE('',#33558);
#29938=PLANE('',#33559);
#29939=PLANE('',#33561);
#29940=PLANE('',#33562);
#29941=PLANE('',#33564);
#29942=PLANE('',#33565);
#29943=PLANE('',#33566);
#29944=PLANE('',#33567);
#29945=PLANE('',#33568);
#29946=PLANE('',#33569);
#29947=PLANE('',#33570);
#29948=PLANE('',#33571);
#29949=PLANE('',#33572);
#29950=PLANE('',#33573);
#29951=PLANE('',#33574);
#29952=PLANE('',#33575);
#29953=PLANE('',#33576);
#29954=PLANE('',#34712);
#29955=PLANE('',#34713);
#29956=PLANE('',#34723);
#29957=PLANE('',#34724);
#29958=PLANE('',#34725);
#29959=PLANE('',#34726);
#29960=PLANE('',#34727);
#29961=PLANE('',#34728);
#29962=PLANE('',#34729);
#29963=PLANE('',#34730);
#29964=PLANE('',#34732);
#29965=PLANE('',#34734);
#29966=PLANE('',#34735);
#29967=PLANE('',#34737);
#29968=PLANE('',#34738);
#29969=PLANE('',#34740);
#29970=PLANE('',#34741);
#29971=PLANE('',#34743);
#29972=PLANE('',#34744);
#29973=PLANE('',#34746);
#29974=PLANE('',#34747);
#29975=PLANE('',#34749);
#29976=PLANE('',#34750);
#29977=PLANE('',#34752);
#29978=PLANE('',#34753);
#29979=PLANE('',#34754);
#29980=PLANE('',#34755);
#29981=PLANE('',#34756);
#29982=PLANE('',#34757);
#29983=PLANE('',#34758);
#29984=PLANE('',#34759);
#29985=PLANE('',#34760);
#29986=PLANE('',#34761);
#29987=PLANE('',#34762);
#29988=PLANE('',#34763);
#29989=PLANE('',#34764);
#29990=PLANE('',#34765);
#29991=PLANE('',#34766);
#29992=PLANE('',#34767);
#29993=PLANE('',#34768);
#29994=PLANE('',#34769);
#29995=PLANE('',#34770);
#29996=PLANE('',#34771);
#29997=PLANE('',#34773);
#29998=PLANE('',#34774);
#29999=PLANE('',#34776);
#30000=PLANE('',#34777);
#30001=PLANE('',#34779);
#30002=PLANE('',#34780);
#30003=PLANE('',#34782);
#30004=PLANE('',#34783);
#30005=PLANE('',#34785);
#30006=PLANE('',#34786);
#30007=PLANE('',#34788);
#30008=PLANE('',#34789);
#30009=PLANE('',#34791);
#30010=PLANE('',#34792);
#30011=PLANE('',#34794);
#30012=PLANE('',#34795);
#30013=PLANE('',#34797);
#30014=PLANE('',#34798);
#30015=PLANE('',#34800);
#30016=PLANE('',#34801);
#30017=PLANE('',#34803);
#30018=PLANE('',#34804);
#30019=PLANE('',#34806);
#30020=PLANE('',#34807);
#30021=PLANE('',#34809);
#30022=PLANE('',#34810);
#30023=PLANE('',#34812);
#30024=PLANE('',#34813);
#30025=PLANE('',#34815);
#30026=PLANE('',#34816);
#30027=PLANE('',#34818);
#30028=PLANE('',#34819);
#30029=PLANE('',#34821);
#30030=PLANE('',#34822);
#30031=PLANE('',#34824);
#30032=PLANE('',#34825);
#30033=PLANE('',#34827);
#30034=PLANE('',#34828);
#30035=PLANE('',#34830);
#30036=PLANE('',#34831);
#30037=PLANE('',#34833);
#30038=PLANE('',#34834);
#30039=PLANE('',#34836);
#30040=PLANE('',#34837);
#30041=PLANE('',#34839);
#30042=PLANE('',#34840);
#30043=PLANE('',#34842);
#30044=PLANE('',#34843);
#30045=PLANE('',#34845);
#30046=PLANE('',#34846);
#30047=PLANE('',#34848);
#30048=PLANE('',#34849);
#30049=PLANE('',#34851);
#30050=PLANE('',#34852);
#30051=PLANE('',#34854);
#30052=PLANE('',#34855);
#30053=PLANE('',#34857);
#30054=PLANE('',#34858);
#30055=PLANE('',#34860);
#30056=PLANE('',#34861);
#30057=PLANE('',#34863);
#30058=PLANE('',#34864);
#30059=PLANE('',#34866);
#30060=PLANE('',#34867);
#30061=PLANE('',#34869);
#30062=PLANE('',#34870);
#30063=PLANE('',#34872);
#30064=PLANE('',#34873);
#30065=PLANE('',#34875);
#30066=PLANE('',#34876);
#30067=PLANE('',#34878);
#30068=PLANE('',#34879);
#30069=PLANE('',#34881);
#30070=PLANE('',#34882);
#30071=PLANE('',#34884);
#30072=PLANE('',#34885);
#30073=PLANE('',#34887);
#30074=PLANE('',#34888);
#30075=PLANE('',#34890);
#30076=PLANE('',#34891);
#30077=PLANE('',#34893);
#30078=PLANE('',#34894);
#30079=PLANE('',#34896);
#30080=PLANE('',#34897);
#30081=PLANE('',#34899);
#30082=PLANE('',#34900);
#30083=PLANE('',#34902);
#30084=PLANE('',#34903);
#30085=PLANE('',#34905);
#30086=PLANE('',#34906);
#30087=PLANE('',#34908);
#30088=PLANE('',#34909);
#30089=PLANE('',#34911);
#30090=PLANE('',#34912);
#30091=PLANE('',#34914);
#30092=PLANE('',#34915);
#30093=PLANE('',#34917);
#30094=PLANE('',#34918);
#30095=PLANE('',#34920);
#30096=PLANE('',#34921);
#30097=PLANE('',#34923);
#30098=PLANE('',#34924);
#30099=PLANE('',#34926);
#30100=PLANE('',#34927);
#30101=PLANE('',#34929);
#30102=PLANE('',#34930);
#30103=PLANE('',#34932);
#30104=PLANE('',#34933);
#30105=PLANE('',#34935);
#30106=PLANE('',#34936);
#30107=PLANE('',#34938);
#30108=PLANE('',#34939);
#30109=PLANE('',#34941);
#30110=PLANE('',#34942);
#30111=PLANE('',#34944);
#30112=PLANE('',#34945);
#30113=PLANE('',#34946);
#30114=PLANE('',#34947);
#30115=PLANE('',#34948);
#30116=PLANE('',#34949);
#30117=PLANE('',#34950);
#30118=PLANE('',#34951);
#30119=PLANE('',#34952);
#30120=PLANE('',#34953);
#30121=PLANE('',#34954);
#30122=PLANE('',#34955);
#30123=PLANE('',#34956);
#30124=PLANE('',#36092);
#30125=PLANE('',#36093);
#30126=PLANE('',#36103);
#30127=PLANE('',#36104);
#30128=PLANE('',#36105);
#30129=PLANE('',#36106);
#30130=PLANE('',#36107);
#30131=PLANE('',#36108);
#30132=PLANE('',#36109);
#30133=PLANE('',#36110);
#30134=PLANE('',#36112);
#30135=PLANE('',#36114);
#30136=PLANE('',#36115);
#30137=PLANE('',#36117);
#30138=PLANE('',#36118);
#30139=PLANE('',#36120);
#30140=PLANE('',#36121);
#30141=PLANE('',#36123);
#30142=PLANE('',#36124);
#30143=PLANE('',#36126);
#30144=PLANE('',#36127);
#30145=PLANE('',#36129);
#30146=PLANE('',#36130);
#30147=PLANE('',#36132);
#30148=PLANE('',#36133);
#30149=PLANE('',#36134);
#30150=PLANE('',#36135);
#30151=PLANE('',#36136);
#30152=PLANE('',#36137);
#30153=PLANE('',#36138);
#30154=PLANE('',#36139);
#30155=PLANE('',#36140);
#30156=PLANE('',#36141);
#30157=PLANE('',#36142);
#30158=PLANE('',#36143);
#30159=PLANE('',#36144);
#30160=PLANE('',#36145);
#30161=PLANE('',#36146);
#30162=PLANE('',#36147);
#30163=PLANE('',#36148);
#30164=PLANE('',#36149);
#30165=PLANE('',#36150);
#30166=PLANE('',#36151);
#30167=PLANE('',#36153);
#30168=PLANE('',#36154);
#30169=PLANE('',#36156);
#30170=PLANE('',#36157);
#30171=PLANE('',#36159);
#30172=PLANE('',#36160);
#30173=PLANE('',#36162);
#30174=PLANE('',#36163);
#30175=PLANE('',#36165);
#30176=PLANE('',#36166);
#30177=PLANE('',#36168);
#30178=PLANE('',#36169);
#30179=PLANE('',#36171);
#30180=PLANE('',#36172);
#30181=PLANE('',#36174);
#30182=PLANE('',#36175);
#30183=PLANE('',#36177);
#30184=PLANE('',#36178);
#30185=PLANE('',#36180);
#30186=PLANE('',#36181);
#30187=PLANE('',#36183);
#30188=PLANE('',#36184);
#30189=PLANE('',#36186);
#30190=PLANE('',#36187);
#30191=PLANE('',#36189);
#30192=PLANE('',#36190);
#30193=PLANE('',#36192);
#30194=PLANE('',#36193);
#30195=PLANE('',#36195);
#30196=PLANE('',#36196);
#30197=PLANE('',#36198);
#30198=PLANE('',#36199);
#30199=PLANE('',#36201);
#30200=PLANE('',#36202);
#30201=PLANE('',#36204);
#30202=PLANE('',#36205);
#30203=PLANE('',#36207);
#30204=PLANE('',#36208);
#30205=PLANE('',#36210);
#30206=PLANE('',#36211);
#30207=PLANE('',#36213);
#30208=PLANE('',#36214);
#30209=PLANE('',#36216);
#30210=PLANE('',#36217);
#30211=PLANE('',#36219);
#30212=PLANE('',#36220);
#30213=PLANE('',#36222);
#30214=PLANE('',#36223);
#30215=PLANE('',#36225);
#30216=PLANE('',#36226);
#30217=PLANE('',#36228);
#30218=PLANE('',#36229);
#30219=PLANE('',#36231);
#30220=PLANE('',#36232);
#30221=PLANE('',#36234);
#30222=PLANE('',#36235);
#30223=PLANE('',#36237);
#30224=PLANE('',#36238);
#30225=PLANE('',#36240);
#30226=PLANE('',#36241);
#30227=PLANE('',#36243);
#30228=PLANE('',#36244);
#30229=PLANE('',#36246);
#30230=PLANE('',#36247);
#30231=PLANE('',#36249);
#30232=PLANE('',#36250);
#30233=PLANE('',#36252);
#30234=PLANE('',#36253);
#30235=PLANE('',#36255);
#30236=PLANE('',#36256);
#30237=PLANE('',#36258);
#30238=PLANE('',#36259);
#30239=PLANE('',#36261);
#30240=PLANE('',#36262);
#30241=PLANE('',#36264);
#30242=PLANE('',#36265);
#30243=PLANE('',#36267);
#30244=PLANE('',#36268);
#30245=PLANE('',#36270);
#30246=PLANE('',#36271);
#30247=PLANE('',#36273);
#30248=PLANE('',#36274);
#30249=PLANE('',#36276);
#30250=PLANE('',#36277);
#30251=PLANE('',#36279);
#30252=PLANE('',#36280);
#30253=PLANE('',#36282);
#30254=PLANE('',#36283);
#30255=PLANE('',#36285);
#30256=PLANE('',#36286);
#30257=PLANE('',#36288);
#30258=PLANE('',#36289);
#30259=PLANE('',#36291);
#30260=PLANE('',#36292);
#30261=PLANE('',#36294);
#30262=PLANE('',#36295);
#30263=PLANE('',#36297);
#30264=PLANE('',#36298);
#30265=PLANE('',#36300);
#30266=PLANE('',#36301);
#30267=PLANE('',#36303);
#30268=PLANE('',#36304);
#30269=PLANE('',#36306);
#30270=PLANE('',#36307);
#30271=PLANE('',#36309);
#30272=PLANE('',#36310);
#30273=PLANE('',#36312);
#30274=PLANE('',#36313);
#30275=PLANE('',#36315);
#30276=PLANE('',#36316);
#30277=PLANE('',#36318);
#30278=PLANE('',#36319);
#30279=PLANE('',#36321);
#30280=PLANE('',#36322);
#30281=PLANE('',#36324);
#30282=PLANE('',#36325);
#30283=PLANE('',#36326);
#30284=PLANE('',#36327);
#30285=PLANE('',#36328);
#30286=PLANE('',#36329);
#30287=PLANE('',#36330);
#30288=PLANE('',#36331);
#30289=PLANE('',#36332);
#30290=PLANE('',#36333);
#30291=PLANE('',#36334);
#30292=PLANE('',#36335);
#30293=PLANE('',#36336);
#30294=ADVANCED_FACE('',(#5134),#29765,.F.);
#30295=ADVANCED_FACE('',(#5135),#29766,.F.);
#30296=ADVANCED_FACE('',(#5136),#29767,.F.);
#30297=ADVANCED_FACE('',(#5137),#29768,.F.);
#30298=ADVANCED_FACE('',(#5138),#29769,.F.);
#30299=ADVANCED_FACE('',(#5139),#29770,.F.);
#30300=ADVANCED_FACE('',(#5140),#29771,.F.);
#30301=ADVANCED_FACE('',(#5141),#29772,.F.);
#30302=ADVANCED_FACE('',(#5142),#29773,.F.);
#30303=ADVANCED_FACE('',(#5143),#4455,.T.);
#30304=ADVANCED_FACE('',(#5144,#3387),#29774,.T.);
#30305=ADVANCED_FACE('',(#5145),#29775,.F.);
#30306=ADVANCED_FACE('',(#5146),#3352,.T.);
#30307=ADVANCED_FACE('',(#5147),#3353,.T.);
#30308=ADVANCED_FACE('',(#5148),#3354,.T.);
#30309=ADVANCED_FACE('',(#5149),#4456,.F.);
#30310=ADVANCED_FACE('',(#5150),#4457,.F.);
#30311=ADVANCED_FACE('',(#5151),#4458,.F.);
#30312=ADVANCED_FACE('',(#5152),#4459,.F.);
#30313=ADVANCED_FACE('',(#5153),#29776,.T.);
#30314=ADVANCED_FACE('',(#5154),#4460,.F.);
#30315=ADVANCED_FACE('',(#5155),#29777,.T.);
#30316=ADVANCED_FACE('',(#5156),#4461,.F.);
#30317=ADVANCED_FACE('',(#5157),#29778,.T.);
#30318=ADVANCED_FACE('',(#5158),#4462,.T.);
#30319=ADVANCED_FACE('',(#5159),#4463,.T.);
#30320=ADVANCED_FACE('',(#5160,#3388,#3389,#3390),#29779,.T.);
#30321=ADVANCED_FACE('',(#5161),#4464,.T.);
#30322=ADVANCED_FACE('',(#5162),#4465,.T.);
#30323=ADVANCED_FACE('',(#5163),#4466,.T.);
#30324=ADVANCED_FACE('',(#5164),#4467,.T.);
#30325=ADVANCED_FACE('',(#5165),#4468,.T.);
#30326=ADVANCED_FACE('',(#5166),#4469,.T.);
#30327=ADVANCED_FACE('',(#5167),#29780,.T.);
#30328=ADVANCED_FACE('',(#5168),#4470,.T.);
#30329=ADVANCED_FACE('',(#5169),#29781,.T.);
#30330=ADVANCED_FACE('',(#5170),#29782,.T.);
#30331=ADVANCED_FACE('',(#5171,#3391,#3392,#3393),#29783,.F.);
#30332=ADVANCED_FACE('',(#5172),#4471,.T.);
#30333=ADVANCED_FACE('',(#5173),#4472,.T.);
#30334=ADVANCED_FACE('',(#5174),#4473,.T.);
#30335=ADVANCED_FACE('',(#5175),#4474,.T.);
#30336=ADVANCED_FACE('',(#5176),#4475,.T.);
#30337=ADVANCED_FACE('',(#5177),#4476,.T.);
#30338=ADVANCED_FACE('',(#5178),#4477,.T.);
#30339=ADVANCED_FACE('',(#5179),#4478,.T.);
#30340=ADVANCED_FACE('',(#5180),#4479,.T.);
#30341=ADVANCED_FACE('',(#5181),#4480,.T.);
#30342=ADVANCED_FACE('',(#5182),#4481,.T.);
#30343=ADVANCED_FACE('',(#5183),#4482,.T.);
#30344=ADVANCED_FACE('',(#5184),#4483,.T.);
#30345=ADVANCED_FACE('',(#5185),#4484,.T.);
#30346=ADVANCED_FACE('',(#5186),#4485,.T.);
#30347=ADVANCED_FACE('',(#5187),#4486,.T.);
#30348=ADVANCED_FACE('',(#5188),#4487,.T.);
#30349=ADVANCED_FACE('',(#5189),#4488,.T.);
#30350=ADVANCED_FACE('',(#5190),#4489,.T.);
#30351=ADVANCED_FACE('',(#5191),#4490,.T.);
#30352=ADVANCED_FACE('',(#5192),#4491,.T.);
#30353=ADVANCED_FACE('',(#5193),#4492,.T.);
#30354=ADVANCED_FACE('',(#5194),#4493,.T.);
#30355=ADVANCED_FACE('',(#5195),#4494,.T.);
#30356=ADVANCED_FACE('',(#5196),#4495,.T.);
#30357=ADVANCED_FACE('',(#5197),#4496,.T.);
#30358=ADVANCED_FACE('',(#5198),#4497,.T.);
#30359=ADVANCED_FACE('',(#5199),#4498,.T.);
#30360=ADVANCED_FACE('',(#5200),#2956,.T.);
#30361=ADVANCED_FACE('',(#5201),#4499,.T.);
#30362=ADVANCED_FACE('',(#5202),#4500,.T.);
#30363=ADVANCED_FACE('',(#5203),#4501,.T.);
#30364=ADVANCED_FACE('',(#5204),#4502,.T.);
#30365=ADVANCED_FACE('',(#5205),#4503,.T.);
#30366=ADVANCED_FACE('',(#5206),#4504,.T.);
#30367=ADVANCED_FACE('',(#5207),#4505,.T.);
#30368=ADVANCED_FACE('',(#5208),#4506,.T.);
#30369=ADVANCED_FACE('',(#5209),#4507,.T.);
#30370=ADVANCED_FACE('',(#5210),#4508,.T.);
#30371=ADVANCED_FACE('',(#5211),#4509,.T.);
#30372=ADVANCED_FACE('',(#5212),#4510,.T.);
#30373=ADVANCED_FACE('',(#5213),#4511,.T.);
#30374=ADVANCED_FACE('',(#5214),#4512,.T.);
#30375=ADVANCED_FACE('',(#5215),#4513,.T.);
#30376=ADVANCED_FACE('',(#5216),#4514,.T.);
#30377=ADVANCED_FACE('',(#5217),#4515,.T.);
#30378=ADVANCED_FACE('',(#5218),#4516,.T.);
#30379=ADVANCED_FACE('',(#5219),#4517,.T.);
#30380=ADVANCED_FACE('',(#5220),#4518,.T.);
#30381=ADVANCED_FACE('',(#5221),#4519,.T.);
#30382=ADVANCED_FACE('',(#5222),#4520,.T.);
#30383=ADVANCED_FACE('',(#5223),#4521,.T.);
#30384=ADVANCED_FACE('',(#5224),#4522,.T.);
#30385=ADVANCED_FACE('',(#5225),#4523,.T.);
#30386=ADVANCED_FACE('',(#5226),#4524,.T.);
#30387=ADVANCED_FACE('',(#5227),#4525,.T.);
#30388=ADVANCED_FACE('',(#5228),#4526,.T.);
#30389=ADVANCED_FACE('',(#5229),#4527,.T.);
#30390=ADVANCED_FACE('',(#5230),#4528,.T.);
#30391=ADVANCED_FACE('',(#5231),#4529,.T.);
#30392=ADVANCED_FACE('',(#5232),#2957,.T.);
#30393=ADVANCED_FACE('',(#5233),#4530,.T.);
#30394=ADVANCED_FACE('',(#5234),#4531,.F.);
#30395=ADVANCED_FACE('',(#5235),#4532,.F.);
#30396=ADVANCED_FACE('',(#5236),#4533,.F.);
#30397=ADVANCED_FACE('',(#5237),#4534,.F.);
#30398=ADVANCED_FACE('',(#5238),#4535,.F.);
#30399=ADVANCED_FACE('',(#5239),#4536,.F.);
#30400=ADVANCED_FACE('',(#5240),#4537,.F.);
#30401=ADVANCED_FACE('',(#5241),#4538,.F.);
#30402=ADVANCED_FACE('',(#5242),#4539,.F.);
#30403=ADVANCED_FACE('',(#5243),#4540,.F.);
#30404=ADVANCED_FACE('',(#5244),#4541,.F.);
#30405=ADVANCED_FACE('',(#5245),#4542,.F.);
#30406=ADVANCED_FACE('',(#5246),#4543,.F.);
#30407=ADVANCED_FACE('',(#5247),#4544,.F.);
#30408=ADVANCED_FACE('',(#5248),#4545,.F.);
#30409=ADVANCED_FACE('',(#5249),#2958,.F.);
#30410=ADVANCED_FACE('',(#5250),#49,.T.);
#30411=ADVANCED_FACE('',(#5251),#2959,.T.);
#30412=ADVANCED_FACE('',(#5252),#2960,.T.);
#30413=ADVANCED_FACE('',(#5253),#50,.F.);
#30414=ADVANCED_FACE('',(#5254),#4546,.T.);
#30415=ADVANCED_FACE('',(#5255),#51,.T.);
#30416=ADVANCED_FACE('',(#5256),#52,.F.);
#30417=ADVANCED_FACE('',(#5257),#53,.T.);
#30418=ADVANCED_FACE('',(#5258),#54,.T.);
#30419=ADVANCED_FACE('',(#5259),#55,.T.);
#30420=ADVANCED_FACE('',(#5260),#56,.T.);
#30421=ADVANCED_FACE('',(#5261),#57,.T.);
#30422=ADVANCED_FACE('',(#5262),#58,.T.);
#30423=ADVANCED_FACE('',(#5263),#59,.T.);
#30424=ADVANCED_FACE('',(#5264),#60,.T.);
#30425=ADVANCED_FACE('',(#5265),#61,.T.);
#30426=ADVANCED_FACE('',(#5266),#62,.T.);
#30427=ADVANCED_FACE('',(#5267),#63,.T.);
#30428=ADVANCED_FACE('',(#5268),#64,.T.);
#30429=ADVANCED_FACE('',(#5269),#65,.T.);
#30430=ADVANCED_FACE('',(#5270),#66,.T.);
#30431=ADVANCED_FACE('',(#5271),#67,.T.);
#30432=ADVANCED_FACE('',(#5272),#68,.T.);
#30433=ADVANCED_FACE('',(#5273),#69,.T.);
#30434=ADVANCED_FACE('',(#5274),#70,.T.);
#30435=ADVANCED_FACE('',(#5275),#71,.T.);
#30436=ADVANCED_FACE('',(#5276),#72,.T.);
#30437=ADVANCED_FACE('',(#5277),#73,.T.);
#30438=ADVANCED_FACE('',(#5278),#74,.T.);
#30439=ADVANCED_FACE('',(#5279),#75,.T.);
#30440=ADVANCED_FACE('',(#5280),#76,.T.);
#30441=ADVANCED_FACE('',(#5281),#77,.T.);
#30442=ADVANCED_FACE('',(#5282),#78,.T.);
#30443=ADVANCED_FACE('',(#5283),#79,.T.);
#30444=ADVANCED_FACE('',(#5284),#80,.T.);
#30445=ADVANCED_FACE('',(#5285),#81,.T.);
#30446=ADVANCED_FACE('',(#5286),#82,.T.);
#30447=ADVANCED_FACE('',(#5287),#83,.T.);
#30448=ADVANCED_FACE('',(#5288),#84,.T.);
#30449=ADVANCED_FACE('',(#5289),#85,.T.);
#30450=ADVANCED_FACE('',(#5290),#86,.T.);
#30451=ADVANCED_FACE('',(#5291),#87,.T.);
#30452=ADVANCED_FACE('',(#5292),#88,.T.);
#30453=ADVANCED_FACE('',(#5293),#89,.T.);
#30454=ADVANCED_FACE('',(#5294),#90,.T.);
#30455=ADVANCED_FACE('',(#5295),#91,.T.);
#30456=ADVANCED_FACE('',(#5296),#92,.T.);
#30457=ADVANCED_FACE('',(#5297),#93,.T.);
#30458=ADVANCED_FACE('',(#5298),#94,.T.);
#30459=ADVANCED_FACE('',(#5299),#95,.T.);
#30460=ADVANCED_FACE('',(#5300),#96,.T.);
#30461=ADVANCED_FACE('',(#5301),#97,.T.);
#30462=ADVANCED_FACE('',(#5302),#98,.T.);
#30463=ADVANCED_FACE('',(#5303),#99,.T.);
#30464=ADVANCED_FACE('',(#5304),#100,.T.);
#30465=ADVANCED_FACE('',(#5305),#101,.T.);
#30466=ADVANCED_FACE('',(#5306),#102,.T.);
#30467=ADVANCED_FACE('',(#5307),#103,.T.);
#30468=ADVANCED_FACE('',(#5308),#104,.T.);
#30469=ADVANCED_FACE('',(#5309),#105,.T.);
#30470=ADVANCED_FACE('',(#5310),#106,.T.);
#30471=ADVANCED_FACE('',(#5311),#107,.T.);
#30472=ADVANCED_FACE('',(#5312),#108,.T.);
#30473=ADVANCED_FACE('',(#5313),#109,.T.);
#30474=ADVANCED_FACE('',(#5314),#110,.T.);
#30475=ADVANCED_FACE('',(#5315),#111,.T.);
#30476=ADVANCED_FACE('',(#5316),#112,.T.);
#30477=ADVANCED_FACE('',(#5317),#113,.T.);
#30478=ADVANCED_FACE('',(#5318),#114,.T.);
#30479=ADVANCED_FACE('',(#5319),#115,.T.);
#30480=ADVANCED_FACE('',(#5320),#116,.T.);
#30481=ADVANCED_FACE('',(#5321),#117,.T.);
#30482=ADVANCED_FACE('',(#5322),#118,.T.);
#30483=ADVANCED_FACE('',(#5323),#119,.T.);
#30484=ADVANCED_FACE('',(#5324),#120,.T.);
#30485=ADVANCED_FACE('',(#5325),#121,.T.);
#30486=ADVANCED_FACE('',(#5326),#122,.T.);
#30487=ADVANCED_FACE('',(#5327),#123,.T.);
#30488=ADVANCED_FACE('',(#5328),#124,.T.);
#30489=ADVANCED_FACE('',(#5329),#125,.T.);
#30490=ADVANCED_FACE('',(#5330),#126,.T.);
#30491=ADVANCED_FACE('',(#5331),#127,.T.);
#30492=ADVANCED_FACE('',(#5332),#128,.T.);
#30493=ADVANCED_FACE('',(#5333),#129,.T.);
#30494=ADVANCED_FACE('',(#5334),#130,.T.);
#30495=ADVANCED_FACE('',(#5335),#131,.T.);
#30496=ADVANCED_FACE('',(#5336),#4547,.T.);
#30497=ADVANCED_FACE('',(#5337),#4548,.T.);
#30498=ADVANCED_FACE('',(#5338),#4549,.T.);
#30499=ADVANCED_FACE('',(#5339),#4550,.T.);
#30500=ADVANCED_FACE('',(#5340),#4551,.T.);
#30501=ADVANCED_FACE('',(#5341),#4552,.T.);
#30502=ADVANCED_FACE('',(#5342),#4553,.T.);
#30503=ADVANCED_FACE('',(#5343),#4554,.T.);
#30504=ADVANCED_FACE('',(#5344),#4555,.T.);
#30505=ADVANCED_FACE('',(#5345),#4556,.T.);
#30506=ADVANCED_FACE('',(#5346),#4557,.T.);
#30507=ADVANCED_FACE('',(#5347),#4558,.T.);
#30508=ADVANCED_FACE('',(#5348),#4559,.T.);
#30509=ADVANCED_FACE('',(#5349),#4560,.T.);
#30510=ADVANCED_FACE('',(#5350),#4561,.T.);
#30511=ADVANCED_FACE('',(#5351),#4562,.T.);
#30512=ADVANCED_FACE('',(#5352),#4563,.T.);
#30513=ADVANCED_FACE('',(#5353),#4564,.T.);
#30514=ADVANCED_FACE('',(#5354),#4565,.T.);
#30515=ADVANCED_FACE('',(#5355),#4566,.T.);
#30516=ADVANCED_FACE('',(#5356),#4567,.T.);
#30517=ADVANCED_FACE('',(#5357),#4568,.T.);
#30518=ADVANCED_FACE('',(#5358),#4569,.T.);
#30519=ADVANCED_FACE('',(#5359),#4570,.T.);
#30520=ADVANCED_FACE('',(#5360),#4571,.T.);
#30521=ADVANCED_FACE('',(#5361),#4572,.T.);
#30522=ADVANCED_FACE('',(#5362),#4573,.T.);
#30523=ADVANCED_FACE('',(#5363),#4574,.T.);
#30524=ADVANCED_FACE('',(#5364),#4575,.T.);
#30525=ADVANCED_FACE('',(#5365),#4576,.T.);
#30526=ADVANCED_FACE('',(#5366),#4577,.T.);
#30527=ADVANCED_FACE('',(#5367),#4578,.T.);
#30528=ADVANCED_FACE('',(#5368),#4579,.T.);
#30529=ADVANCED_FACE('',(#5369),#4580,.T.);
#30530=ADVANCED_FACE('',(#5370),#4581,.T.);
#30531=ADVANCED_FACE('',(#5371),#4582,.T.);
#30532=ADVANCED_FACE('',(#5372),#4583,.T.);
#30533=ADVANCED_FACE('',(#5373),#4584,.T.);
#30534=ADVANCED_FACE('',(#5374),#4585,.T.);
#30535=ADVANCED_FACE('',(#5375),#4586,.T.);
#30536=ADVANCED_FACE('',(#5376),#4587,.T.);
#30537=ADVANCED_FACE('',(#5377),#4588,.T.);
#30538=ADVANCED_FACE('',(#5378),#4589,.T.);
#30539=ADVANCED_FACE('',(#5379),#4590,.T.);
#30540=ADVANCED_FACE('',(#5380),#4591,.T.);
#30541=ADVANCED_FACE('',(#5381),#4592,.T.);
#30542=ADVANCED_FACE('',(#5382),#4593,.T.);
#30543=ADVANCED_FACE('',(#5383),#4594,.T.);
#30544=ADVANCED_FACE('',(#5384),#4595,.T.);
#30545=ADVANCED_FACE('',(#5385),#4596,.T.);
#30546=ADVANCED_FACE('',(#5386),#4597,.T.);
#30547=ADVANCED_FACE('',(#5387),#4598,.T.);
#30548=ADVANCED_FACE('',(#5388),#4599,.T.);
#30549=ADVANCED_FACE('',(#5389),#4600,.T.);
#30550=ADVANCED_FACE('',(#5390),#4601,.T.);
#30551=ADVANCED_FACE('',(#5391),#4602,.T.);
#30552=ADVANCED_FACE('',(#5392),#4603,.T.);
#30553=ADVANCED_FACE('',(#5393),#4604,.T.);
#30554=ADVANCED_FACE('',(#5394),#4605,.T.);
#30555=ADVANCED_FACE('',(#5395),#4606,.T.);
#30556=ADVANCED_FACE('',(#5396),#4607,.T.);
#30557=ADVANCED_FACE('',(#5397),#4608,.T.);
#30558=ADVANCED_FACE('',(#5398),#4609,.T.);
#30559=ADVANCED_FACE('',(#5399),#4610,.T.);
#30560=ADVANCED_FACE('',(#5400),#4611,.T.);
#30561=ADVANCED_FACE('',(#5401),#4612,.T.);
#30562=ADVANCED_FACE('',(#5402),#4613,.T.);
#30563=ADVANCED_FACE('',(#5403),#4614,.T.);
#30564=ADVANCED_FACE('',(#5404),#4615,.T.);
#30565=ADVANCED_FACE('',(#5405),#4616,.T.);
#30566=ADVANCED_FACE('',(#5406),#4617,.T.);
#30567=ADVANCED_FACE('',(#5407),#4618,.T.);
#30568=ADVANCED_FACE('',(#5408),#4619,.T.);
#30569=ADVANCED_FACE('',(#5409),#4620,.T.);
#30570=ADVANCED_FACE('',(#5410),#4621,.T.);
#30571=ADVANCED_FACE('',(#5411),#4622,.T.);
#30572=ADVANCED_FACE('',(#5412),#4623,.T.);
#30573=ADVANCED_FACE('',(#5413),#4624,.T.);
#30574=ADVANCED_FACE('',(#5414),#4625,.T.);
#30575=ADVANCED_FACE('',(#5415),#132,.T.);
#30576=ADVANCED_FACE('',(#5416),#133,.T.);
#30577=ADVANCED_FACE('',(#5417),#134,.T.);
#30578=ADVANCED_FACE('',(#5418),#135,.T.);
#30579=ADVANCED_FACE('',(#5419),#136,.T.);
#30580=ADVANCED_FACE('',(#5420),#137,.T.);
#30581=ADVANCED_FACE('',(#5421),#138,.T.);
#30582=ADVANCED_FACE('',(#5422),#139,.T.);
#30583=ADVANCED_FACE('',(#5423),#140,.T.);
#30584=ADVANCED_FACE('',(#5424),#141,.T.);
#30585=ADVANCED_FACE('',(#5425),#142,.T.);
#30586=ADVANCED_FACE('',(#5426),#143,.T.);
#30587=ADVANCED_FACE('',(#5427),#144,.T.);
#30588=ADVANCED_FACE('',(#5428),#145,.T.);
#30589=ADVANCED_FACE('',(#5429),#146,.T.);
#30590=ADVANCED_FACE('',(#5430),#147,.T.);
#30591=ADVANCED_FACE('',(#5431),#148,.T.);
#30592=ADVANCED_FACE('',(#5432),#149,.T.);
#30593=ADVANCED_FACE('',(#5433),#150,.T.);
#30594=ADVANCED_FACE('',(#5434),#151,.T.);
#30595=ADVANCED_FACE('',(#5435),#152,.T.);
#30596=ADVANCED_FACE('',(#5436),#153,.T.);
#30597=ADVANCED_FACE('',(#5437),#154,.T.);
#30598=ADVANCED_FACE('',(#5438),#155,.T.);
#30599=ADVANCED_FACE('',(#5439),#156,.T.);
#30600=ADVANCED_FACE('',(#5440),#157,.T.);
#30601=ADVANCED_FACE('',(#5441),#158,.T.);
#30602=ADVANCED_FACE('',(#5442),#159,.T.);
#30603=ADVANCED_FACE('',(#5443),#160,.T.);
#30604=ADVANCED_FACE('',(#5444),#161,.T.);
#30605=ADVANCED_FACE('',(#5445),#162,.T.);
#30606=ADVANCED_FACE('',(#5446),#163,.T.);
#30607=ADVANCED_FACE('',(#5447),#164,.T.);
#30608=ADVANCED_FACE('',(#5448),#165,.T.);
#30609=ADVANCED_FACE('',(#5449),#166,.T.);
#30610=ADVANCED_FACE('',(#5450),#167,.T.);
#30611=ADVANCED_FACE('',(#5451),#168,.T.);
#30612=ADVANCED_FACE('',(#5452),#169,.T.);
#30613=ADVANCED_FACE('',(#5453),#170,.T.);
#30614=ADVANCED_FACE('',(#5454),#171,.T.);
#30615=ADVANCED_FACE('',(#5455),#172,.T.);
#30616=ADVANCED_FACE('',(#5456),#173,.T.);
#30617=ADVANCED_FACE('',(#5457),#174,.T.);
#30618=ADVANCED_FACE('',(#5458),#175,.T.);
#30619=ADVANCED_FACE('',(#5459),#176,.T.);
#30620=ADVANCED_FACE('',(#5460),#177,.T.);
#30621=ADVANCED_FACE('',(#5461),#178,.T.);
#30622=ADVANCED_FACE('',(#5462),#179,.T.);
#30623=ADVANCED_FACE('',(#5463),#180,.T.);
#30624=ADVANCED_FACE('',(#5464),#181,.T.);
#30625=ADVANCED_FACE('',(#5465),#182,.T.);
#30626=ADVANCED_FACE('',(#5466),#183,.T.);
#30627=ADVANCED_FACE('',(#5467),#184,.T.);
#30628=ADVANCED_FACE('',(#5468),#185,.T.);
#30629=ADVANCED_FACE('',(#5469),#186,.T.);
#30630=ADVANCED_FACE('',(#5470),#187,.T.);
#30631=ADVANCED_FACE('',(#5471),#188,.T.);
#30632=ADVANCED_FACE('',(#5472),#189,.T.);
#30633=ADVANCED_FACE('',(#5473),#190,.T.);
#30634=ADVANCED_FACE('',(#5474),#191,.T.);
#30635=ADVANCED_FACE('',(#5475),#192,.T.);
#30636=ADVANCED_FACE('',(#5476),#193,.T.);
#30637=ADVANCED_FACE('',(#5477),#194,.T.);
#30638=ADVANCED_FACE('',(#5478),#195,.T.);
#30639=ADVANCED_FACE('',(#5479),#196,.T.);
#30640=ADVANCED_FACE('',(#5480),#197,.T.);
#30641=ADVANCED_FACE('',(#5481),#198,.T.);
#30642=ADVANCED_FACE('',(#5482),#199,.T.);
#30643=ADVANCED_FACE('',(#5483),#200,.T.);
#30644=ADVANCED_FACE('',(#5484),#201,.T.);
#30645=ADVANCED_FACE('',(#5485),#202,.T.);
#30646=ADVANCED_FACE('',(#5486),#203,.T.);
#30647=ADVANCED_FACE('',(#5487),#204,.T.);
#30648=ADVANCED_FACE('',(#5488),#205,.T.);
#30649=ADVANCED_FACE('',(#5489),#206,.T.);
#30650=ADVANCED_FACE('',(#5490),#207,.T.);
#30651=ADVANCED_FACE('',(#5491),#208,.T.);
#30652=ADVANCED_FACE('',(#5492),#209,.T.);
#30653=ADVANCED_FACE('',(#5493),#210,.T.);
#30654=ADVANCED_FACE('',(#5494),#29784,.T.);
#30655=ADVANCED_FACE('',(#5495,#3394),#29785,.T.);
#30656=ADVANCED_FACE('',(#5496),#211,.T.);
#30657=ADVANCED_FACE('',(#5497),#4626,.T.);
#30658=ADVANCED_FACE('',(#5498),#212,.T.);
#30659=ADVANCED_FACE('',(#5499,#3395),#29786,.T.);
#30660=ADVANCED_FACE('',(#5500),#29787,.T.);
#30661=ADVANCED_FACE('',(#5501),#29788,.F.);
#30662=ADVANCED_FACE('',(#5502),#29789,.F.);
#30663=ADVANCED_FACE('',(#5503),#29790,.F.);
#30664=ADVANCED_FACE('',(#5504),#29791,.F.);
#30665=ADVANCED_FACE('',(#5505),#29792,.F.);
#30666=ADVANCED_FACE('',(#5506),#29793,.F.);
#30667=ADVANCED_FACE('',(#5507),#43,.T.);
#30668=ADVANCED_FACE('',(#5508),#44,.T.);
#30669=ADVANCED_FACE('',(#5509),#2961,.T.);
#30670=ADVANCED_FACE('',(#5510),#29794,.F.);
#30671=ADVANCED_FACE('',(#5511),#4627,.F.);
#30672=ADVANCED_FACE('',(#5512),#29795,.F.);
#30673=ADVANCED_FACE('',(#5513),#29796,.F.);
#30674=ADVANCED_FACE('',(#5514),#4628,.F.);
#30675=ADVANCED_FACE('',(#5515),#29797,.F.);
#30676=ADVANCED_FACE('',(#5516),#29798,.F.);
#30677=ADVANCED_FACE('',(#5517),#4629,.F.);
#30678=ADVANCED_FACE('',(#5518),#29799,.F.);
#30679=ADVANCED_FACE('',(#5519),#29800,.F.);
#30680=ADVANCED_FACE('',(#5520),#4630,.F.);
#30681=ADVANCED_FACE('',(#5521),#29801,.F.);
#30682=ADVANCED_FACE('',(#5522),#29802,.F.);
#30683=ADVANCED_FACE('',(#5523),#4631,.F.);
#30684=ADVANCED_FACE('',(#5524),#29803,.F.);
#30685=ADVANCED_FACE('',(#5525),#29804,.F.);
#30686=ADVANCED_FACE('',(#5526),#4632,.F.);
#30687=ADVANCED_FACE('',(#5527),#29805,.F.);
#30688=ADVANCED_FACE('',(#5528),#29806,.F.);
#30689=ADVANCED_FACE('',(#5529),#4633,.F.);
#30690=ADVANCED_FACE('',(#5530),#29807,.F.);
#30691=ADVANCED_FACE('',(#5531),#29808,.F.);
#30692=ADVANCED_FACE('',(#5532),#29809,.F.);
#30693=ADVANCED_FACE('',(#5533),#29810,.F.);
#30694=ADVANCED_FACE('',(#5534),#29811,.F.);
#30695=ADVANCED_FACE('',(#5535),#29812,.F.);
#30696=ADVANCED_FACE('',(#5536),#29813,.F.);
#30697=ADVANCED_FACE('',(#5537),#29814,.F.);
#30698=ADVANCED_FACE('',(#5538),#29815,.F.);
#30699=ADVANCED_FACE('',(#5539),#29816,.F.);
#30700=ADVANCED_FACE('',(#5540),#29817,.F.);
#30701=ADVANCED_FACE('',(#5541),#29818,.F.);
#30702=ADVANCED_FACE('',(#5542),#29819,.F.);
#30703=ADVANCED_FACE('',(#5543),#29820,.F.);
#30704=ADVANCED_FACE('',(#5544),#29821,.F.);
#30705=ADVANCED_FACE('',(#5545),#29822,.F.);
#30706=ADVANCED_FACE('',(#5546),#29823,.F.);
#30707=ADVANCED_FACE('',(#5547),#29824,.F.);
#30708=ADVANCED_FACE('',(#5548),#29825,.F.);
#30709=ADVANCED_FACE('',(#5549),#29826,.F.);
#30710=ADVANCED_FACE('',(#5550),#4634,.F.);
#30711=ADVANCED_FACE('',(#5551),#29827,.F.);
#30712=ADVANCED_FACE('',(#5552),#29828,.F.);
#30713=ADVANCED_FACE('',(#5553),#4635,.F.);
#30714=ADVANCED_FACE('',(#5554),#29829,.F.);
#30715=ADVANCED_FACE('',(#5555),#29830,.F.);
#30716=ADVANCED_FACE('',(#5556),#4636,.F.);
#30717=ADVANCED_FACE('',(#5557),#29831,.F.);
#30718=ADVANCED_FACE('',(#5558),#29832,.F.);
#30719=ADVANCED_FACE('',(#5559),#4637,.F.);
#30720=ADVANCED_FACE('',(#5560),#29833,.F.);
#30721=ADVANCED_FACE('',(#5561),#29834,.F.);
#30722=ADVANCED_FACE('',(#5562),#4638,.F.);
#30723=ADVANCED_FACE('',(#5563),#29835,.F.);
#30724=ADVANCED_FACE('',(#5564),#29836,.F.);
#30725=ADVANCED_FACE('',(#5565),#4639,.F.);
#30726=ADVANCED_FACE('',(#5566),#29837,.F.);
#30727=ADVANCED_FACE('',(#5567),#29838,.F.);
#30728=ADVANCED_FACE('',(#5568),#4640,.F.);
#30729=ADVANCED_FACE('',(#5569),#29839,.F.);
#30730=ADVANCED_FACE('',(#5570),#29840,.F.);
#30731=ADVANCED_FACE('',(#5571),#4641,.F.);
#30732=ADVANCED_FACE('',(#5572),#29841,.F.);
#30733=ADVANCED_FACE('',(#5573),#29842,.F.);
#30734=ADVANCED_FACE('',(#5574),#4642,.F.);
#30735=ADVANCED_FACE('',(#5575),#29843,.F.);
#30736=ADVANCED_FACE('',(#5576),#29844,.F.);
#30737=ADVANCED_FACE('',(#5577),#4643,.F.);
#30738=ADVANCED_FACE('',(#5578),#29845,.F.);
#30739=ADVANCED_FACE('',(#5579),#29846,.F.);
#30740=ADVANCED_FACE('',(#5580),#4644,.F.);
#30741=ADVANCED_FACE('',(#5581),#29847,.F.);
#30742=ADVANCED_FACE('',(#5582),#29848,.F.);
#30743=ADVANCED_FACE('',(#5583),#4645,.F.);
#30744=ADVANCED_FACE('',(#5584),#29849,.F.);
#30745=ADVANCED_FACE('',(#5585),#29850,.F.);
#30746=ADVANCED_FACE('',(#5586),#4646,.F.);
#30747=ADVANCED_FACE('',(#5587),#29851,.F.);
#30748=ADVANCED_FACE('',(#5588),#29852,.F.);
#30749=ADVANCED_FACE('',(#5589),#4647,.F.);
#30750=ADVANCED_FACE('',(#5590),#29853,.F.);
#30751=ADVANCED_FACE('',(#5591),#29854,.F.);
#30752=ADVANCED_FACE('',(#5592),#4648,.F.);
#30753=ADVANCED_FACE('',(#5593),#29855,.F.);
#30754=ADVANCED_FACE('',(#5594),#29856,.F.);
#30755=ADVANCED_FACE('',(#5595),#4649,.F.);
#30756=ADVANCED_FACE('',(#5596),#29857,.F.);
#30757=ADVANCED_FACE('',(#5597),#29858,.F.);
#30758=ADVANCED_FACE('',(#5598),#4650,.F.);
#30759=ADVANCED_FACE('',(#5599),#29859,.F.);
#30760=ADVANCED_FACE('',(#5600),#29860,.F.);
#30761=ADVANCED_FACE('',(#5601),#4651,.F.);
#30762=ADVANCED_FACE('',(#5602),#29861,.F.);
#30763=ADVANCED_FACE('',(#5603),#29862,.F.);
#30764=ADVANCED_FACE('',(#5604),#4652,.F.);
#30765=ADVANCED_FACE('',(#5605),#29863,.F.);
#30766=ADVANCED_FACE('',(#5606),#29864,.F.);
#30767=ADVANCED_FACE('',(#5607),#4653,.F.);
#30768=ADVANCED_FACE('',(#5608),#29865,.F.);
#30769=ADVANCED_FACE('',(#5609),#29866,.F.);
#30770=ADVANCED_FACE('',(#5610),#4654,.F.);
#30771=ADVANCED_FACE('',(#5611),#29867,.F.);
#30772=ADVANCED_FACE('',(#5612),#29868,.F.);
#30773=ADVANCED_FACE('',(#5613),#4655,.F.);
#30774=ADVANCED_FACE('',(#5614),#29869,.F.);
#30775=ADVANCED_FACE('',(#5615),#29870,.F.);
#30776=ADVANCED_FACE('',(#5616),#4656,.F.);
#30777=ADVANCED_FACE('',(#5617),#29871,.F.);
#30778=ADVANCED_FACE('',(#5618),#29872,.F.);
#30779=ADVANCED_FACE('',(#5619),#4657,.F.);
#30780=ADVANCED_FACE('',(#5620),#29873,.F.);
#30781=ADVANCED_FACE('',(#5621),#29874,.F.);
#30782=ADVANCED_FACE('',(#5622),#4658,.F.);
#30783=ADVANCED_FACE('',(#5623),#29875,.F.);
#30784=ADVANCED_FACE('',(#5624),#29876,.F.);
#30785=ADVANCED_FACE('',(#5625),#4659,.F.);
#30786=ADVANCED_FACE('',(#5626),#29877,.F.);
#30787=ADVANCED_FACE('',(#5627),#29878,.F.);
#30788=ADVANCED_FACE('',(#5628),#4660,.F.);
#30789=ADVANCED_FACE('',(#5629),#29879,.F.);
#30790=ADVANCED_FACE('',(#5630),#29880,.F.);
#30791=ADVANCED_FACE('',(#5631),#4661,.F.);
#30792=ADVANCED_FACE('',(#5632),#29881,.F.);
#30793=ADVANCED_FACE('',(#5633),#29882,.F.);
#30794=ADVANCED_FACE('',(#5634),#4662,.F.);
#30795=ADVANCED_FACE('',(#5635),#29883,.F.);
#30796=ADVANCED_FACE('',(#5636),#29884,.F.);
#30797=ADVANCED_FACE('',(#5637),#4663,.F.);
#30798=ADVANCED_FACE('',(#5638),#29885,.F.);
#30799=ADVANCED_FACE('',(#5639),#29886,.F.);
#30800=ADVANCED_FACE('',(#5640),#4664,.F.);
#30801=ADVANCED_FACE('',(#5641),#29887,.F.);
#30802=ADVANCED_FACE('',(#5642),#29888,.F.);
#30803=ADVANCED_FACE('',(#5643),#4665,.F.);
#30804=ADVANCED_FACE('',(#5644),#29889,.F.);
#30805=ADVANCED_FACE('',(#5645),#29890,.F.);
#30806=ADVANCED_FACE('',(#5646),#4666,.F.);
#30807=ADVANCED_FACE('',(#5647),#29891,.F.);
#30808=ADVANCED_FACE('',(#5648),#29892,.F.);
#30809=ADVANCED_FACE('',(#5649),#4667,.F.);
#30810=ADVANCED_FACE('',(#5650),#29893,.F.);
#30811=ADVANCED_FACE('',(#5651),#29894,.F.);
#30812=ADVANCED_FACE('',(#5652),#4668,.F.);
#30813=ADVANCED_FACE('',(#5653),#29895,.F.);
#30814=ADVANCED_FACE('',(#5654),#29896,.F.);
#30815=ADVANCED_FACE('',(#5655),#4669,.F.);
#30816=ADVANCED_FACE('',(#5656),#29897,.F.);
#30817=ADVANCED_FACE('',(#5657),#29898,.F.);
#30818=ADVANCED_FACE('',(#5658),#4670,.F.);
#30819=ADVANCED_FACE('',(#5659),#29899,.F.);
#30820=ADVANCED_FACE('',(#5660),#29900,.F.);
#30821=ADVANCED_FACE('',(#5661),#4671,.F.);
#30822=ADVANCED_FACE('',(#5662),#29901,.F.);
#30823=ADVANCED_FACE('',(#5663),#29902,.F.);
#30824=ADVANCED_FACE('',(#5664),#4672,.F.);
#30825=ADVANCED_FACE('',(#5665),#29903,.F.);
#30826=ADVANCED_FACE('',(#5666),#29904,.F.);
#30827=ADVANCED_FACE('',(#5667),#4673,.F.);
#30828=ADVANCED_FACE('',(#5668),#29905,.F.);
#30829=ADVANCED_FACE('',(#5669),#29906,.F.);
#30830=ADVANCED_FACE('',(#5670),#4674,.F.);
#30831=ADVANCED_FACE('',(#5671),#29907,.F.);
#30832=ADVANCED_FACE('',(#5672),#29908,.F.);
#30833=ADVANCED_FACE('',(#5673),#4675,.F.);
#30834=ADVANCED_FACE('',(#5674),#29909,.F.);
#30835=ADVANCED_FACE('',(#5675),#29910,.F.);
#30836=ADVANCED_FACE('',(#5676),#4676,.F.);
#30837=ADVANCED_FACE('',(#5677),#29911,.F.);
#30838=ADVANCED_FACE('',(#5678),#29912,.F.);
#30839=ADVANCED_FACE('',(#5679),#4677,.F.);
#30840=ADVANCED_FACE('',(#5680),#29913,.F.);
#30841=ADVANCED_FACE('',(#5681),#29914,.F.);
#30842=ADVANCED_FACE('',(#5682),#4678,.F.);
#30843=ADVANCED_FACE('',(#5683),#29915,.F.);
#30844=ADVANCED_FACE('',(#5684),#29916,.F.);
#30845=ADVANCED_FACE('',(#5685),#4679,.F.);
#30846=ADVANCED_FACE('',(#5686),#29917,.F.);
#30847=ADVANCED_FACE('',(#5687),#29918,.F.);
#30848=ADVANCED_FACE('',(#5688),#4680,.F.);
#30849=ADVANCED_FACE('',(#5689),#29919,.F.);
#30850=ADVANCED_FACE('',(#5690),#29920,.F.);
#30851=ADVANCED_FACE('',(#5691),#4681,.F.);
#30852=ADVANCED_FACE('',(#5692),#29921,.F.);
#30853=ADVANCED_FACE('',(#5693),#29922,.F.);
#30854=ADVANCED_FACE('',(#5694),#4682,.F.);
#30855=ADVANCED_FACE('',(#5695),#29923,.F.);
#30856=ADVANCED_FACE('',(#5696),#29924,.F.);
#30857=ADVANCED_FACE('',(#5697),#4683,.F.);
#30858=ADVANCED_FACE('',(#5698),#29925,.F.);
#30859=ADVANCED_FACE('',(#5699),#29926,.F.);
#30860=ADVANCED_FACE('',(#5700),#4684,.F.);
#30861=ADVANCED_FACE('',(#5701),#29927,.F.);
#30862=ADVANCED_FACE('',(#5702),#29928,.F.);
#30863=ADVANCED_FACE('',(#5703),#4685,.F.);
#30864=ADVANCED_FACE('',(#5704),#29929,.F.);
#30865=ADVANCED_FACE('',(#5705),#29930,.F.);
#30866=ADVANCED_FACE('',(#5706),#4686,.F.);
#30867=ADVANCED_FACE('',(#5707),#29931,.F.);
#30868=ADVANCED_FACE('',(#5708),#29932,.F.);
#30869=ADVANCED_FACE('',(#5709),#4687,.F.);
#30870=ADVANCED_FACE('',(#5710),#29933,.F.);
#30871=ADVANCED_FACE('',(#5711),#29934,.F.);
#30872=ADVANCED_FACE('',(#5712),#4688,.F.);
#30873=ADVANCED_FACE('',(#5713),#29935,.F.);
#30874=ADVANCED_FACE('',(#5714),#29936,.F.);
#30875=ADVANCED_FACE('',(#5715),#4689,.F.);
#30876=ADVANCED_FACE('',(#5716),#29937,.F.);
#30877=ADVANCED_FACE('',(#5717),#29938,.F.);
#30878=ADVANCED_FACE('',(#5718),#4690,.F.);
#30879=ADVANCED_FACE('',(#5719),#29939,.F.);
#30880=ADVANCED_FACE('',(#5720),#29940,.F.);
#30881=ADVANCED_FACE('',(#5721),#4691,.F.);
#30882=ADVANCED_FACE('',(#5722),#29941,.F.);
#30883=ADVANCED_FACE('',(#5723),#29942,.F.);
#30884=ADVANCED_FACE('',(#5724),#29943,.F.);
#30885=ADVANCED_FACE('',(#5725),#29944,.F.);
#30886=ADVANCED_FACE('',(#5726),#29945,.F.);
#30887=ADVANCED_FACE('',(#5727),#29946,.F.);
#30888=ADVANCED_FACE('',(#5728),#29947,.F.);
#30889=ADVANCED_FACE('',(#5729),#29948,.F.);
#30890=ADVANCED_FACE('',(#5730),#29949,.F.);
#30891=ADVANCED_FACE('',(#5731),#29950,.F.);
#30892=ADVANCED_FACE('',(#5732),#29951,.F.);
#30893=ADVANCED_FACE('',(#5733),#29952,.F.);
#30894=ADVANCED_FACE('',(#5734),#29953,.F.);
#30895=ADVANCED_FACE('',(#5735),#4692,.T.);
#30896=ADVANCED_FACE('',(#5736),#4693,.T.);
#30897=ADVANCED_FACE('',(#5737),#4694,.T.);
#30898=ADVANCED_FACE('',(#5738),#4695,.T.);
#30899=ADVANCED_FACE('',(#5739),#4696,.T.);
#30900=ADVANCED_FACE('',(#5740),#4697,.T.);
#30901=ADVANCED_FACE('',(#5741),#4698,.T.);
#30902=ADVANCED_FACE('',(#5742),#4699,.T.);
#30903=ADVANCED_FACE('',(#5743),#4700,.T.);
#30904=ADVANCED_FACE('',(#5744),#4701,.T.);
#30905=ADVANCED_FACE('',(#5745),#4702,.T.);
#30906=ADVANCED_FACE('',(#5746),#4703,.T.);
#30907=ADVANCED_FACE('',(#5747),#4704,.T.);
#30908=ADVANCED_FACE('',(#5748),#4705,.T.);
#30909=ADVANCED_FACE('',(#5749),#4706,.T.);
#30910=ADVANCED_FACE('',(#5750),#4707,.T.);
#30911=ADVANCED_FACE('',(#5751),#4708,.T.);
#30912=ADVANCED_FACE('',(#5752),#4709,.T.);
#30913=ADVANCED_FACE('',(#5753),#4710,.T.);
#30914=ADVANCED_FACE('',(#5754),#4711,.T.);
#30915=ADVANCED_FACE('',(#5755),#4712,.T.);
#30916=ADVANCED_FACE('',(#5756),#4713,.T.);
#30917=ADVANCED_FACE('',(#5757),#4714,.T.);
#30918=ADVANCED_FACE('',(#5758),#4715,.T.);
#30919=ADVANCED_FACE('',(#5759),#4716,.T.);
#30920=ADVANCED_FACE('',(#5760),#4717,.T.);
#30921=ADVANCED_FACE('',(#5761),#4718,.T.);
#30922=ADVANCED_FACE('',(#5762),#4719,.T.);
#30923=ADVANCED_FACE('',(#5763),#2962,.T.);
#30924=ADVANCED_FACE('',(#5764),#4720,.T.);
#30925=ADVANCED_FACE('',(#5765),#4721,.T.);
#30926=ADVANCED_FACE('',(#5766),#4722,.T.);
#30927=ADVANCED_FACE('',(#5767),#4723,.T.);
#30928=ADVANCED_FACE('',(#5768),#4724,.T.);
#30929=ADVANCED_FACE('',(#5769),#4725,.T.);
#30930=ADVANCED_FACE('',(#5770),#4726,.T.);
#30931=ADVANCED_FACE('',(#5771),#4727,.T.);
#30932=ADVANCED_FACE('',(#5772),#4728,.T.);
#30933=ADVANCED_FACE('',(#5773),#4729,.T.);
#30934=ADVANCED_FACE('',(#5774),#4730,.T.);
#30935=ADVANCED_FACE('',(#5775),#4731,.T.);
#30936=ADVANCED_FACE('',(#5776),#4732,.T.);
#30937=ADVANCED_FACE('',(#5777),#4733,.T.);
#30938=ADVANCED_FACE('',(#5778),#4734,.T.);
#30939=ADVANCED_FACE('',(#5779),#4735,.T.);
#30940=ADVANCED_FACE('',(#5780),#4736,.T.);
#30941=ADVANCED_FACE('',(#5781),#4737,.T.);
#30942=ADVANCED_FACE('',(#5782),#4738,.T.);
#30943=ADVANCED_FACE('',(#5783),#4739,.T.);
#30944=ADVANCED_FACE('',(#5784),#4740,.T.);
#30945=ADVANCED_FACE('',(#5785),#4741,.T.);
#30946=ADVANCED_FACE('',(#5786),#4742,.T.);
#30947=ADVANCED_FACE('',(#5787),#4743,.T.);
#30948=ADVANCED_FACE('',(#5788),#4744,.T.);
#30949=ADVANCED_FACE('',(#5789),#4745,.T.);
#30950=ADVANCED_FACE('',(#5790),#4746,.T.);
#30951=ADVANCED_FACE('',(#5791),#4747,.T.);
#30952=ADVANCED_FACE('',(#5792),#4748,.T.);
#30953=ADVANCED_FACE('',(#5793),#4749,.T.);
#30954=ADVANCED_FACE('',(#5794),#4750,.T.);
#30955=ADVANCED_FACE('',(#5795),#2963,.T.);
#30956=ADVANCED_FACE('',(#5796),#4751,.T.);
#30957=ADVANCED_FACE('',(#5797),#4752,.F.);
#30958=ADVANCED_FACE('',(#5798),#4753,.F.);
#30959=ADVANCED_FACE('',(#5799),#4754,.F.);
#30960=ADVANCED_FACE('',(#5800),#4755,.F.);
#30961=ADVANCED_FACE('',(#5801),#4756,.F.);
#30962=ADVANCED_FACE('',(#5802),#4757,.F.);
#30963=ADVANCED_FACE('',(#5803),#4758,.F.);
#30964=ADVANCED_FACE('',(#5804),#4759,.F.);
#30965=ADVANCED_FACE('',(#5805),#4760,.F.);
#30966=ADVANCED_FACE('',(#5806),#4761,.F.);
#30967=ADVANCED_FACE('',(#5807),#4762,.F.);
#30968=ADVANCED_FACE('',(#5808),#4763,.F.);
#30969=ADVANCED_FACE('',(#5809),#4764,.F.);
#30970=ADVANCED_FACE('',(#5810),#4765,.F.);
#30971=ADVANCED_FACE('',(#5811),#4766,.F.);
#30972=ADVANCED_FACE('',(#5812),#2964,.F.);
#30973=ADVANCED_FACE('',(#5813),#213,.T.);
#30974=ADVANCED_FACE('',(#5814),#2965,.T.);
#30975=ADVANCED_FACE('',(#5815),#2966,.T.);
#30976=ADVANCED_FACE('',(#5816),#214,.F.);
#30977=ADVANCED_FACE('',(#5817),#4767,.T.);
#30978=ADVANCED_FACE('',(#5818),#215,.T.);
#30979=ADVANCED_FACE('',(#5819),#216,.F.);
#30980=ADVANCED_FACE('',(#5820),#217,.T.);
#30981=ADVANCED_FACE('',(#5821),#218,.T.);
#30982=ADVANCED_FACE('',(#5822),#219,.T.);
#30983=ADVANCED_FACE('',(#5823),#220,.T.);
#30984=ADVANCED_FACE('',(#5824),#221,.T.);
#30985=ADVANCED_FACE('',(#5825),#222,.T.);
#30986=ADVANCED_FACE('',(#5826),#223,.T.);
#30987=ADVANCED_FACE('',(#5827),#224,.T.);
#30988=ADVANCED_FACE('',(#5828),#225,.T.);
#30989=ADVANCED_FACE('',(#5829),#226,.T.);
#30990=ADVANCED_FACE('',(#5830),#227,.T.);
#30991=ADVANCED_FACE('',(#5831),#228,.T.);
#30992=ADVANCED_FACE('',(#5832),#229,.T.);
#30993=ADVANCED_FACE('',(#5833),#230,.T.);
#30994=ADVANCED_FACE('',(#5834),#231,.T.);
#30995=ADVANCED_FACE('',(#5835),#232,.T.);
#30996=ADVANCED_FACE('',(#5836),#233,.T.);
#30997=ADVANCED_FACE('',(#5837),#234,.T.);
#30998=ADVANCED_FACE('',(#5838),#235,.T.);
#30999=ADVANCED_FACE('',(#5839),#236,.T.);
#31000=ADVANCED_FACE('',(#5840),#237,.T.);
#31001=ADVANCED_FACE('',(#5841),#238,.T.);
#31002=ADVANCED_FACE('',(#5842),#239,.T.);
#31003=ADVANCED_FACE('',(#5843),#240,.T.);
#31004=ADVANCED_FACE('',(#5844),#241,.T.);
#31005=ADVANCED_FACE('',(#5845),#242,.T.);
#31006=ADVANCED_FACE('',(#5846),#243,.T.);
#31007=ADVANCED_FACE('',(#5847),#244,.T.);
#31008=ADVANCED_FACE('',(#5848),#245,.T.);
#31009=ADVANCED_FACE('',(#5849),#246,.T.);
#31010=ADVANCED_FACE('',(#5850),#247,.T.);
#31011=ADVANCED_FACE('',(#5851),#248,.T.);
#31012=ADVANCED_FACE('',(#5852),#249,.T.);
#31013=ADVANCED_FACE('',(#5853),#250,.T.);
#31014=ADVANCED_FACE('',(#5854),#251,.T.);
#31015=ADVANCED_FACE('',(#5855),#252,.T.);
#31016=ADVANCED_FACE('',(#5856),#253,.T.);
#31017=ADVANCED_FACE('',(#5857),#254,.T.);
#31018=ADVANCED_FACE('',(#5858),#255,.T.);
#31019=ADVANCED_FACE('',(#5859),#256,.T.);
#31020=ADVANCED_FACE('',(#5860),#257,.T.);
#31021=ADVANCED_FACE('',(#5861),#258,.T.);
#31022=ADVANCED_FACE('',(#5862),#259,.T.);
#31023=ADVANCED_FACE('',(#5863),#260,.T.);
#31024=ADVANCED_FACE('',(#5864),#261,.T.);
#31025=ADVANCED_FACE('',(#5865),#262,.T.);
#31026=ADVANCED_FACE('',(#5866),#263,.T.);
#31027=ADVANCED_FACE('',(#5867),#264,.T.);
#31028=ADVANCED_FACE('',(#5868),#265,.T.);
#31029=ADVANCED_FACE('',(#5869),#266,.T.);
#31030=ADVANCED_FACE('',(#5870),#267,.T.);
#31031=ADVANCED_FACE('',(#5871),#268,.T.);
#31032=ADVANCED_FACE('',(#5872),#269,.T.);
#31033=ADVANCED_FACE('',(#5873),#270,.T.);
#31034=ADVANCED_FACE('',(#5874),#271,.T.);
#31035=ADVANCED_FACE('',(#5875),#272,.T.);
#31036=ADVANCED_FACE('',(#5876),#273,.T.);
#31037=ADVANCED_FACE('',(#5877),#274,.T.);
#31038=ADVANCED_FACE('',(#5878),#275,.T.);
#31039=ADVANCED_FACE('',(#5879),#276,.T.);
#31040=ADVANCED_FACE('',(#5880),#277,.T.);
#31041=ADVANCED_FACE('',(#5881),#278,.T.);
#31042=ADVANCED_FACE('',(#5882),#279,.T.);
#31043=ADVANCED_FACE('',(#5883),#280,.T.);
#31044=ADVANCED_FACE('',(#5884),#281,.T.);
#31045=ADVANCED_FACE('',(#5885),#282,.T.);
#31046=ADVANCED_FACE('',(#5886),#283,.T.);
#31047=ADVANCED_FACE('',(#5887),#284,.T.);
#31048=ADVANCED_FACE('',(#5888),#285,.T.);
#31049=ADVANCED_FACE('',(#5889),#286,.T.);
#31050=ADVANCED_FACE('',(#5890),#287,.T.);
#31051=ADVANCED_FACE('',(#5891),#288,.T.);
#31052=ADVANCED_FACE('',(#5892),#289,.T.);
#31053=ADVANCED_FACE('',(#5893),#290,.T.);
#31054=ADVANCED_FACE('',(#5894),#291,.T.);
#31055=ADVANCED_FACE('',(#5895),#292,.T.);
#31056=ADVANCED_FACE('',(#5896),#293,.T.);
#31057=ADVANCED_FACE('',(#5897),#294,.T.);
#31058=ADVANCED_FACE('',(#5898),#295,.T.);
#31059=ADVANCED_FACE('',(#5899),#4768,.T.);
#31060=ADVANCED_FACE('',(#5900),#4769,.T.);
#31061=ADVANCED_FACE('',(#5901),#4770,.T.);
#31062=ADVANCED_FACE('',(#5902),#4771,.T.);
#31063=ADVANCED_FACE('',(#5903),#4772,.T.);
#31064=ADVANCED_FACE('',(#5904),#4773,.T.);
#31065=ADVANCED_FACE('',(#5905),#4774,.T.);
#31066=ADVANCED_FACE('',(#5906),#4775,.T.);
#31067=ADVANCED_FACE('',(#5907),#4776,.T.);
#31068=ADVANCED_FACE('',(#5908),#4777,.T.);
#31069=ADVANCED_FACE('',(#5909),#4778,.T.);
#31070=ADVANCED_FACE('',(#5910),#4779,.T.);
#31071=ADVANCED_FACE('',(#5911),#4780,.T.);
#31072=ADVANCED_FACE('',(#5912),#4781,.T.);
#31073=ADVANCED_FACE('',(#5913),#4782,.T.);
#31074=ADVANCED_FACE('',(#5914),#4783,.T.);
#31075=ADVANCED_FACE('',(#5915),#4784,.T.);
#31076=ADVANCED_FACE('',(#5916),#4785,.T.);
#31077=ADVANCED_FACE('',(#5917),#4786,.T.);
#31078=ADVANCED_FACE('',(#5918),#4787,.T.);
#31079=ADVANCED_FACE('',(#5919),#4788,.T.);
#31080=ADVANCED_FACE('',(#5920),#4789,.T.);
#31081=ADVANCED_FACE('',(#5921),#4790,.T.);
#31082=ADVANCED_FACE('',(#5922),#4791,.T.);
#31083=ADVANCED_FACE('',(#5923),#4792,.T.);
#31084=ADVANCED_FACE('',(#5924),#4793,.T.);
#31085=ADVANCED_FACE('',(#5925),#4794,.T.);
#31086=ADVANCED_FACE('',(#5926),#4795,.T.);
#31087=ADVANCED_FACE('',(#5927),#4796,.T.);
#31088=ADVANCED_FACE('',(#5928),#4797,.T.);
#31089=ADVANCED_FACE('',(#5929),#4798,.T.);
#31090=ADVANCED_FACE('',(#5930),#4799,.T.);
#31091=ADVANCED_FACE('',(#5931),#4800,.T.);
#31092=ADVANCED_FACE('',(#5932),#4801,.T.);
#31093=ADVANCED_FACE('',(#5933),#4802,.T.);
#31094=ADVANCED_FACE('',(#5934),#4803,.T.);
#31095=ADVANCED_FACE('',(#5935),#4804,.T.);
#31096=ADVANCED_FACE('',(#5936),#4805,.T.);
#31097=ADVANCED_FACE('',(#5937),#4806,.T.);
#31098=ADVANCED_FACE('',(#5938),#4807,.T.);
#31099=ADVANCED_FACE('',(#5939),#4808,.T.);
#31100=ADVANCED_FACE('',(#5940),#4809,.T.);
#31101=ADVANCED_FACE('',(#5941),#4810,.T.);
#31102=ADVANCED_FACE('',(#5942),#4811,.T.);
#31103=ADVANCED_FACE('',(#5943),#4812,.T.);
#31104=ADVANCED_FACE('',(#5944),#4813,.T.);
#31105=ADVANCED_FACE('',(#5945),#4814,.T.);
#31106=ADVANCED_FACE('',(#5946),#4815,.T.);
#31107=ADVANCED_FACE('',(#5947),#4816,.T.);
#31108=ADVANCED_FACE('',(#5948),#4817,.T.);
#31109=ADVANCED_FACE('',(#5949),#4818,.T.);
#31110=ADVANCED_FACE('',(#5950),#4819,.T.);
#31111=ADVANCED_FACE('',(#5951),#4820,.T.);
#31112=ADVANCED_FACE('',(#5952),#4821,.T.);
#31113=ADVANCED_FACE('',(#5953),#4822,.T.);
#31114=ADVANCED_FACE('',(#5954),#4823,.T.);
#31115=ADVANCED_FACE('',(#5955),#4824,.T.);
#31116=ADVANCED_FACE('',(#5956),#4825,.T.);
#31117=ADVANCED_FACE('',(#5957),#4826,.T.);
#31118=ADVANCED_FACE('',(#5958),#4827,.T.);
#31119=ADVANCED_FACE('',(#5959),#4828,.T.);
#31120=ADVANCED_FACE('',(#5960),#4829,.T.);
#31121=ADVANCED_FACE('',(#5961),#4830,.T.);
#31122=ADVANCED_FACE('',(#5962),#4831,.T.);
#31123=ADVANCED_FACE('',(#5963),#4832,.T.);
#31124=ADVANCED_FACE('',(#5964),#4833,.T.);
#31125=ADVANCED_FACE('',(#5965),#4834,.T.);
#31126=ADVANCED_FACE('',(#5966),#4835,.T.);
#31127=ADVANCED_FACE('',(#5967),#4836,.T.);
#31128=ADVANCED_FACE('',(#5968),#4837,.T.);
#31129=ADVANCED_FACE('',(#5969),#4838,.T.);
#31130=ADVANCED_FACE('',(#5970),#4839,.T.);
#31131=ADVANCED_FACE('',(#5971),#4840,.T.);
#31132=ADVANCED_FACE('',(#5972),#4841,.T.);
#31133=ADVANCED_FACE('',(#5973),#4842,.T.);
#31134=ADVANCED_FACE('',(#5974),#4843,.T.);
#31135=ADVANCED_FACE('',(#5975),#4844,.T.);
#31136=ADVANCED_FACE('',(#5976),#4845,.T.);
#31137=ADVANCED_FACE('',(#5977),#4846,.T.);
#31138=ADVANCED_FACE('',(#5978),#296,.T.);
#31139=ADVANCED_FACE('',(#5979),#297,.T.);
#31140=ADVANCED_FACE('',(#5980),#298,.T.);
#31141=ADVANCED_FACE('',(#5981),#299,.T.);
#31142=ADVANCED_FACE('',(#5982),#300,.T.);
#31143=ADVANCED_FACE('',(#5983),#301,.T.);
#31144=ADVANCED_FACE('',(#5984),#302,.T.);
#31145=ADVANCED_FACE('',(#5985),#303,.T.);
#31146=ADVANCED_FACE('',(#5986),#304,.T.);
#31147=ADVANCED_FACE('',(#5987),#305,.T.);
#31148=ADVANCED_FACE('',(#5988),#306,.T.);
#31149=ADVANCED_FACE('',(#5989),#307,.T.);
#31150=ADVANCED_FACE('',(#5990),#308,.T.);
#31151=ADVANCED_FACE('',(#5991),#309,.T.);
#31152=ADVANCED_FACE('',(#5992),#310,.T.);
#31153=ADVANCED_FACE('',(#5993),#311,.T.);
#31154=ADVANCED_FACE('',(#5994),#312,.T.);
#31155=ADVANCED_FACE('',(#5995),#313,.T.);
#31156=ADVANCED_FACE('',(#5996),#314,.T.);
#31157=ADVANCED_FACE('',(#5997),#315,.T.);
#31158=ADVANCED_FACE('',(#5998),#316,.T.);
#31159=ADVANCED_FACE('',(#5999),#317,.T.);
#31160=ADVANCED_FACE('',(#6000),#318,.T.);
#31161=ADVANCED_FACE('',(#6001),#319,.T.);
#31162=ADVANCED_FACE('',(#6002),#320,.T.);
#31163=ADVANCED_FACE('',(#6003),#321,.T.);
#31164=ADVANCED_FACE('',(#6004),#322,.T.);
#31165=ADVANCED_FACE('',(#6005),#323,.T.);
#31166=ADVANCED_FACE('',(#6006),#324,.T.);
#31167=ADVANCED_FACE('',(#6007),#325,.T.);
#31168=ADVANCED_FACE('',(#6008),#326,.T.);
#31169=ADVANCED_FACE('',(#6009),#327,.T.);
#31170=ADVANCED_FACE('',(#6010),#328,.T.);
#31171=ADVANCED_FACE('',(#6011),#329,.T.);
#31172=ADVANCED_FACE('',(#6012),#330,.T.);
#31173=ADVANCED_FACE('',(#6013),#331,.T.);
#31174=ADVANCED_FACE('',(#6014),#332,.T.);
#31175=ADVANCED_FACE('',(#6015),#333,.T.);
#31176=ADVANCED_FACE('',(#6016),#334,.T.);
#31177=ADVANCED_FACE('',(#6017),#335,.T.);
#31178=ADVANCED_FACE('',(#6018),#336,.T.);
#31179=ADVANCED_FACE('',(#6019),#337,.T.);
#31180=ADVANCED_FACE('',(#6020),#338,.T.);
#31181=ADVANCED_FACE('',(#6021),#339,.T.);
#31182=ADVANCED_FACE('',(#6022),#340,.T.);
#31183=ADVANCED_FACE('',(#6023),#341,.T.);
#31184=ADVANCED_FACE('',(#6024),#342,.T.);
#31185=ADVANCED_FACE('',(#6025),#343,.T.);
#31186=ADVANCED_FACE('',(#6026),#344,.T.);
#31187=ADVANCED_FACE('',(#6027),#345,.T.);
#31188=ADVANCED_FACE('',(#6028),#346,.T.);
#31189=ADVANCED_FACE('',(#6029),#347,.T.);
#31190=ADVANCED_FACE('',(#6030),#348,.T.);
#31191=ADVANCED_FACE('',(#6031),#349,.T.);
#31192=ADVANCED_FACE('',(#6032),#350,.T.);
#31193=ADVANCED_FACE('',(#6033),#351,.T.);
#31194=ADVANCED_FACE('',(#6034),#352,.T.);
#31195=ADVANCED_FACE('',(#6035),#353,.T.);
#31196=ADVANCED_FACE('',(#6036),#354,.T.);
#31197=ADVANCED_FACE('',(#6037),#355,.T.);
#31198=ADVANCED_FACE('',(#6038),#356,.T.);
#31199=ADVANCED_FACE('',(#6039),#357,.T.);
#31200=ADVANCED_FACE('',(#6040),#358,.T.);
#31201=ADVANCED_FACE('',(#6041),#359,.T.);
#31202=ADVANCED_FACE('',(#6042),#360,.T.);
#31203=ADVANCED_FACE('',(#6043),#361,.T.);
#31204=ADVANCED_FACE('',(#6044),#362,.T.);
#31205=ADVANCED_FACE('',(#6045),#363,.T.);
#31206=ADVANCED_FACE('',(#6046),#364,.T.);
#31207=ADVANCED_FACE('',(#6047),#365,.T.);
#31208=ADVANCED_FACE('',(#6048),#366,.T.);
#31209=ADVANCED_FACE('',(#6049),#367,.T.);
#31210=ADVANCED_FACE('',(#6050),#368,.T.);
#31211=ADVANCED_FACE('',(#6051),#369,.T.);
#31212=ADVANCED_FACE('',(#6052),#370,.T.);
#31213=ADVANCED_FACE('',(#6053),#371,.T.);
#31214=ADVANCED_FACE('',(#6054),#372,.T.);
#31215=ADVANCED_FACE('',(#6055),#373,.T.);
#31216=ADVANCED_FACE('',(#6056),#374,.T.);
#31217=ADVANCED_FACE('',(#6057),#29954,.T.);
#31218=ADVANCED_FACE('',(#6058,#3396),#29955,.T.);
#31219=ADVANCED_FACE('',(#6059),#375,.T.);
#31220=ADVANCED_FACE('',(#6060),#4847,.T.);
#31221=ADVANCED_FACE('',(#6061),#376,.T.);
#31222=ADVANCED_FACE('',(#6062,#3397),#29956,.T.);
#31223=ADVANCED_FACE('',(#6063),#29957,.T.);
#31224=ADVANCED_FACE('',(#6064),#29958,.F.);
#31225=ADVANCED_FACE('',(#6065),#29959,.F.);
#31226=ADVANCED_FACE('',(#6066),#29960,.F.);
#31227=ADVANCED_FACE('',(#6067),#29961,.F.);
#31228=ADVANCED_FACE('',(#6068),#29962,.F.);
#31229=ADVANCED_FACE('',(#6069),#29963,.F.);
#31230=ADVANCED_FACE('',(#6070),#45,.T.);
#31231=ADVANCED_FACE('',(#6071),#46,.T.);
#31232=ADVANCED_FACE('',(#6072),#2967,.T.);
#31233=ADVANCED_FACE('',(#6073),#29964,.F.);
#31234=ADVANCED_FACE('',(#6074),#4848,.F.);
#31235=ADVANCED_FACE('',(#6075),#29965,.F.);
#31236=ADVANCED_FACE('',(#6076),#29966,.F.);
#31237=ADVANCED_FACE('',(#6077),#4849,.F.);
#31238=ADVANCED_FACE('',(#6078),#29967,.F.);
#31239=ADVANCED_FACE('',(#6079),#29968,.F.);
#31240=ADVANCED_FACE('',(#6080),#4850,.F.);
#31241=ADVANCED_FACE('',(#6081),#29969,.F.);
#31242=ADVANCED_FACE('',(#6082),#29970,.F.);
#31243=ADVANCED_FACE('',(#6083),#4851,.F.);
#31244=ADVANCED_FACE('',(#6084),#29971,.F.);
#31245=ADVANCED_FACE('',(#6085),#29972,.F.);
#31246=ADVANCED_FACE('',(#6086),#4852,.F.);
#31247=ADVANCED_FACE('',(#6087),#29973,.F.);
#31248=ADVANCED_FACE('',(#6088),#29974,.F.);
#31249=ADVANCED_FACE('',(#6089),#4853,.F.);
#31250=ADVANCED_FACE('',(#6090),#29975,.F.);
#31251=ADVANCED_FACE('',(#6091),#29976,.F.);
#31252=ADVANCED_FACE('',(#6092),#4854,.F.);
#31253=ADVANCED_FACE('',(#6093),#29977,.F.);
#31254=ADVANCED_FACE('',(#6094),#29978,.F.);
#31255=ADVANCED_FACE('',(#6095),#29979,.F.);
#31256=ADVANCED_FACE('',(#6096),#29980,.F.);
#31257=ADVANCED_FACE('',(#6097),#29981,.F.);
#31258=ADVANCED_FACE('',(#6098),#29982,.F.);
#31259=ADVANCED_FACE('',(#6099),#29983,.F.);
#31260=ADVANCED_FACE('',(#6100),#29984,.F.);
#31261=ADVANCED_FACE('',(#6101),#29985,.F.);
#31262=ADVANCED_FACE('',(#6102),#29986,.F.);
#31263=ADVANCED_FACE('',(#6103),#29987,.F.);
#31264=ADVANCED_FACE('',(#6104),#29988,.F.);
#31265=ADVANCED_FACE('',(#6105),#29989,.F.);
#31266=ADVANCED_FACE('',(#6106),#29990,.F.);
#31267=ADVANCED_FACE('',(#6107),#29991,.F.);
#31268=ADVANCED_FACE('',(#6108),#29992,.F.);
#31269=ADVANCED_FACE('',(#6109),#29993,.F.);
#31270=ADVANCED_FACE('',(#6110),#29994,.F.);
#31271=ADVANCED_FACE('',(#6111),#29995,.F.);
#31272=ADVANCED_FACE('',(#6112),#29996,.F.);
#31273=ADVANCED_FACE('',(#6113),#4855,.F.);
#31274=ADVANCED_FACE('',(#6114),#29997,.F.);
#31275=ADVANCED_FACE('',(#6115),#29998,.F.);
#31276=ADVANCED_FACE('',(#6116),#4856,.F.);
#31277=ADVANCED_FACE('',(#6117),#29999,.F.);
#31278=ADVANCED_FACE('',(#6118),#30000,.F.);
#31279=ADVANCED_FACE('',(#6119),#4857,.F.);
#31280=ADVANCED_FACE('',(#6120),#30001,.F.);
#31281=ADVANCED_FACE('',(#6121),#30002,.F.);
#31282=ADVANCED_FACE('',(#6122),#4858,.F.);
#31283=ADVANCED_FACE('',(#6123),#30003,.F.);
#31284=ADVANCED_FACE('',(#6124),#30004,.F.);
#31285=ADVANCED_FACE('',(#6125),#4859,.F.);
#31286=ADVANCED_FACE('',(#6126),#30005,.F.);
#31287=ADVANCED_FACE('',(#6127),#30006,.F.);
#31288=ADVANCED_FACE('',(#6128),#4860,.F.);
#31289=ADVANCED_FACE('',(#6129),#30007,.F.);
#31290=ADVANCED_FACE('',(#6130),#30008,.F.);
#31291=ADVANCED_FACE('',(#6131),#4861,.F.);
#31292=ADVANCED_FACE('',(#6132),#30009,.F.);
#31293=ADVANCED_FACE('',(#6133),#30010,.F.);
#31294=ADVANCED_FACE('',(#6134),#4862,.F.);
#31295=ADVANCED_FACE('',(#6135),#30011,.F.);
#31296=ADVANCED_FACE('',(#6136),#30012,.F.);
#31297=ADVANCED_FACE('',(#6137),#4863,.F.);
#31298=ADVANCED_FACE('',(#6138),#30013,.F.);
#31299=ADVANCED_FACE('',(#6139),#30014,.F.);
#31300=ADVANCED_FACE('',(#6140),#4864,.F.);
#31301=ADVANCED_FACE('',(#6141),#30015,.F.);
#31302=ADVANCED_FACE('',(#6142),#30016,.F.);
#31303=ADVANCED_FACE('',(#6143),#4865,.F.);
#31304=ADVANCED_FACE('',(#6144),#30017,.F.);
#31305=ADVANCED_FACE('',(#6145),#30018,.F.);
#31306=ADVANCED_FACE('',(#6146),#4866,.F.);
#31307=ADVANCED_FACE('',(#6147),#30019,.F.);
#31308=ADVANCED_FACE('',(#6148),#30020,.F.);
#31309=ADVANCED_FACE('',(#6149),#4867,.F.);
#31310=ADVANCED_FACE('',(#6150),#30021,.F.);
#31311=ADVANCED_FACE('',(#6151),#30022,.F.);
#31312=ADVANCED_FACE('',(#6152),#4868,.F.);
#31313=ADVANCED_FACE('',(#6153),#30023,.F.);
#31314=ADVANCED_FACE('',(#6154),#30024,.F.);
#31315=ADVANCED_FACE('',(#6155),#4869,.F.);
#31316=ADVANCED_FACE('',(#6156),#30025,.F.);
#31317=ADVANCED_FACE('',(#6157),#30026,.F.);
#31318=ADVANCED_FACE('',(#6158),#4870,.F.);
#31319=ADVANCED_FACE('',(#6159),#30027,.F.);
#31320=ADVANCED_FACE('',(#6160),#30028,.F.);
#31321=ADVANCED_FACE('',(#6161),#4871,.F.);
#31322=ADVANCED_FACE('',(#6162),#30029,.F.);
#31323=ADVANCED_FACE('',(#6163),#30030,.F.);
#31324=ADVANCED_FACE('',(#6164),#4872,.F.);
#31325=ADVANCED_FACE('',(#6165),#30031,.F.);
#31326=ADVANCED_FACE('',(#6166),#30032,.F.);
#31327=ADVANCED_FACE('',(#6167),#4873,.F.);
#31328=ADVANCED_FACE('',(#6168),#30033,.F.);
#31329=ADVANCED_FACE('',(#6169),#30034,.F.);
#31330=ADVANCED_FACE('',(#6170),#4874,.F.);
#31331=ADVANCED_FACE('',(#6171),#30035,.F.);
#31332=ADVANCED_FACE('',(#6172),#30036,.F.);
#31333=ADVANCED_FACE('',(#6173),#4875,.F.);
#31334=ADVANCED_FACE('',(#6174),#30037,.F.);
#31335=ADVANCED_FACE('',(#6175),#30038,.F.);
#31336=ADVANCED_FACE('',(#6176),#4876,.F.);
#31337=ADVANCED_FACE('',(#6177),#30039,.F.);
#31338=ADVANCED_FACE('',(#6178),#30040,.F.);
#31339=ADVANCED_FACE('',(#6179),#4877,.F.);
#31340=ADVANCED_FACE('',(#6180),#30041,.F.);
#31341=ADVANCED_FACE('',(#6181),#30042,.F.);
#31342=ADVANCED_FACE('',(#6182),#4878,.F.);
#31343=ADVANCED_FACE('',(#6183),#30043,.F.);
#31344=ADVANCED_FACE('',(#6184),#30044,.F.);
#31345=ADVANCED_FACE('',(#6185),#4879,.F.);
#31346=ADVANCED_FACE('',(#6186),#30045,.F.);
#31347=ADVANCED_FACE('',(#6187),#30046,.F.);
#31348=ADVANCED_FACE('',(#6188),#4880,.F.);
#31349=ADVANCED_FACE('',(#6189),#30047,.F.);
#31350=ADVANCED_FACE('',(#6190),#30048,.F.);
#31351=ADVANCED_FACE('',(#6191),#4881,.F.);
#31352=ADVANCED_FACE('',(#6192),#30049,.F.);
#31353=ADVANCED_FACE('',(#6193),#30050,.F.);
#31354=ADVANCED_FACE('',(#6194),#4882,.F.);
#31355=ADVANCED_FACE('',(#6195),#30051,.F.);
#31356=ADVANCED_FACE('',(#6196),#30052,.F.);
#31357=ADVANCED_FACE('',(#6197),#4883,.F.);
#31358=ADVANCED_FACE('',(#6198),#30053,.F.);
#31359=ADVANCED_FACE('',(#6199),#30054,.F.);
#31360=ADVANCED_FACE('',(#6200),#4884,.F.);
#31361=ADVANCED_FACE('',(#6201),#30055,.F.);
#31362=ADVANCED_FACE('',(#6202),#30056,.F.);
#31363=ADVANCED_FACE('',(#6203),#4885,.F.);
#31364=ADVANCED_FACE('',(#6204),#30057,.F.);
#31365=ADVANCED_FACE('',(#6205),#30058,.F.);
#31366=ADVANCED_FACE('',(#6206),#4886,.F.);
#31367=ADVANCED_FACE('',(#6207),#30059,.F.);
#31368=ADVANCED_FACE('',(#6208),#30060,.F.);
#31369=ADVANCED_FACE('',(#6209),#4887,.F.);
#31370=ADVANCED_FACE('',(#6210),#30061,.F.);
#31371=ADVANCED_FACE('',(#6211),#30062,.F.);
#31372=ADVANCED_FACE('',(#6212),#4888,.F.);
#31373=ADVANCED_FACE('',(#6213),#30063,.F.);
#31374=ADVANCED_FACE('',(#6214),#30064,.F.);
#31375=ADVANCED_FACE('',(#6215),#4889,.F.);
#31376=ADVANCED_FACE('',(#6216),#30065,.F.);
#31377=ADVANCED_FACE('',(#6217),#30066,.F.);
#31378=ADVANCED_FACE('',(#6218),#4890,.F.);
#31379=ADVANCED_FACE('',(#6219),#30067,.F.);
#31380=ADVANCED_FACE('',(#6220),#30068,.F.);
#31381=ADVANCED_FACE('',(#6221),#4891,.F.);
#31382=ADVANCED_FACE('',(#6222),#30069,.F.);
#31383=ADVANCED_FACE('',(#6223),#30070,.F.);
#31384=ADVANCED_FACE('',(#6224),#4892,.F.);
#31385=ADVANCED_FACE('',(#6225),#30071,.F.);
#31386=ADVANCED_FACE('',(#6226),#30072,.F.);
#31387=ADVANCED_FACE('',(#6227),#4893,.F.);
#31388=ADVANCED_FACE('',(#6228),#30073,.F.);
#31389=ADVANCED_FACE('',(#6229),#30074,.F.);
#31390=ADVANCED_FACE('',(#6230),#4894,.F.);
#31391=ADVANCED_FACE('',(#6231),#30075,.F.);
#31392=ADVANCED_FACE('',(#6232),#30076,.F.);
#31393=ADVANCED_FACE('',(#6233),#4895,.F.);
#31394=ADVANCED_FACE('',(#6234),#30077,.F.);
#31395=ADVANCED_FACE('',(#6235),#30078,.F.);
#31396=ADVANCED_FACE('',(#6236),#4896,.F.);
#31397=ADVANCED_FACE('',(#6237),#30079,.F.);
#31398=ADVANCED_FACE('',(#6238),#30080,.F.);
#31399=ADVANCED_FACE('',(#6239),#4897,.F.);
#31400=ADVANCED_FACE('',(#6240),#30081,.F.);
#31401=ADVANCED_FACE('',(#6241),#30082,.F.);
#31402=ADVANCED_FACE('',(#6242),#4898,.F.);
#31403=ADVANCED_FACE('',(#6243),#30083,.F.);
#31404=ADVANCED_FACE('',(#6244),#30084,.F.);
#31405=ADVANCED_FACE('',(#6245),#4899,.F.);
#31406=ADVANCED_FACE('',(#6246),#30085,.F.);
#31407=ADVANCED_FACE('',(#6247),#30086,.F.);
#31408=ADVANCED_FACE('',(#6248),#4900,.F.);
#31409=ADVANCED_FACE('',(#6249),#30087,.F.);
#31410=ADVANCED_FACE('',(#6250),#30088,.F.);
#31411=ADVANCED_FACE('',(#6251),#4901,.F.);
#31412=ADVANCED_FACE('',(#6252),#30089,.F.);
#31413=ADVANCED_FACE('',(#6253),#30090,.F.);
#31414=ADVANCED_FACE('',(#6254),#4902,.F.);
#31415=ADVANCED_FACE('',(#6255),#30091,.F.);
#31416=ADVANCED_FACE('',(#6256),#30092,.F.);
#31417=ADVANCED_FACE('',(#6257),#4903,.F.);
#31418=ADVANCED_FACE('',(#6258),#30093,.F.);
#31419=ADVANCED_FACE('',(#6259),#30094,.F.);
#31420=ADVANCED_FACE('',(#6260),#4904,.F.);
#31421=ADVANCED_FACE('',(#6261),#30095,.F.);
#31422=ADVANCED_FACE('',(#6262),#30096,.F.);
#31423=ADVANCED_FACE('',(#6263),#4905,.F.);
#31424=ADVANCED_FACE('',(#6264),#30097,.F.);
#31425=ADVANCED_FACE('',(#6265),#30098,.F.);
#31426=ADVANCED_FACE('',(#6266),#4906,.F.);
#31427=ADVANCED_FACE('',(#6267),#30099,.F.);
#31428=ADVANCED_FACE('',(#6268),#30100,.F.);
#31429=ADVANCED_FACE('',(#6269),#4907,.F.);
#31430=ADVANCED_FACE('',(#6270),#30101,.F.);
#31431=ADVANCED_FACE('',(#6271),#30102,.F.);
#31432=ADVANCED_FACE('',(#6272),#4908,.F.);
#31433=ADVANCED_FACE('',(#6273),#30103,.F.);
#31434=ADVANCED_FACE('',(#6274),#30104,.F.);
#31435=ADVANCED_FACE('',(#6275),#4909,.F.);
#31436=ADVANCED_FACE('',(#6276),#30105,.F.);
#31437=ADVANCED_FACE('',(#6277),#30106,.F.);
#31438=ADVANCED_FACE('',(#6278),#4910,.F.);
#31439=ADVANCED_FACE('',(#6279),#30107,.F.);
#31440=ADVANCED_FACE('',(#6280),#30108,.F.);
#31441=ADVANCED_FACE('',(#6281),#4911,.F.);
#31442=ADVANCED_FACE('',(#6282),#30109,.F.);
#31443=ADVANCED_FACE('',(#6283),#30110,.F.);
#31444=ADVANCED_FACE('',(#6284),#4912,.F.);
#31445=ADVANCED_FACE('',(#6285),#30111,.F.);
#31446=ADVANCED_FACE('',(#6286),#30112,.F.);
#31447=ADVANCED_FACE('',(#6287),#30113,.F.);
#31448=ADVANCED_FACE('',(#6288),#30114,.F.);
#31449=ADVANCED_FACE('',(#6289),#30115,.F.);
#31450=ADVANCED_FACE('',(#6290),#30116,.F.);
#31451=ADVANCED_FACE('',(#6291),#30117,.F.);
#31452=ADVANCED_FACE('',(#6292),#30118,.F.);
#31453=ADVANCED_FACE('',(#6293),#30119,.F.);
#31454=ADVANCED_FACE('',(#6294),#30120,.F.);
#31455=ADVANCED_FACE('',(#6295),#30121,.F.);
#31456=ADVANCED_FACE('',(#6296),#30122,.F.);
#31457=ADVANCED_FACE('',(#6297),#30123,.F.);
#31458=ADVANCED_FACE('',(#6298),#4913,.T.);
#31459=ADVANCED_FACE('',(#6299),#4914,.T.);
#31460=ADVANCED_FACE('',(#6300),#4915,.T.);
#31461=ADVANCED_FACE('',(#6301),#4916,.T.);
#31462=ADVANCED_FACE('',(#6302),#4917,.T.);
#31463=ADVANCED_FACE('',(#6303),#4918,.T.);
#31464=ADVANCED_FACE('',(#6304),#4919,.T.);
#31465=ADVANCED_FACE('',(#6305),#4920,.T.);
#31466=ADVANCED_FACE('',(#6306),#4921,.T.);
#31467=ADVANCED_FACE('',(#6307),#4922,.T.);
#31468=ADVANCED_FACE('',(#6308),#4923,.T.);
#31469=ADVANCED_FACE('',(#6309),#4924,.T.);
#31470=ADVANCED_FACE('',(#6310),#4925,.T.);
#31471=ADVANCED_FACE('',(#6311),#4926,.T.);
#31472=ADVANCED_FACE('',(#6312),#4927,.T.);
#31473=ADVANCED_FACE('',(#6313),#4928,.T.);
#31474=ADVANCED_FACE('',(#6314),#4929,.T.);
#31475=ADVANCED_FACE('',(#6315),#4930,.T.);
#31476=ADVANCED_FACE('',(#6316),#4931,.T.);
#31477=ADVANCED_FACE('',(#6317),#4932,.T.);
#31478=ADVANCED_FACE('',(#6318),#4933,.T.);
#31479=ADVANCED_FACE('',(#6319),#4934,.T.);
#31480=ADVANCED_FACE('',(#6320),#4935,.T.);
#31481=ADVANCED_FACE('',(#6321),#4936,.T.);
#31482=ADVANCED_FACE('',(#6322),#4937,.T.);
#31483=ADVANCED_FACE('',(#6323),#4938,.T.);
#31484=ADVANCED_FACE('',(#6324),#4939,.T.);
#31485=ADVANCED_FACE('',(#6325),#4940,.T.);
#31486=ADVANCED_FACE('',(#6326),#2968,.T.);
#31487=ADVANCED_FACE('',(#6327),#4941,.T.);
#31488=ADVANCED_FACE('',(#6328),#4942,.T.);
#31489=ADVANCED_FACE('',(#6329),#4943,.T.);
#31490=ADVANCED_FACE('',(#6330),#4944,.T.);
#31491=ADVANCED_FACE('',(#6331),#4945,.T.);
#31492=ADVANCED_FACE('',(#6332),#4946,.T.);
#31493=ADVANCED_FACE('',(#6333),#4947,.T.);
#31494=ADVANCED_FACE('',(#6334),#4948,.T.);
#31495=ADVANCED_FACE('',(#6335),#4949,.T.);
#31496=ADVANCED_FACE('',(#6336),#4950,.T.);
#31497=ADVANCED_FACE('',(#6337),#4951,.T.);
#31498=ADVANCED_FACE('',(#6338),#4952,.T.);
#31499=ADVANCED_FACE('',(#6339),#4953,.T.);
#31500=ADVANCED_FACE('',(#6340),#4954,.T.);
#31501=ADVANCED_FACE('',(#6341),#4955,.T.);
#31502=ADVANCED_FACE('',(#6342),#4956,.T.);
#31503=ADVANCED_FACE('',(#6343),#4957,.T.);
#31504=ADVANCED_FACE('',(#6344),#4958,.T.);
#31505=ADVANCED_FACE('',(#6345),#4959,.T.);
#31506=ADVANCED_FACE('',(#6346),#4960,.T.);
#31507=ADVANCED_FACE('',(#6347),#4961,.T.);
#31508=ADVANCED_FACE('',(#6348),#4962,.T.);
#31509=ADVANCED_FACE('',(#6349),#4963,.T.);
#31510=ADVANCED_FACE('',(#6350),#4964,.T.);
#31511=ADVANCED_FACE('',(#6351),#4965,.T.);
#31512=ADVANCED_FACE('',(#6352),#4966,.T.);
#31513=ADVANCED_FACE('',(#6353),#4967,.T.);
#31514=ADVANCED_FACE('',(#6354),#4968,.T.);
#31515=ADVANCED_FACE('',(#6355),#4969,.T.);
#31516=ADVANCED_FACE('',(#6356),#4970,.T.);
#31517=ADVANCED_FACE('',(#6357),#4971,.T.);
#31518=ADVANCED_FACE('',(#6358),#2969,.T.);
#31519=ADVANCED_FACE('',(#6359),#4972,.T.);
#31520=ADVANCED_FACE('',(#6360),#4973,.F.);
#31521=ADVANCED_FACE('',(#6361),#4974,.F.);
#31522=ADVANCED_FACE('',(#6362),#4975,.F.);
#31523=ADVANCED_FACE('',(#6363),#4976,.F.);
#31524=ADVANCED_FACE('',(#6364),#4977,.F.);
#31525=ADVANCED_FACE('',(#6365),#4978,.F.);
#31526=ADVANCED_FACE('',(#6366),#4979,.F.);
#31527=ADVANCED_FACE('',(#6367),#4980,.F.);
#31528=ADVANCED_FACE('',(#6368),#4981,.F.);
#31529=ADVANCED_FACE('',(#6369),#4982,.F.);
#31530=ADVANCED_FACE('',(#6370),#4983,.F.);
#31531=ADVANCED_FACE('',(#6371),#4984,.F.);
#31532=ADVANCED_FACE('',(#6372),#4985,.F.);
#31533=ADVANCED_FACE('',(#6373),#4986,.F.);
#31534=ADVANCED_FACE('',(#6374),#4987,.F.);
#31535=ADVANCED_FACE('',(#6375),#2970,.F.);
#31536=ADVANCED_FACE('',(#6376),#377,.T.);
#31537=ADVANCED_FACE('',(#6377),#2971,.T.);
#31538=ADVANCED_FACE('',(#6378),#2972,.T.);
#31539=ADVANCED_FACE('',(#6379),#378,.F.);
#31540=ADVANCED_FACE('',(#6380),#4988,.T.);
#31541=ADVANCED_FACE('',(#6381),#379,.T.);
#31542=ADVANCED_FACE('',(#6382),#380,.F.);
#31543=ADVANCED_FACE('',(#6383),#381,.T.);
#31544=ADVANCED_FACE('',(#6384),#382,.T.);
#31545=ADVANCED_FACE('',(#6385),#383,.T.);
#31546=ADVANCED_FACE('',(#6386),#384,.T.);
#31547=ADVANCED_FACE('',(#6387),#385,.T.);
#31548=ADVANCED_FACE('',(#6388),#386,.T.);
#31549=ADVANCED_FACE('',(#6389),#387,.T.);
#31550=ADVANCED_FACE('',(#6390),#388,.T.);
#31551=ADVANCED_FACE('',(#6391),#389,.T.);
#31552=ADVANCED_FACE('',(#6392),#390,.T.);
#31553=ADVANCED_FACE('',(#6393),#391,.T.);
#31554=ADVANCED_FACE('',(#6394),#392,.T.);
#31555=ADVANCED_FACE('',(#6395),#393,.T.);
#31556=ADVANCED_FACE('',(#6396),#394,.T.);
#31557=ADVANCED_FACE('',(#6397),#395,.T.);
#31558=ADVANCED_FACE('',(#6398),#396,.T.);
#31559=ADVANCED_FACE('',(#6399),#397,.T.);
#31560=ADVANCED_FACE('',(#6400),#398,.T.);
#31561=ADVANCED_FACE('',(#6401),#399,.T.);
#31562=ADVANCED_FACE('',(#6402),#400,.T.);
#31563=ADVANCED_FACE('',(#6403),#401,.T.);
#31564=ADVANCED_FACE('',(#6404),#402,.T.);
#31565=ADVANCED_FACE('',(#6405),#403,.T.);
#31566=ADVANCED_FACE('',(#6406),#404,.T.);
#31567=ADVANCED_FACE('',(#6407),#405,.T.);
#31568=ADVANCED_FACE('',(#6408),#406,.T.);
#31569=ADVANCED_FACE('',(#6409),#407,.T.);
#31570=ADVANCED_FACE('',(#6410),#408,.T.);
#31571=ADVANCED_FACE('',(#6411),#409,.T.);
#31572=ADVANCED_FACE('',(#6412),#410,.T.);
#31573=ADVANCED_FACE('',(#6413),#411,.T.);
#31574=ADVANCED_FACE('',(#6414),#412,.T.);
#31575=ADVANCED_FACE('',(#6415),#413,.T.);
#31576=ADVANCED_FACE('',(#6416),#414,.T.);
#31577=ADVANCED_FACE('',(#6417),#415,.T.);
#31578=ADVANCED_FACE('',(#6418),#416,.T.);
#31579=ADVANCED_FACE('',(#6419),#417,.T.);
#31580=ADVANCED_FACE('',(#6420),#418,.T.);
#31581=ADVANCED_FACE('',(#6421),#419,.T.);
#31582=ADVANCED_FACE('',(#6422),#420,.T.);
#31583=ADVANCED_FACE('',(#6423),#421,.T.);
#31584=ADVANCED_FACE('',(#6424),#422,.T.);
#31585=ADVANCED_FACE('',(#6425),#423,.T.);
#31586=ADVANCED_FACE('',(#6426),#424,.T.);
#31587=ADVANCED_FACE('',(#6427),#425,.T.);
#31588=ADVANCED_FACE('',(#6428),#426,.T.);
#31589=ADVANCED_FACE('',(#6429),#427,.T.);
#31590=ADVANCED_FACE('',(#6430),#428,.T.);
#31591=ADVANCED_FACE('',(#6431),#429,.T.);
#31592=ADVANCED_FACE('',(#6432),#430,.T.);
#31593=ADVANCED_FACE('',(#6433),#431,.T.);
#31594=ADVANCED_FACE('',(#6434),#432,.T.);
#31595=ADVANCED_FACE('',(#6435),#433,.T.);
#31596=ADVANCED_FACE('',(#6436),#434,.T.);
#31597=ADVANCED_FACE('',(#6437),#435,.T.);
#31598=ADVANCED_FACE('',(#6438),#436,.T.);
#31599=ADVANCED_FACE('',(#6439),#437,.T.);
#31600=ADVANCED_FACE('',(#6440),#438,.T.);
#31601=ADVANCED_FACE('',(#6441),#439,.T.);
#31602=ADVANCED_FACE('',(#6442),#440,.T.);
#31603=ADVANCED_FACE('',(#6443),#441,.T.);
#31604=ADVANCED_FACE('',(#6444),#442,.T.);
#31605=ADVANCED_FACE('',(#6445),#443,.T.);
#31606=ADVANCED_FACE('',(#6446),#444,.T.);
#31607=ADVANCED_FACE('',(#6447),#445,.T.);
#31608=ADVANCED_FACE('',(#6448),#446,.T.);
#31609=ADVANCED_FACE('',(#6449),#447,.T.);
#31610=ADVANCED_FACE('',(#6450),#448,.T.);
#31611=ADVANCED_FACE('',(#6451),#449,.T.);
#31612=ADVANCED_FACE('',(#6452),#450,.T.);
#31613=ADVANCED_FACE('',(#6453),#451,.T.);
#31614=ADVANCED_FACE('',(#6454),#452,.T.);
#31615=ADVANCED_FACE('',(#6455),#453,.T.);
#31616=ADVANCED_FACE('',(#6456),#454,.T.);
#31617=ADVANCED_FACE('',(#6457),#455,.T.);
#31618=ADVANCED_FACE('',(#6458),#456,.T.);
#31619=ADVANCED_FACE('',(#6459),#457,.T.);
#31620=ADVANCED_FACE('',(#6460),#458,.T.);
#31621=ADVANCED_FACE('',(#6461),#459,.T.);
#31622=ADVANCED_FACE('',(#6462),#4989,.T.);
#31623=ADVANCED_FACE('',(#6463),#4990,.T.);
#31624=ADVANCED_FACE('',(#6464),#4991,.T.);
#31625=ADVANCED_FACE('',(#6465),#4992,.T.);
#31626=ADVANCED_FACE('',(#6466),#4993,.T.);
#31627=ADVANCED_FACE('',(#6467),#4994,.T.);
#31628=ADVANCED_FACE('',(#6468),#4995,.T.);
#31629=ADVANCED_FACE('',(#6469),#4996,.T.);
#31630=ADVANCED_FACE('',(#6470),#4997,.T.);
#31631=ADVANCED_FACE('',(#6471),#4998,.T.);
#31632=ADVANCED_FACE('',(#6472),#4999,.T.);
#31633=ADVANCED_FACE('',(#6473),#5000,.T.);
#31634=ADVANCED_FACE('',(#6474),#5001,.T.);
#31635=ADVANCED_FACE('',(#6475),#5002,.T.);
#31636=ADVANCED_FACE('',(#6476),#5003,.T.);
#31637=ADVANCED_FACE('',(#6477),#5004,.T.);
#31638=ADVANCED_FACE('',(#6478),#5005,.T.);
#31639=ADVANCED_FACE('',(#6479),#5006,.T.);
#31640=ADVANCED_FACE('',(#6480),#5007,.T.);
#31641=ADVANCED_FACE('',(#6481),#5008,.T.);
#31642=ADVANCED_FACE('',(#6482),#5009,.T.);
#31643=ADVANCED_FACE('',(#6483),#5010,.T.);
#31644=ADVANCED_FACE('',(#6484),#5011,.T.);
#31645=ADVANCED_FACE('',(#6485),#5012,.T.);
#31646=ADVANCED_FACE('',(#6486),#5013,.T.);
#31647=ADVANCED_FACE('',(#6487),#5014,.T.);
#31648=ADVANCED_FACE('',(#6488),#5015,.T.);
#31649=ADVANCED_FACE('',(#6489),#5016,.T.);
#31650=ADVANCED_FACE('',(#6490),#5017,.T.);
#31651=ADVANCED_FACE('',(#6491),#5018,.T.);
#31652=ADVANCED_FACE('',(#6492),#5019,.T.);
#31653=ADVANCED_FACE('',(#6493),#5020,.T.);
#31654=ADVANCED_FACE('',(#6494),#5021,.T.);
#31655=ADVANCED_FACE('',(#6495),#5022,.T.);
#31656=ADVANCED_FACE('',(#6496),#5023,.T.);
#31657=ADVANCED_FACE('',(#6497),#5024,.T.);
#31658=ADVANCED_FACE('',(#6498),#5025,.T.);
#31659=ADVANCED_FACE('',(#6499),#5026,.T.);
#31660=ADVANCED_FACE('',(#6500),#5027,.T.);
#31661=ADVANCED_FACE('',(#6501),#5028,.T.);
#31662=ADVANCED_FACE('',(#6502),#5029,.T.);
#31663=ADVANCED_FACE('',(#6503),#5030,.T.);
#31664=ADVANCED_FACE('',(#6504),#5031,.T.);
#31665=ADVANCED_FACE('',(#6505),#5032,.T.);
#31666=ADVANCED_FACE('',(#6506),#5033,.T.);
#31667=ADVANCED_FACE('',(#6507),#5034,.T.);
#31668=ADVANCED_FACE('',(#6508),#5035,.T.);
#31669=ADVANCED_FACE('',(#6509),#5036,.T.);
#31670=ADVANCED_FACE('',(#6510),#5037,.T.);
#31671=ADVANCED_FACE('',(#6511),#5038,.T.);
#31672=ADVANCED_FACE('',(#6512),#5039,.T.);
#31673=ADVANCED_FACE('',(#6513),#5040,.T.);
#31674=ADVANCED_FACE('',(#6514),#5041,.T.);
#31675=ADVANCED_FACE('',(#6515),#5042,.T.);
#31676=ADVANCED_FACE('',(#6516),#5043,.T.);
#31677=ADVANCED_FACE('',(#6517),#5044,.T.);
#31678=ADVANCED_FACE('',(#6518),#5045,.T.);
#31679=ADVANCED_FACE('',(#6519),#5046,.T.);
#31680=ADVANCED_FACE('',(#6520),#5047,.T.);
#31681=ADVANCED_FACE('',(#6521),#5048,.T.);
#31682=ADVANCED_FACE('',(#6522),#5049,.T.);
#31683=ADVANCED_FACE('',(#6523),#5050,.T.);
#31684=ADVANCED_FACE('',(#6524),#5051,.T.);
#31685=ADVANCED_FACE('',(#6525),#5052,.T.);
#31686=ADVANCED_FACE('',(#6526),#5053,.T.);
#31687=ADVANCED_FACE('',(#6527),#5054,.T.);
#31688=ADVANCED_FACE('',(#6528),#5055,.T.);
#31689=ADVANCED_FACE('',(#6529),#5056,.T.);
#31690=ADVANCED_FACE('',(#6530),#5057,.T.);
#31691=ADVANCED_FACE('',(#6531),#5058,.T.);
#31692=ADVANCED_FACE('',(#6532),#5059,.T.);
#31693=ADVANCED_FACE('',(#6533),#5060,.T.);
#31694=ADVANCED_FACE('',(#6534),#5061,.T.);
#31695=ADVANCED_FACE('',(#6535),#5062,.T.);
#31696=ADVANCED_FACE('',(#6536),#5063,.T.);
#31697=ADVANCED_FACE('',(#6537),#5064,.T.);
#31698=ADVANCED_FACE('',(#6538),#5065,.T.);
#31699=ADVANCED_FACE('',(#6539),#5066,.T.);
#31700=ADVANCED_FACE('',(#6540),#5067,.T.);
#31701=ADVANCED_FACE('',(#6541),#460,.T.);
#31702=ADVANCED_FACE('',(#6542),#461,.T.);
#31703=ADVANCED_FACE('',(#6543),#462,.T.);
#31704=ADVANCED_FACE('',(#6544),#463,.T.);
#31705=ADVANCED_FACE('',(#6545),#464,.T.);
#31706=ADVANCED_FACE('',(#6546),#465,.T.);
#31707=ADVANCED_FACE('',(#6547),#466,.T.);
#31708=ADVANCED_FACE('',(#6548),#467,.T.);
#31709=ADVANCED_FACE('',(#6549),#468,.T.);
#31710=ADVANCED_FACE('',(#6550),#469,.T.);
#31711=ADVANCED_FACE('',(#6551),#470,.T.);
#31712=ADVANCED_FACE('',(#6552),#471,.T.);
#31713=ADVANCED_FACE('',(#6553),#472,.T.);
#31714=ADVANCED_FACE('',(#6554),#473,.T.);
#31715=ADVANCED_FACE('',(#6555),#474,.T.);
#31716=ADVANCED_FACE('',(#6556),#475,.T.);
#31717=ADVANCED_FACE('',(#6557),#476,.T.);
#31718=ADVANCED_FACE('',(#6558),#477,.T.);
#31719=ADVANCED_FACE('',(#6559),#478,.T.);
#31720=ADVANCED_FACE('',(#6560),#479,.T.);
#31721=ADVANCED_FACE('',(#6561),#480,.T.);
#31722=ADVANCED_FACE('',(#6562),#481,.T.);
#31723=ADVANCED_FACE('',(#6563),#482,.T.);
#31724=ADVANCED_FACE('',(#6564),#483,.T.);
#31725=ADVANCED_FACE('',(#6565),#484,.T.);
#31726=ADVANCED_FACE('',(#6566),#485,.T.);
#31727=ADVANCED_FACE('',(#6567),#486,.T.);
#31728=ADVANCED_FACE('',(#6568),#487,.T.);
#31729=ADVANCED_FACE('',(#6569),#488,.T.);
#31730=ADVANCED_FACE('',(#6570),#489,.T.);
#31731=ADVANCED_FACE('',(#6571),#490,.T.);
#31732=ADVANCED_FACE('',(#6572),#491,.T.);
#31733=ADVANCED_FACE('',(#6573),#492,.T.);
#31734=ADVANCED_FACE('',(#6574),#493,.T.);
#31735=ADVANCED_FACE('',(#6575),#494,.T.);
#31736=ADVANCED_FACE('',(#6576),#495,.T.);
#31737=ADVANCED_FACE('',(#6577),#496,.T.);
#31738=ADVANCED_FACE('',(#6578),#497,.T.);
#31739=ADVANCED_FACE('',(#6579),#498,.T.);
#31740=ADVANCED_FACE('',(#6580),#499,.T.);
#31741=ADVANCED_FACE('',(#6581),#500,.T.);
#31742=ADVANCED_FACE('',(#6582),#501,.T.);
#31743=ADVANCED_FACE('',(#6583),#502,.T.);
#31744=ADVANCED_FACE('',(#6584),#503,.T.);
#31745=ADVANCED_FACE('',(#6585),#504,.T.);
#31746=ADVANCED_FACE('',(#6586),#505,.T.);
#31747=ADVANCED_FACE('',(#6587),#506,.T.);
#31748=ADVANCED_FACE('',(#6588),#507,.T.);
#31749=ADVANCED_FACE('',(#6589),#508,.T.);
#31750=ADVANCED_FACE('',(#6590),#509,.T.);
#31751=ADVANCED_FACE('',(#6591),#510,.T.);
#31752=ADVANCED_FACE('',(#6592),#511,.T.);
#31753=ADVANCED_FACE('',(#6593),#512,.T.);
#31754=ADVANCED_FACE('',(#6594),#513,.T.);
#31755=ADVANCED_FACE('',(#6595),#514,.T.);
#31756=ADVANCED_FACE('',(#6596),#515,.T.);
#31757=ADVANCED_FACE('',(#6597),#516,.T.);
#31758=ADVANCED_FACE('',(#6598),#517,.T.);
#31759=ADVANCED_FACE('',(#6599),#518,.T.);
#31760=ADVANCED_FACE('',(#6600),#519,.T.);
#31761=ADVANCED_FACE('',(#6601),#520,.T.);
#31762=ADVANCED_FACE('',(#6602),#521,.T.);
#31763=ADVANCED_FACE('',(#6603),#522,.T.);
#31764=ADVANCED_FACE('',(#6604),#523,.T.);
#31765=ADVANCED_FACE('',(#6605),#524,.T.);
#31766=ADVANCED_FACE('',(#6606),#525,.T.);
#31767=ADVANCED_FACE('',(#6607),#526,.T.);
#31768=ADVANCED_FACE('',(#6608),#527,.T.);
#31769=ADVANCED_FACE('',(#6609),#528,.T.);
#31770=ADVANCED_FACE('',(#6610),#529,.T.);
#31771=ADVANCED_FACE('',(#6611),#530,.T.);
#31772=ADVANCED_FACE('',(#6612),#531,.T.);
#31773=ADVANCED_FACE('',(#6613),#532,.T.);
#31774=ADVANCED_FACE('',(#6614),#533,.T.);
#31775=ADVANCED_FACE('',(#6615),#534,.T.);
#31776=ADVANCED_FACE('',(#6616),#535,.T.);
#31777=ADVANCED_FACE('',(#6617),#536,.T.);
#31778=ADVANCED_FACE('',(#6618),#537,.T.);
#31779=ADVANCED_FACE('',(#6619),#538,.T.);
#31780=ADVANCED_FACE('',(#6620),#30124,.T.);
#31781=ADVANCED_FACE('',(#6621,#3398),#30125,.T.);
#31782=ADVANCED_FACE('',(#6622),#539,.T.);
#31783=ADVANCED_FACE('',(#6623),#5068,.T.);
#31784=ADVANCED_FACE('',(#6624),#540,.T.);
#31785=ADVANCED_FACE('',(#6625,#3399),#30126,.T.);
#31786=ADVANCED_FACE('',(#6626),#30127,.T.);
#31787=ADVANCED_FACE('',(#6627),#30128,.F.);
#31788=ADVANCED_FACE('',(#6628),#30129,.F.);
#31789=ADVANCED_FACE('',(#6629),#30130,.F.);
#31790=ADVANCED_FACE('',(#6630),#30131,.F.);
#31791=ADVANCED_FACE('',(#6631),#30132,.F.);
#31792=ADVANCED_FACE('',(#6632),#30133,.F.);
#31793=ADVANCED_FACE('',(#6633),#47,.T.);
#31794=ADVANCED_FACE('',(#6634),#48,.T.);
#31795=ADVANCED_FACE('',(#6635),#2973,.T.);
#31796=ADVANCED_FACE('',(#6636),#30134,.F.);
#31797=ADVANCED_FACE('',(#6637),#5069,.F.);
#31798=ADVANCED_FACE('',(#6638),#30135,.F.);
#31799=ADVANCED_FACE('',(#6639),#30136,.F.);
#31800=ADVANCED_FACE('',(#6640),#5070,.F.);
#31801=ADVANCED_FACE('',(#6641),#30137,.F.);
#31802=ADVANCED_FACE('',(#6642),#30138,.F.);
#31803=ADVANCED_FACE('',(#6643),#5071,.F.);
#31804=ADVANCED_FACE('',(#6644),#30139,.F.);
#31805=ADVANCED_FACE('',(#6645),#30140,.F.);
#31806=ADVANCED_FACE('',(#6646),#5072,.F.);
#31807=ADVANCED_FACE('',(#6647),#30141,.F.);
#31808=ADVANCED_FACE('',(#6648),#30142,.F.);
#31809=ADVANCED_FACE('',(#6649),#5073,.F.);
#31810=ADVANCED_FACE('',(#6650),#30143,.F.);
#31811=ADVANCED_FACE('',(#6651),#30144,.F.);
#31812=ADVANCED_FACE('',(#6652),#5074,.F.);
#31813=ADVANCED_FACE('',(#6653),#30145,.F.);
#31814=ADVANCED_FACE('',(#6654),#30146,.F.);
#31815=ADVANCED_FACE('',(#6655),#5075,.F.);
#31816=ADVANCED_FACE('',(#6656),#30147,.F.);
#31817=ADVANCED_FACE('',(#6657),#30148,.F.);
#31818=ADVANCED_FACE('',(#6658),#30149,.F.);
#31819=ADVANCED_FACE('',(#6659),#30150,.F.);
#31820=ADVANCED_FACE('',(#6660),#30151,.F.);
#31821=ADVANCED_FACE('',(#6661),#30152,.F.);
#31822=ADVANCED_FACE('',(#6662),#30153,.F.);
#31823=ADVANCED_FACE('',(#6663),#30154,.F.);
#31824=ADVANCED_FACE('',(#6664),#30155,.F.);
#31825=ADVANCED_FACE('',(#6665),#30156,.F.);
#31826=ADVANCED_FACE('',(#6666),#30157,.F.);
#31827=ADVANCED_FACE('',(#6667),#30158,.F.);
#31828=ADVANCED_FACE('',(#6668),#30159,.F.);
#31829=ADVANCED_FACE('',(#6669),#30160,.F.);
#31830=ADVANCED_FACE('',(#6670),#30161,.F.);
#31831=ADVANCED_FACE('',(#6671),#30162,.F.);
#31832=ADVANCED_FACE('',(#6672),#30163,.F.);
#31833=ADVANCED_FACE('',(#6673),#30164,.F.);
#31834=ADVANCED_FACE('',(#6674),#30165,.F.);
#31835=ADVANCED_FACE('',(#6675),#30166,.F.);
#31836=ADVANCED_FACE('',(#6676),#5076,.F.);
#31837=ADVANCED_FACE('',(#6677),#30167,.F.);
#31838=ADVANCED_FACE('',(#6678),#30168,.F.);
#31839=ADVANCED_FACE('',(#6679),#5077,.F.);
#31840=ADVANCED_FACE('',(#6680),#30169,.F.);
#31841=ADVANCED_FACE('',(#6681),#30170,.F.);
#31842=ADVANCED_FACE('',(#6682),#5078,.F.);
#31843=ADVANCED_FACE('',(#6683),#30171,.F.);
#31844=ADVANCED_FACE('',(#6684),#30172,.F.);
#31845=ADVANCED_FACE('',(#6685),#5079,.F.);
#31846=ADVANCED_FACE('',(#6686),#30173,.F.);
#31847=ADVANCED_FACE('',(#6687),#30174,.F.);
#31848=ADVANCED_FACE('',(#6688),#5080,.F.);
#31849=ADVANCED_FACE('',(#6689),#30175,.F.);
#31850=ADVANCED_FACE('',(#6690),#30176,.F.);
#31851=ADVANCED_FACE('',(#6691),#5081,.F.);
#31852=ADVANCED_FACE('',(#6692),#30177,.F.);
#31853=ADVANCED_FACE('',(#6693),#30178,.F.);
#31854=ADVANCED_FACE('',(#6694),#5082,.F.);
#31855=ADVANCED_FACE('',(#6695),#30179,.F.);
#31856=ADVANCED_FACE('',(#6696),#30180,.F.);
#31857=ADVANCED_FACE('',(#6697),#5083,.F.);
#31858=ADVANCED_FACE('',(#6698),#30181,.F.);
#31859=ADVANCED_FACE('',(#6699),#30182,.F.);
#31860=ADVANCED_FACE('',(#6700),#5084,.F.);
#31861=ADVANCED_FACE('',(#6701),#30183,.F.);
#31862=ADVANCED_FACE('',(#6702),#30184,.F.);
#31863=ADVANCED_FACE('',(#6703),#5085,.F.);
#31864=ADVANCED_FACE('',(#6704),#30185,.F.);
#31865=ADVANCED_FACE('',(#6705),#30186,.F.);
#31866=ADVANCED_FACE('',(#6706),#5086,.F.);
#31867=ADVANCED_FACE('',(#6707),#30187,.F.);
#31868=ADVANCED_FACE('',(#6708),#30188,.F.);
#31869=ADVANCED_FACE('',(#6709),#5087,.F.);
#31870=ADVANCED_FACE('',(#6710),#30189,.F.);
#31871=ADVANCED_FACE('',(#6711),#30190,.F.);
#31872=ADVANCED_FACE('',(#6712),#5088,.F.);
#31873=ADVANCED_FACE('',(#6713),#30191,.F.);
#31874=ADVANCED_FACE('',(#6714),#30192,.F.);
#31875=ADVANCED_FACE('',(#6715),#5089,.F.);
#31876=ADVANCED_FACE('',(#6716),#30193,.F.);
#31877=ADVANCED_FACE('',(#6717),#30194,.F.);
#31878=ADVANCED_FACE('',(#6718),#5090,.F.);
#31879=ADVANCED_FACE('',(#6719),#30195,.F.);
#31880=ADVANCED_FACE('',(#6720),#30196,.F.);
#31881=ADVANCED_FACE('',(#6721),#5091,.F.);
#31882=ADVANCED_FACE('',(#6722),#30197,.F.);
#31883=ADVANCED_FACE('',(#6723),#30198,.F.);
#31884=ADVANCED_FACE('',(#6724),#5092,.F.);
#31885=ADVANCED_FACE('',(#6725),#30199,.F.);
#31886=ADVANCED_FACE('',(#6726),#30200,.F.);
#31887=ADVANCED_FACE('',(#6727),#5093,.F.);
#31888=ADVANCED_FACE('',(#6728),#30201,.F.);
#31889=ADVANCED_FACE('',(#6729),#30202,.F.);
#31890=ADVANCED_FACE('',(#6730),#5094,.F.);
#31891=ADVANCED_FACE('',(#6731),#30203,.F.);
#31892=ADVANCED_FACE('',(#6732),#30204,.F.);
#31893=ADVANCED_FACE('',(#6733),#5095,.F.);
#31894=ADVANCED_FACE('',(#6734),#30205,.F.);
#31895=ADVANCED_FACE('',(#6735),#30206,.F.);
#31896=ADVANCED_FACE('',(#6736),#5096,.F.);
#31897=ADVANCED_FACE('',(#6737),#30207,.F.);
#31898=ADVANCED_FACE('',(#6738),#30208,.F.);
#31899=ADVANCED_FACE('',(#6739),#5097,.F.);
#31900=ADVANCED_FACE('',(#6740),#30209,.F.);
#31901=ADVANCED_FACE('',(#6741),#30210,.F.);
#31902=ADVANCED_FACE('',(#6742),#5098,.F.);
#31903=ADVANCED_FACE('',(#6743),#30211,.F.);
#31904=ADVANCED_FACE('',(#6744),#30212,.F.);
#31905=ADVANCED_FACE('',(#6745),#5099,.F.);
#31906=ADVANCED_FACE('',(#6746),#30213,.F.);
#31907=ADVANCED_FACE('',(#6747),#30214,.F.);
#31908=ADVANCED_FACE('',(#6748),#5100,.F.);
#31909=ADVANCED_FACE('',(#6749),#30215,.F.);
#31910=ADVANCED_FACE('',(#6750),#30216,.F.);
#31911=ADVANCED_FACE('',(#6751),#5101,.F.);
#31912=ADVANCED_FACE('',(#6752),#30217,.F.);
#31913=ADVANCED_FACE('',(#6753),#30218,.F.);
#31914=ADVANCED_FACE('',(#6754),#5102,.F.);
#31915=ADVANCED_FACE('',(#6755),#30219,.F.);
#31916=ADVANCED_FACE('',(#6756),#30220,.F.);
#31917=ADVANCED_FACE('',(#6757),#5103,.F.);
#31918=ADVANCED_FACE('',(#6758),#30221,.F.);
#31919=ADVANCED_FACE('',(#6759),#30222,.F.);
#31920=ADVANCED_FACE('',(#6760),#5104,.F.);
#31921=ADVANCED_FACE('',(#6761),#30223,.F.);
#31922=ADVANCED_FACE('',(#6762),#30224,.F.);
#31923=ADVANCED_FACE('',(#6763),#5105,.F.);
#31924=ADVANCED_FACE('',(#6764),#30225,.F.);
#31925=ADVANCED_FACE('',(#6765),#30226,.F.);
#31926=ADVANCED_FACE('',(#6766),#5106,.F.);
#31927=ADVANCED_FACE('',(#6767),#30227,.F.);
#31928=ADVANCED_FACE('',(#6768),#30228,.F.);
#31929=ADVANCED_FACE('',(#6769),#5107,.F.);
#31930=ADVANCED_FACE('',(#6770),#30229,.F.);
#31931=ADVANCED_FACE('',(#6771),#30230,.F.);
#31932=ADVANCED_FACE('',(#6772),#5108,.F.);
#31933=ADVANCED_FACE('',(#6773),#30231,.F.);
#31934=ADVANCED_FACE('',(#6774),#30232,.F.);
#31935=ADVANCED_FACE('',(#6775),#5109,.F.);
#31936=ADVANCED_FACE('',(#6776),#30233,.F.);
#31937=ADVANCED_FACE('',(#6777),#30234,.F.);
#31938=ADVANCED_FACE('',(#6778),#5110,.F.);
#31939=ADVANCED_FACE('',(#6779),#30235,.F.);
#31940=ADVANCED_FACE('',(#6780),#30236,.F.);
#31941=ADVANCED_FACE('',(#6781),#5111,.F.);
#31942=ADVANCED_FACE('',(#6782),#30237,.F.);
#31943=ADVANCED_FACE('',(#6783),#30238,.F.);
#31944=ADVANCED_FACE('',(#6784),#5112,.F.);
#31945=ADVANCED_FACE('',(#6785),#30239,.F.);
#31946=ADVANCED_FACE('',(#6786),#30240,.F.);
#31947=ADVANCED_FACE('',(#6787),#5113,.F.);
#31948=ADVANCED_FACE('',(#6788),#30241,.F.);
#31949=ADVANCED_FACE('',(#6789),#30242,.F.);
#31950=ADVANCED_FACE('',(#6790),#5114,.F.);
#31951=ADVANCED_FACE('',(#6791),#30243,.F.);
#31952=ADVANCED_FACE('',(#6792),#30244,.F.);
#31953=ADVANCED_FACE('',(#6793),#5115,.F.);
#31954=ADVANCED_FACE('',(#6794),#30245,.F.);
#31955=ADVANCED_FACE('',(#6795),#30246,.F.);
#31956=ADVANCED_FACE('',(#6796),#5116,.F.);
#31957=ADVANCED_FACE('',(#6797),#30247,.F.);
#31958=ADVANCED_FACE('',(#6798),#30248,.F.);
#31959=ADVANCED_FACE('',(#6799),#5117,.F.);
#31960=ADVANCED_FACE('',(#6800),#30249,.F.);
#31961=ADVANCED_FACE('',(#6801),#30250,.F.);
#31962=ADVANCED_FACE('',(#6802),#5118,.F.);
#31963=ADVANCED_FACE('',(#6803),#30251,.F.);
#31964=ADVANCED_FACE('',(#6804),#30252,.F.);
#31965=ADVANCED_FACE('',(#6805),#5119,.F.);
#31966=ADVANCED_FACE('',(#6806),#30253,.F.);
#31967=ADVANCED_FACE('',(#6807),#30254,.F.);
#31968=ADVANCED_FACE('',(#6808),#5120,.F.);
#31969=ADVANCED_FACE('',(#6809),#30255,.F.);
#31970=ADVANCED_FACE('',(#6810),#30256,.F.);
#31971=ADVANCED_FACE('',(#6811),#5121,.F.);
#31972=ADVANCED_FACE('',(#6812),#30257,.F.);
#31973=ADVANCED_FACE('',(#6813),#30258,.F.);
#31974=ADVANCED_FACE('',(#6814),#5122,.F.);
#31975=ADVANCED_FACE('',(#6815),#30259,.F.);
#31976=ADVANCED_FACE('',(#6816),#30260,.F.);
#31977=ADVANCED_FACE('',(#6817),#5123,.F.);
#31978=ADVANCED_FACE('',(#6818),#30261,.F.);
#31979=ADVANCED_FACE('',(#6819),#30262,.F.);
#31980=ADVANCED_FACE('',(#6820),#5124,.F.);
#31981=ADVANCED_FACE('',(#6821),#30263,.F.);
#31982=ADVANCED_FACE('',(#6822),#30264,.F.);
#31983=ADVANCED_FACE('',(#6823),#5125,.F.);
#31984=ADVANCED_FACE('',(#6824),#30265,.F.);
#31985=ADVANCED_FACE('',(#6825),#30266,.F.);
#31986=ADVANCED_FACE('',(#6826),#5126,.F.);
#31987=ADVANCED_FACE('',(#6827),#30267,.F.);
#31988=ADVANCED_FACE('',(#6828),#30268,.F.);
#31989=ADVANCED_FACE('',(#6829),#5127,.F.);
#31990=ADVANCED_FACE('',(#6830),#30269,.F.);
#31991=ADVANCED_FACE('',(#6831),#30270,.F.);
#31992=ADVANCED_FACE('',(#6832),#5128,.F.);
#31993=ADVANCED_FACE('',(#6833),#30271,.F.);
#31994=ADVANCED_FACE('',(#6834),#30272,.F.);
#31995=ADVANCED_FACE('',(#6835),#5129,.F.);
#31996=ADVANCED_FACE('',(#6836),#30273,.F.);
#31997=ADVANCED_FACE('',(#6837),#30274,.F.);
#31998=ADVANCED_FACE('',(#6838),#5130,.F.);
#31999=ADVANCED_FACE('',(#6839),#30275,.F.);
#32000=ADVANCED_FACE('',(#6840),#30276,.F.);
#32001=ADVANCED_FACE('',(#6841),#5131,.F.);
#32002=ADVANCED_FACE('',(#6842),#30277,.F.);
#32003=ADVANCED_FACE('',(#6843),#30278,.F.);
#32004=ADVANCED_FACE('',(#6844),#5132,.F.);
#32005=ADVANCED_FACE('',(#6845),#30279,.F.);
#32006=ADVANCED_FACE('',(#6846),#30280,.F.);
#32007=ADVANCED_FACE('',(#6847),#5133,.F.);
#32008=ADVANCED_FACE('',(#6848),#30281,.F.);
#32009=ADVANCED_FACE('',(#6849),#30282,.F.);
#32010=ADVANCED_FACE('',(#6850),#30283,.F.);
#32011=ADVANCED_FACE('',(#6851),#30284,.F.);
#32012=ADVANCED_FACE('',(#6852),#30285,.F.);
#32013=ADVANCED_FACE('',(#6853),#30286,.F.);
#32014=ADVANCED_FACE('',(#6854),#30287,.F.);
#32015=ADVANCED_FACE('',(#6855),#30288,.F.);
#32016=ADVANCED_FACE('',(#6856),#30289,.F.);
#32017=ADVANCED_FACE('',(#6857),#30290,.F.);
#32018=ADVANCED_FACE('',(#6858),#30291,.F.);
#32019=ADVANCED_FACE('',(#6859),#30292,.F.);
#32020=ADVANCED_FACE('',(#6860),#30293,.F.);
#32021=CLOSED_SHELL('',(#30294,#30295,#30296,#30297,#30298,#30299,#30300,
#30301,#30302,#30303,#30304,#30305));
#32022=CLOSED_SHELL('',(#30306));
#32023=CLOSED_SHELL('',(#30307));
#32024=CLOSED_SHELL('',(#30308));
#32025=CLOSED_SHELL('',(#30309,#30310,#30311,#30312,#30313,#30314,#30315,
#30316,#30317,#30318,#30319,#30320,#30321,#30322,#30323,#30324,#30325,#30326,
#30327,#30328,#30329,#30330,#30331));
#32026=CLOSED_SHELL('',(#30332,#30333,#30334,#30335,#30336,#30337,#30338,
#30339,#30340,#30341,#30342,#30343,#30344,#30345,#30346,#30347,#30348,#30349,
#30350,#30351,#30352,#30353,#30354,#30355,#30356,#30357,#30358,#30359,#30360,
#30361,#30362,#30363,#30364,#30365,#30366,#30367,#30368,#30369,#30370,#30371,
#30372,#30373,#30374,#30375,#30376,#30377,#30378,#30379,#30380,#30381,#30382,
#30383,#30384,#30385,#30386,#30387,#30388,#30389,#30390,#30391,#30392,#30393,
#30394,#30395,#30396,#30397,#30398,#30399,#30400,#30401,#30402,#30403,#30404,
#30405,#30406,#30407,#30408,#30409,#30410,#30411,#30412,#30413,#30414,#30415,
#30416,#30417,#30418,#30419,#30420,#30421,#30422,#30423,#30424,#30425,#30426,
#30427,#30428,#30429,#30430,#30431,#30432,#30433,#30434,#30435,#30436,#30437,
#30438,#30439,#30440,#30441,#30442,#30443,#30444,#30445,#30446,#30447,#30448,
#30449,#30450,#30451,#30452,#30453,#30454,#30455,#30456,#30457,#30458,#30459,
#30460,#30461,#30462,#30463,#30464,#30465,#30466,#30467,#30468,#30469,#30470,
#30471,#30472,#30473,#30474,#30475,#30476,#30477,#30478,#30479,#30480,#30481,
#30482,#30483,#30484,#30485,#30486,#30487,#30488,#30489,#30490,#30491,#30492,
#30493,#30494,#30495,#30496,#30497,#30498,#30499,#30500,#30501,#30502,#30503,
#30504,#30505,#30506,#30507,#30508,#30509,#30510,#30511,#30512,#30513,#30514,
#30515,#30516,#30517,#30518,#30519,#30520,#30521,#30522,#30523,#30524,#30525,
#30526,#30527,#30528,#30529,#30530,#30531,#30532,#30533,#30534,#30535,#30536,
#30537,#30538,#30539,#30540,#30541,#30542,#30543,#30544,#30545,#30546,#30547,
#30548,#30549,#30550,#30551,#30552,#30553,#30554,#30555,#30556,#30557,#30558,
#30559,#30560,#30561,#30562,#30563,#30564,#30565,#30566,#30567,#30568,#30569,
#30570,#30571,#30572,#30573,#30574,#30575,#30576,#30577,#30578,#30579,#30580,
#30581,#30582,#30583,#30584,#30585,#30586,#30587,#30588,#30589,#30590,#30591,
#30592,#30593,#30594,#30595,#30596,#30597,#30598,#30599,#30600,#30601,#30602,
#30603,#30604,#30605,#30606,#30607,#30608,#30609,#30610,#30611,#30612,#30613,
#30614,#30615,#30616,#30617,#30618,#30619,#30620,#30621,#30622,#30623,#30624,
#30625,#30626,#30627,#30628,#30629,#30630,#30631,#30632,#30633,#30634,#30635,
#30636,#30637,#30638,#30639,#30640,#30641,#30642,#30643,#30644,#30645,#30646,
#30647,#30648,#30649,#30650,#30651,#30652,#30653,#30654,#30655,#30656,#30657,
#30658,#30659,#30660,#30661,#30662,#30663,#30664,#30665,#30666,#30667,#30668,
#30669,#30670,#30671,#30672,#30673,#30674,#30675,#30676,#30677,#30678,#30679,
#30680,#30681,#30682,#30683,#30684,#30685,#30686,#30687,#30688,#30689,#30690,
#30691,#30692,#30693,#30694,#30695,#30696,#30697,#30698,#30699,#30700,#30701,
#30702,#30703,#30704,#30705,#30706,#30707,#30708,#30709,#30710,#30711,#30712,
#30713,#30714,#30715,#30716,#30717,#30718,#30719,#30720,#30721,#30722,#30723,
#30724,#30725,#30726,#30727,#30728,#30729,#30730,#30731,#30732,#30733,#30734,
#30735,#30736,#30737,#30738,#30739,#30740,#30741,#30742,#30743,#30744,#30745,
#30746,#30747,#30748,#30749,#30750,#30751,#30752,#30753,#30754,#30755,#30756,
#30757,#30758,#30759,#30760,#30761,#30762,#30763,#30764,#30765,#30766,#30767,
#30768,#30769,#30770,#30771,#30772,#30773,#30774,#30775,#30776,#30777,#30778,
#30779,#30780,#30781,#30782,#30783,#30784,#30785,#30786,#30787,#30788,#30789,
#30790,#30791,#30792,#30793,#30794,#30795,#30796,#30797,#30798,#30799,#30800,
#30801,#30802,#30803,#30804,#30805,#30806,#30807,#30808,#30809,#30810,#30811,
#30812,#30813,#30814,#30815,#30816,#30817,#30818,#30819,#30820,#30821,#30822,
#30823,#30824,#30825,#30826,#30827,#30828,#30829,#30830,#30831,#30832,#30833,
#30834,#30835,#30836,#30837,#30838,#30839,#30840,#30841,#30842,#30843,#30844,
#30845,#30846,#30847,#30848,#30849,#30850,#30851,#30852,#30853,#30854,#30855,
#30856,#30857,#30858,#30859,#30860,#30861,#30862,#30863,#30864,#30865,#30866,
#30867,#30868,#30869,#30870,#30871,#30872,#30873,#30874,#30875,#30876,#30877,
#30878,#30879,#30880,#30881,#30882,#30883,#30884,#30885,#30886,#30887,#30888,
#30889,#30890,#30891,#30892,#30893,#30894));
#32027=CLOSED_SHELL('',(#30895,#30896,#30897,#30898,#30899,#30900,#30901,
#30902,#30903,#30904,#30905,#30906,#30907,#30908,#30909,#30910,#30911,#30912,
#30913,#30914,#30915,#30916,#30917,#30918,#30919,#30920,#30921,#30922,#30923,
#30924,#30925,#30926,#30927,#30928,#30929,#30930,#30931,#30932,#30933,#30934,
#30935,#30936,#30937,#30938,#30939,#30940,#30941,#30942,#30943,#30944,#30945,
#30946,#30947,#30948,#30949,#30950,#30951,#30952,#30953,#30954,#30955,#30956,
#30957,#30958,#30959,#30960,#30961,#30962,#30963,#30964,#30965,#30966,#30967,
#30968,#30969,#30970,#30971,#30972,#30973,#30974,#30975,#30976,#30977,#30978,
#30979,#30980,#30981,#30982,#30983,#30984,#30985,#30986,#30987,#30988,#30989,
#30990,#30991,#30992,#30993,#30994,#30995,#30996,#30997,#30998,#30999,#31000,
#31001,#31002,#31003,#31004,#31005,#31006,#31007,#31008,#31009,#31010,#31011,
#31012,#31013,#31014,#31015,#31016,#31017,#31018,#31019,#31020,#31021,#31022,
#31023,#31024,#31025,#31026,#31027,#31028,#31029,#31030,#31031,#31032,#31033,
#31034,#31035,#31036,#31037,#31038,#31039,#31040,#31041,#31042,#31043,#31044,
#31045,#31046,#31047,#31048,#31049,#31050,#31051,#31052,#31053,#31054,#31055,
#31056,#31057,#31058,#31059,#31060,#31061,#31062,#31063,#31064,#31065,#31066,
#31067,#31068,#31069,#31070,#31071,#31072,#31073,#31074,#31075,#31076,#31077,
#31078,#31079,#31080,#31081,#31082,#31083,#31084,#31085,#31086,#31087,#31088,
#31089,#31090,#31091,#31092,#31093,#31094,#31095,#31096,#31097,#31098,#31099,
#31100,#31101,#31102,#31103,#31104,#31105,#31106,#31107,#31108,#31109,#31110,
#31111,#31112,#31113,#31114,#31115,#31116,#31117,#31118,#31119,#31120,#31121,
#31122,#31123,#31124,#31125,#31126,#31127,#31128,#31129,#31130,#31131,#31132,
#31133,#31134,#31135,#31136,#31137,#31138,#31139,#31140,#31141,#31142,#31143,
#31144,#31145,#31146,#31147,#31148,#31149,#31150,#31151,#31152,#31153,#31154,
#31155,#31156,#31157,#31158,#31159,#31160,#31161,#31162,#31163,#31164,#31165,
#31166,#31167,#31168,#31169,#31170,#31171,#31172,#31173,#31174,#31175,#31176,
#31177,#31178,#31179,#31180,#31181,#31182,#31183,#31184,#31185,#31186,#31187,
#31188,#31189,#31190,#31191,#31192,#31193,#31194,#31195,#31196,#31197,#31198,
#31199,#31200,#31201,#31202,#31203,#31204,#31205,#31206,#31207,#31208,#31209,
#31210,#31211,#31212,#31213,#31214,#31215,#31216,#31217,#31218,#31219,#31220,
#31221,#31222,#31223,#31224,#31225,#31226,#31227,#31228,#31229,#31230,#31231,
#31232,#31233,#31234,#31235,#31236,#31237,#31238,#31239,#31240,#31241,#31242,
#31243,#31244,#31245,#31246,#31247,#31248,#31249,#31250,#31251,#31252,#31253,
#31254,#31255,#31256,#31257,#31258,#31259,#31260,#31261,#31262,#31263,#31264,
#31265,#31266,#31267,#31268,#31269,#31270,#31271,#31272,#31273,#31274,#31275,
#31276,#31277,#31278,#31279,#31280,#31281,#31282,#31283,#31284,#31285,#31286,
#31287,#31288,#31289,#31290,#31291,#31292,#31293,#31294,#31295,#31296,#31297,
#31298,#31299,#31300,#31301,#31302,#31303,#31304,#31305,#31306,#31307,#31308,
#31309,#31310,#31311,#31312,#31313,#31314,#31315,#31316,#31317,#31318,#31319,
#31320,#31321,#31322,#31323,#31324,#31325,#31326,#31327,#31328,#31329,#31330,
#31331,#31332,#31333,#31334,#31335,#31336,#31337,#31338,#31339,#31340,#31341,
#31342,#31343,#31344,#31345,#31346,#31347,#31348,#31349,#31350,#31351,#31352,
#31353,#31354,#31355,#31356,#31357,#31358,#31359,#31360,#31361,#31362,#31363,
#31364,#31365,#31366,#31367,#31368,#31369,#31370,#31371,#31372,#31373,#31374,
#31375,#31376,#31377,#31378,#31379,#31380,#31381,#31382,#31383,#31384,#31385,
#31386,#31387,#31388,#31389,#31390,#31391,#31392,#31393,#31394,#31395,#31396,
#31397,#31398,#31399,#31400,#31401,#31402,#31403,#31404,#31405,#31406,#31407,
#31408,#31409,#31410,#31411,#31412,#31413,#31414,#31415,#31416,#31417,#31418,
#31419,#31420,#31421,#31422,#31423,#31424,#31425,#31426,#31427,#31428,#31429,
#31430,#31431,#31432,#31433,#31434,#31435,#31436,#31437,#31438,#31439,#31440,
#31441,#31442,#31443,#31444,#31445,#31446,#31447,#31448,#31449,#31450,#31451,
#31452,#31453,#31454,#31455,#31456,#31457));
#32028=CLOSED_SHELL('',(#31458,#31459,#31460,#31461,#31462,#31463,#31464,
#31465,#31466,#31467,#31468,#31469,#31470,#31471,#31472,#31473,#31474,#31475,
#31476,#31477,#31478,#31479,#31480,#31481,#31482,#31483,#31484,#31485,#31486,
#31487,#31488,#31489,#31490,#31491,#31492,#31493,#31494,#31495,#31496,#31497,
#31498,#31499,#31500,#31501,#31502,#31503,#31504,#31505,#31506,#31507,#31508,
#31509,#31510,#31511,#31512,#31513,#31514,#31515,#31516,#31517,#31518,#31519,
#31520,#31521,#31522,#31523,#31524,#31525,#31526,#31527,#31528,#31529,#31530,
#31531,#31532,#31533,#31534,#31535,#31536,#31537,#31538,#31539,#31540,#31541,
#31542,#31543,#31544,#31545,#31546,#31547,#31548,#31549,#31550,#31551,#31552,
#31553,#31554,#31555,#31556,#31557,#31558,#31559,#31560,#31561,#31562,#31563,
#31564,#31565,#31566,#31567,#31568,#31569,#31570,#31571,#31572,#31573,#31574,
#31575,#31576,#31577,#31578,#31579,#31580,#31581,#31582,#31583,#31584,#31585,
#31586,#31587,#31588,#31589,#31590,#31591,#31592,#31593,#31594,#31595,#31596,
#31597,#31598,#31599,#31600,#31601,#31602,#31603,#31604,#31605,#31606,#31607,
#31608,#31609,#31610,#31611,#31612,#31613,#31614,#31615,#31616,#31617,#31618,
#31619,#31620,#31621,#31622,#31623,#31624,#31625,#31626,#31627,#31628,#31629,
#31630,#31631,#31632,#31633,#31634,#31635,#31636,#31637,#31638,#31639,#31640,
#31641,#31642,#31643,#31644,#31645,#31646,#31647,#31648,#31649,#31650,#31651,
#31652,#31653,#31654,#31655,#31656,#31657,#31658,#31659,#31660,#31661,#31662,
#31663,#31664,#31665,#31666,#31667,#31668,#31669,#31670,#31671,#31672,#31673,
#31674,#31675,#31676,#31677,#31678,#31679,#31680,#31681,#31682,#31683,#31684,
#31685,#31686,#31687,#31688,#31689,#31690,#31691,#31692,#31693,#31694,#31695,
#31696,#31697,#31698,#31699,#31700,#31701,#31702,#31703,#31704,#31705,#31706,
#31707,#31708,#31709,#31710,#31711,#31712,#31713,#31714,#31715,#31716,#31717,
#31718,#31719,#31720,#31721,#31722,#31723,#31724,#31725,#31726,#31727,#31728,
#31729,#31730,#31731,#31732,#31733,#31734,#31735,#31736,#31737,#31738,#31739,
#31740,#31741,#31742,#31743,#31744,#31745,#31746,#31747,#31748,#31749,#31750,
#31751,#31752,#31753,#31754,#31755,#31756,#31757,#31758,#31759,#31760,#31761,
#31762,#31763,#31764,#31765,#31766,#31767,#31768,#31769,#31770,#31771,#31772,
#31773,#31774,#31775,#31776,#31777,#31778,#31779,#31780,#31781,#31782,#31783,
#31784,#31785,#31786,#31787,#31788,#31789,#31790,#31791,#31792,#31793,#31794,
#31795,#31796,#31797,#31798,#31799,#31800,#31801,#31802,#31803,#31804,#31805,
#31806,#31807,#31808,#31809,#31810,#31811,#31812,#31813,#31814,#31815,#31816,
#31817,#31818,#31819,#31820,#31821,#31822,#31823,#31824,#31825,#31826,#31827,
#31828,#31829,#31830,#31831,#31832,#31833,#31834,#31835,#31836,#31837,#31838,
#31839,#31840,#31841,#31842,#31843,#31844,#31845,#31846,#31847,#31848,#31849,
#31850,#31851,#31852,#31853,#31854,#31855,#31856,#31857,#31858,#31859,#31860,
#31861,#31862,#31863,#31864,#31865,#31866,#31867,#31868,#31869,#31870,#31871,
#31872,#31873,#31874,#31875,#31876,#31877,#31878,#31879,#31880,#31881,#31882,
#31883,#31884,#31885,#31886,#31887,#31888,#31889,#31890,#31891,#31892,#31893,
#31894,#31895,#31896,#31897,#31898,#31899,#31900,#31901,#31902,#31903,#31904,
#31905,#31906,#31907,#31908,#31909,#31910,#31911,#31912,#31913,#31914,#31915,
#31916,#31917,#31918,#31919,#31920,#31921,#31922,#31923,#31924,#31925,#31926,
#31927,#31928,#31929,#31930,#31931,#31932,#31933,#31934,#31935,#31936,#31937,
#31938,#31939,#31940,#31941,#31942,#31943,#31944,#31945,#31946,#31947,#31948,
#31949,#31950,#31951,#31952,#31953,#31954,#31955,#31956,#31957,#31958,#31959,
#31960,#31961,#31962,#31963,#31964,#31965,#31966,#31967,#31968,#31969,#31970,
#31971,#31972,#31973,#31974,#31975,#31976,#31977,#31978,#31979,#31980,#31981,
#31982,#31983,#31984,#31985,#31986,#31987,#31988,#31989,#31990,#31991,#31992,
#31993,#31994,#31995,#31996,#31997,#31998,#31999,#32000,#32001,#32002,#32003,
#32004,#32005,#32006,#32007,#32008,#32009,#32010,#32011,#32012,#32013,#32014,
#32015,#32016,#32017,#32018,#32019,#32020));
#32029=DERIVED_UNIT_ELEMENT(#32045,1.);
#32030=DERIVED_UNIT_ELEMENT(#75338,-3.);
#32031=DERIVED_UNIT_ELEMENT(#32045,1.);
#32032=DERIVED_UNIT_ELEMENT(#75338,-3.);
#32033=DERIVED_UNIT_ELEMENT(#32045,1.);
#32034=DERIVED_UNIT_ELEMENT(#75338,-3.);
#32035=DERIVED_UNIT_ELEMENT(#32045,1.);
#32036=DERIVED_UNIT_ELEMENT(#75338,-3.);
#32037=DERIVED_UNIT_ELEMENT(#32045,1.);
#32038=DERIVED_UNIT_ELEMENT(#75338,-3.);
#32039=DERIVED_UNIT_ELEMENT(#32045,1.);
#32040=DERIVED_UNIT_ELEMENT(#75338,-3.);
#32041=DERIVED_UNIT_ELEMENT(#32045,1.);
#32042=DERIVED_UNIT_ELEMENT(#75338,-3.);
#32043=DERIVED_UNIT_ELEMENT(#32045,1.);
#32044=DERIVED_UNIT_ELEMENT(#75338,-3.);
#32045=(
MASS_UNIT()
NAMED_UNIT(*)
SI_UNIT(.KILO.,.GRAM.)
);
#32046=DERIVED_UNIT((#32029,#32030));
#32047=DERIVED_UNIT((#32031,#32032));
#32048=DERIVED_UNIT((#32033,#32034));
#32049=DERIVED_UNIT((#32035,#32036));
#32050=DERIVED_UNIT((#32037,#32038));
#32051=DERIVED_UNIT((#32039,#32040));
#32052=DERIVED_UNIT((#32041,#32042));
#32053=DERIVED_UNIT((#32043,#32044));
#32054=MEASURE_REPRESENTATION_ITEM('density measure',
POSITIVE_RATIO_MEASURE(8000.),#32046);
#32055=MEASURE_REPRESENTATION_ITEM('density measure',
POSITIVE_RATIO_MEASURE(8000.),#32047);
#32056=MEASURE_REPRESENTATION_ITEM('density measure',
POSITIVE_RATIO_MEASURE(8000.),#32048);
#32057=MEASURE_REPRESENTATION_ITEM('density measure',
POSITIVE_RATIO_MEASURE(8000.),#32049);
#32058=MEASURE_REPRESENTATION_ITEM('density measure',
POSITIVE_RATIO_MEASURE(8000.),#32050);
#32059=MEASURE_REPRESENTATION_ITEM('density measure',
POSITIVE_RATIO_MEASURE(7850.),#32051);
#32060=MEASURE_REPRESENTATION_ITEM('density measure',
POSITIVE_RATIO_MEASURE(7850.),#32052);
#32061=MEASURE_REPRESENTATION_ITEM('density measure',
POSITIVE_RATIO_MEASURE(7850.),#32053);
#32062=PROPERTY_DEFINITION_REPRESENTATION(#32102,#32078);
#32063=PROPERTY_DEFINITION_REPRESENTATION(#32103,#32079);
#32064=PROPERTY_DEFINITION_REPRESENTATION(#32104,#32080);
#32065=PROPERTY_DEFINITION_REPRESENTATION(#32105,#32081);
#32066=PROPERTY_DEFINITION_REPRESENTATION(#32106,#32082);
#32067=PROPERTY_DEFINITION_REPRESENTATION(#32107,#32083);
#32068=PROPERTY_DEFINITION_REPRESENTATION(#32108,#32084);
#32069=PROPERTY_DEFINITION_REPRESENTATION(#32109,#32085);
#32070=PROPERTY_DEFINITION_REPRESENTATION(#32110,#32086);
#32071=PROPERTY_DEFINITION_REPRESENTATION(#32111,#32087);
#32072=PROPERTY_DEFINITION_REPRESENTATION(#32112,#32088);
#32073=PROPERTY_DEFINITION_REPRESENTATION(#32113,#32089);
#32074=PROPERTY_DEFINITION_REPRESENTATION(#32114,#32090);
#32075=PROPERTY_DEFINITION_REPRESENTATION(#32115,#32091);
#32076=PROPERTY_DEFINITION_REPRESENTATION(#32116,#32092);
#32077=PROPERTY_DEFINITION_REPRESENTATION(#32117,#32093);
#32078=REPRESENTATION('material name',(#32094),#75328);
#32079=REPRESENTATION('density',(#32054),#75328);
#32080=REPRESENTATION('material name',(#32095),#75329);
#32081=REPRESENTATION('density',(#32055),#75329);
#32082=REPRESENTATION('material name',(#32096),#75330);
#32083=REPRESENTATION('density',(#32056),#75330);
#32084=REPRESENTATION('material name',(#32097),#75331);
#32085=REPRESENTATION('density',(#32057),#75331);
#32086=REPRESENTATION('material name',(#32098),#75332);
#32087=REPRESENTATION('density',(#32058),#75332);
#32088=REPRESENTATION('material name',(#32099),#75333);
#32089=REPRESENTATION('density',(#32059),#75333);
#32090=REPRESENTATION('material name',(#32100),#75334);
#32091=REPRESENTATION('density',(#32060),#75334);
#32092=REPRESENTATION('material name',(#32101),#75335);
#32093=REPRESENTATION('density',(#32061),#75335);
#32094=DESCRIPTIVE_REPRESENTATION_ITEM('Stainless Steel',
'Stainless Steel');
#32095=DESCRIPTIVE_REPRESENTATION_ITEM('Stainless Steel',
'Stainless Steel');
#32096=DESCRIPTIVE_REPRESENTATION_ITEM('Stainless Steel',
'Stainless Steel');
#32097=DESCRIPTIVE_REPRESENTATION_ITEM('Stainless Steel',
'Stainless Steel');
#32098=DESCRIPTIVE_REPRESENTATION_ITEM('Stainless Steel',
'Stainless Steel');
#32099=DESCRIPTIVE_REPRESENTATION_ITEM('Steel','Steel');
#32100=DESCRIPTIVE_REPRESENTATION_ITEM('Steel','Steel');
#32101=DESCRIPTIVE_REPRESENTATION_ITEM('Steel','Steel');
#32102=PROPERTY_DEFINITION('material property','material name',#75378);
#32103=PROPERTY_DEFINITION('material property','density of part',#75378);
#32104=PROPERTY_DEFINITION('material property','material name',#75379);
#32105=PROPERTY_DEFINITION('material property','density of part',#75379);
#32106=PROPERTY_DEFINITION('material property','material name',#75380);
#32107=PROPERTY_DEFINITION('material property','density of part',#75380);
#32108=PROPERTY_DEFINITION('material property','material name',#75381);
#32109=PROPERTY_DEFINITION('material property','density of part',#75381);
#32110=PROPERTY_DEFINITION('material property','material name',#75382);
#32111=PROPERTY_DEFINITION('material property','density of part',#75382);
#32112=PROPERTY_DEFINITION('material property','material name',#75383);
#32113=PROPERTY_DEFINITION('material property','density of part',#75383);
#32114=PROPERTY_DEFINITION('material property','material name',#75384);
#32115=PROPERTY_DEFINITION('material property','density of part',#75384);
#32116=PROPERTY_DEFINITION('material property','material name',#75385);
#32117=PROPERTY_DEFINITION('material property','density of part',#75385);
#32118=AXIS2_PLACEMENT_3D('',#46045,#36345,#36346);
#32119=AXIS2_PLACEMENT_3D('',#46046,#36347,#36348);
#32120=AXIS2_PLACEMENT_3D('',#46047,#36349,#36350);
#32121=AXIS2_PLACEMENT_3D('',#46056,#36355,#36356);
#32122=AXIS2_PLACEMENT_3D('',#46064,#36361,#36362);
#32123=AXIS2_PLACEMENT_3D('',#46070,#36366,#36367);
#32124=AXIS2_PLACEMENT_3D('',#46072,#36369,#36370);
#32125=AXIS2_PLACEMENT_3D('',#46076,#36373,#36374);
#32126=AXIS2_PLACEMENT_3D('',#46078,#36376,#36377);
#32127=AXIS2_PLACEMENT_3D('',#46084,#36381,#36382);
#32128=AXIS2_PLACEMENT_3D('',#46088,#36385,#36386);
#32129=AXIS2_PLACEMENT_3D('',#46090,#36388,#36389);
#32130=AXIS2_PLACEMENT_3D('',#46092,#36390,#36391);
#32131=AXIS2_PLACEMENT_3D('',#46095,#36393,#36394);
#32132=AXIS2_PLACEMENT_3D('',#46096,#36395,#36396);
#32133=AXIS2_PLACEMENT_3D('',#46097,#36397,#36398);
#32134=AXIS2_PLACEMENT_3D('',#46098,#36399,#36400);
#32135=AXIS2_PLACEMENT_3D('',#46099,#36401,#36402);
#32136=AXIS2_PLACEMENT_3D('',#46102,#36403,#36404);
#32137=AXIS2_PLACEMENT_3D('',#46103,#36405,#36406);
#32138=AXIS2_PLACEMENT_3D('',#46104,#36407,#36408);
#32139=AXIS2_PLACEMENT_3D('',#46107,#36409,#36410);
#32140=AXIS2_PLACEMENT_3D('',#46108,#36411,#36412);
#32141=AXIS2_PLACEMENT_3D('',#46109,#36413,#36414);
#32142=AXIS2_PLACEMENT_3D('',#46112,#36415,#36416);
#32143=AXIS2_PLACEMENT_3D('',#46113,#36417,#36418);
#32144=AXIS2_PLACEMENT_3D('',#46114,#36419,#36420);
#32145=AXIS2_PLACEMENT_3D('',#46116,#36421,#36422);
#32146=AXIS2_PLACEMENT_3D('',#46119,#36424,#36425);
#32147=AXIS2_PLACEMENT_3D('',#46120,#36426,#36427);
#32148=AXIS2_PLACEMENT_3D('',#46122,#36428,#36429);
#32149=AXIS2_PLACEMENT_3D('',#46125,#36431,#36432);
#32150=AXIS2_PLACEMENT_3D('',#46126,#36433,#36434);
#32151=AXIS2_PLACEMENT_3D('',#46128,#36435,#36436);
#32152=AXIS2_PLACEMENT_3D('',#46131,#36438,#36439);
#32153=AXIS2_PLACEMENT_3D('',#46132,#36440,#36441);
#32154=AXIS2_PLACEMENT_3D('',#46135,#36442,#36443);
#32155=AXIS2_PLACEMENT_3D('',#46139,#36445,#36446);
#32156=AXIS2_PLACEMENT_3D('',#46141,#36448,#36449);
#32157=AXIS2_PLACEMENT_3D('',#46147,#36453,#36454);
#32158=AXIS2_PLACEMENT_3D('',#46150,#36455,#36456);
#32159=AXIS2_PLACEMENT_3D('',#46154,#36458,#36459);
#32160=AXIS2_PLACEMENT_3D('',#46156,#36461,#36462);
#32161=AXIS2_PLACEMENT_3D('',#46162,#36466,#36467);
#32162=AXIS2_PLACEMENT_3D('',#46165,#36468,#36469);
#32163=AXIS2_PLACEMENT_3D('',#46169,#36471,#36472);
#32164=AXIS2_PLACEMENT_3D('',#46171,#36474,#36475);
#32165=AXIS2_PLACEMENT_3D('',#46177,#36479,#36480);
#32166=AXIS2_PLACEMENT_3D('',#46180,#36481,#36482);
#32167=AXIS2_PLACEMENT_3D('',#46184,#36484,#36485);
#32168=AXIS2_PLACEMENT_3D('',#46186,#36487,#36488);
#32169=AXIS2_PLACEMENT_3D('',#46188,#36489,#36490);
#32170=AXIS2_PLACEMENT_3D('',#46191,#36492,#36493);
#32171=AXIS2_PLACEMENT_3D('',#46192,#36494,#36495);
#32172=AXIS2_PLACEMENT_3D('',#46195,#36497,#36498);
#32173=AXIS2_PLACEMENT_3D('',#46197,#36499,#36500);
#32174=AXIS2_PLACEMENT_3D('',#46199,#36501,#36502);
#32175=AXIS2_PLACEMENT_3D('',#46202,#36504,#36505);
#32176=AXIS2_PLACEMENT_3D('',#46204,#36506,#36507);
#32177=AXIS2_PLACEMENT_3D('',#46206,#36508,#36509);
#32178=AXIS2_PLACEMENT_3D('',#46208,#36511,#36512);
#32179=AXIS2_PLACEMENT_3D('',#46209,#36513,#36514);
#32180=AXIS2_PLACEMENT_3D('',#46211,#36515,#36516);
#32181=AXIS2_PLACEMENT_3D('',#46213,#36518,#36519);
#32182=AXIS2_PLACEMENT_3D('',#46215,#36520,#36521);
#32183=AXIS2_PLACEMENT_3D('',#46217,#36523,#36524);
#32184=AXIS2_PLACEMENT_3D('',#46219,#36525,#36526);
#32185=AXIS2_PLACEMENT_3D('',#46221,#36528,#36529);
#32186=AXIS2_PLACEMENT_3D('',#46223,#36530,#36531);
#32187=AXIS2_PLACEMENT_3D('',#46225,#36533,#36534);
#32188=AXIS2_PLACEMENT_3D('',#46226,#36535,#36536);
#32189=AXIS2_PLACEMENT_3D('',#46227,#36537,#36538);
#32190=AXIS2_PLACEMENT_3D('',#46231,#36540,#36541);
#32191=AXIS2_PLACEMENT_3D('',#46233,#36543,#36544);
#32192=AXIS2_PLACEMENT_3D('',#46235,#36546,#36547);
#32193=AXIS2_PLACEMENT_3D('',#46236,#36548,#36549);
#32194=AXIS2_PLACEMENT_3D('',#46237,#36550,#36551);
#32195=AXIS2_PLACEMENT_3D('',#46239,#36553,#36554);
#32196=AXIS2_PLACEMENT_3D('',#46241,#36556,#36557);
#32197=AXIS2_PLACEMENT_3D('',#46242,#36558,#36559);
#32198=AXIS2_PLACEMENT_3D('',#46243,#36560,#36561);
#32199=AXIS2_PLACEMENT_3D('',#46286,#36564,#36565);
#32200=AXIS2_PLACEMENT_3D('',#46288,#36566,#36567);
#32201=AXIS2_PLACEMENT_3D('',#46323,#36568,#36569);
#32202=AXIS2_PLACEMENT_3D('',#46399,#36571,#36572);
#32203=AXIS2_PLACEMENT_3D('',#46477,#36574,#36575);
#32204=AXIS2_PLACEMENT_3D('',#46553,#36577,#36578);
#32205=AXIS2_PLACEMENT_3D('',#46629,#36580,#36581);
#32206=AXIS2_PLACEMENT_3D('',#46705,#36583,#36584);
#32207=AXIS2_PLACEMENT_3D('',#46781,#36586,#36587);
#32208=AXIS2_PLACEMENT_3D('',#46859,#36589,#36590);
#32209=AXIS2_PLACEMENT_3D('',#46937,#36592,#36593);
#32210=AXIS2_PLACEMENT_3D('',#47013,#36595,#36596);
#32211=AXIS2_PLACEMENT_3D('',#47089,#36598,#36599);
#32212=AXIS2_PLACEMENT_3D('',#47165,#36601,#36602);
#32213=AXIS2_PLACEMENT_3D('',#47241,#36604,#36605);
#32214=AXIS2_PLACEMENT_3D('',#47319,#36607,#36608);
#32215=AXIS2_PLACEMENT_3D('',#47395,#36610,#36611);
#32216=AXIS2_PLACEMENT_3D('',#47473,#36613,#36614);
#32217=AXIS2_PLACEMENT_3D('',#47549,#36616,#36617);
#32218=AXIS2_PLACEMENT_3D('',#47625,#36619,#36620);
#32219=AXIS2_PLACEMENT_3D('',#47701,#36622,#36623);
#32220=AXIS2_PLACEMENT_3D('',#47777,#36625,#36626);
#32221=AXIS2_PLACEMENT_3D('',#47855,#36628,#36629);
#32222=AXIS2_PLACEMENT_3D('',#47933,#36631,#36632);
#32223=AXIS2_PLACEMENT_3D('',#48009,#36634,#36635);
#32224=AXIS2_PLACEMENT_3D('',#48085,#36637,#36638);
#32225=AXIS2_PLACEMENT_3D('',#48161,#36640,#36641);
#32226=AXIS2_PLACEMENT_3D('',#48237,#36643,#36644);
#32227=AXIS2_PLACEMENT_3D('',#48315,#36646,#36647);
#32228=AXIS2_PLACEMENT_3D('',#48391,#36649,#36650);
#32229=AXIS2_PLACEMENT_3D('',#48416,#36652,#36653);
#32230=AXIS2_PLACEMENT_3D('',#48417,#36654,#36655);
#32231=AXIS2_PLACEMENT_3D('',#48429,#36657,#36658);
#32232=AXIS2_PLACEMENT_3D('',#48430,#36659,#36660);
#32233=AXIS2_PLACEMENT_3D('',#48506,#36662,#36663);
#32234=AXIS2_PLACEMENT_3D('',#48582,#36665,#36666);
#32235=AXIS2_PLACEMENT_3D('',#48660,#36668,#36669);
#32236=AXIS2_PLACEMENT_3D('',#48736,#36671,#36672);
#32237=AXIS2_PLACEMENT_3D('',#48814,#36674,#36675);
#32238=AXIS2_PLACEMENT_3D('',#48890,#36677,#36678);
#32239=AXIS2_PLACEMENT_3D('',#48966,#36680,#36681);
#32240=AXIS2_PLACEMENT_3D('',#49042,#36683,#36684);
#32241=AXIS2_PLACEMENT_3D('',#49118,#36686,#36687);
#32242=AXIS2_PLACEMENT_3D('',#49196,#36689,#36690);
#32243=AXIS2_PLACEMENT_3D('',#49272,#36692,#36693);
#32244=AXIS2_PLACEMENT_3D('',#49350,#36695,#36696);
#32245=AXIS2_PLACEMENT_3D('',#49426,#36698,#36699);
#32246=AXIS2_PLACEMENT_3D('',#49502,#36701,#36702);
#32247=AXIS2_PLACEMENT_3D('',#49578,#36704,#36705);
#32248=AXIS2_PLACEMENT_3D('',#49654,#36707,#36708);
#32249=AXIS2_PLACEMENT_3D('',#49730,#36710,#36711);
#32250=AXIS2_PLACEMENT_3D('',#49808,#36713,#36714);
#32251=AXIS2_PLACEMENT_3D('',#49884,#36716,#36717);
#32252=AXIS2_PLACEMENT_3D('',#49962,#36719,#36720);
#32253=AXIS2_PLACEMENT_3D('',#50038,#36722,#36723);
#32254=AXIS2_PLACEMENT_3D('',#50114,#36725,#36726);
#32255=AXIS2_PLACEMENT_3D('',#50190,#36728,#36729);
#32256=AXIS2_PLACEMENT_3D('',#50266,#36731,#36732);
#32257=AXIS2_PLACEMENT_3D('',#50344,#36734,#36735);
#32258=AXIS2_PLACEMENT_3D('',#50420,#36737,#36738);
#32259=AXIS2_PLACEMENT_3D('',#50498,#36740,#36741);
#32260=AXIS2_PLACEMENT_3D('',#50574,#36743,#36744);
#32261=AXIS2_PLACEMENT_3D('',#50650,#36746,#36747);
#32262=AXIS2_PLACEMENT_3D('',#50660,#36748,#36749);
#32263=AXIS2_PLACEMENT_3D('',#50661,#36750,#36751);
#32264=AXIS2_PLACEMENT_3D('',#50662,#36752,#36753);
#32265=AXIS2_PLACEMENT_3D('',#50677,#36754,#36755);
#32266=AXIS2_PLACEMENT_3D('',#50700,#36756,#36757);
#32267=AXIS2_PLACEMENT_3D('',#50767,#36758,#36759);
#32268=AXIS2_PLACEMENT_3D('',#50770,#36760,#36761);
#32269=AXIS2_PLACEMENT_3D('',#50774,#36763,#36764);
#32270=AXIS2_PLACEMENT_3D('',#50776,#36766,#36767);
#32271=AXIS2_PLACEMENT_3D('',#50779,#36768,#36769);
#32272=AXIS2_PLACEMENT_3D('',#50783,#36771,#36772);
#32273=AXIS2_PLACEMENT_3D('',#50785,#36774,#36775);
#32274=AXIS2_PLACEMENT_3D('',#50788,#36776,#36777);
#32275=AXIS2_PLACEMENT_3D('',#50792,#36779,#36780);
#32276=AXIS2_PLACEMENT_3D('',#50794,#36782,#36783);
#32277=AXIS2_PLACEMENT_3D('',#50797,#36784,#36785);
#32278=AXIS2_PLACEMENT_3D('',#50801,#36787,#36788);
#32279=AXIS2_PLACEMENT_3D('',#50803,#36790,#36791);
#32280=AXIS2_PLACEMENT_3D('',#50806,#36792,#36793);
#32281=AXIS2_PLACEMENT_3D('',#50810,#36795,#36796);
#32282=AXIS2_PLACEMENT_3D('',#50812,#36798,#36799);
#32283=AXIS2_PLACEMENT_3D('',#50815,#36800,#36801);
#32284=AXIS2_PLACEMENT_3D('',#50819,#36803,#36804);
#32285=AXIS2_PLACEMENT_3D('',#50821,#36806,#36807);
#32286=AXIS2_PLACEMENT_3D('',#50824,#36808,#36809);
#32287=AXIS2_PLACEMENT_3D('',#50828,#36811,#36812);
#32288=AXIS2_PLACEMENT_3D('',#50830,#36814,#36815);
#32289=AXIS2_PLACEMENT_3D('',#50833,#36816,#36817);
#32290=AXIS2_PLACEMENT_3D('',#50837,#36819,#36820);
#32291=AXIS2_PLACEMENT_3D('',#50839,#36822,#36823);
#32292=AXIS2_PLACEMENT_3D('',#50842,#36824,#36825);
#32293=AXIS2_PLACEMENT_3D('',#50846,#36827,#36828);
#32294=AXIS2_PLACEMENT_3D('',#50848,#36830,#36831);
#32295=AXIS2_PLACEMENT_3D('',#50851,#36832,#36833);
#32296=AXIS2_PLACEMENT_3D('',#50855,#36835,#36836);
#32297=AXIS2_PLACEMENT_3D('',#50857,#36838,#36839);
#32298=AXIS2_PLACEMENT_3D('',#50860,#36840,#36841);
#32299=AXIS2_PLACEMENT_3D('',#50864,#36843,#36844);
#32300=AXIS2_PLACEMENT_3D('',#50866,#36846,#36847);
#32301=AXIS2_PLACEMENT_3D('',#50869,#36848,#36849);
#32302=AXIS2_PLACEMENT_3D('',#50873,#36851,#36852);
#32303=AXIS2_PLACEMENT_3D('',#50875,#36854,#36855);
#32304=AXIS2_PLACEMENT_3D('',#50878,#36856,#36857);
#32305=AXIS2_PLACEMENT_3D('',#50882,#36859,#36860);
#32306=AXIS2_PLACEMENT_3D('',#50884,#36862,#36863);
#32307=AXIS2_PLACEMENT_3D('',#50887,#36864,#36865);
#32308=AXIS2_PLACEMENT_3D('',#50891,#36867,#36868);
#32309=AXIS2_PLACEMENT_3D('',#50893,#36870,#36871);
#32310=AXIS2_PLACEMENT_3D('',#50896,#36872,#36873);
#32311=AXIS2_PLACEMENT_3D('',#50900,#36875,#36876);
#32312=AXIS2_PLACEMENT_3D('',#50902,#36878,#36879);
#32313=AXIS2_PLACEMENT_3D('',#50933,#36881,#36882);
#32314=AXIS2_PLACEMENT_3D('',#50934,#36883,#36884);
#32315=AXIS2_PLACEMENT_3D('',#50936,#36885,#36886);
#32316=AXIS2_PLACEMENT_3D('',#50938,#36887,#36888);
#32317=AXIS2_PLACEMENT_3D('',#50939,#36889,#36890);
#32318=AXIS2_PLACEMENT_3D('',#50940,#36891,#36892);
#32319=AXIS2_PLACEMENT_3D('',#50956,#36893,#36894);
#32320=AXIS2_PLACEMENT_3D('',#50962,#36895,#36896);
#32321=AXIS2_PLACEMENT_3D('',#50968,#36897,#36898);
#32322=AXIS2_PLACEMENT_3D('',#50974,#36899,#36900);
#32323=AXIS2_PLACEMENT_3D('',#50980,#36901,#36902);
#32324=AXIS2_PLACEMENT_3D('',#50986,#36903,#36904);
#32325=AXIS2_PLACEMENT_3D('',#50992,#36905,#36906);
#32326=AXIS2_PLACEMENT_3D('',#50998,#36907,#36908);
#32327=AXIS2_PLACEMENT_3D('',#51004,#36909,#36910);
#32328=AXIS2_PLACEMENT_3D('',#51010,#36911,#36912);
#32329=AXIS2_PLACEMENT_3D('',#51016,#36913,#36914);
#32330=AXIS2_PLACEMENT_3D('',#51022,#36915,#36916);
#32331=AXIS2_PLACEMENT_3D('',#51028,#36917,#36918);
#32332=AXIS2_PLACEMENT_3D('',#51034,#36919,#36920);
#32333=AXIS2_PLACEMENT_3D('',#51040,#36921,#36922);
#32334=AXIS2_PLACEMENT_3D('',#51046,#36923,#36924);
#32335=AXIS2_PLACEMENT_3D('',#51052,#36925,#36926);
#32336=AXIS2_PLACEMENT_3D('',#51058,#36927,#36928);
#32337=AXIS2_PLACEMENT_3D('',#51064,#36929,#36930);
#32338=AXIS2_PLACEMENT_3D('',#51070,#36931,#36932);
#32339=AXIS2_PLACEMENT_3D('',#51076,#36933,#36934);
#32340=AXIS2_PLACEMENT_3D('',#51082,#36935,#36936);
#32341=AXIS2_PLACEMENT_3D('',#51088,#36937,#36938);
#32342=AXIS2_PLACEMENT_3D('',#51094,#36939,#36940);
#32343=AXIS2_PLACEMENT_3D('',#51100,#36941,#36942);
#32344=AXIS2_PLACEMENT_3D('',#51106,#36943,#36944);
#32345=AXIS2_PLACEMENT_3D('',#51112,#36945,#36946);
#32346=AXIS2_PLACEMENT_3D('',#51118,#36947,#36948);
#32347=AXIS2_PLACEMENT_3D('',#51124,#36949,#36950);
#32348=AXIS2_PLACEMENT_3D('',#51130,#36951,#36952);
#32349=AXIS2_PLACEMENT_3D('',#51136,#36953,#36954);
#32350=AXIS2_PLACEMENT_3D('',#51142,#36955,#36956);
#32351=AXIS2_PLACEMENT_3D('',#51148,#36957,#36958);
#32352=AXIS2_PLACEMENT_3D('',#51154,#36959,#36960);
#32353=AXIS2_PLACEMENT_3D('',#51160,#36961,#36962);
#32354=AXIS2_PLACEMENT_3D('',#51166,#36963,#36964);
#32355=AXIS2_PLACEMENT_3D('',#51172,#36965,#36966);
#32356=AXIS2_PLACEMENT_3D('',#51178,#36967,#36968);
#32357=AXIS2_PLACEMENT_3D('',#51184,#36969,#36970);
#32358=AXIS2_PLACEMENT_3D('',#51190,#36971,#36972);
#32359=AXIS2_PLACEMENT_3D('',#51196,#36973,#36974);
#32360=AXIS2_PLACEMENT_3D('',#51202,#36975,#36976);
#32361=AXIS2_PLACEMENT_3D('',#51208,#36977,#36978);
#32362=AXIS2_PLACEMENT_3D('',#51214,#36979,#36980);
#32363=AXIS2_PLACEMENT_3D('',#51220,#36981,#36982);
#32364=AXIS2_PLACEMENT_3D('',#51226,#36983,#36984);
#32365=AXIS2_PLACEMENT_3D('',#51232,#36985,#36986);
#32366=AXIS2_PLACEMENT_3D('',#51238,#36987,#36988);
#32367=AXIS2_PLACEMENT_3D('',#51244,#36989,#36990);
#32368=AXIS2_PLACEMENT_3D('',#51250,#36991,#36992);
#32369=AXIS2_PLACEMENT_3D('',#51256,#36993,#36994);
#32370=AXIS2_PLACEMENT_3D('',#51262,#36995,#36996);
#32371=AXIS2_PLACEMENT_3D('',#51268,#36997,#36998);
#32372=AXIS2_PLACEMENT_3D('',#51274,#36999,#37000);
#32373=AXIS2_PLACEMENT_3D('',#51280,#37001,#37002);
#32374=AXIS2_PLACEMENT_3D('',#51286,#37003,#37004);
#32375=AXIS2_PLACEMENT_3D('',#51292,#37005,#37006);
#32376=AXIS2_PLACEMENT_3D('',#51298,#37007,#37008);
#32377=AXIS2_PLACEMENT_3D('',#51304,#37009,#37010);
#32378=AXIS2_PLACEMENT_3D('',#51310,#37011,#37012);
#32379=AXIS2_PLACEMENT_3D('',#51316,#37013,#37014);
#32380=AXIS2_PLACEMENT_3D('',#51322,#37015,#37016);
#32381=AXIS2_PLACEMENT_3D('',#51328,#37017,#37018);
#32382=AXIS2_PLACEMENT_3D('',#51334,#37019,#37020);
#32383=AXIS2_PLACEMENT_3D('',#51340,#37021,#37022);
#32384=AXIS2_PLACEMENT_3D('',#51346,#37023,#37024);
#32385=AXIS2_PLACEMENT_3D('',#51352,#37025,#37026);
#32386=AXIS2_PLACEMENT_3D('',#51358,#37027,#37028);
#32387=AXIS2_PLACEMENT_3D('',#51364,#37029,#37030);
#32388=AXIS2_PLACEMENT_3D('',#51370,#37031,#37032);
#32389=AXIS2_PLACEMENT_3D('',#51376,#37033,#37034);
#32390=AXIS2_PLACEMENT_3D('',#51382,#37035,#37036);
#32391=AXIS2_PLACEMENT_3D('',#51388,#37037,#37038);
#32392=AXIS2_PLACEMENT_3D('',#51394,#37039,#37040);
#32393=AXIS2_PLACEMENT_3D('',#51400,#37041,#37042);
#32394=AXIS2_PLACEMENT_3D('',#51406,#37043,#37044);
#32395=AXIS2_PLACEMENT_3D('',#51412,#37045,#37046);
#32396=AXIS2_PLACEMENT_3D('',#51418,#37047,#37048);
#32397=AXIS2_PLACEMENT_3D('',#51424,#37049,#37050);
#32398=AXIS2_PLACEMENT_3D('',#51430,#37051,#37052);
#32399=AXIS2_PLACEMENT_3D('',#51436,#37053,#37054);
#32400=AXIS2_PLACEMENT_3D('',#51442,#37055,#37056);
#32401=AXIS2_PLACEMENT_3D('',#51448,#37057,#37058);
#32402=AXIS2_PLACEMENT_3D('',#51454,#37059,#37060);
#32403=AXIS2_PLACEMENT_3D('',#51460,#37061,#37062);
#32404=AXIS2_PLACEMENT_3D('',#51466,#37063,#37064);
#32405=AXIS2_PLACEMENT_3D('',#51472,#37065,#37066);
#32406=AXIS2_PLACEMENT_3D('',#51478,#37067,#37068);
#32407=AXIS2_PLACEMENT_3D('',#51484,#37069,#37070);
#32408=AXIS2_PLACEMENT_3D('',#51490,#37071,#37072);
#32409=AXIS2_PLACEMENT_3D('',#51496,#37073,#37074);
#32410=AXIS2_PLACEMENT_3D('',#51505,#37075,#37076);
#32411=AXIS2_PLACEMENT_3D('',#51514,#37077,#37078);
#32412=AXIS2_PLACEMENT_3D('',#51523,#37079,#37080);
#32413=AXIS2_PLACEMENT_3D('',#51532,#37081,#37082);
#32414=AXIS2_PLACEMENT_3D('',#51541,#37083,#37084);
#32415=AXIS2_PLACEMENT_3D('',#51550,#37085,#37086);
#32416=AXIS2_PLACEMENT_3D('',#51559,#37087,#37088);
#32417=AXIS2_PLACEMENT_3D('',#51568,#37089,#37090);
#32418=AXIS2_PLACEMENT_3D('',#51577,#37091,#37092);
#32419=AXIS2_PLACEMENT_3D('',#51586,#37093,#37094);
#32420=AXIS2_PLACEMENT_3D('',#51595,#37095,#37096);
#32421=AXIS2_PLACEMENT_3D('',#51604,#37097,#37098);
#32422=AXIS2_PLACEMENT_3D('',#51613,#37099,#37100);
#32423=AXIS2_PLACEMENT_3D('',#51622,#37101,#37102);
#32424=AXIS2_PLACEMENT_3D('',#51631,#37103,#37104);
#32425=AXIS2_PLACEMENT_3D('',#51637,#37105,#37106);
#32426=AXIS2_PLACEMENT_3D('',#51643,#37107,#37108);
#32427=AXIS2_PLACEMENT_3D('',#51649,#37109,#37110);
#32428=AXIS2_PLACEMENT_3D('',#51655,#37111,#37112);
#32429=AXIS2_PLACEMENT_3D('',#51661,#37113,#37114);
#32430=AXIS2_PLACEMENT_3D('',#51667,#37115,#37116);
#32431=AXIS2_PLACEMENT_3D('',#51673,#37117,#37118);
#32432=AXIS2_PLACEMENT_3D('',#51679,#37119,#37120);
#32433=AXIS2_PLACEMENT_3D('',#51685,#37121,#37122);
#32434=AXIS2_PLACEMENT_3D('',#51691,#37123,#37124);
#32435=AXIS2_PLACEMENT_3D('',#51697,#37125,#37126);
#32436=AXIS2_PLACEMENT_3D('',#51703,#37127,#37128);
#32437=AXIS2_PLACEMENT_3D('',#51709,#37129,#37130);
#32438=AXIS2_PLACEMENT_3D('',#51715,#37131,#37132);
#32439=AXIS2_PLACEMENT_3D('',#51721,#37133,#37134);
#32440=AXIS2_PLACEMENT_3D('',#51727,#37135,#37136);
#32441=AXIS2_PLACEMENT_3D('',#51733,#37137,#37138);
#32442=AXIS2_PLACEMENT_3D('',#51739,#37139,#37140);
#32443=AXIS2_PLACEMENT_3D('',#51745,#37141,#37142);
#32444=AXIS2_PLACEMENT_3D('',#51751,#37143,#37144);
#32445=AXIS2_PLACEMENT_3D('',#51757,#37145,#37146);
#32446=AXIS2_PLACEMENT_3D('',#51763,#37147,#37148);
#32447=AXIS2_PLACEMENT_3D('',#51769,#37149,#37150);
#32448=AXIS2_PLACEMENT_3D('',#51775,#37151,#37152);
#32449=AXIS2_PLACEMENT_3D('',#51781,#37153,#37154);
#32450=AXIS2_PLACEMENT_3D('',#51787,#37155,#37156);
#32451=AXIS2_PLACEMENT_3D('',#51793,#37157,#37158);
#32452=AXIS2_PLACEMENT_3D('',#51799,#37159,#37160);
#32453=AXIS2_PLACEMENT_3D('',#51805,#37161,#37162);
#32454=AXIS2_PLACEMENT_3D('',#51811,#37163,#37164);
#32455=AXIS2_PLACEMENT_3D('',#51817,#37165,#37166);
#32456=AXIS2_PLACEMENT_3D('',#51823,#37167,#37168);
#32457=AXIS2_PLACEMENT_3D('',#51829,#37169,#37170);
#32458=AXIS2_PLACEMENT_3D('',#51835,#37171,#37172);
#32459=AXIS2_PLACEMENT_3D('',#51841,#37173,#37174);
#32460=AXIS2_PLACEMENT_3D('',#51847,#37175,#37176);
#32461=AXIS2_PLACEMENT_3D('',#51853,#37177,#37178);
#32462=AXIS2_PLACEMENT_3D('',#51859,#37179,#37180);
#32463=AXIS2_PLACEMENT_3D('',#51873,#37182,#37183);
#32464=AXIS2_PLACEMENT_3D('',#51889,#37184,#37185);
#32465=AXIS2_PLACEMENT_3D('',#51895,#37186,#37187);
#32466=AXIS2_PLACEMENT_3D('',#51901,#37188,#37189);
#32467=AXIS2_PLACEMENT_3D('',#51907,#37190,#37191);
#32468=AXIS2_PLACEMENT_3D('',#51913,#37192,#37193);
#32469=AXIS2_PLACEMENT_3D('',#51919,#37194,#37195);
#32470=AXIS2_PLACEMENT_3D('',#51925,#37196,#37197);
#32471=AXIS2_PLACEMENT_3D('',#51931,#37198,#37199);
#32472=AXIS2_PLACEMENT_3D('',#51937,#37200,#37201);
#32473=AXIS2_PLACEMENT_3D('',#51943,#37202,#37203);
#32474=AXIS2_PLACEMENT_3D('',#51949,#37204,#37205);
#32475=AXIS2_PLACEMENT_3D('',#51955,#37206,#37207);
#32476=AXIS2_PLACEMENT_3D('',#51961,#37208,#37209);
#32477=AXIS2_PLACEMENT_3D('',#51967,#37210,#37211);
#32478=AXIS2_PLACEMENT_3D('',#51973,#37212,#37213);
#32479=AXIS2_PLACEMENT_3D('',#51979,#37214,#37215);
#32480=AXIS2_PLACEMENT_3D('',#51985,#37216,#37217);
#32481=AXIS2_PLACEMENT_3D('',#51991,#37218,#37219);
#32482=AXIS2_PLACEMENT_3D('',#51997,#37220,#37221);
#32483=AXIS2_PLACEMENT_3D('',#52003,#37222,#37223);
#32484=AXIS2_PLACEMENT_3D('',#52009,#37224,#37225);
#32485=AXIS2_PLACEMENT_3D('',#52015,#37226,#37227);
#32486=AXIS2_PLACEMENT_3D('',#52021,#37228,#37229);
#32487=AXIS2_PLACEMENT_3D('',#52027,#37230,#37231);
#32488=AXIS2_PLACEMENT_3D('',#52033,#37232,#37233);
#32489=AXIS2_PLACEMENT_3D('',#52039,#37234,#37235);
#32490=AXIS2_PLACEMENT_3D('',#52045,#37236,#37237);
#32491=AXIS2_PLACEMENT_3D('',#52051,#37238,#37239);
#32492=AXIS2_PLACEMENT_3D('',#52057,#37240,#37241);
#32493=AXIS2_PLACEMENT_3D('',#52063,#37242,#37243);
#32494=AXIS2_PLACEMENT_3D('',#52069,#37244,#37245);
#32495=AXIS2_PLACEMENT_3D('',#52075,#37246,#37247);
#32496=AXIS2_PLACEMENT_3D('',#52081,#37248,#37249);
#32497=AXIS2_PLACEMENT_3D('',#52087,#37250,#37251);
#32498=AXIS2_PLACEMENT_3D('',#52093,#37252,#37253);
#32499=AXIS2_PLACEMENT_3D('',#52099,#37254,#37255);
#32500=AXIS2_PLACEMENT_3D('',#52105,#37256,#37257);
#32501=AXIS2_PLACEMENT_3D('',#52111,#37258,#37259);
#32502=AXIS2_PLACEMENT_3D('',#52117,#37260,#37261);
#32503=AXIS2_PLACEMENT_3D('',#52123,#37262,#37263);
#32504=AXIS2_PLACEMENT_3D('',#52129,#37264,#37265);
#32505=AXIS2_PLACEMENT_3D('',#52135,#37266,#37267);
#32506=AXIS2_PLACEMENT_3D('',#52141,#37268,#37269);
#32507=AXIS2_PLACEMENT_3D('',#52147,#37270,#37271);
#32508=AXIS2_PLACEMENT_3D('',#52153,#37272,#37273);
#32509=AXIS2_PLACEMENT_3D('',#52159,#37274,#37275);
#32510=AXIS2_PLACEMENT_3D('',#52165,#37276,#37277);
#32511=AXIS2_PLACEMENT_3D('',#52171,#37278,#37279);
#32512=AXIS2_PLACEMENT_3D('',#52177,#37280,#37281);
#32513=AXIS2_PLACEMENT_3D('',#52183,#37282,#37283);
#32514=AXIS2_PLACEMENT_3D('',#52189,#37284,#37285);
#32515=AXIS2_PLACEMENT_3D('',#52195,#37286,#37287);
#32516=AXIS2_PLACEMENT_3D('',#52201,#37288,#37289);
#32517=AXIS2_PLACEMENT_3D('',#52207,#37290,#37291);
#32518=AXIS2_PLACEMENT_3D('',#52213,#37292,#37293);
#32519=AXIS2_PLACEMENT_3D('',#52219,#37294,#37295);
#32520=AXIS2_PLACEMENT_3D('',#52225,#37296,#37297);
#32521=AXIS2_PLACEMENT_3D('',#52231,#37298,#37299);
#32522=AXIS2_PLACEMENT_3D('',#52237,#37300,#37301);
#32523=AXIS2_PLACEMENT_3D('',#52243,#37302,#37303);
#32524=AXIS2_PLACEMENT_3D('',#52249,#37304,#37305);
#32525=AXIS2_PLACEMENT_3D('',#52255,#37306,#37307);
#32526=AXIS2_PLACEMENT_3D('',#52261,#37308,#37309);
#32527=AXIS2_PLACEMENT_3D('',#52267,#37310,#37311);
#32528=AXIS2_PLACEMENT_3D('',#52273,#37312,#37313);
#32529=AXIS2_PLACEMENT_3D('',#52279,#37314,#37315);
#32530=AXIS2_PLACEMENT_3D('',#52285,#37316,#37317);
#32531=AXIS2_PLACEMENT_3D('',#52291,#37318,#37319);
#32532=AXIS2_PLACEMENT_3D('',#52297,#37320,#37321);
#32533=AXIS2_PLACEMENT_3D('',#52303,#37322,#37323);
#32534=AXIS2_PLACEMENT_3D('',#52309,#37324,#37325);
#32535=AXIS2_PLACEMENT_3D('',#52315,#37326,#37327);
#32536=AXIS2_PLACEMENT_3D('',#52321,#37328,#37329);
#32537=AXIS2_PLACEMENT_3D('',#52327,#37330,#37331);
#32538=AXIS2_PLACEMENT_3D('',#52333,#37332,#37333);
#32539=AXIS2_PLACEMENT_3D('',#52339,#37334,#37335);
#32540=AXIS2_PLACEMENT_3D('',#52345,#37336,#37337);
#32541=AXIS2_PLACEMENT_3D('',#52351,#37338,#37339);
#32542=AXIS2_PLACEMENT_3D('',#52357,#37340,#37341);
#32543=AXIS2_PLACEMENT_3D('',#52363,#37342,#37343);
#32544=AXIS2_PLACEMENT_3D('',#52369,#37344,#37345);
#32545=AXIS2_PLACEMENT_3D('',#52375,#37346,#37347);
#32546=AXIS2_PLACEMENT_3D('',#52381,#37348,#37349);
#32547=AXIS2_PLACEMENT_3D('',#52387,#37350,#37351);
#32548=AXIS2_PLACEMENT_3D('',#52393,#37352,#37353);
#32549=AXIS2_PLACEMENT_3D('',#52399,#37354,#37355);
#32550=AXIS2_PLACEMENT_3D('',#52405,#37356,#37357);
#32551=AXIS2_PLACEMENT_3D('',#52411,#37358,#37359);
#32552=AXIS2_PLACEMENT_3D('',#52417,#37360,#37361);
#32553=AXIS2_PLACEMENT_3D('',#52423,#37362,#37363);
#32554=AXIS2_PLACEMENT_3D('',#52429,#37364,#37365);
#32555=AXIS2_PLACEMENT_3D('',#52435,#37366,#37367);
#32556=AXIS2_PLACEMENT_3D('',#52441,#37368,#37369);
#32557=AXIS2_PLACEMENT_3D('',#52447,#37370,#37371);
#32558=AXIS2_PLACEMENT_3D('',#52453,#37372,#37373);
#32559=AXIS2_PLACEMENT_3D('',#52459,#37374,#37375);
#32560=AXIS2_PLACEMENT_3D('',#52465,#37376,#37377);
#32561=AXIS2_PLACEMENT_3D('',#52471,#37378,#37379);
#32562=AXIS2_PLACEMENT_3D('',#52477,#37380,#37381);
#32563=AXIS2_PLACEMENT_3D('',#52483,#37382,#37383);
#32564=AXIS2_PLACEMENT_3D('',#52489,#37384,#37385);
#32565=AXIS2_PLACEMENT_3D('',#52495,#37386,#37387);
#32566=AXIS2_PLACEMENT_3D('',#52501,#37388,#37389);
#32567=AXIS2_PLACEMENT_3D('',#52507,#37390,#37391);
#32568=AXIS2_PLACEMENT_3D('',#52513,#37392,#37393);
#32569=AXIS2_PLACEMENT_3D('',#52519,#37394,#37395);
#32570=AXIS2_PLACEMENT_3D('',#52525,#37396,#37397);
#32571=AXIS2_PLACEMENT_3D('',#52531,#37398,#37399);
#32572=AXIS2_PLACEMENT_3D('',#52537,#37400,#37401);
#32573=AXIS2_PLACEMENT_3D('',#52543,#37402,#37403);
#32574=AXIS2_PLACEMENT_3D('',#52549,#37404,#37405);
#32575=AXIS2_PLACEMENT_3D('',#52555,#37406,#37407);
#32576=AXIS2_PLACEMENT_3D('',#52561,#37408,#37409);
#32577=AXIS2_PLACEMENT_3D('',#52567,#37410,#37411);
#32578=AXIS2_PLACEMENT_3D('',#52573,#37412,#37413);
#32579=AXIS2_PLACEMENT_3D('',#52579,#37414,#37415);
#32580=AXIS2_PLACEMENT_3D('',#52585,#37416,#37417);
#32581=AXIS2_PLACEMENT_3D('',#52591,#37418,#37419);
#32582=AXIS2_PLACEMENT_3D('',#52597,#37420,#37421);
#32583=AXIS2_PLACEMENT_3D('',#52606,#37422,#37423);
#32584=AXIS2_PLACEMENT_3D('',#52615,#37424,#37425);
#32585=AXIS2_PLACEMENT_3D('',#52624,#37426,#37427);
#32586=AXIS2_PLACEMENT_3D('',#52633,#37428,#37429);
#32587=AXIS2_PLACEMENT_3D('',#52642,#37430,#37431);
#32588=AXIS2_PLACEMENT_3D('',#52651,#37432,#37433);
#32589=AXIS2_PLACEMENT_3D('',#52660,#37434,#37435);
#32590=AXIS2_PLACEMENT_3D('',#52669,#37436,#37437);
#32591=AXIS2_PLACEMENT_3D('',#52678,#37438,#37439);
#32592=AXIS2_PLACEMENT_3D('',#52687,#37440,#37441);
#32593=AXIS2_PLACEMENT_3D('',#52696,#37442,#37443);
#32594=AXIS2_PLACEMENT_3D('',#52705,#37444,#37445);
#32595=AXIS2_PLACEMENT_3D('',#52714,#37446,#37447);
#32596=AXIS2_PLACEMENT_3D('',#52723,#37448,#37449);
#32597=AXIS2_PLACEMENT_3D('',#52732,#37450,#37451);
#32598=AXIS2_PLACEMENT_3D('',#52738,#37452,#37453);
#32599=AXIS2_PLACEMENT_3D('',#52744,#37454,#37455);
#32600=AXIS2_PLACEMENT_3D('',#52750,#37456,#37457);
#32601=AXIS2_PLACEMENT_3D('',#52756,#37458,#37459);
#32602=AXIS2_PLACEMENT_3D('',#52762,#37460,#37461);
#32603=AXIS2_PLACEMENT_3D('',#52768,#37462,#37463);
#32604=AXIS2_PLACEMENT_3D('',#52774,#37464,#37465);
#32605=AXIS2_PLACEMENT_3D('',#52780,#37466,#37467);
#32606=AXIS2_PLACEMENT_3D('',#52786,#37468,#37469);
#32607=AXIS2_PLACEMENT_3D('',#52792,#37470,#37471);
#32608=AXIS2_PLACEMENT_3D('',#52808,#37473,#37474);
#32609=AXIS2_PLACEMENT_3D('',#52809,#37475,#37476);
#32610=AXIS2_PLACEMENT_3D('',#52810,#37477,#37478);
#32611=AXIS2_PLACEMENT_3D('',#52812,#37479,#37480);
#32612=AXIS2_PLACEMENT_3D('',#52813,#37481,#37482);
#32613=AXIS2_PLACEMENT_3D('',#52814,#37483,#37484);
#32614=AXIS2_PLACEMENT_3D('',#52816,#37485,#37486);
#32615=AXIS2_PLACEMENT_3D('',#52818,#37488,#37489);
#32616=AXIS2_PLACEMENT_3D('',#52820,#37490,#37491);
#32617=AXIS2_PLACEMENT_3D('',#52821,#37492,#37493);
#32618=AXIS2_PLACEMENT_3D('',#52822,#37494,#37495);
#32619=AXIS2_PLACEMENT_3D('',#52824,#37496,#37497);
#32620=AXIS2_PLACEMENT_3D('',#52825,#37498,#37499);
#32621=AXIS2_PLACEMENT_3D('',#52826,#37500,#37501);
#32622=AXIS2_PLACEMENT_3D('',#52828,#37502,#37503);
#32623=AXIS2_PLACEMENT_3D('',#52830,#37504,#37505);
#32624=AXIS2_PLACEMENT_3D('',#52831,#37506,#37507);
#32625=AXIS2_PLACEMENT_3D('',#52832,#37508,#37509);
#32626=AXIS2_PLACEMENT_3D('',#52834,#37510,#37511);
#32627=AXIS2_PLACEMENT_3D('',#52836,#37512,#37513);
#32628=AXIS2_PLACEMENT_3D('',#52837,#37514,#37515);
#32629=AXIS2_PLACEMENT_3D('',#52838,#37516,#37517);
#32630=AXIS2_PLACEMENT_3D('',#52840,#37518,#37519);
#32631=AXIS2_PLACEMENT_3D('',#52842,#37520,#37521);
#32632=AXIS2_PLACEMENT_3D('',#52843,#37522,#37523);
#32633=AXIS2_PLACEMENT_3D('',#52844,#37524,#37525);
#32634=AXIS2_PLACEMENT_3D('',#52846,#37526,#37527);
#32635=AXIS2_PLACEMENT_3D('',#52848,#37528,#37529);
#32636=AXIS2_PLACEMENT_3D('',#52849,#37530,#37531);
#32637=AXIS2_PLACEMENT_3D('',#52850,#37532,#37533);
#32638=AXIS2_PLACEMENT_3D('',#52852,#37534,#37535);
#32639=AXIS2_PLACEMENT_3D('',#52854,#37536,#37537);
#32640=AXIS2_PLACEMENT_3D('',#52855,#37538,#37539);
#32641=AXIS2_PLACEMENT_3D('',#52856,#37540,#37541);
#32642=AXIS2_PLACEMENT_3D('',#52858,#37542,#37543);
#32643=AXIS2_PLACEMENT_3D('',#52860,#37544,#37545);
#32644=AXIS2_PLACEMENT_3D('',#52861,#37546,#37547);
#32645=AXIS2_PLACEMENT_3D('',#52862,#37548,#37549);
#32646=AXIS2_PLACEMENT_3D('',#52864,#37550,#37551);
#32647=AXIS2_PLACEMENT_3D('',#52866,#37552,#37553);
#32648=AXIS2_PLACEMENT_3D('',#52867,#37554,#37555);
#32649=AXIS2_PLACEMENT_3D('',#52868,#37556,#37557);
#32650=AXIS2_PLACEMENT_3D('',#52870,#37558,#37559);
#32651=AXIS2_PLACEMENT_3D('',#52872,#37560,#37561);
#32652=AXIS2_PLACEMENT_3D('',#52873,#37562,#37563);
#32653=AXIS2_PLACEMENT_3D('',#52874,#37564,#37565);
#32654=AXIS2_PLACEMENT_3D('',#52876,#37566,#37567);
#32655=AXIS2_PLACEMENT_3D('',#52878,#37568,#37569);
#32656=AXIS2_PLACEMENT_3D('',#52879,#37570,#37571);
#32657=AXIS2_PLACEMENT_3D('',#52880,#37572,#37573);
#32658=AXIS2_PLACEMENT_3D('',#52882,#37574,#37575);
#32659=AXIS2_PLACEMENT_3D('',#52884,#37576,#37577);
#32660=AXIS2_PLACEMENT_3D('',#52885,#37578,#37579);
#32661=AXIS2_PLACEMENT_3D('',#52886,#37580,#37581);
#32662=AXIS2_PLACEMENT_3D('',#52888,#37582,#37583);
#32663=AXIS2_PLACEMENT_3D('',#52890,#37584,#37585);
#32664=AXIS2_PLACEMENT_3D('',#52891,#37586,#37587);
#32665=AXIS2_PLACEMENT_3D('',#52892,#37588,#37589);
#32666=AXIS2_PLACEMENT_3D('',#52894,#37590,#37591);
#32667=AXIS2_PLACEMENT_3D('',#52896,#37592,#37593);
#32668=AXIS2_PLACEMENT_3D('',#52897,#37594,#37595);
#32669=AXIS2_PLACEMENT_3D('',#52898,#37596,#37597);
#32670=AXIS2_PLACEMENT_3D('',#52900,#37598,#37599);
#32671=AXIS2_PLACEMENT_3D('',#52902,#37600,#37601);
#32672=AXIS2_PLACEMENT_3D('',#52903,#37602,#37603);
#32673=AXIS2_PLACEMENT_3D('',#52904,#37604,#37605);
#32674=AXIS2_PLACEMENT_3D('',#52906,#37606,#37607);
#32675=AXIS2_PLACEMENT_3D('',#52908,#37608,#37609);
#32676=AXIS2_PLACEMENT_3D('',#52909,#37610,#37611);
#32677=AXIS2_PLACEMENT_3D('',#52910,#37612,#37613);
#32678=AXIS2_PLACEMENT_3D('',#52912,#37614,#37615);
#32679=AXIS2_PLACEMENT_3D('',#52914,#37616,#37617);
#32680=AXIS2_PLACEMENT_3D('',#52915,#37618,#37619);
#32681=AXIS2_PLACEMENT_3D('',#52916,#37620,#37621);
#32682=AXIS2_PLACEMENT_3D('',#52918,#37622,#37623);
#32683=AXIS2_PLACEMENT_3D('',#52920,#37624,#37625);
#32684=AXIS2_PLACEMENT_3D('',#52921,#37626,#37627);
#32685=AXIS2_PLACEMENT_3D('',#52922,#37628,#37629);
#32686=AXIS2_PLACEMENT_3D('',#52924,#37630,#37631);
#32687=AXIS2_PLACEMENT_3D('',#52926,#37632,#37633);
#32688=AXIS2_PLACEMENT_3D('',#52927,#37634,#37635);
#32689=AXIS2_PLACEMENT_3D('',#52928,#37636,#37637);
#32690=AXIS2_PLACEMENT_3D('',#52930,#37638,#37639);
#32691=AXIS2_PLACEMENT_3D('',#52932,#37640,#37641);
#32692=AXIS2_PLACEMENT_3D('',#52933,#37642,#37643);
#32693=AXIS2_PLACEMENT_3D('',#52934,#37644,#37645);
#32694=AXIS2_PLACEMENT_3D('',#52936,#37646,#37647);
#32695=AXIS2_PLACEMENT_3D('',#52938,#37648,#37649);
#32696=AXIS2_PLACEMENT_3D('',#52939,#37650,#37651);
#32697=AXIS2_PLACEMENT_3D('',#52940,#37652,#37653);
#32698=AXIS2_PLACEMENT_3D('',#52942,#37654,#37655);
#32699=AXIS2_PLACEMENT_3D('',#52944,#37656,#37657);
#32700=AXIS2_PLACEMENT_3D('',#52945,#37658,#37659);
#32701=AXIS2_PLACEMENT_3D('',#52946,#37660,#37661);
#32702=AXIS2_PLACEMENT_3D('',#52948,#37662,#37663);
#32703=AXIS2_PLACEMENT_3D('',#52950,#37664,#37665);
#32704=AXIS2_PLACEMENT_3D('',#52951,#37666,#37667);
#32705=AXIS2_PLACEMENT_3D('',#52952,#37668,#37669);
#32706=AXIS2_PLACEMENT_3D('',#52954,#37670,#37671);
#32707=AXIS2_PLACEMENT_3D('',#52956,#37672,#37673);
#32708=AXIS2_PLACEMENT_3D('',#52957,#37674,#37675);
#32709=AXIS2_PLACEMENT_3D('',#52958,#37676,#37677);
#32710=AXIS2_PLACEMENT_3D('',#52960,#37678,#37679);
#32711=AXIS2_PLACEMENT_3D('',#52962,#37680,#37681);
#32712=AXIS2_PLACEMENT_3D('',#52963,#37682,#37683);
#32713=AXIS2_PLACEMENT_3D('',#52964,#37684,#37685);
#32714=AXIS2_PLACEMENT_3D('',#52966,#37686,#37687);
#32715=AXIS2_PLACEMENT_3D('',#52968,#37688,#37689);
#32716=AXIS2_PLACEMENT_3D('',#52969,#37690,#37691);
#32717=AXIS2_PLACEMENT_3D('',#52970,#37692,#37693);
#32718=AXIS2_PLACEMENT_3D('',#52972,#37694,#37695);
#32719=AXIS2_PLACEMENT_3D('',#52974,#37696,#37697);
#32720=AXIS2_PLACEMENT_3D('',#52975,#37698,#37699);
#32721=AXIS2_PLACEMENT_3D('',#52976,#37700,#37701);
#32722=AXIS2_PLACEMENT_3D('',#52978,#37702,#37703);
#32723=AXIS2_PLACEMENT_3D('',#52980,#37704,#37705);
#32724=AXIS2_PLACEMENT_3D('',#52981,#37706,#37707);
#32725=AXIS2_PLACEMENT_3D('',#52982,#37708,#37709);
#32726=AXIS2_PLACEMENT_3D('',#52984,#37710,#37711);
#32727=AXIS2_PLACEMENT_3D('',#52986,#37712,#37713);
#32728=AXIS2_PLACEMENT_3D('',#52987,#37714,#37715);
#32729=AXIS2_PLACEMENT_3D('',#52988,#37716,#37717);
#32730=AXIS2_PLACEMENT_3D('',#52990,#37718,#37719);
#32731=AXIS2_PLACEMENT_3D('',#52992,#37720,#37721);
#32732=AXIS2_PLACEMENT_3D('',#52993,#37722,#37723);
#32733=AXIS2_PLACEMENT_3D('',#52994,#37724,#37725);
#32734=AXIS2_PLACEMENT_3D('',#52996,#37726,#37727);
#32735=AXIS2_PLACEMENT_3D('',#52998,#37728,#37729);
#32736=AXIS2_PLACEMENT_3D('',#52999,#37730,#37731);
#32737=AXIS2_PLACEMENT_3D('',#53000,#37732,#37733);
#32738=AXIS2_PLACEMENT_3D('',#53002,#37734,#37735);
#32739=AXIS2_PLACEMENT_3D('',#53004,#37736,#37737);
#32740=AXIS2_PLACEMENT_3D('',#53005,#37738,#37739);
#32741=AXIS2_PLACEMENT_3D('',#53006,#37740,#37741);
#32742=AXIS2_PLACEMENT_3D('',#53008,#37742,#37743);
#32743=AXIS2_PLACEMENT_3D('',#53010,#37744,#37745);
#32744=AXIS2_PLACEMENT_3D('',#53011,#37746,#37747);
#32745=AXIS2_PLACEMENT_3D('',#53012,#37748,#37749);
#32746=AXIS2_PLACEMENT_3D('',#53014,#37750,#37751);
#32747=AXIS2_PLACEMENT_3D('',#53016,#37752,#37753);
#32748=AXIS2_PLACEMENT_3D('',#53017,#37754,#37755);
#32749=AXIS2_PLACEMENT_3D('',#53018,#37756,#37757);
#32750=AXIS2_PLACEMENT_3D('',#53020,#37758,#37759);
#32751=AXIS2_PLACEMENT_3D('',#53022,#37760,#37761);
#32752=AXIS2_PLACEMENT_3D('',#53023,#37762,#37763);
#32753=AXIS2_PLACEMENT_3D('',#53024,#37764,#37765);
#32754=AXIS2_PLACEMENT_3D('',#53026,#37766,#37767);
#32755=AXIS2_PLACEMENT_3D('',#53028,#37768,#37769);
#32756=AXIS2_PLACEMENT_3D('',#53029,#37770,#37771);
#32757=AXIS2_PLACEMENT_3D('',#53030,#37772,#37773);
#32758=AXIS2_PLACEMENT_3D('',#53032,#37774,#37775);
#32759=AXIS2_PLACEMENT_3D('',#53034,#37776,#37777);
#32760=AXIS2_PLACEMENT_3D('',#53035,#37778,#37779);
#32761=AXIS2_PLACEMENT_3D('',#53036,#37780,#37781);
#32762=AXIS2_PLACEMENT_3D('',#53038,#37782,#37783);
#32763=AXIS2_PLACEMENT_3D('',#53040,#37784,#37785);
#32764=AXIS2_PLACEMENT_3D('',#53041,#37786,#37787);
#32765=AXIS2_PLACEMENT_3D('',#53042,#37788,#37789);
#32766=AXIS2_PLACEMENT_3D('',#53044,#37790,#37791);
#32767=AXIS2_PLACEMENT_3D('',#53046,#37792,#37793);
#32768=AXIS2_PLACEMENT_3D('',#53047,#37794,#37795);
#32769=AXIS2_PLACEMENT_3D('',#53048,#37796,#37797);
#32770=AXIS2_PLACEMENT_3D('',#53050,#37798,#37799);
#32771=AXIS2_PLACEMENT_3D('',#53052,#37800,#37801);
#32772=AXIS2_PLACEMENT_3D('',#53053,#37802,#37803);
#32773=AXIS2_PLACEMENT_3D('',#53054,#37804,#37805);
#32774=AXIS2_PLACEMENT_3D('',#53056,#37806,#37807);
#32775=AXIS2_PLACEMENT_3D('',#53058,#37808,#37809);
#32776=AXIS2_PLACEMENT_3D('',#53059,#37810,#37811);
#32777=AXIS2_PLACEMENT_3D('',#53060,#37812,#37813);
#32778=AXIS2_PLACEMENT_3D('',#53062,#37814,#37815);
#32779=AXIS2_PLACEMENT_3D('',#53064,#37816,#37817);
#32780=AXIS2_PLACEMENT_3D('',#53065,#37818,#37819);
#32781=AXIS2_PLACEMENT_3D('',#53066,#37820,#37821);
#32782=AXIS2_PLACEMENT_3D('',#53068,#37822,#37823);
#32783=AXIS2_PLACEMENT_3D('',#53070,#37824,#37825);
#32784=AXIS2_PLACEMENT_3D('',#53071,#37826,#37827);
#32785=AXIS2_PLACEMENT_3D('',#53072,#37828,#37829);
#32786=AXIS2_PLACEMENT_3D('',#53074,#37830,#37831);
#32787=AXIS2_PLACEMENT_3D('',#53076,#37832,#37833);
#32788=AXIS2_PLACEMENT_3D('',#53077,#37834,#37835);
#32789=AXIS2_PLACEMENT_3D('',#53078,#37836,#37837);
#32790=AXIS2_PLACEMENT_3D('',#53080,#37838,#37839);
#32791=AXIS2_PLACEMENT_3D('',#53082,#37840,#37841);
#32792=AXIS2_PLACEMENT_3D('',#53083,#37842,#37843);
#32793=AXIS2_PLACEMENT_3D('',#53084,#37844,#37845);
#32794=AXIS2_PLACEMENT_3D('',#53086,#37846,#37847);
#32795=AXIS2_PLACEMENT_3D('',#53088,#37848,#37849);
#32796=AXIS2_PLACEMENT_3D('',#53089,#37850,#37851);
#32797=AXIS2_PLACEMENT_3D('',#53090,#37852,#37853);
#32798=AXIS2_PLACEMENT_3D('',#53092,#37854,#37855);
#32799=AXIS2_PLACEMENT_3D('',#53094,#37856,#37857);
#32800=AXIS2_PLACEMENT_3D('',#53095,#37858,#37859);
#32801=AXIS2_PLACEMENT_3D('',#53096,#37860,#37861);
#32802=AXIS2_PLACEMENT_3D('',#53098,#37862,#37863);
#32803=AXIS2_PLACEMENT_3D('',#53100,#37864,#37865);
#32804=AXIS2_PLACEMENT_3D('',#53101,#37866,#37867);
#32805=AXIS2_PLACEMENT_3D('',#53102,#37868,#37869);
#32806=AXIS2_PLACEMENT_3D('',#53104,#37870,#37871);
#32807=AXIS2_PLACEMENT_3D('',#53106,#37872,#37873);
#32808=AXIS2_PLACEMENT_3D('',#53107,#37874,#37875);
#32809=AXIS2_PLACEMENT_3D('',#53108,#37876,#37877);
#32810=AXIS2_PLACEMENT_3D('',#53110,#37878,#37879);
#32811=AXIS2_PLACEMENT_3D('',#53112,#37880,#37881);
#32812=AXIS2_PLACEMENT_3D('',#53113,#37882,#37883);
#32813=AXIS2_PLACEMENT_3D('',#53114,#37884,#37885);
#32814=AXIS2_PLACEMENT_3D('',#53116,#37886,#37887);
#32815=AXIS2_PLACEMENT_3D('',#53118,#37888,#37889);
#32816=AXIS2_PLACEMENT_3D('',#53119,#37890,#37891);
#32817=AXIS2_PLACEMENT_3D('',#53120,#37892,#37893);
#32818=AXIS2_PLACEMENT_3D('',#53122,#37894,#37895);
#32819=AXIS2_PLACEMENT_3D('',#53124,#37896,#37897);
#32820=AXIS2_PLACEMENT_3D('',#53125,#37898,#37899);
#32821=AXIS2_PLACEMENT_3D('',#53126,#37900,#37901);
#32822=AXIS2_PLACEMENT_3D('',#53128,#37902,#37903);
#32823=AXIS2_PLACEMENT_3D('',#53130,#37904,#37905);
#32824=AXIS2_PLACEMENT_3D('',#53131,#37906,#37907);
#32825=AXIS2_PLACEMENT_3D('',#53132,#37908,#37909);
#32826=AXIS2_PLACEMENT_3D('',#53134,#37910,#37911);
#32827=AXIS2_PLACEMENT_3D('',#53136,#37912,#37913);
#32828=AXIS2_PLACEMENT_3D('',#53137,#37914,#37915);
#32829=AXIS2_PLACEMENT_3D('',#53138,#37916,#37917);
#32830=AXIS2_PLACEMENT_3D('',#53140,#37918,#37919);
#32831=AXIS2_PLACEMENT_3D('',#53142,#37920,#37921);
#32832=AXIS2_PLACEMENT_3D('',#53143,#37922,#37923);
#32833=AXIS2_PLACEMENT_3D('',#53144,#37924,#37925);
#32834=AXIS2_PLACEMENT_3D('',#53146,#37926,#37927);
#32835=AXIS2_PLACEMENT_3D('',#53148,#37928,#37929);
#32836=AXIS2_PLACEMENT_3D('',#53149,#37930,#37931);
#32837=AXIS2_PLACEMENT_3D('',#53150,#37932,#37933);
#32838=AXIS2_PLACEMENT_3D('',#53152,#37934,#37935);
#32839=AXIS2_PLACEMENT_3D('',#53154,#37936,#37937);
#32840=AXIS2_PLACEMENT_3D('',#53155,#37938,#37939);
#32841=AXIS2_PLACEMENT_3D('',#53156,#37940,#37941);
#32842=AXIS2_PLACEMENT_3D('',#53158,#37942,#37943);
#32843=AXIS2_PLACEMENT_3D('',#53160,#37944,#37945);
#32844=AXIS2_PLACEMENT_3D('',#53161,#37946,#37947);
#32845=AXIS2_PLACEMENT_3D('',#53162,#37948,#37949);
#32846=AXIS2_PLACEMENT_3D('',#53164,#37950,#37951);
#32847=AXIS2_PLACEMENT_3D('',#53166,#37952,#37953);
#32848=AXIS2_PLACEMENT_3D('',#53167,#37954,#37955);
#32849=AXIS2_PLACEMENT_3D('',#53168,#37956,#37957);
#32850=AXIS2_PLACEMENT_3D('',#53170,#37958,#37959);
#32851=AXIS2_PLACEMENT_3D('',#53172,#37960,#37961);
#32852=AXIS2_PLACEMENT_3D('',#53173,#37962,#37963);
#32853=AXIS2_PLACEMENT_3D('',#53174,#37964,#37965);
#32854=AXIS2_PLACEMENT_3D('',#53176,#37966,#37967);
#32855=AXIS2_PLACEMENT_3D('',#53178,#37968,#37969);
#32856=AXIS2_PLACEMENT_3D('',#53179,#37970,#37971);
#32857=AXIS2_PLACEMENT_3D('',#53180,#37972,#37973);
#32858=AXIS2_PLACEMENT_3D('',#53182,#37974,#37975);
#32859=AXIS2_PLACEMENT_3D('',#53184,#37976,#37977);
#32860=AXIS2_PLACEMENT_3D('',#53185,#37978,#37979);
#32861=AXIS2_PLACEMENT_3D('',#53186,#37980,#37981);
#32862=AXIS2_PLACEMENT_3D('',#53188,#37982,#37983);
#32863=AXIS2_PLACEMENT_3D('',#53190,#37984,#37985);
#32864=AXIS2_PLACEMENT_3D('',#53191,#37986,#37987);
#32865=AXIS2_PLACEMENT_3D('',#53192,#37988,#37989);
#32866=AXIS2_PLACEMENT_3D('',#53194,#37990,#37991);
#32867=AXIS2_PLACEMENT_3D('',#53196,#37992,#37993);
#32868=AXIS2_PLACEMENT_3D('',#53197,#37994,#37995);
#32869=AXIS2_PLACEMENT_3D('',#53198,#37996,#37997);
#32870=AXIS2_PLACEMENT_3D('',#53200,#37998,#37999);
#32871=AXIS2_PLACEMENT_3D('',#53202,#38000,#38001);
#32872=AXIS2_PLACEMENT_3D('',#53203,#38002,#38003);
#32873=AXIS2_PLACEMENT_3D('',#53204,#38004,#38005);
#32874=AXIS2_PLACEMENT_3D('',#53206,#38006,#38007);
#32875=AXIS2_PLACEMENT_3D('',#53208,#38008,#38009);
#32876=AXIS2_PLACEMENT_3D('',#53209,#38010,#38011);
#32877=AXIS2_PLACEMENT_3D('',#53210,#38012,#38013);
#32878=AXIS2_PLACEMENT_3D('',#53212,#38014,#38015);
#32879=AXIS2_PLACEMENT_3D('',#53214,#38016,#38017);
#32880=AXIS2_PLACEMENT_3D('',#53215,#38018,#38019);
#32881=AXIS2_PLACEMENT_3D('',#53216,#38020,#38021);
#32882=AXIS2_PLACEMENT_3D('',#53218,#38022,#38023);
#32883=AXIS2_PLACEMENT_3D('',#53220,#38024,#38025);
#32884=AXIS2_PLACEMENT_3D('',#53221,#38026,#38027);
#32885=AXIS2_PLACEMENT_3D('',#53222,#38028,#38029);
#32886=AXIS2_PLACEMENT_3D('',#53224,#38030,#38031);
#32887=AXIS2_PLACEMENT_3D('',#53226,#38032,#38033);
#32888=AXIS2_PLACEMENT_3D('',#53227,#38034,#38035);
#32889=AXIS2_PLACEMENT_3D('',#53228,#38036,#38037);
#32890=AXIS2_PLACEMENT_3D('',#53230,#38038,#38039);
#32891=AXIS2_PLACEMENT_3D('',#53232,#38040,#38041);
#32892=AXIS2_PLACEMENT_3D('',#53233,#38042,#38043);
#32893=AXIS2_PLACEMENT_3D('',#53234,#38044,#38045);
#32894=AXIS2_PLACEMENT_3D('',#53236,#38046,#38047);
#32895=AXIS2_PLACEMENT_3D('',#53238,#38048,#38049);
#32896=AXIS2_PLACEMENT_3D('',#53239,#38050,#38051);
#32897=AXIS2_PLACEMENT_3D('',#53240,#38052,#38053);
#32898=AXIS2_PLACEMENT_3D('',#53242,#38054,#38055);
#32899=AXIS2_PLACEMENT_3D('',#53244,#38056,#38057);
#32900=AXIS2_PLACEMENT_3D('',#53245,#38058,#38059);
#32901=AXIS2_PLACEMENT_3D('',#53246,#38060,#38061);
#32902=AXIS2_PLACEMENT_3D('',#53248,#38062,#38063);
#32903=AXIS2_PLACEMENT_3D('',#53250,#38064,#38065);
#32904=AXIS2_PLACEMENT_3D('',#53251,#38066,#38067);
#32905=AXIS2_PLACEMENT_3D('',#53252,#38068,#38069);
#32906=AXIS2_PLACEMENT_3D('',#53254,#38070,#38071);
#32907=AXIS2_PLACEMENT_3D('',#53256,#38072,#38073);
#32908=AXIS2_PLACEMENT_3D('',#53257,#38074,#38075);
#32909=AXIS2_PLACEMENT_3D('',#53258,#38076,#38077);
#32910=AXIS2_PLACEMENT_3D('',#53260,#38078,#38079);
#32911=AXIS2_PLACEMENT_3D('',#53262,#38080,#38081);
#32912=AXIS2_PLACEMENT_3D('',#53263,#38082,#38083);
#32913=AXIS2_PLACEMENT_3D('',#53264,#38084,#38085);
#32914=AXIS2_PLACEMENT_3D('',#53266,#38086,#38087);
#32915=AXIS2_PLACEMENT_3D('',#53268,#38088,#38089);
#32916=AXIS2_PLACEMENT_3D('',#53269,#38090,#38091);
#32917=AXIS2_PLACEMENT_3D('',#53270,#38092,#38093);
#32918=AXIS2_PLACEMENT_3D('',#53272,#38094,#38095);
#32919=AXIS2_PLACEMENT_3D('',#53274,#38096,#38097);
#32920=AXIS2_PLACEMENT_3D('',#53275,#38098,#38099);
#32921=AXIS2_PLACEMENT_3D('',#53276,#38100,#38101);
#32922=AXIS2_PLACEMENT_3D('',#53278,#38102,#38103);
#32923=AXIS2_PLACEMENT_3D('',#53280,#38104,#38105);
#32924=AXIS2_PLACEMENT_3D('',#53281,#38106,#38107);
#32925=AXIS2_PLACEMENT_3D('',#53282,#38108,#38109);
#32926=AXIS2_PLACEMENT_3D('',#53284,#38110,#38111);
#32927=AXIS2_PLACEMENT_3D('',#53286,#38112,#38113);
#32928=AXIS2_PLACEMENT_3D('',#53287,#38114,#38115);
#32929=AXIS2_PLACEMENT_3D('',#53288,#38116,#38117);
#32930=AXIS2_PLACEMENT_3D('',#53290,#38118,#38119);
#32931=AXIS2_PLACEMENT_3D('',#53292,#38120,#38121);
#32932=AXIS2_PLACEMENT_3D('',#53293,#38122,#38123);
#32933=AXIS2_PLACEMENT_3D('',#53294,#38124,#38125);
#32934=AXIS2_PLACEMENT_3D('',#53296,#38126,#38127);
#32935=AXIS2_PLACEMENT_3D('',#53298,#38128,#38129);
#32936=AXIS2_PLACEMENT_3D('',#53299,#38130,#38131);
#32937=AXIS2_PLACEMENT_3D('',#53300,#38132,#38133);
#32938=AXIS2_PLACEMENT_3D('',#53304,#38135,#38136);
#32939=AXIS2_PLACEMENT_3D('',#53306,#38138,#38139);
#32940=AXIS2_PLACEMENT_3D('',#53311,#38142,#38143);
#32941=AXIS2_PLACEMENT_3D('',#53312,#38144,#38145);
#32942=AXIS2_PLACEMENT_3D('',#53317,#38148,#38149);
#32943=AXIS2_PLACEMENT_3D('',#53318,#38150,#38151);
#32944=AXIS2_PLACEMENT_3D('',#53323,#38154,#38155);
#32945=AXIS2_PLACEMENT_3D('',#53324,#38156,#38157);
#32946=AXIS2_PLACEMENT_3D('',#53329,#38160,#38161);
#32947=AXIS2_PLACEMENT_3D('',#53330,#38162,#38163);
#32948=AXIS2_PLACEMENT_3D('',#53335,#38166,#38167);
#32949=AXIS2_PLACEMENT_3D('',#53336,#38168,#38169);
#32950=AXIS2_PLACEMENT_3D('',#53341,#38172,#38173);
#32951=AXIS2_PLACEMENT_3D('',#53342,#38174,#38175);
#32952=AXIS2_PLACEMENT_3D('',#53347,#38178,#38179);
#32953=AXIS2_PLACEMENT_3D('',#53348,#38180,#38181);
#32954=AXIS2_PLACEMENT_3D('',#53353,#38184,#38185);
#32955=AXIS2_PLACEMENT_3D('',#53354,#38186,#38187);
#32956=AXIS2_PLACEMENT_3D('',#53359,#38190,#38191);
#32957=AXIS2_PLACEMENT_3D('',#53360,#38192,#38193);
#32958=AXIS2_PLACEMENT_3D('',#53365,#38196,#38197);
#32959=AXIS2_PLACEMENT_3D('',#53366,#38198,#38199);
#32960=AXIS2_PLACEMENT_3D('',#53371,#38202,#38203);
#32961=AXIS2_PLACEMENT_3D('',#53372,#38204,#38205);
#32962=AXIS2_PLACEMENT_3D('',#53377,#38208,#38209);
#32963=AXIS2_PLACEMENT_3D('',#53378,#38210,#38211);
#32964=AXIS2_PLACEMENT_3D('',#53383,#38214,#38215);
#32965=AXIS2_PLACEMENT_3D('',#53384,#38216,#38217);
#32966=AXIS2_PLACEMENT_3D('',#53389,#38220,#38221);
#32967=AXIS2_PLACEMENT_3D('',#53390,#38222,#38223);
#32968=AXIS2_PLACEMENT_3D('',#53395,#38226,#38227);
#32969=AXIS2_PLACEMENT_3D('',#53396,#38228,#38229);
#32970=AXIS2_PLACEMENT_3D('',#53401,#38232,#38233);
#32971=AXIS2_PLACEMENT_3D('',#53402,#38234,#38235);
#32972=AXIS2_PLACEMENT_3D('',#53407,#38238,#38239);
#32973=AXIS2_PLACEMENT_3D('',#53408,#38240,#38241);
#32974=AXIS2_PLACEMENT_3D('',#53413,#38244,#38245);
#32975=AXIS2_PLACEMENT_3D('',#53414,#38246,#38247);
#32976=AXIS2_PLACEMENT_3D('',#53419,#38250,#38251);
#32977=AXIS2_PLACEMENT_3D('',#53420,#38252,#38253);
#32978=AXIS2_PLACEMENT_3D('',#53425,#38256,#38257);
#32979=AXIS2_PLACEMENT_3D('',#53426,#38258,#38259);
#32980=AXIS2_PLACEMENT_3D('',#53431,#38262,#38263);
#32981=AXIS2_PLACEMENT_3D('',#53432,#38264,#38265);
#32982=AXIS2_PLACEMENT_3D('',#53437,#38268,#38269);
#32983=AXIS2_PLACEMENT_3D('',#53438,#38270,#38271);
#32984=AXIS2_PLACEMENT_3D('',#53443,#38274,#38275);
#32985=AXIS2_PLACEMENT_3D('',#53444,#38276,#38277);
#32986=AXIS2_PLACEMENT_3D('',#53449,#38280,#38281);
#32987=AXIS2_PLACEMENT_3D('',#53450,#38282,#38283);
#32988=AXIS2_PLACEMENT_3D('',#53455,#38286,#38287);
#32989=AXIS2_PLACEMENT_3D('',#53456,#38288,#38289);
#32990=AXIS2_PLACEMENT_3D('',#53461,#38292,#38293);
#32991=AXIS2_PLACEMENT_3D('',#53462,#38294,#38295);
#32992=AXIS2_PLACEMENT_3D('',#53467,#38298,#38299);
#32993=AXIS2_PLACEMENT_3D('',#53468,#38300,#38301);
#32994=AXIS2_PLACEMENT_3D('',#53473,#38304,#38305);
#32995=AXIS2_PLACEMENT_3D('',#53474,#38306,#38307);
#32996=AXIS2_PLACEMENT_3D('',#53479,#38310,#38311);
#32997=AXIS2_PLACEMENT_3D('',#53480,#38312,#38313);
#32998=AXIS2_PLACEMENT_3D('',#53485,#38316,#38317);
#32999=AXIS2_PLACEMENT_3D('',#53486,#38318,#38319);
#33000=AXIS2_PLACEMENT_3D('',#53491,#38322,#38323);
#33001=AXIS2_PLACEMENT_3D('',#53492,#38324,#38325);
#33002=AXIS2_PLACEMENT_3D('',#53497,#38328,#38329);
#33003=AXIS2_PLACEMENT_3D('',#53498,#38330,#38331);
#33004=AXIS2_PLACEMENT_3D('',#53503,#38334,#38335);
#33005=AXIS2_PLACEMENT_3D('',#53504,#38336,#38337);
#33006=AXIS2_PLACEMENT_3D('',#53509,#38340,#38341);
#33007=AXIS2_PLACEMENT_3D('',#53510,#38342,#38343);
#33008=AXIS2_PLACEMENT_3D('',#53515,#38346,#38347);
#33009=AXIS2_PLACEMENT_3D('',#53516,#38348,#38349);
#33010=AXIS2_PLACEMENT_3D('',#53521,#38352,#38353);
#33011=AXIS2_PLACEMENT_3D('',#53522,#38354,#38355);
#33012=AXIS2_PLACEMENT_3D('',#53527,#38358,#38359);
#33013=AXIS2_PLACEMENT_3D('',#53528,#38360,#38361);
#33014=AXIS2_PLACEMENT_3D('',#53533,#38364,#38365);
#33015=AXIS2_PLACEMENT_3D('',#53534,#38366,#38367);
#33016=AXIS2_PLACEMENT_3D('',#53539,#38370,#38371);
#33017=AXIS2_PLACEMENT_3D('',#53540,#38372,#38373);
#33018=AXIS2_PLACEMENT_3D('',#53545,#38376,#38377);
#33019=AXIS2_PLACEMENT_3D('',#53546,#38378,#38379);
#33020=AXIS2_PLACEMENT_3D('',#53551,#38382,#38383);
#33021=AXIS2_PLACEMENT_3D('',#53552,#38384,#38385);
#33022=AXIS2_PLACEMENT_3D('',#53557,#38388,#38389);
#33023=AXIS2_PLACEMENT_3D('',#53558,#38390,#38391);
#33024=AXIS2_PLACEMENT_3D('',#53563,#38394,#38395);
#33025=AXIS2_PLACEMENT_3D('',#53564,#38396,#38397);
#33026=AXIS2_PLACEMENT_3D('',#53569,#38400,#38401);
#33027=AXIS2_PLACEMENT_3D('',#53570,#38402,#38403);
#33028=AXIS2_PLACEMENT_3D('',#53575,#38406,#38407);
#33029=AXIS2_PLACEMENT_3D('',#53576,#38408,#38409);
#33030=AXIS2_PLACEMENT_3D('',#53581,#38412,#38413);
#33031=AXIS2_PLACEMENT_3D('',#53582,#38414,#38415);
#33032=AXIS2_PLACEMENT_3D('',#53587,#38418,#38419);
#33033=AXIS2_PLACEMENT_3D('',#53588,#38420,#38421);
#33034=AXIS2_PLACEMENT_3D('',#53593,#38424,#38425);
#33035=AXIS2_PLACEMENT_3D('',#53594,#38426,#38427);
#33036=AXIS2_PLACEMENT_3D('',#53599,#38430,#38431);
#33037=AXIS2_PLACEMENT_3D('',#53600,#38432,#38433);
#33038=AXIS2_PLACEMENT_3D('',#53605,#38436,#38437);
#33039=AXIS2_PLACEMENT_3D('',#53606,#38438,#38439);
#33040=AXIS2_PLACEMENT_3D('',#53611,#38442,#38443);
#33041=AXIS2_PLACEMENT_3D('',#53612,#38444,#38445);
#33042=AXIS2_PLACEMENT_3D('',#53617,#38448,#38449);
#33043=AXIS2_PLACEMENT_3D('',#53618,#38450,#38451);
#33044=AXIS2_PLACEMENT_3D('',#53623,#38454,#38455);
#33045=AXIS2_PLACEMENT_3D('',#53624,#38456,#38457);
#33046=AXIS2_PLACEMENT_3D('',#53629,#38460,#38461);
#33047=AXIS2_PLACEMENT_3D('',#53630,#38462,#38463);
#33048=AXIS2_PLACEMENT_3D('',#53635,#38466,#38467);
#33049=AXIS2_PLACEMENT_3D('',#53636,#38468,#38469);
#33050=AXIS2_PLACEMENT_3D('',#53641,#38472,#38473);
#33051=AXIS2_PLACEMENT_3D('',#53642,#38474,#38475);
#33052=AXIS2_PLACEMENT_3D('',#53647,#38478,#38479);
#33053=AXIS2_PLACEMENT_3D('',#53648,#38480,#38481);
#33054=AXIS2_PLACEMENT_3D('',#53653,#38484,#38485);
#33055=AXIS2_PLACEMENT_3D('',#53654,#38486,#38487);
#33056=AXIS2_PLACEMENT_3D('',#53659,#38490,#38491);
#33057=AXIS2_PLACEMENT_3D('',#53660,#38492,#38493);
#33058=AXIS2_PLACEMENT_3D('',#53665,#38496,#38497);
#33059=AXIS2_PLACEMENT_3D('',#53666,#38498,#38499);
#33060=AXIS2_PLACEMENT_3D('',#53671,#38502,#38503);
#33061=AXIS2_PLACEMENT_3D('',#53672,#38504,#38505);
#33062=AXIS2_PLACEMENT_3D('',#53677,#38508,#38509);
#33063=AXIS2_PLACEMENT_3D('',#53678,#38510,#38511);
#33064=AXIS2_PLACEMENT_3D('',#53683,#38514,#38515);
#33065=AXIS2_PLACEMENT_3D('',#53684,#38516,#38517);
#33066=AXIS2_PLACEMENT_3D('',#53688,#38519,#38520);
#33067=AXIS2_PLACEMENT_3D('',#53690,#38522,#38523);
#33068=AXIS2_PLACEMENT_3D('',#53694,#38525,#38526);
#33069=AXIS2_PLACEMENT_3D('',#53696,#38528,#38529);
#33070=AXIS2_PLACEMENT_3D('',#53700,#38531,#38532);
#33071=AXIS2_PLACEMENT_3D('',#53702,#38534,#38535);
#33072=AXIS2_PLACEMENT_3D('',#53706,#38537,#38538);
#33073=AXIS2_PLACEMENT_3D('',#53708,#38540,#38541);
#33074=AXIS2_PLACEMENT_3D('',#53712,#38543,#38544);
#33075=AXIS2_PLACEMENT_3D('',#53714,#38546,#38547);
#33076=AXIS2_PLACEMENT_3D('',#53718,#38549,#38550);
#33077=AXIS2_PLACEMENT_3D('',#53720,#38552,#38553);
#33078=AXIS2_PLACEMENT_3D('',#53724,#38555,#38556);
#33079=AXIS2_PLACEMENT_3D('',#53726,#38558,#38559);
#33080=AXIS2_PLACEMENT_3D('',#53730,#38561,#38562);
#33081=AXIS2_PLACEMENT_3D('',#53732,#38564,#38565);
#33082=AXIS2_PLACEMENT_3D('',#53736,#38567,#38568);
#33083=AXIS2_PLACEMENT_3D('',#53738,#38570,#38571);
#33084=AXIS2_PLACEMENT_3D('',#53742,#38573,#38574);
#33085=AXIS2_PLACEMENT_3D('',#53744,#38576,#38577);
#33086=AXIS2_PLACEMENT_3D('',#53748,#38579,#38580);
#33087=AXIS2_PLACEMENT_3D('',#53750,#38582,#38583);
#33088=AXIS2_PLACEMENT_3D('',#53754,#38585,#38586);
#33089=AXIS2_PLACEMENT_3D('',#53756,#38588,#38589);
#33090=AXIS2_PLACEMENT_3D('',#53760,#38591,#38592);
#33091=AXIS2_PLACEMENT_3D('',#53762,#38594,#38595);
#33092=AXIS2_PLACEMENT_3D('',#53766,#38597,#38598);
#33093=AXIS2_PLACEMENT_3D('',#53768,#38600,#38601);
#33094=AXIS2_PLACEMENT_3D('',#53773,#38604,#38605);
#33095=AXIS2_PLACEMENT_3D('',#53774,#38606,#38607);
#33096=AXIS2_PLACEMENT_3D('',#53775,#38608,#38609);
#33097=AXIS2_PLACEMENT_3D('',#53776,#38610,#38611);
#33098=AXIS2_PLACEMENT_3D('',#53777,#38612,#38613);
#33099=AXIS2_PLACEMENT_3D('',#53778,#38614,#38615);
#33100=AXIS2_PLACEMENT_3D('',#53779,#38616,#38617);
#33101=AXIS2_PLACEMENT_3D('',#53780,#38618,#38619);
#33102=AXIS2_PLACEMENT_3D('',#53781,#38620,#38621);
#33103=AXIS2_PLACEMENT_3D('',#53782,#38622,#38623);
#33104=AXIS2_PLACEMENT_3D('',#53783,#38624,#38625);
#33105=AXIS2_PLACEMENT_3D('',#53784,#38626,#38627);
#33106=AXIS2_PLACEMENT_3D('',#53785,#38628,#38629);
#33107=AXIS2_PLACEMENT_3D('',#53786,#38630,#38631);
#33108=AXIS2_PLACEMENT_3D('',#53787,#38632,#38633);
#33109=AXIS2_PLACEMENT_3D('',#53788,#38634,#38635);
#33110=AXIS2_PLACEMENT_3D('',#53789,#38636,#38637);
#33111=AXIS2_PLACEMENT_3D('',#53790,#38638,#38639);
#33112=AXIS2_PLACEMENT_3D('',#53791,#38640,#38641);
#33113=AXIS2_PLACEMENT_3D('',#53792,#38642,#38643);
#33114=AXIS2_PLACEMENT_3D('',#53793,#38644,#38645);
#33115=AXIS2_PLACEMENT_3D('',#53794,#38646,#38647);
#33116=AXIS2_PLACEMENT_3D('',#53795,#38648,#38649);
#33117=AXIS2_PLACEMENT_3D('',#53796,#38650,#38651);
#33118=AXIS2_PLACEMENT_3D('',#53797,#38652,#38653);
#33119=AXIS2_PLACEMENT_3D('',#53798,#38654,#38655);
#33120=AXIS2_PLACEMENT_3D('',#53799,#38656,#38657);
#33121=AXIS2_PLACEMENT_3D('',#53800,#38658,#38659);
#33122=AXIS2_PLACEMENT_3D('',#53801,#38660,#38661);
#33123=AXIS2_PLACEMENT_3D('',#53802,#38662,#38663);
#33124=AXIS2_PLACEMENT_3D('',#53803,#38664,#38665);
#33125=AXIS2_PLACEMENT_3D('',#53804,#38666,#38667);
#33126=AXIS2_PLACEMENT_3D('',#53805,#38668,#38669);
#33127=AXIS2_PLACEMENT_3D('',#53806,#38670,#38671);
#33128=AXIS2_PLACEMENT_3D('',#53807,#38672,#38673);
#33129=AXIS2_PLACEMENT_3D('',#53808,#38674,#38675);
#33130=AXIS2_PLACEMENT_3D('',#53809,#38676,#38677);
#33131=AXIS2_PLACEMENT_3D('',#53810,#38678,#38679);
#33132=AXIS2_PLACEMENT_3D('',#53811,#38680,#38681);
#33133=AXIS2_PLACEMENT_3D('',#53812,#38682,#38683);
#33134=AXIS2_PLACEMENT_3D('',#53813,#38684,#38685);
#33135=AXIS2_PLACEMENT_3D('',#53814,#38686,#38687);
#33136=AXIS2_PLACEMENT_3D('',#53815,#38688,#38689);
#33137=AXIS2_PLACEMENT_3D('',#53816,#38690,#38691);
#33138=AXIS2_PLACEMENT_3D('',#53817,#38692,#38693);
#33139=AXIS2_PLACEMENT_3D('',#53818,#38694,#38695);
#33140=AXIS2_PLACEMENT_3D('',#53819,#38696,#38697);
#33141=AXIS2_PLACEMENT_3D('',#53820,#38698,#38699);
#33142=AXIS2_PLACEMENT_3D('',#53821,#38700,#38701);
#33143=AXIS2_PLACEMENT_3D('',#53822,#38702,#38703);
#33144=AXIS2_PLACEMENT_3D('',#53823,#38704,#38705);
#33145=AXIS2_PLACEMENT_3D('',#53824,#38706,#38707);
#33146=AXIS2_PLACEMENT_3D('',#53825,#38708,#38709);
#33147=AXIS2_PLACEMENT_3D('',#53826,#38710,#38711);
#33148=AXIS2_PLACEMENT_3D('',#53827,#38712,#38713);
#33149=AXIS2_PLACEMENT_3D('',#53828,#38714,#38715);
#33150=AXIS2_PLACEMENT_3D('',#53829,#38716,#38717);
#33151=AXIS2_PLACEMENT_3D('',#53830,#38718,#38719);
#33152=AXIS2_PLACEMENT_3D('',#53831,#38720,#38721);
#33153=AXIS2_PLACEMENT_3D('',#53832,#38722,#38723);
#33154=AXIS2_PLACEMENT_3D('',#53833,#38724,#38725);
#33155=AXIS2_PLACEMENT_3D('',#53834,#38726,#38727);
#33156=AXIS2_PLACEMENT_3D('',#53835,#38728,#38729);
#33157=AXIS2_PLACEMENT_3D('',#53836,#38730,#38731);
#33158=AXIS2_PLACEMENT_3D('',#53837,#38732,#38733);
#33159=AXIS2_PLACEMENT_3D('',#53838,#38734,#38735);
#33160=AXIS2_PLACEMENT_3D('',#53839,#38736,#38737);
#33161=AXIS2_PLACEMENT_3D('',#53840,#38738,#38739);
#33162=AXIS2_PLACEMENT_3D('',#53841,#38740,#38741);
#33163=AXIS2_PLACEMENT_3D('',#53842,#38742,#38743);
#33164=AXIS2_PLACEMENT_3D('',#53843,#38744,#38745);
#33165=AXIS2_PLACEMENT_3D('',#53844,#38746,#38747);
#33166=AXIS2_PLACEMENT_3D('',#53845,#38748,#38749);
#33167=AXIS2_PLACEMENT_3D('',#53846,#38750,#38751);
#33168=AXIS2_PLACEMENT_3D('',#53847,#38752,#38753);
#33169=AXIS2_PLACEMENT_3D('',#53848,#38754,#38755);
#33170=AXIS2_PLACEMENT_3D('',#53849,#38756,#38757);
#33171=AXIS2_PLACEMENT_3D('',#53850,#38758,#38759);
#33172=AXIS2_PLACEMENT_3D('',#53851,#38760,#38761);
#33173=AXIS2_PLACEMENT_3D('',#53852,#38762,#38763);
#33174=AXIS2_PLACEMENT_3D('',#53853,#38764,#38765);
#33175=AXIS2_PLACEMENT_3D('',#53854,#38766,#38767);
#33176=AXIS2_PLACEMENT_3D('',#53855,#38768,#38769);
#33177=AXIS2_PLACEMENT_3D('',#53856,#38770,#38771);
#33178=AXIS2_PLACEMENT_3D('',#53857,#38772,#38773);
#33179=AXIS2_PLACEMENT_3D('',#53858,#38774,#38775);
#33180=AXIS2_PLACEMENT_3D('',#53859,#38776,#38777);
#33181=AXIS2_PLACEMENT_3D('',#53860,#38778,#38779);
#33182=AXIS2_PLACEMENT_3D('',#53861,#38780,#38781);
#33183=AXIS2_PLACEMENT_3D('',#53862,#38782,#38783);
#33184=AXIS2_PLACEMENT_3D('',#53863,#38784,#38785);
#33185=AXIS2_PLACEMENT_3D('',#53864,#38786,#38787);
#33186=AXIS2_PLACEMENT_3D('',#53865,#38788,#38789);
#33187=AXIS2_PLACEMENT_3D('',#53866,#38790,#38791);
#33188=AXIS2_PLACEMENT_3D('',#53867,#38792,#38793);
#33189=AXIS2_PLACEMENT_3D('',#53868,#38794,#38795);
#33190=AXIS2_PLACEMENT_3D('',#53869,#38796,#38797);
#33191=AXIS2_PLACEMENT_3D('',#53870,#38798,#38799);
#33192=AXIS2_PLACEMENT_3D('',#53871,#38800,#38801);
#33193=AXIS2_PLACEMENT_3D('',#53872,#38802,#38803);
#33194=AXIS2_PLACEMENT_3D('',#53873,#38804,#38805);
#33195=AXIS2_PLACEMENT_3D('',#53874,#38806,#38807);
#33196=AXIS2_PLACEMENT_3D('',#53875,#38808,#38809);
#33197=AXIS2_PLACEMENT_3D('',#53876,#38810,#38811);
#33198=AXIS2_PLACEMENT_3D('',#53877,#38812,#38813);
#33199=AXIS2_PLACEMENT_3D('',#53878,#38814,#38815);
#33200=AXIS2_PLACEMENT_3D('',#53879,#38816,#38817);
#33201=AXIS2_PLACEMENT_3D('',#53880,#38818,#38819);
#33202=AXIS2_PLACEMENT_3D('',#53881,#38820,#38821);
#33203=AXIS2_PLACEMENT_3D('',#53882,#38822,#38823);
#33204=AXIS2_PLACEMENT_3D('',#53883,#38824,#38825);
#33205=AXIS2_PLACEMENT_3D('',#53884,#38826,#38827);
#33206=AXIS2_PLACEMENT_3D('',#53885,#38828,#38829);
#33207=AXIS2_PLACEMENT_3D('',#53886,#38830,#38831);
#33208=AXIS2_PLACEMENT_3D('',#53887,#38832,#38833);
#33209=AXIS2_PLACEMENT_3D('',#53888,#38834,#38835);
#33210=AXIS2_PLACEMENT_3D('',#53889,#38836,#38837);
#33211=AXIS2_PLACEMENT_3D('',#53890,#38838,#38839);
#33212=AXIS2_PLACEMENT_3D('',#53891,#38840,#38841);
#33213=AXIS2_PLACEMENT_3D('',#53892,#38842,#38843);
#33214=AXIS2_PLACEMENT_3D('',#53893,#38844,#38845);
#33215=AXIS2_PLACEMENT_3D('',#53894,#38846,#38847);
#33216=AXIS2_PLACEMENT_3D('',#53895,#38848,#38849);
#33217=AXIS2_PLACEMENT_3D('',#53896,#38850,#38851);
#33218=AXIS2_PLACEMENT_3D('',#53897,#38852,#38853);
#33219=AXIS2_PLACEMENT_3D('',#53898,#38854,#38855);
#33220=AXIS2_PLACEMENT_3D('',#53899,#38856,#38857);
#33221=AXIS2_PLACEMENT_3D('',#53900,#38858,#38859);
#33222=AXIS2_PLACEMENT_3D('',#53901,#38860,#38861);
#33223=AXIS2_PLACEMENT_3D('',#53902,#38862,#38863);
#33224=AXIS2_PLACEMENT_3D('',#53903,#38864,#38865);
#33225=AXIS2_PLACEMENT_3D('',#53904,#38866,#38867);
#33226=AXIS2_PLACEMENT_3D('',#53905,#38868,#38869);
#33227=AXIS2_PLACEMENT_3D('',#53906,#38870,#38871);
#33228=AXIS2_PLACEMENT_3D('',#53907,#38872,#38873);
#33229=AXIS2_PLACEMENT_3D('',#53908,#38874,#38875);
#33230=AXIS2_PLACEMENT_3D('',#53909,#38876,#38877);
#33231=AXIS2_PLACEMENT_3D('',#53910,#38878,#38879);
#33232=AXIS2_PLACEMENT_3D('',#53911,#38880,#38881);
#33233=AXIS2_PLACEMENT_3D('',#53912,#38882,#38883);
#33234=AXIS2_PLACEMENT_3D('',#53913,#38884,#38885);
#33235=AXIS2_PLACEMENT_3D('',#53914,#38886,#38887);
#33236=AXIS2_PLACEMENT_3D('',#53915,#38888,#38889);
#33237=AXIS2_PLACEMENT_3D('',#53916,#38890,#38891);
#33238=AXIS2_PLACEMENT_3D('',#53917,#38892,#38893);
#33239=AXIS2_PLACEMENT_3D('',#53918,#38894,#38895);
#33240=AXIS2_PLACEMENT_3D('',#53919,#38896,#38897);
#33241=AXIS2_PLACEMENT_3D('',#53920,#38898,#38899);
#33242=AXIS2_PLACEMENT_3D('',#53921,#38900,#38901);
#33243=AXIS2_PLACEMENT_3D('',#53922,#38902,#38903);
#33244=AXIS2_PLACEMENT_3D('',#53923,#38904,#38905);
#33245=AXIS2_PLACEMENT_3D('',#53924,#38906,#38907);
#33246=AXIS2_PLACEMENT_3D('',#53925,#38908,#38909);
#33247=AXIS2_PLACEMENT_3D('',#53926,#38910,#38911);
#33248=AXIS2_PLACEMENT_3D('',#53927,#38912,#38913);
#33249=AXIS2_PLACEMENT_3D('',#53928,#38914,#38915);
#33250=AXIS2_PLACEMENT_3D('',#53929,#38916,#38917);
#33251=AXIS2_PLACEMENT_3D('',#53930,#38918,#38919);
#33252=AXIS2_PLACEMENT_3D('',#53931,#38920,#38921);
#33253=AXIS2_PLACEMENT_3D('',#53932,#38922,#38923);
#33254=AXIS2_PLACEMENT_3D('',#53933,#38924,#38925);
#33255=AXIS2_PLACEMENT_3D('',#53934,#38926,#38927);
#33256=AXIS2_PLACEMENT_3D('',#53935,#38928,#38929);
#33257=AXIS2_PLACEMENT_3D('',#53936,#38930,#38931);
#33258=AXIS2_PLACEMENT_3D('',#53937,#38932,#38933);
#33259=AXIS2_PLACEMENT_3D('',#53938,#38934,#38935);
#33260=AXIS2_PLACEMENT_3D('',#53939,#38936,#38937);
#33261=AXIS2_PLACEMENT_3D('',#53940,#38938,#38939);
#33262=AXIS2_PLACEMENT_3D('',#53941,#38940,#38941);
#33263=AXIS2_PLACEMENT_3D('',#53942,#38942,#38943);
#33264=AXIS2_PLACEMENT_3D('',#53943,#38944,#38945);
#33265=AXIS2_PLACEMENT_3D('',#53944,#38946,#38947);
#33266=AXIS2_PLACEMENT_3D('',#53945,#38948,#38949);
#33267=AXIS2_PLACEMENT_3D('',#53946,#38950,#38951);
#33268=AXIS2_PLACEMENT_3D('',#53947,#38952,#38953);
#33269=AXIS2_PLACEMENT_3D('',#53948,#38954,#38955);
#33270=AXIS2_PLACEMENT_3D('',#53949,#38956,#38957);
#33271=AXIS2_PLACEMENT_3D('',#53950,#38958,#38959);
#33272=AXIS2_PLACEMENT_3D('',#53951,#38960,#38961);
#33273=AXIS2_PLACEMENT_3D('',#53952,#38962,#38963);
#33274=AXIS2_PLACEMENT_3D('',#53953,#38964,#38965);
#33275=AXIS2_PLACEMENT_3D('',#53954,#38966,#38967);
#33276=AXIS2_PLACEMENT_3D('',#53955,#38968,#38969);
#33277=AXIS2_PLACEMENT_3D('',#53956,#38970,#38971);
#33278=AXIS2_PLACEMENT_3D('',#53957,#38972,#38973);
#33279=AXIS2_PLACEMENT_3D('',#53958,#38974,#38975);
#33280=AXIS2_PLACEMENT_3D('',#53959,#38976,#38977);
#33281=AXIS2_PLACEMENT_3D('',#53960,#38978,#38979);
#33282=AXIS2_PLACEMENT_3D('',#53961,#38980,#38981);
#33283=AXIS2_PLACEMENT_3D('',#53962,#38982,#38983);
#33284=AXIS2_PLACEMENT_3D('',#53963,#38984,#38985);
#33285=AXIS2_PLACEMENT_3D('',#53964,#38986,#38987);
#33286=AXIS2_PLACEMENT_3D('',#53965,#38988,#38989);
#33287=AXIS2_PLACEMENT_3D('',#53966,#38990,#38991);
#33288=AXIS2_PLACEMENT_3D('',#53967,#38992,#38993);
#33289=AXIS2_PLACEMENT_3D('',#53968,#38994,#38995);
#33290=AXIS2_PLACEMENT_3D('',#53969,#38996,#38997);
#33291=AXIS2_PLACEMENT_3D('',#53970,#38998,#38999);
#33292=AXIS2_PLACEMENT_3D('',#53971,#39000,#39001);
#33293=AXIS2_PLACEMENT_3D('',#53972,#39002,#39003);
#33294=AXIS2_PLACEMENT_3D('',#53973,#39004,#39005);
#33295=AXIS2_PLACEMENT_3D('',#53974,#39006,#39007);
#33296=AXIS2_PLACEMENT_3D('',#53975,#39008,#39009);
#33297=AXIS2_PLACEMENT_3D('',#53976,#39010,#39011);
#33298=AXIS2_PLACEMENT_3D('',#53977,#39012,#39013);
#33299=AXIS2_PLACEMENT_3D('',#53978,#39014,#39015);
#33300=AXIS2_PLACEMENT_3D('',#53979,#39016,#39017);
#33301=AXIS2_PLACEMENT_3D('',#53980,#39018,#39019);
#33302=AXIS2_PLACEMENT_3D('',#53981,#39020,#39021);
#33303=AXIS2_PLACEMENT_3D('',#53982,#39022,#39023);
#33304=AXIS2_PLACEMENT_3D('',#53983,#39024,#39025);
#33305=AXIS2_PLACEMENT_3D('',#53984,#39026,#39027);
#33306=AXIS2_PLACEMENT_3D('',#53985,#39028,#39029);
#33307=AXIS2_PLACEMENT_3D('',#53986,#39030,#39031);
#33308=AXIS2_PLACEMENT_3D('',#53987,#39032,#39033);
#33309=AXIS2_PLACEMENT_3D('',#53988,#39034,#39035);
#33310=AXIS2_PLACEMENT_3D('',#53989,#39036,#39037);
#33311=AXIS2_PLACEMENT_3D('',#53990,#39038,#39039);
#33312=AXIS2_PLACEMENT_3D('',#53991,#39040,#39041);
#33313=AXIS2_PLACEMENT_3D('',#53992,#39042,#39043);
#33314=AXIS2_PLACEMENT_3D('',#53993,#39044,#39045);
#33315=AXIS2_PLACEMENT_3D('',#53994,#39046,#39047);
#33316=AXIS2_PLACEMENT_3D('',#53995,#39048,#39049);
#33317=AXIS2_PLACEMENT_3D('',#53996,#39050,#39051);
#33318=AXIS2_PLACEMENT_3D('',#53997,#39052,#39053);
#33319=AXIS2_PLACEMENT_3D('',#53998,#39054,#39055);
#33320=AXIS2_PLACEMENT_3D('',#53999,#39056,#39057);
#33321=AXIS2_PLACEMENT_3D('',#54000,#39058,#39059);
#33322=AXIS2_PLACEMENT_3D('',#54001,#39060,#39061);
#33323=AXIS2_PLACEMENT_3D('',#54002,#39062,#39063);
#33324=AXIS2_PLACEMENT_3D('',#54003,#39064,#39065);
#33325=AXIS2_PLACEMENT_3D('',#54004,#39066,#39067);
#33326=AXIS2_PLACEMENT_3D('',#54005,#39068,#39069);
#33327=AXIS2_PLACEMENT_3D('',#54006,#39070,#39071);
#33328=AXIS2_PLACEMENT_3D('',#54007,#39072,#39073);
#33329=AXIS2_PLACEMENT_3D('',#54008,#39074,#39075);
#33330=AXIS2_PLACEMENT_3D('',#54009,#39076,#39077);
#33331=AXIS2_PLACEMENT_3D('',#54010,#39078,#39079);
#33332=AXIS2_PLACEMENT_3D('',#54011,#39080,#39081);
#33333=AXIS2_PLACEMENT_3D('',#54012,#39082,#39083);
#33334=AXIS2_PLACEMENT_3D('',#54013,#39084,#39085);
#33335=AXIS2_PLACEMENT_3D('',#54015,#39086,#39087);
#33336=AXIS2_PLACEMENT_3D('',#54017,#39088,#39089);
#33337=AXIS2_PLACEMENT_3D('',#54018,#39090,#39091);
#33338=AXIS2_PLACEMENT_3D('',#54019,#39092,#39093);
#33339=AXIS2_PLACEMENT_3D('',#54024,#39096,#39097);
#33340=AXIS2_PLACEMENT_3D('',#54025,#39098,#39099);
#33341=AXIS2_PLACEMENT_3D('',#54026,#39100,#39101);
#33342=AXIS2_PLACEMENT_3D('',#54027,#39102,#39103);
#33343=AXIS2_PLACEMENT_3D('',#54028,#39104,#39105);
#33344=AXIS2_PLACEMENT_3D('',#54029,#39106,#39107);
#33345=AXIS2_PLACEMENT_3D('',#54042,#39114,#39115);
#33346=AXIS2_PLACEMENT_3D('',#54045,#39118,#39119);
#33347=AXIS2_PLACEMENT_3D('',#54047,#39121,#39122);
#33348=AXIS2_PLACEMENT_3D('',#54049,#39124,#39125);
#33349=AXIS2_PLACEMENT_3D('',#54051,#39127,#39128);
#33350=AXIS2_PLACEMENT_3D('',#54053,#39130,#39131);
#33351=AXIS2_PLACEMENT_3D('',#55575,#39133,#39134);
#33352=AXIS2_PLACEMENT_3D('',#55576,#39135,#39136);
#33353=AXIS2_PLACEMENT_3D('',#55578,#39138,#39139);
#33354=AXIS2_PLACEMENT_3D('',#55580,#39141,#39142);
#33355=AXIS2_PLACEMENT_3D('',#55581,#39143,#39144);
#33356=AXIS2_PLACEMENT_3D('',#55583,#39146,#39147);
#33357=AXIS2_PLACEMENT_3D('',#55585,#39149,#39150);
#33358=AXIS2_PLACEMENT_3D('',#55586,#39151,#39152);
#33359=AXIS2_PLACEMENT_3D('',#55588,#39154,#39155);
#33360=AXIS2_PLACEMENT_3D('',#55590,#39157,#39158);
#33361=AXIS2_PLACEMENT_3D('',#55591,#39159,#39160);
#33362=AXIS2_PLACEMENT_3D('',#55593,#39162,#39163);
#33363=AXIS2_PLACEMENT_3D('',#55595,#39165,#39166);
#33364=AXIS2_PLACEMENT_3D('',#55596,#39167,#39168);
#33365=AXIS2_PLACEMENT_3D('',#55598,#39170,#39171);
#33366=AXIS2_PLACEMENT_3D('',#55600,#39173,#39174);
#33367=AXIS2_PLACEMENT_3D('',#55601,#39175,#39176);
#33368=AXIS2_PLACEMENT_3D('',#55603,#39178,#39179);
#33369=AXIS2_PLACEMENT_3D('',#55605,#39181,#39182);
#33370=AXIS2_PLACEMENT_3D('',#55606,#39183,#39184);
#33371=AXIS2_PLACEMENT_3D('',#55608,#39186,#39187);
#33372=AXIS2_PLACEMENT_3D('',#55610,#39189,#39190);
#33373=AXIS2_PLACEMENT_3D('',#55611,#39191,#39192);
#33374=AXIS2_PLACEMENT_3D('',#55612,#39193,#39194);
#33375=AXIS2_PLACEMENT_3D('',#55613,#39195,#39196);
#33376=AXIS2_PLACEMENT_3D('',#55614,#39197,#39198);
#33377=AXIS2_PLACEMENT_3D('',#55615,#39199,#39200);
#33378=AXIS2_PLACEMENT_3D('',#55616,#39201,#39202);
#33379=AXIS2_PLACEMENT_3D('',#55617,#39203,#39204);
#33380=AXIS2_PLACEMENT_3D('',#55618,#39205,#39206);
#33381=AXIS2_PLACEMENT_3D('',#55619,#39207,#39208);
#33382=AXIS2_PLACEMENT_3D('',#55620,#39209,#39210);
#33383=AXIS2_PLACEMENT_3D('',#55621,#39211,#39212);
#33384=AXIS2_PLACEMENT_3D('',#55622,#39213,#39214);
#33385=AXIS2_PLACEMENT_3D('',#55623,#39215,#39216);
#33386=AXIS2_PLACEMENT_3D('',#55624,#39217,#39218);
#33387=AXIS2_PLACEMENT_3D('',#55625,#39219,#39220);
#33388=AXIS2_PLACEMENT_3D('',#55626,#39221,#39222);
#33389=AXIS2_PLACEMENT_3D('',#55627,#39223,#39224);
#33390=AXIS2_PLACEMENT_3D('',#55628,#39225,#39226);
#33391=AXIS2_PLACEMENT_3D('',#55629,#39227,#39228);
#33392=AXIS2_PLACEMENT_3D('',#55631,#39230,#39231);
#33393=AXIS2_PLACEMENT_3D('',#55633,#39233,#39234);
#33394=AXIS2_PLACEMENT_3D('',#55634,#39235,#39236);
#33395=AXIS2_PLACEMENT_3D('',#55636,#39238,#39239);
#33396=AXIS2_PLACEMENT_3D('',#55638,#39241,#39242);
#33397=AXIS2_PLACEMENT_3D('',#55639,#39243,#39244);
#33398=AXIS2_PLACEMENT_3D('',#55641,#39246,#39247);
#33399=AXIS2_PLACEMENT_3D('',#55643,#39249,#39250);
#33400=AXIS2_PLACEMENT_3D('',#55644,#39251,#39252);
#33401=AXIS2_PLACEMENT_3D('',#55646,#39254,#39255);
#33402=AXIS2_PLACEMENT_3D('',#55648,#39257,#39258);
#33403=AXIS2_PLACEMENT_3D('',#55649,#39259,#39260);
#33404=AXIS2_PLACEMENT_3D('',#55651,#39262,#39263);
#33405=AXIS2_PLACEMENT_3D('',#55653,#39265,#39266);
#33406=AXIS2_PLACEMENT_3D('',#55654,#39267,#39268);
#33407=AXIS2_PLACEMENT_3D('',#55656,#39270,#39271);
#33408=AXIS2_PLACEMENT_3D('',#55658,#39273,#39274);
#33409=AXIS2_PLACEMENT_3D('',#55659,#39275,#39276);
#33410=AXIS2_PLACEMENT_3D('',#55661,#39278,#39279);
#33411=AXIS2_PLACEMENT_3D('',#55663,#39281,#39282);
#33412=AXIS2_PLACEMENT_3D('',#55664,#39283,#39284);
#33413=AXIS2_PLACEMENT_3D('',#55666,#39286,#39287);
#33414=AXIS2_PLACEMENT_3D('',#55668,#39289,#39290);
#33415=AXIS2_PLACEMENT_3D('',#55669,#39291,#39292);
#33416=AXIS2_PLACEMENT_3D('',#55671,#39294,#39295);
#33417=AXIS2_PLACEMENT_3D('',#55673,#39297,#39298);
#33418=AXIS2_PLACEMENT_3D('',#55674,#39299,#39300);
#33419=AXIS2_PLACEMENT_3D('',#55676,#39302,#39303);
#33420=AXIS2_PLACEMENT_3D('',#55678,#39305,#39306);
#33421=AXIS2_PLACEMENT_3D('',#55679,#39307,#39308);
#33422=AXIS2_PLACEMENT_3D('',#55681,#39310,#39311);
#33423=AXIS2_PLACEMENT_3D('',#55683,#39313,#39314);
#33424=AXIS2_PLACEMENT_3D('',#55684,#39315,#39316);
#33425=AXIS2_PLACEMENT_3D('',#55686,#39318,#39319);
#33426=AXIS2_PLACEMENT_3D('',#55688,#39321,#39322);
#33427=AXIS2_PLACEMENT_3D('',#55689,#39323,#39324);
#33428=AXIS2_PLACEMENT_3D('',#55691,#39326,#39327);
#33429=AXIS2_PLACEMENT_3D('',#55693,#39329,#39330);
#33430=AXIS2_PLACEMENT_3D('',#55694,#39331,#39332);
#33431=AXIS2_PLACEMENT_3D('',#55696,#39334,#39335);
#33432=AXIS2_PLACEMENT_3D('',#55698,#39337,#39338);
#33433=AXIS2_PLACEMENT_3D('',#55699,#39339,#39340);
#33434=AXIS2_PLACEMENT_3D('',#55701,#39342,#39343);
#33435=AXIS2_PLACEMENT_3D('',#55703,#39345,#39346);
#33436=AXIS2_PLACEMENT_3D('',#55704,#39347,#39348);
#33437=AXIS2_PLACEMENT_3D('',#55706,#39350,#39351);
#33438=AXIS2_PLACEMENT_3D('',#55708,#39353,#39354);
#33439=AXIS2_PLACEMENT_3D('',#55709,#39355,#39356);
#33440=AXIS2_PLACEMENT_3D('',#55711,#39358,#39359);
#33441=AXIS2_PLACEMENT_3D('',#55713,#39361,#39362);
#33442=AXIS2_PLACEMENT_3D('',#55714,#39363,#39364);
#33443=AXIS2_PLACEMENT_3D('',#55716,#39366,#39367);
#33444=AXIS2_PLACEMENT_3D('',#55718,#39369,#39370);
#33445=AXIS2_PLACEMENT_3D('',#55719,#39371,#39372);
#33446=AXIS2_PLACEMENT_3D('',#55721,#39374,#39375);
#33447=AXIS2_PLACEMENT_3D('',#55723,#39377,#39378);
#33448=AXIS2_PLACEMENT_3D('',#55724,#39379,#39380);
#33449=AXIS2_PLACEMENT_3D('',#55726,#39382,#39383);
#33450=AXIS2_PLACEMENT_3D('',#55728,#39385,#39386);
#33451=AXIS2_PLACEMENT_3D('',#55729,#39387,#39388);
#33452=AXIS2_PLACEMENT_3D('',#55731,#39390,#39391);
#33453=AXIS2_PLACEMENT_3D('',#55733,#39393,#39394);
#33454=AXIS2_PLACEMENT_3D('',#55734,#39395,#39396);
#33455=AXIS2_PLACEMENT_3D('',#55736,#39398,#39399);
#33456=AXIS2_PLACEMENT_3D('',#55738,#39401,#39402);
#33457=AXIS2_PLACEMENT_3D('',#55739,#39403,#39404);
#33458=AXIS2_PLACEMENT_3D('',#55741,#39406,#39407);
#33459=AXIS2_PLACEMENT_3D('',#55743,#39409,#39410);
#33460=AXIS2_PLACEMENT_3D('',#55744,#39411,#39412);
#33461=AXIS2_PLACEMENT_3D('',#55746,#39414,#39415);
#33462=AXIS2_PLACEMENT_3D('',#55748,#39417,#39418);
#33463=AXIS2_PLACEMENT_3D('',#55749,#39419,#39420);
#33464=AXIS2_PLACEMENT_3D('',#55751,#39422,#39423);
#33465=AXIS2_PLACEMENT_3D('',#55753,#39425,#39426);
#33466=AXIS2_PLACEMENT_3D('',#55754,#39427,#39428);
#33467=AXIS2_PLACEMENT_3D('',#55756,#39430,#39431);
#33468=AXIS2_PLACEMENT_3D('',#55758,#39433,#39434);
#33469=AXIS2_PLACEMENT_3D('',#55759,#39435,#39436);
#33470=AXIS2_PLACEMENT_3D('',#55761,#39438,#39439);
#33471=AXIS2_PLACEMENT_3D('',#55763,#39441,#39442);
#33472=AXIS2_PLACEMENT_3D('',#55764,#39443,#39444);
#33473=AXIS2_PLACEMENT_3D('',#55766,#39446,#39447);
#33474=AXIS2_PLACEMENT_3D('',#55768,#39449,#39450);
#33475=AXIS2_PLACEMENT_3D('',#55769,#39451,#39452);
#33476=AXIS2_PLACEMENT_3D('',#55771,#39454,#39455);
#33477=AXIS2_PLACEMENT_3D('',#55773,#39457,#39458);
#33478=AXIS2_PLACEMENT_3D('',#55774,#39459,#39460);
#33479=AXIS2_PLACEMENT_3D('',#55776,#39462,#39463);
#33480=AXIS2_PLACEMENT_3D('',#55778,#39465,#39466);
#33481=AXIS2_PLACEMENT_3D('',#55779,#39467,#39468);
#33482=AXIS2_PLACEMENT_3D('',#55781,#39470,#39471);
#33483=AXIS2_PLACEMENT_3D('',#55783,#39473,#39474);
#33484=AXIS2_PLACEMENT_3D('',#55784,#39475,#39476);
#33485=AXIS2_PLACEMENT_3D('',#55786,#39478,#39479);
#33486=AXIS2_PLACEMENT_3D('',#55788,#39481,#39482);
#33487=AXIS2_PLACEMENT_3D('',#55789,#39483,#39484);
#33488=AXIS2_PLACEMENT_3D('',#55791,#39486,#39487);
#33489=AXIS2_PLACEMENT_3D('',#55793,#39489,#39490);
#33490=AXIS2_PLACEMENT_3D('',#55794,#39491,#39492);
#33491=AXIS2_PLACEMENT_3D('',#55796,#39494,#39495);
#33492=AXIS2_PLACEMENT_3D('',#55798,#39497,#39498);
#33493=AXIS2_PLACEMENT_3D('',#55799,#39499,#39500);
#33494=AXIS2_PLACEMENT_3D('',#55801,#39502,#39503);
#33495=AXIS2_PLACEMENT_3D('',#55803,#39505,#39506);
#33496=AXIS2_PLACEMENT_3D('',#55804,#39507,#39508);
#33497=AXIS2_PLACEMENT_3D('',#55806,#39510,#39511);
#33498=AXIS2_PLACEMENT_3D('',#55808,#39513,#39514);
#33499=AXIS2_PLACEMENT_3D('',#55809,#39515,#39516);
#33500=AXIS2_PLACEMENT_3D('',#55811,#39518,#39519);
#33501=AXIS2_PLACEMENT_3D('',#55813,#39521,#39522);
#33502=AXIS2_PLACEMENT_3D('',#55814,#39523,#39524);
#33503=AXIS2_PLACEMENT_3D('',#55816,#39526,#39527);
#33504=AXIS2_PLACEMENT_3D('',#55818,#39529,#39530);
#33505=AXIS2_PLACEMENT_3D('',#55819,#39531,#39532);
#33506=AXIS2_PLACEMENT_3D('',#55821,#39534,#39535);
#33507=AXIS2_PLACEMENT_3D('',#55823,#39537,#39538);
#33508=AXIS2_PLACEMENT_3D('',#55824,#39539,#39540);
#33509=AXIS2_PLACEMENT_3D('',#55826,#39542,#39543);
#33510=AXIS2_PLACEMENT_3D('',#55828,#39545,#39546);
#33511=AXIS2_PLACEMENT_3D('',#55829,#39547,#39548);
#33512=AXIS2_PLACEMENT_3D('',#55831,#39550,#39551);
#33513=AXIS2_PLACEMENT_3D('',#55833,#39553,#39554);
#33514=AXIS2_PLACEMENT_3D('',#55834,#39555,#39556);
#33515=AXIS2_PLACEMENT_3D('',#55836,#39558,#39559);
#33516=AXIS2_PLACEMENT_3D('',#55838,#39561,#39562);
#33517=AXIS2_PLACEMENT_3D('',#55839,#39563,#39564);
#33518=AXIS2_PLACEMENT_3D('',#55841,#39566,#39567);
#33519=AXIS2_PLACEMENT_3D('',#55843,#39569,#39570);
#33520=AXIS2_PLACEMENT_3D('',#55844,#39571,#39572);
#33521=AXIS2_PLACEMENT_3D('',#55846,#39574,#39575);
#33522=AXIS2_PLACEMENT_3D('',#55848,#39577,#39578);
#33523=AXIS2_PLACEMENT_3D('',#55849,#39579,#39580);
#33524=AXIS2_PLACEMENT_3D('',#55851,#39582,#39583);
#33525=AXIS2_PLACEMENT_3D('',#55853,#39585,#39586);
#33526=AXIS2_PLACEMENT_3D('',#55854,#39587,#39588);
#33527=AXIS2_PLACEMENT_3D('',#55856,#39590,#39591);
#33528=AXIS2_PLACEMENT_3D('',#55858,#39593,#39594);
#33529=AXIS2_PLACEMENT_3D('',#55859,#39595,#39596);
#33530=AXIS2_PLACEMENT_3D('',#55861,#39598,#39599);
#33531=AXIS2_PLACEMENT_3D('',#55863,#39601,#39602);
#33532=AXIS2_PLACEMENT_3D('',#55864,#39603,#39604);
#33533=AXIS2_PLACEMENT_3D('',#55866,#39606,#39607);
#33534=AXIS2_PLACEMENT_3D('',#55868,#39609,#39610);
#33535=AXIS2_PLACEMENT_3D('',#55869,#39611,#39612);
#33536=AXIS2_PLACEMENT_3D('',#55871,#39614,#39615);
#33537=AXIS2_PLACEMENT_3D('',#55873,#39617,#39618);
#33538=AXIS2_PLACEMENT_3D('',#55874,#39619,#39620);
#33539=AXIS2_PLACEMENT_3D('',#55876,#39622,#39623);
#33540=AXIS2_PLACEMENT_3D('',#55878,#39625,#39626);
#33541=AXIS2_PLACEMENT_3D('',#55879,#39627,#39628);
#33542=AXIS2_PLACEMENT_3D('',#55881,#39630,#39631);
#33543=AXIS2_PLACEMENT_3D('',#55883,#39633,#39634);
#33544=AXIS2_PLACEMENT_3D('',#55884,#39635,#39636);
#33545=AXIS2_PLACEMENT_3D('',#55886,#39638,#39639);
#33546=AXIS2_PLACEMENT_3D('',#55888,#39641,#39642);
#33547=AXIS2_PLACEMENT_3D('',#55889,#39643,#39644);
#33548=AXIS2_PLACEMENT_3D('',#55891,#39646,#39647);
#33549=AXIS2_PLACEMENT_3D('',#55893,#39649,#39650);
#33550=AXIS2_PLACEMENT_3D('',#55894,#39651,#39652);
#33551=AXIS2_PLACEMENT_3D('',#55896,#39654,#39655);
#33552=AXIS2_PLACEMENT_3D('',#55898,#39657,#39658);
#33553=AXIS2_PLACEMENT_3D('',#55899,#39659,#39660);
#33554=AXIS2_PLACEMENT_3D('',#55901,#39662,#39663);
#33555=AXIS2_PLACEMENT_3D('',#55903,#39665,#39666);
#33556=AXIS2_PLACEMENT_3D('',#55904,#39667,#39668);
#33557=AXIS2_PLACEMENT_3D('',#55906,#39670,#39671);
#33558=AXIS2_PLACEMENT_3D('',#55908,#39673,#39674);
#33559=AXIS2_PLACEMENT_3D('',#55909,#39675,#39676);
#33560=AXIS2_PLACEMENT_3D('',#55911,#39678,#39679);
#33561=AXIS2_PLACEMENT_3D('',#55913,#39681,#39682);
#33562=AXIS2_PLACEMENT_3D('',#55914,#39683,#39684);
#33563=AXIS2_PLACEMENT_3D('',#55916,#39686,#39687);
#33564=AXIS2_PLACEMENT_3D('',#55918,#39689,#39690);
#33565=AXIS2_PLACEMENT_3D('',#55919,#39691,#39692);
#33566=AXIS2_PLACEMENT_3D('',#55920,#39693,#39694);
#33567=AXIS2_PLACEMENT_3D('',#55921,#39695,#39696);
#33568=AXIS2_PLACEMENT_3D('',#55922,#39697,#39698);
#33569=AXIS2_PLACEMENT_3D('',#55923,#39699,#39700);
#33570=AXIS2_PLACEMENT_3D('',#55924,#39701,#39702);
#33571=AXIS2_PLACEMENT_3D('',#55925,#39703,#39704);
#33572=AXIS2_PLACEMENT_3D('',#55926,#39705,#39706);
#33573=AXIS2_PLACEMENT_3D('',#55927,#39707,#39708);
#33574=AXIS2_PLACEMENT_3D('',#55928,#39709,#39710);
#33575=AXIS2_PLACEMENT_3D('',#55929,#39711,#39712);
#33576=AXIS2_PLACEMENT_3D('',#55930,#39713,#39714);
#33577=AXIS2_PLACEMENT_3D('',#55931,#39715,#39716);
#33578=AXIS2_PLACEMENT_3D('',#55932,#39717,#39718);
#33579=AXIS2_PLACEMENT_3D('',#55975,#39721,#39722);
#33580=AXIS2_PLACEMENT_3D('',#55977,#39723,#39724);
#33581=AXIS2_PLACEMENT_3D('',#56012,#39725,#39726);
#33582=AXIS2_PLACEMENT_3D('',#56088,#39728,#39729);
#33583=AXIS2_PLACEMENT_3D('',#56166,#39731,#39732);
#33584=AXIS2_PLACEMENT_3D('',#56242,#39734,#39735);
#33585=AXIS2_PLACEMENT_3D('',#56318,#39737,#39738);
#33586=AXIS2_PLACEMENT_3D('',#56394,#39740,#39741);
#33587=AXIS2_PLACEMENT_3D('',#56470,#39743,#39744);
#33588=AXIS2_PLACEMENT_3D('',#56548,#39746,#39747);
#33589=AXIS2_PLACEMENT_3D('',#56626,#39749,#39750);
#33590=AXIS2_PLACEMENT_3D('',#56702,#39752,#39753);
#33591=AXIS2_PLACEMENT_3D('',#56778,#39755,#39756);
#33592=AXIS2_PLACEMENT_3D('',#56854,#39758,#39759);
#33593=AXIS2_PLACEMENT_3D('',#56930,#39761,#39762);
#33594=AXIS2_PLACEMENT_3D('',#57008,#39764,#39765);
#33595=AXIS2_PLACEMENT_3D('',#57084,#39767,#39768);
#33596=AXIS2_PLACEMENT_3D('',#57162,#39770,#39771);
#33597=AXIS2_PLACEMENT_3D('',#57238,#39773,#39774);
#33598=AXIS2_PLACEMENT_3D('',#57314,#39776,#39777);
#33599=AXIS2_PLACEMENT_3D('',#57390,#39779,#39780);
#33600=AXIS2_PLACEMENT_3D('',#57466,#39782,#39783);
#33601=AXIS2_PLACEMENT_3D('',#57544,#39785,#39786);
#33602=AXIS2_PLACEMENT_3D('',#57622,#39788,#39789);
#33603=AXIS2_PLACEMENT_3D('',#57698,#39791,#39792);
#33604=AXIS2_PLACEMENT_3D('',#57774,#39794,#39795);
#33605=AXIS2_PLACEMENT_3D('',#57850,#39797,#39798);
#33606=AXIS2_PLACEMENT_3D('',#57926,#39800,#39801);
#33607=AXIS2_PLACEMENT_3D('',#58004,#39803,#39804);
#33608=AXIS2_PLACEMENT_3D('',#58080,#39806,#39807);
#33609=AXIS2_PLACEMENT_3D('',#58105,#39809,#39810);
#33610=AXIS2_PLACEMENT_3D('',#58106,#39811,#39812);
#33611=AXIS2_PLACEMENT_3D('',#58118,#39814,#39815);
#33612=AXIS2_PLACEMENT_3D('',#58119,#39816,#39817);
#33613=AXIS2_PLACEMENT_3D('',#58195,#39819,#39820);
#33614=AXIS2_PLACEMENT_3D('',#58271,#39822,#39823);
#33615=AXIS2_PLACEMENT_3D('',#58349,#39825,#39826);
#33616=AXIS2_PLACEMENT_3D('',#58425,#39828,#39829);
#33617=AXIS2_PLACEMENT_3D('',#58503,#39831,#39832);
#33618=AXIS2_PLACEMENT_3D('',#58579,#39834,#39835);
#33619=AXIS2_PLACEMENT_3D('',#58655,#39837,#39838);
#33620=AXIS2_PLACEMENT_3D('',#58731,#39840,#39841);
#33621=AXIS2_PLACEMENT_3D('',#58807,#39843,#39844);
#33622=AXIS2_PLACEMENT_3D('',#58885,#39846,#39847);
#33623=AXIS2_PLACEMENT_3D('',#58961,#39849,#39850);
#33624=AXIS2_PLACEMENT_3D('',#59039,#39852,#39853);
#33625=AXIS2_PLACEMENT_3D('',#59115,#39855,#39856);
#33626=AXIS2_PLACEMENT_3D('',#59191,#39858,#39859);
#33627=AXIS2_PLACEMENT_3D('',#59267,#39861,#39862);
#33628=AXIS2_PLACEMENT_3D('',#59343,#39864,#39865);
#33629=AXIS2_PLACEMENT_3D('',#59419,#39867,#39868);
#33630=AXIS2_PLACEMENT_3D('',#59497,#39870,#39871);
#33631=AXIS2_PLACEMENT_3D('',#59573,#39873,#39874);
#33632=AXIS2_PLACEMENT_3D('',#59651,#39876,#39877);
#33633=AXIS2_PLACEMENT_3D('',#59727,#39879,#39880);
#33634=AXIS2_PLACEMENT_3D('',#59803,#39882,#39883);
#33635=AXIS2_PLACEMENT_3D('',#59879,#39885,#39886);
#33636=AXIS2_PLACEMENT_3D('',#59955,#39888,#39889);
#33637=AXIS2_PLACEMENT_3D('',#60033,#39891,#39892);
#33638=AXIS2_PLACEMENT_3D('',#60109,#39894,#39895);
#33639=AXIS2_PLACEMENT_3D('',#60187,#39897,#39898);
#33640=AXIS2_PLACEMENT_3D('',#60263,#39900,#39901);
#33641=AXIS2_PLACEMENT_3D('',#60339,#39903,#39904);
#33642=AXIS2_PLACEMENT_3D('',#60349,#39905,#39906);
#33643=AXIS2_PLACEMENT_3D('',#60350,#39907,#39908);
#33644=AXIS2_PLACEMENT_3D('',#60351,#39909,#39910);
#33645=AXIS2_PLACEMENT_3D('',#60366,#39911,#39912);
#33646=AXIS2_PLACEMENT_3D('',#60389,#39913,#39914);
#33647=AXIS2_PLACEMENT_3D('',#60456,#39915,#39916);
#33648=AXIS2_PLACEMENT_3D('',#60459,#39917,#39918);
#33649=AXIS2_PLACEMENT_3D('',#60463,#39920,#39921);
#33650=AXIS2_PLACEMENT_3D('',#60465,#39923,#39924);
#33651=AXIS2_PLACEMENT_3D('',#60468,#39925,#39926);
#33652=AXIS2_PLACEMENT_3D('',#60472,#39928,#39929);
#33653=AXIS2_PLACEMENT_3D('',#60474,#39931,#39932);
#33654=AXIS2_PLACEMENT_3D('',#60477,#39933,#39934);
#33655=AXIS2_PLACEMENT_3D('',#60481,#39936,#39937);
#33656=AXIS2_PLACEMENT_3D('',#60483,#39939,#39940);
#33657=AXIS2_PLACEMENT_3D('',#60486,#39941,#39942);
#33658=AXIS2_PLACEMENT_3D('',#60490,#39944,#39945);
#33659=AXIS2_PLACEMENT_3D('',#60492,#39947,#39948);
#33660=AXIS2_PLACEMENT_3D('',#60495,#39949,#39950);
#33661=AXIS2_PLACEMENT_3D('',#60499,#39952,#39953);
#33662=AXIS2_PLACEMENT_3D('',#60501,#39955,#39956);
#33663=AXIS2_PLACEMENT_3D('',#60504,#39957,#39958);
#33664=AXIS2_PLACEMENT_3D('',#60508,#39960,#39961);
#33665=AXIS2_PLACEMENT_3D('',#60510,#39963,#39964);
#33666=AXIS2_PLACEMENT_3D('',#60513,#39965,#39966);
#33667=AXIS2_PLACEMENT_3D('',#60517,#39968,#39969);
#33668=AXIS2_PLACEMENT_3D('',#60519,#39971,#39972);
#33669=AXIS2_PLACEMENT_3D('',#60522,#39973,#39974);
#33670=AXIS2_PLACEMENT_3D('',#60526,#39976,#39977);
#33671=AXIS2_PLACEMENT_3D('',#60528,#39979,#39980);
#33672=AXIS2_PLACEMENT_3D('',#60531,#39981,#39982);
#33673=AXIS2_PLACEMENT_3D('',#60535,#39984,#39985);
#33674=AXIS2_PLACEMENT_3D('',#60537,#39987,#39988);
#33675=AXIS2_PLACEMENT_3D('',#60540,#39989,#39990);
#33676=AXIS2_PLACEMENT_3D('',#60544,#39992,#39993);
#33677=AXIS2_PLACEMENT_3D('',#60546,#39995,#39996);
#33678=AXIS2_PLACEMENT_3D('',#60549,#39997,#39998);
#33679=AXIS2_PLACEMENT_3D('',#60553,#40000,#40001);
#33680=AXIS2_PLACEMENT_3D('',#60555,#40003,#40004);
#33681=AXIS2_PLACEMENT_3D('',#60558,#40005,#40006);
#33682=AXIS2_PLACEMENT_3D('',#60562,#40008,#40009);
#33683=AXIS2_PLACEMENT_3D('',#60564,#40011,#40012);
#33684=AXIS2_PLACEMENT_3D('',#60567,#40013,#40014);
#33685=AXIS2_PLACEMENT_3D('',#60571,#40016,#40017);
#33686=AXIS2_PLACEMENT_3D('',#60573,#40019,#40020);
#33687=AXIS2_PLACEMENT_3D('',#60576,#40021,#40022);
#33688=AXIS2_PLACEMENT_3D('',#60580,#40024,#40025);
#33689=AXIS2_PLACEMENT_3D('',#60582,#40027,#40028);
#33690=AXIS2_PLACEMENT_3D('',#60585,#40029,#40030);
#33691=AXIS2_PLACEMENT_3D('',#60589,#40032,#40033);
#33692=AXIS2_PLACEMENT_3D('',#60591,#40035,#40036);
#33693=AXIS2_PLACEMENT_3D('',#60622,#40038,#40039);
#33694=AXIS2_PLACEMENT_3D('',#60623,#40040,#40041);
#33695=AXIS2_PLACEMENT_3D('',#60625,#40042,#40043);
#33696=AXIS2_PLACEMENT_3D('',#60627,#40044,#40045);
#33697=AXIS2_PLACEMENT_3D('',#60628,#40046,#40047);
#33698=AXIS2_PLACEMENT_3D('',#60629,#40048,#40049);
#33699=AXIS2_PLACEMENT_3D('',#60645,#40050,#40051);
#33700=AXIS2_PLACEMENT_3D('',#60651,#40052,#40053);
#33701=AXIS2_PLACEMENT_3D('',#60657,#40054,#40055);
#33702=AXIS2_PLACEMENT_3D('',#60663,#40056,#40057);
#33703=AXIS2_PLACEMENT_3D('',#60669,#40058,#40059);
#33704=AXIS2_PLACEMENT_3D('',#60675,#40060,#40061);
#33705=AXIS2_PLACEMENT_3D('',#60681,#40062,#40063);
#33706=AXIS2_PLACEMENT_3D('',#60687,#40064,#40065);
#33707=AXIS2_PLACEMENT_3D('',#60693,#40066,#40067);
#33708=AXIS2_PLACEMENT_3D('',#60699,#40068,#40069);
#33709=AXIS2_PLACEMENT_3D('',#60705,#40070,#40071);
#33710=AXIS2_PLACEMENT_3D('',#60711,#40072,#40073);
#33711=AXIS2_PLACEMENT_3D('',#60717,#40074,#40075);
#33712=AXIS2_PLACEMENT_3D('',#60723,#40076,#40077);
#33713=AXIS2_PLACEMENT_3D('',#60729,#40078,#40079);
#33714=AXIS2_PLACEMENT_3D('',#60735,#40080,#40081);
#33715=AXIS2_PLACEMENT_3D('',#60741,#40082,#40083);
#33716=AXIS2_PLACEMENT_3D('',#60747,#40084,#40085);
#33717=AXIS2_PLACEMENT_3D('',#60753,#40086,#40087);
#33718=AXIS2_PLACEMENT_3D('',#60759,#40088,#40089);
#33719=AXIS2_PLACEMENT_3D('',#60765,#40090,#40091);
#33720=AXIS2_PLACEMENT_3D('',#60771,#40092,#40093);
#33721=AXIS2_PLACEMENT_3D('',#60777,#40094,#40095);
#33722=AXIS2_PLACEMENT_3D('',#60783,#40096,#40097);
#33723=AXIS2_PLACEMENT_3D('',#60789,#40098,#40099);
#33724=AXIS2_PLACEMENT_3D('',#60795,#40100,#40101);
#33725=AXIS2_PLACEMENT_3D('',#60801,#40102,#40103);
#33726=AXIS2_PLACEMENT_3D('',#60807,#40104,#40105);
#33727=AXIS2_PLACEMENT_3D('',#60813,#40106,#40107);
#33728=AXIS2_PLACEMENT_3D('',#60819,#40108,#40109);
#33729=AXIS2_PLACEMENT_3D('',#60825,#40110,#40111);
#33730=AXIS2_PLACEMENT_3D('',#60831,#40112,#40113);
#33731=AXIS2_PLACEMENT_3D('',#60837,#40114,#40115);
#33732=AXIS2_PLACEMENT_3D('',#60843,#40116,#40117);
#33733=AXIS2_PLACEMENT_3D('',#60849,#40118,#40119);
#33734=AXIS2_PLACEMENT_3D('',#60855,#40120,#40121);
#33735=AXIS2_PLACEMENT_3D('',#60861,#40122,#40123);
#33736=AXIS2_PLACEMENT_3D('',#60867,#40124,#40125);
#33737=AXIS2_PLACEMENT_3D('',#60873,#40126,#40127);
#33738=AXIS2_PLACEMENT_3D('',#60879,#40128,#40129);
#33739=AXIS2_PLACEMENT_3D('',#60885,#40130,#40131);
#33740=AXIS2_PLACEMENT_3D('',#60891,#40132,#40133);
#33741=AXIS2_PLACEMENT_3D('',#60897,#40134,#40135);
#33742=AXIS2_PLACEMENT_3D('',#60903,#40136,#40137);
#33743=AXIS2_PLACEMENT_3D('',#60909,#40138,#40139);
#33744=AXIS2_PLACEMENT_3D('',#60915,#40140,#40141);
#33745=AXIS2_PLACEMENT_3D('',#60921,#40142,#40143);
#33746=AXIS2_PLACEMENT_3D('',#60927,#40144,#40145);
#33747=AXIS2_PLACEMENT_3D('',#60933,#40146,#40147);
#33748=AXIS2_PLACEMENT_3D('',#60939,#40148,#40149);
#33749=AXIS2_PLACEMENT_3D('',#60945,#40150,#40151);
#33750=AXIS2_PLACEMENT_3D('',#60951,#40152,#40153);
#33751=AXIS2_PLACEMENT_3D('',#60957,#40154,#40155);
#33752=AXIS2_PLACEMENT_3D('',#60963,#40156,#40157);
#33753=AXIS2_PLACEMENT_3D('',#60969,#40158,#40159);
#33754=AXIS2_PLACEMENT_3D('',#60975,#40160,#40161);
#33755=AXIS2_PLACEMENT_3D('',#60981,#40162,#40163);
#33756=AXIS2_PLACEMENT_3D('',#60987,#40164,#40165);
#33757=AXIS2_PLACEMENT_3D('',#60993,#40166,#40167);
#33758=AXIS2_PLACEMENT_3D('',#60999,#40168,#40169);
#33759=AXIS2_PLACEMENT_3D('',#61005,#40170,#40171);
#33760=AXIS2_PLACEMENT_3D('',#61011,#40172,#40173);
#33761=AXIS2_PLACEMENT_3D('',#61017,#40174,#40175);
#33762=AXIS2_PLACEMENT_3D('',#61023,#40176,#40177);
#33763=AXIS2_PLACEMENT_3D('',#61029,#40178,#40179);
#33764=AXIS2_PLACEMENT_3D('',#61035,#40180,#40181);
#33765=AXIS2_PLACEMENT_3D('',#61041,#40182,#40183);
#33766=AXIS2_PLACEMENT_3D('',#61047,#40184,#40185);
#33767=AXIS2_PLACEMENT_3D('',#61053,#40186,#40187);
#33768=AXIS2_PLACEMENT_3D('',#61059,#40188,#40189);
#33769=AXIS2_PLACEMENT_3D('',#61065,#40190,#40191);
#33770=AXIS2_PLACEMENT_3D('',#61071,#40192,#40193);
#33771=AXIS2_PLACEMENT_3D('',#61077,#40194,#40195);
#33772=AXIS2_PLACEMENT_3D('',#61083,#40196,#40197);
#33773=AXIS2_PLACEMENT_3D('',#61089,#40198,#40199);
#33774=AXIS2_PLACEMENT_3D('',#61095,#40200,#40201);
#33775=AXIS2_PLACEMENT_3D('',#61101,#40202,#40203);
#33776=AXIS2_PLACEMENT_3D('',#61107,#40204,#40205);
#33777=AXIS2_PLACEMENT_3D('',#61113,#40206,#40207);
#33778=AXIS2_PLACEMENT_3D('',#61119,#40208,#40209);
#33779=AXIS2_PLACEMENT_3D('',#61125,#40210,#40211);
#33780=AXIS2_PLACEMENT_3D('',#61131,#40212,#40213);
#33781=AXIS2_PLACEMENT_3D('',#61137,#40214,#40215);
#33782=AXIS2_PLACEMENT_3D('',#61143,#40216,#40217);
#33783=AXIS2_PLACEMENT_3D('',#61149,#40218,#40219);
#33784=AXIS2_PLACEMENT_3D('',#61155,#40220,#40221);
#33785=AXIS2_PLACEMENT_3D('',#61161,#40222,#40223);
#33786=AXIS2_PLACEMENT_3D('',#61167,#40224,#40225);
#33787=AXIS2_PLACEMENT_3D('',#61173,#40226,#40227);
#33788=AXIS2_PLACEMENT_3D('',#61179,#40228,#40229);
#33789=AXIS2_PLACEMENT_3D('',#61185,#40230,#40231);
#33790=AXIS2_PLACEMENT_3D('',#61194,#40232,#40233);
#33791=AXIS2_PLACEMENT_3D('',#61203,#40234,#40235);
#33792=AXIS2_PLACEMENT_3D('',#61212,#40236,#40237);
#33793=AXIS2_PLACEMENT_3D('',#61221,#40238,#40239);
#33794=AXIS2_PLACEMENT_3D('',#61230,#40240,#40241);
#33795=AXIS2_PLACEMENT_3D('',#61239,#40242,#40243);
#33796=AXIS2_PLACEMENT_3D('',#61248,#40244,#40245);
#33797=AXIS2_PLACEMENT_3D('',#61257,#40246,#40247);
#33798=AXIS2_PLACEMENT_3D('',#61266,#40248,#40249);
#33799=AXIS2_PLACEMENT_3D('',#61275,#40250,#40251);
#33800=AXIS2_PLACEMENT_3D('',#61284,#40252,#40253);
#33801=AXIS2_PLACEMENT_3D('',#61293,#40254,#40255);
#33802=AXIS2_PLACEMENT_3D('',#61302,#40256,#40257);
#33803=AXIS2_PLACEMENT_3D('',#61311,#40258,#40259);
#33804=AXIS2_PLACEMENT_3D('',#61320,#40260,#40261);
#33805=AXIS2_PLACEMENT_3D('',#61326,#40262,#40263);
#33806=AXIS2_PLACEMENT_3D('',#61332,#40264,#40265);
#33807=AXIS2_PLACEMENT_3D('',#61338,#40266,#40267);
#33808=AXIS2_PLACEMENT_3D('',#61344,#40268,#40269);
#33809=AXIS2_PLACEMENT_3D('',#61350,#40270,#40271);
#33810=AXIS2_PLACEMENT_3D('',#61356,#40272,#40273);
#33811=AXIS2_PLACEMENT_3D('',#61362,#40274,#40275);
#33812=AXIS2_PLACEMENT_3D('',#61368,#40276,#40277);
#33813=AXIS2_PLACEMENT_3D('',#61374,#40278,#40279);
#33814=AXIS2_PLACEMENT_3D('',#61380,#40280,#40281);
#33815=AXIS2_PLACEMENT_3D('',#61386,#40282,#40283);
#33816=AXIS2_PLACEMENT_3D('',#61392,#40284,#40285);
#33817=AXIS2_PLACEMENT_3D('',#61398,#40286,#40287);
#33818=AXIS2_PLACEMENT_3D('',#61404,#40288,#40289);
#33819=AXIS2_PLACEMENT_3D('',#61410,#40290,#40291);
#33820=AXIS2_PLACEMENT_3D('',#61416,#40292,#40293);
#33821=AXIS2_PLACEMENT_3D('',#61422,#40294,#40295);
#33822=AXIS2_PLACEMENT_3D('',#61428,#40296,#40297);
#33823=AXIS2_PLACEMENT_3D('',#61434,#40298,#40299);
#33824=AXIS2_PLACEMENT_3D('',#61440,#40300,#40301);
#33825=AXIS2_PLACEMENT_3D('',#61446,#40302,#40303);
#33826=AXIS2_PLACEMENT_3D('',#61452,#40304,#40305);
#33827=AXIS2_PLACEMENT_3D('',#61458,#40306,#40307);
#33828=AXIS2_PLACEMENT_3D('',#61464,#40308,#40309);
#33829=AXIS2_PLACEMENT_3D('',#61470,#40310,#40311);
#33830=AXIS2_PLACEMENT_3D('',#61476,#40312,#40313);
#33831=AXIS2_PLACEMENT_3D('',#61482,#40314,#40315);
#33832=AXIS2_PLACEMENT_3D('',#61488,#40316,#40317);
#33833=AXIS2_PLACEMENT_3D('',#61494,#40318,#40319);
#33834=AXIS2_PLACEMENT_3D('',#61500,#40320,#40321);
#33835=AXIS2_PLACEMENT_3D('',#61506,#40322,#40323);
#33836=AXIS2_PLACEMENT_3D('',#61512,#40324,#40325);
#33837=AXIS2_PLACEMENT_3D('',#61518,#40326,#40327);
#33838=AXIS2_PLACEMENT_3D('',#61524,#40328,#40329);
#33839=AXIS2_PLACEMENT_3D('',#61530,#40330,#40331);
#33840=AXIS2_PLACEMENT_3D('',#61536,#40332,#40333);
#33841=AXIS2_PLACEMENT_3D('',#61542,#40334,#40335);
#33842=AXIS2_PLACEMENT_3D('',#61548,#40336,#40337);
#33843=AXIS2_PLACEMENT_3D('',#61562,#40339,#40340);
#33844=AXIS2_PLACEMENT_3D('',#61578,#40341,#40342);
#33845=AXIS2_PLACEMENT_3D('',#61584,#40343,#40344);
#33846=AXIS2_PLACEMENT_3D('',#61590,#40345,#40346);
#33847=AXIS2_PLACEMENT_3D('',#61596,#40347,#40348);
#33848=AXIS2_PLACEMENT_3D('',#61602,#40349,#40350);
#33849=AXIS2_PLACEMENT_3D('',#61608,#40351,#40352);
#33850=AXIS2_PLACEMENT_3D('',#61614,#40353,#40354);
#33851=AXIS2_PLACEMENT_3D('',#61620,#40355,#40356);
#33852=AXIS2_PLACEMENT_3D('',#61626,#40357,#40358);
#33853=AXIS2_PLACEMENT_3D('',#61632,#40359,#40360);
#33854=AXIS2_PLACEMENT_3D('',#61638,#40361,#40362);
#33855=AXIS2_PLACEMENT_3D('',#61644,#40363,#40364);
#33856=AXIS2_PLACEMENT_3D('',#61650,#40365,#40366);
#33857=AXIS2_PLACEMENT_3D('',#61656,#40367,#40368);
#33858=AXIS2_PLACEMENT_3D('',#61662,#40369,#40370);
#33859=AXIS2_PLACEMENT_3D('',#61668,#40371,#40372);
#33860=AXIS2_PLACEMENT_3D('',#61674,#40373,#40374);
#33861=AXIS2_PLACEMENT_3D('',#61680,#40375,#40376);
#33862=AXIS2_PLACEMENT_3D('',#61686,#40377,#40378);
#33863=AXIS2_PLACEMENT_3D('',#61692,#40379,#40380);
#33864=AXIS2_PLACEMENT_3D('',#61698,#40381,#40382);
#33865=AXIS2_PLACEMENT_3D('',#61704,#40383,#40384);
#33866=AXIS2_PLACEMENT_3D('',#61710,#40385,#40386);
#33867=AXIS2_PLACEMENT_3D('',#61716,#40387,#40388);
#33868=AXIS2_PLACEMENT_3D('',#61722,#40389,#40390);
#33869=AXIS2_PLACEMENT_3D('',#61728,#40391,#40392);
#33870=AXIS2_PLACEMENT_3D('',#61734,#40393,#40394);
#33871=AXIS2_PLACEMENT_3D('',#61740,#40395,#40396);
#33872=AXIS2_PLACEMENT_3D('',#61746,#40397,#40398);
#33873=AXIS2_PLACEMENT_3D('',#61752,#40399,#40400);
#33874=AXIS2_PLACEMENT_3D('',#61758,#40401,#40402);
#33875=AXIS2_PLACEMENT_3D('',#61764,#40403,#40404);
#33876=AXIS2_PLACEMENT_3D('',#61770,#40405,#40406);
#33877=AXIS2_PLACEMENT_3D('',#61776,#40407,#40408);
#33878=AXIS2_PLACEMENT_3D('',#61782,#40409,#40410);
#33879=AXIS2_PLACEMENT_3D('',#61788,#40411,#40412);
#33880=AXIS2_PLACEMENT_3D('',#61794,#40413,#40414);
#33881=AXIS2_PLACEMENT_3D('',#61800,#40415,#40416);
#33882=AXIS2_PLACEMENT_3D('',#61806,#40417,#40418);
#33883=AXIS2_PLACEMENT_3D('',#61812,#40419,#40420);
#33884=AXIS2_PLACEMENT_3D('',#61818,#40421,#40422);
#33885=AXIS2_PLACEMENT_3D('',#61824,#40423,#40424);
#33886=AXIS2_PLACEMENT_3D('',#61830,#40425,#40426);
#33887=AXIS2_PLACEMENT_3D('',#61836,#40427,#40428);
#33888=AXIS2_PLACEMENT_3D('',#61842,#40429,#40430);
#33889=AXIS2_PLACEMENT_3D('',#61848,#40431,#40432);
#33890=AXIS2_PLACEMENT_3D('',#61854,#40433,#40434);
#33891=AXIS2_PLACEMENT_3D('',#61860,#40435,#40436);
#33892=AXIS2_PLACEMENT_3D('',#61866,#40437,#40438);
#33893=AXIS2_PLACEMENT_3D('',#61872,#40439,#40440);
#33894=AXIS2_PLACEMENT_3D('',#61878,#40441,#40442);
#33895=AXIS2_PLACEMENT_3D('',#61884,#40443,#40444);
#33896=AXIS2_PLACEMENT_3D('',#61890,#40445,#40446);
#33897=AXIS2_PLACEMENT_3D('',#61896,#40447,#40448);
#33898=AXIS2_PLACEMENT_3D('',#61902,#40449,#40450);
#33899=AXIS2_PLACEMENT_3D('',#61908,#40451,#40452);
#33900=AXIS2_PLACEMENT_3D('',#61914,#40453,#40454);
#33901=AXIS2_PLACEMENT_3D('',#61920,#40455,#40456);
#33902=AXIS2_PLACEMENT_3D('',#61926,#40457,#40458);
#33903=AXIS2_PLACEMENT_3D('',#61932,#40459,#40460);
#33904=AXIS2_PLACEMENT_3D('',#61938,#40461,#40462);
#33905=AXIS2_PLACEMENT_3D('',#61944,#40463,#40464);
#33906=AXIS2_PLACEMENT_3D('',#61950,#40465,#40466);
#33907=AXIS2_PLACEMENT_3D('',#61956,#40467,#40468);
#33908=AXIS2_PLACEMENT_3D('',#61962,#40469,#40470);
#33909=AXIS2_PLACEMENT_3D('',#61968,#40471,#40472);
#33910=AXIS2_PLACEMENT_3D('',#61974,#40473,#40474);
#33911=AXIS2_PLACEMENT_3D('',#61980,#40475,#40476);
#33912=AXIS2_PLACEMENT_3D('',#61986,#40477,#40478);
#33913=AXIS2_PLACEMENT_3D('',#61992,#40479,#40480);
#33914=AXIS2_PLACEMENT_3D('',#61998,#40481,#40482);
#33915=AXIS2_PLACEMENT_3D('',#62004,#40483,#40484);
#33916=AXIS2_PLACEMENT_3D('',#62010,#40485,#40486);
#33917=AXIS2_PLACEMENT_3D('',#62016,#40487,#40488);
#33918=AXIS2_PLACEMENT_3D('',#62022,#40489,#40490);
#33919=AXIS2_PLACEMENT_3D('',#62028,#40491,#40492);
#33920=AXIS2_PLACEMENT_3D('',#62034,#40493,#40494);
#33921=AXIS2_PLACEMENT_3D('',#62040,#40495,#40496);
#33922=AXIS2_PLACEMENT_3D('',#62046,#40497,#40498);
#33923=AXIS2_PLACEMENT_3D('',#62052,#40499,#40500);
#33924=AXIS2_PLACEMENT_3D('',#62058,#40501,#40502);
#33925=AXIS2_PLACEMENT_3D('',#62064,#40503,#40504);
#33926=AXIS2_PLACEMENT_3D('',#62070,#40505,#40506);
#33927=AXIS2_PLACEMENT_3D('',#62076,#40507,#40508);
#33928=AXIS2_PLACEMENT_3D('',#62082,#40509,#40510);
#33929=AXIS2_PLACEMENT_3D('',#62088,#40511,#40512);
#33930=AXIS2_PLACEMENT_3D('',#62094,#40513,#40514);
#33931=AXIS2_PLACEMENT_3D('',#62100,#40515,#40516);
#33932=AXIS2_PLACEMENT_3D('',#62106,#40517,#40518);
#33933=AXIS2_PLACEMENT_3D('',#62112,#40519,#40520);
#33934=AXIS2_PLACEMENT_3D('',#62118,#40521,#40522);
#33935=AXIS2_PLACEMENT_3D('',#62124,#40523,#40524);
#33936=AXIS2_PLACEMENT_3D('',#62130,#40525,#40526);
#33937=AXIS2_PLACEMENT_3D('',#62136,#40527,#40528);
#33938=AXIS2_PLACEMENT_3D('',#62142,#40529,#40530);
#33939=AXIS2_PLACEMENT_3D('',#62148,#40531,#40532);
#33940=AXIS2_PLACEMENT_3D('',#62154,#40533,#40534);
#33941=AXIS2_PLACEMENT_3D('',#62160,#40535,#40536);
#33942=AXIS2_PLACEMENT_3D('',#62166,#40537,#40538);
#33943=AXIS2_PLACEMENT_3D('',#62172,#40539,#40540);
#33944=AXIS2_PLACEMENT_3D('',#62178,#40541,#40542);
#33945=AXIS2_PLACEMENT_3D('',#62184,#40543,#40544);
#33946=AXIS2_PLACEMENT_3D('',#62190,#40545,#40546);
#33947=AXIS2_PLACEMENT_3D('',#62196,#40547,#40548);
#33948=AXIS2_PLACEMENT_3D('',#62202,#40549,#40550);
#33949=AXIS2_PLACEMENT_3D('',#62208,#40551,#40552);
#33950=AXIS2_PLACEMENT_3D('',#62214,#40553,#40554);
#33951=AXIS2_PLACEMENT_3D('',#62220,#40555,#40556);
#33952=AXIS2_PLACEMENT_3D('',#62226,#40557,#40558);
#33953=AXIS2_PLACEMENT_3D('',#62232,#40559,#40560);
#33954=AXIS2_PLACEMENT_3D('',#62238,#40561,#40562);
#33955=AXIS2_PLACEMENT_3D('',#62244,#40563,#40564);
#33956=AXIS2_PLACEMENT_3D('',#62250,#40565,#40566);
#33957=AXIS2_PLACEMENT_3D('',#62256,#40567,#40568);
#33958=AXIS2_PLACEMENT_3D('',#62262,#40569,#40570);
#33959=AXIS2_PLACEMENT_3D('',#62268,#40571,#40572);
#33960=AXIS2_PLACEMENT_3D('',#62274,#40573,#40574);
#33961=AXIS2_PLACEMENT_3D('',#62280,#40575,#40576);
#33962=AXIS2_PLACEMENT_3D('',#62286,#40577,#40578);
#33963=AXIS2_PLACEMENT_3D('',#62295,#40579,#40580);
#33964=AXIS2_PLACEMENT_3D('',#62304,#40581,#40582);
#33965=AXIS2_PLACEMENT_3D('',#62313,#40583,#40584);
#33966=AXIS2_PLACEMENT_3D('',#62322,#40585,#40586);
#33967=AXIS2_PLACEMENT_3D('',#62331,#40587,#40588);
#33968=AXIS2_PLACEMENT_3D('',#62340,#40589,#40590);
#33969=AXIS2_PLACEMENT_3D('',#62349,#40591,#40592);
#33970=AXIS2_PLACEMENT_3D('',#62358,#40593,#40594);
#33971=AXIS2_PLACEMENT_3D('',#62367,#40595,#40596);
#33972=AXIS2_PLACEMENT_3D('',#62376,#40597,#40598);
#33973=AXIS2_PLACEMENT_3D('',#62385,#40599,#40600);
#33974=AXIS2_PLACEMENT_3D('',#62394,#40601,#40602);
#33975=AXIS2_PLACEMENT_3D('',#62403,#40603,#40604);
#33976=AXIS2_PLACEMENT_3D('',#62412,#40605,#40606);
#33977=AXIS2_PLACEMENT_3D('',#62421,#40607,#40608);
#33978=AXIS2_PLACEMENT_3D('',#62427,#40609,#40610);
#33979=AXIS2_PLACEMENT_3D('',#62433,#40611,#40612);
#33980=AXIS2_PLACEMENT_3D('',#62439,#40613,#40614);
#33981=AXIS2_PLACEMENT_3D('',#62445,#40615,#40616);
#33982=AXIS2_PLACEMENT_3D('',#62451,#40617,#40618);
#33983=AXIS2_PLACEMENT_3D('',#62457,#40619,#40620);
#33984=AXIS2_PLACEMENT_3D('',#62463,#40621,#40622);
#33985=AXIS2_PLACEMENT_3D('',#62469,#40623,#40624);
#33986=AXIS2_PLACEMENT_3D('',#62475,#40625,#40626);
#33987=AXIS2_PLACEMENT_3D('',#62481,#40627,#40628);
#33988=AXIS2_PLACEMENT_3D('',#62497,#40630,#40631);
#33989=AXIS2_PLACEMENT_3D('',#62498,#40632,#40633);
#33990=AXIS2_PLACEMENT_3D('',#62499,#40634,#40635);
#33991=AXIS2_PLACEMENT_3D('',#62501,#40636,#40637);
#33992=AXIS2_PLACEMENT_3D('',#62502,#40638,#40639);
#33993=AXIS2_PLACEMENT_3D('',#62503,#40640,#40641);
#33994=AXIS2_PLACEMENT_3D('',#62505,#40642,#40643);
#33995=AXIS2_PLACEMENT_3D('',#62507,#40645,#40646);
#33996=AXIS2_PLACEMENT_3D('',#62509,#40647,#40648);
#33997=AXIS2_PLACEMENT_3D('',#62510,#40649,#40650);
#33998=AXIS2_PLACEMENT_3D('',#62511,#40651,#40652);
#33999=AXIS2_PLACEMENT_3D('',#62513,#40653,#40654);
#34000=AXIS2_PLACEMENT_3D('',#62514,#40655,#40656);
#34001=AXIS2_PLACEMENT_3D('',#62515,#40657,#40658);
#34002=AXIS2_PLACEMENT_3D('',#62517,#40659,#40660);
#34003=AXIS2_PLACEMENT_3D('',#62519,#40661,#40662);
#34004=AXIS2_PLACEMENT_3D('',#62520,#40663,#40664);
#34005=AXIS2_PLACEMENT_3D('',#62521,#40665,#40666);
#34006=AXIS2_PLACEMENT_3D('',#62523,#40667,#40668);
#34007=AXIS2_PLACEMENT_3D('',#62525,#40669,#40670);
#34008=AXIS2_PLACEMENT_3D('',#62526,#40671,#40672);
#34009=AXIS2_PLACEMENT_3D('',#62527,#40673,#40674);
#34010=AXIS2_PLACEMENT_3D('',#62529,#40675,#40676);
#34011=AXIS2_PLACEMENT_3D('',#62531,#40677,#40678);
#34012=AXIS2_PLACEMENT_3D('',#62532,#40679,#40680);
#34013=AXIS2_PLACEMENT_3D('',#62533,#40681,#40682);
#34014=AXIS2_PLACEMENT_3D('',#62535,#40683,#40684);
#34015=AXIS2_PLACEMENT_3D('',#62537,#40685,#40686);
#34016=AXIS2_PLACEMENT_3D('',#62538,#40687,#40688);
#34017=AXIS2_PLACEMENT_3D('',#62539,#40689,#40690);
#34018=AXIS2_PLACEMENT_3D('',#62541,#40691,#40692);
#34019=AXIS2_PLACEMENT_3D('',#62543,#40693,#40694);
#34020=AXIS2_PLACEMENT_3D('',#62544,#40695,#40696);
#34021=AXIS2_PLACEMENT_3D('',#62545,#40697,#40698);
#34022=AXIS2_PLACEMENT_3D('',#62547,#40699,#40700);
#34023=AXIS2_PLACEMENT_3D('',#62549,#40701,#40702);
#34024=AXIS2_PLACEMENT_3D('',#62550,#40703,#40704);
#34025=AXIS2_PLACEMENT_3D('',#62551,#40705,#40706);
#34026=AXIS2_PLACEMENT_3D('',#62553,#40707,#40708);
#34027=AXIS2_PLACEMENT_3D('',#62555,#40709,#40710);
#34028=AXIS2_PLACEMENT_3D('',#62556,#40711,#40712);
#34029=AXIS2_PLACEMENT_3D('',#62557,#40713,#40714);
#34030=AXIS2_PLACEMENT_3D('',#62559,#40715,#40716);
#34031=AXIS2_PLACEMENT_3D('',#62561,#40717,#40718);
#34032=AXIS2_PLACEMENT_3D('',#62562,#40719,#40720);
#34033=AXIS2_PLACEMENT_3D('',#62563,#40721,#40722);
#34034=AXIS2_PLACEMENT_3D('',#62565,#40723,#40724);
#34035=AXIS2_PLACEMENT_3D('',#62567,#40725,#40726);
#34036=AXIS2_PLACEMENT_3D('',#62568,#40727,#40728);
#34037=AXIS2_PLACEMENT_3D('',#62569,#40729,#40730);
#34038=AXIS2_PLACEMENT_3D('',#62571,#40731,#40732);
#34039=AXIS2_PLACEMENT_3D('',#62573,#40733,#40734);
#34040=AXIS2_PLACEMENT_3D('',#62574,#40735,#40736);
#34041=AXIS2_PLACEMENT_3D('',#62575,#40737,#40738);
#34042=AXIS2_PLACEMENT_3D('',#62577,#40739,#40740);
#34043=AXIS2_PLACEMENT_3D('',#62579,#40741,#40742);
#34044=AXIS2_PLACEMENT_3D('',#62580,#40743,#40744);
#34045=AXIS2_PLACEMENT_3D('',#62581,#40745,#40746);
#34046=AXIS2_PLACEMENT_3D('',#62583,#40747,#40748);
#34047=AXIS2_PLACEMENT_3D('',#62585,#40749,#40750);
#34048=AXIS2_PLACEMENT_3D('',#62586,#40751,#40752);
#34049=AXIS2_PLACEMENT_3D('',#62587,#40753,#40754);
#34050=AXIS2_PLACEMENT_3D('',#62589,#40755,#40756);
#34051=AXIS2_PLACEMENT_3D('',#62591,#40757,#40758);
#34052=AXIS2_PLACEMENT_3D('',#62592,#40759,#40760);
#34053=AXIS2_PLACEMENT_3D('',#62593,#40761,#40762);
#34054=AXIS2_PLACEMENT_3D('',#62595,#40763,#40764);
#34055=AXIS2_PLACEMENT_3D('',#62597,#40765,#40766);
#34056=AXIS2_PLACEMENT_3D('',#62598,#40767,#40768);
#34057=AXIS2_PLACEMENT_3D('',#62599,#40769,#40770);
#34058=AXIS2_PLACEMENT_3D('',#62601,#40771,#40772);
#34059=AXIS2_PLACEMENT_3D('',#62603,#40773,#40774);
#34060=AXIS2_PLACEMENT_3D('',#62604,#40775,#40776);
#34061=AXIS2_PLACEMENT_3D('',#62605,#40777,#40778);
#34062=AXIS2_PLACEMENT_3D('',#62607,#40779,#40780);
#34063=AXIS2_PLACEMENT_3D('',#62609,#40781,#40782);
#34064=AXIS2_PLACEMENT_3D('',#62610,#40783,#40784);
#34065=AXIS2_PLACEMENT_3D('',#62611,#40785,#40786);
#34066=AXIS2_PLACEMENT_3D('',#62613,#40787,#40788);
#34067=AXIS2_PLACEMENT_3D('',#62615,#40789,#40790);
#34068=AXIS2_PLACEMENT_3D('',#62616,#40791,#40792);
#34069=AXIS2_PLACEMENT_3D('',#62617,#40793,#40794);
#34070=AXIS2_PLACEMENT_3D('',#62619,#40795,#40796);
#34071=AXIS2_PLACEMENT_3D('',#62621,#40797,#40798);
#34072=AXIS2_PLACEMENT_3D('',#62622,#40799,#40800);
#34073=AXIS2_PLACEMENT_3D('',#62623,#40801,#40802);
#34074=AXIS2_PLACEMENT_3D('',#62625,#40803,#40804);
#34075=AXIS2_PLACEMENT_3D('',#62627,#40805,#40806);
#34076=AXIS2_PLACEMENT_3D('',#62628,#40807,#40808);
#34077=AXIS2_PLACEMENT_3D('',#62629,#40809,#40810);
#34078=AXIS2_PLACEMENT_3D('',#62631,#40811,#40812);
#34079=AXIS2_PLACEMENT_3D('',#62633,#40813,#40814);
#34080=AXIS2_PLACEMENT_3D('',#62634,#40815,#40816);
#34081=AXIS2_PLACEMENT_3D('',#62635,#40817,#40818);
#34082=AXIS2_PLACEMENT_3D('',#62637,#40819,#40820);
#34083=AXIS2_PLACEMENT_3D('',#62639,#40821,#40822);
#34084=AXIS2_PLACEMENT_3D('',#62640,#40823,#40824);
#34085=AXIS2_PLACEMENT_3D('',#62641,#40825,#40826);
#34086=AXIS2_PLACEMENT_3D('',#62643,#40827,#40828);
#34087=AXIS2_PLACEMENT_3D('',#62645,#40829,#40830);
#34088=AXIS2_PLACEMENT_3D('',#62646,#40831,#40832);
#34089=AXIS2_PLACEMENT_3D('',#62647,#40833,#40834);
#34090=AXIS2_PLACEMENT_3D('',#62649,#40835,#40836);
#34091=AXIS2_PLACEMENT_3D('',#62651,#40837,#40838);
#34092=AXIS2_PLACEMENT_3D('',#62652,#40839,#40840);
#34093=AXIS2_PLACEMENT_3D('',#62653,#40841,#40842);
#34094=AXIS2_PLACEMENT_3D('',#62655,#40843,#40844);
#34095=AXIS2_PLACEMENT_3D('',#62657,#40845,#40846);
#34096=AXIS2_PLACEMENT_3D('',#62658,#40847,#40848);
#34097=AXIS2_PLACEMENT_3D('',#62659,#40849,#40850);
#34098=AXIS2_PLACEMENT_3D('',#62661,#40851,#40852);
#34099=AXIS2_PLACEMENT_3D('',#62663,#40853,#40854);
#34100=AXIS2_PLACEMENT_3D('',#62664,#40855,#40856);
#34101=AXIS2_PLACEMENT_3D('',#62665,#40857,#40858);
#34102=AXIS2_PLACEMENT_3D('',#62667,#40859,#40860);
#34103=AXIS2_PLACEMENT_3D('',#62669,#40861,#40862);
#34104=AXIS2_PLACEMENT_3D('',#62670,#40863,#40864);
#34105=AXIS2_PLACEMENT_3D('',#62671,#40865,#40866);
#34106=AXIS2_PLACEMENT_3D('',#62673,#40867,#40868);
#34107=AXIS2_PLACEMENT_3D('',#62675,#40869,#40870);
#34108=AXIS2_PLACEMENT_3D('',#62676,#40871,#40872);
#34109=AXIS2_PLACEMENT_3D('',#62677,#40873,#40874);
#34110=AXIS2_PLACEMENT_3D('',#62679,#40875,#40876);
#34111=AXIS2_PLACEMENT_3D('',#62681,#40877,#40878);
#34112=AXIS2_PLACEMENT_3D('',#62682,#40879,#40880);
#34113=AXIS2_PLACEMENT_3D('',#62683,#40881,#40882);
#34114=AXIS2_PLACEMENT_3D('',#62685,#40883,#40884);
#34115=AXIS2_PLACEMENT_3D('',#62687,#40885,#40886);
#34116=AXIS2_PLACEMENT_3D('',#62688,#40887,#40888);
#34117=AXIS2_PLACEMENT_3D('',#62689,#40889,#40890);
#34118=AXIS2_PLACEMENT_3D('',#62691,#40891,#40892);
#34119=AXIS2_PLACEMENT_3D('',#62693,#40893,#40894);
#34120=AXIS2_PLACEMENT_3D('',#62694,#40895,#40896);
#34121=AXIS2_PLACEMENT_3D('',#62695,#40897,#40898);
#34122=AXIS2_PLACEMENT_3D('',#62697,#40899,#40900);
#34123=AXIS2_PLACEMENT_3D('',#62699,#40901,#40902);
#34124=AXIS2_PLACEMENT_3D('',#62700,#40903,#40904);
#34125=AXIS2_PLACEMENT_3D('',#62701,#40905,#40906);
#34126=AXIS2_PLACEMENT_3D('',#62703,#40907,#40908);
#34127=AXIS2_PLACEMENT_3D('',#62705,#40909,#40910);
#34128=AXIS2_PLACEMENT_3D('',#62706,#40911,#40912);
#34129=AXIS2_PLACEMENT_3D('',#62707,#40913,#40914);
#34130=AXIS2_PLACEMENT_3D('',#62709,#40915,#40916);
#34131=AXIS2_PLACEMENT_3D('',#62711,#40917,#40918);
#34132=AXIS2_PLACEMENT_3D('',#62712,#40919,#40920);
#34133=AXIS2_PLACEMENT_3D('',#62713,#40921,#40922);
#34134=AXIS2_PLACEMENT_3D('',#62715,#40923,#40924);
#34135=AXIS2_PLACEMENT_3D('',#62717,#40925,#40926);
#34136=AXIS2_PLACEMENT_3D('',#62718,#40927,#40928);
#34137=AXIS2_PLACEMENT_3D('',#62719,#40929,#40930);
#34138=AXIS2_PLACEMENT_3D('',#62721,#40931,#40932);
#34139=AXIS2_PLACEMENT_3D('',#62723,#40933,#40934);
#34140=AXIS2_PLACEMENT_3D('',#62724,#40935,#40936);
#34141=AXIS2_PLACEMENT_3D('',#62725,#40937,#40938);
#34142=AXIS2_PLACEMENT_3D('',#62727,#40939,#40940);
#34143=AXIS2_PLACEMENT_3D('',#62729,#40941,#40942);
#34144=AXIS2_PLACEMENT_3D('',#62730,#40943,#40944);
#34145=AXIS2_PLACEMENT_3D('',#62731,#40945,#40946);
#34146=AXIS2_PLACEMENT_3D('',#62733,#40947,#40948);
#34147=AXIS2_PLACEMENT_3D('',#62735,#40949,#40950);
#34148=AXIS2_PLACEMENT_3D('',#62736,#40951,#40952);
#34149=AXIS2_PLACEMENT_3D('',#62737,#40953,#40954);
#34150=AXIS2_PLACEMENT_3D('',#62739,#40955,#40956);
#34151=AXIS2_PLACEMENT_3D('',#62741,#40957,#40958);
#34152=AXIS2_PLACEMENT_3D('',#62742,#40959,#40960);
#34153=AXIS2_PLACEMENT_3D('',#62743,#40961,#40962);
#34154=AXIS2_PLACEMENT_3D('',#62745,#40963,#40964);
#34155=AXIS2_PLACEMENT_3D('',#62747,#40965,#40966);
#34156=AXIS2_PLACEMENT_3D('',#62748,#40967,#40968);
#34157=AXIS2_PLACEMENT_3D('',#62749,#40969,#40970);
#34158=AXIS2_PLACEMENT_3D('',#62751,#40971,#40972);
#34159=AXIS2_PLACEMENT_3D('',#62753,#40973,#40974);
#34160=AXIS2_PLACEMENT_3D('',#62754,#40975,#40976);
#34161=AXIS2_PLACEMENT_3D('',#62755,#40977,#40978);
#34162=AXIS2_PLACEMENT_3D('',#62757,#40979,#40980);
#34163=AXIS2_PLACEMENT_3D('',#62759,#40981,#40982);
#34164=AXIS2_PLACEMENT_3D('',#62760,#40983,#40984);
#34165=AXIS2_PLACEMENT_3D('',#62761,#40985,#40986);
#34166=AXIS2_PLACEMENT_3D('',#62763,#40987,#40988);
#34167=AXIS2_PLACEMENT_3D('',#62765,#40989,#40990);
#34168=AXIS2_PLACEMENT_3D('',#62766,#40991,#40992);
#34169=AXIS2_PLACEMENT_3D('',#62767,#40993,#40994);
#34170=AXIS2_PLACEMENT_3D('',#62769,#40995,#40996);
#34171=AXIS2_PLACEMENT_3D('',#62771,#40997,#40998);
#34172=AXIS2_PLACEMENT_3D('',#62772,#40999,#41000);
#34173=AXIS2_PLACEMENT_3D('',#62773,#41001,#41002);
#34174=AXIS2_PLACEMENT_3D('',#62775,#41003,#41004);
#34175=AXIS2_PLACEMENT_3D('',#62777,#41005,#41006);
#34176=AXIS2_PLACEMENT_3D('',#62778,#41007,#41008);
#34177=AXIS2_PLACEMENT_3D('',#62779,#41009,#41010);
#34178=AXIS2_PLACEMENT_3D('',#62781,#41011,#41012);
#34179=AXIS2_PLACEMENT_3D('',#62783,#41013,#41014);
#34180=AXIS2_PLACEMENT_3D('',#62784,#41015,#41016);
#34181=AXIS2_PLACEMENT_3D('',#62785,#41017,#41018);
#34182=AXIS2_PLACEMENT_3D('',#62787,#41019,#41020);
#34183=AXIS2_PLACEMENT_3D('',#62789,#41021,#41022);
#34184=AXIS2_PLACEMENT_3D('',#62790,#41023,#41024);
#34185=AXIS2_PLACEMENT_3D('',#62791,#41025,#41026);
#34186=AXIS2_PLACEMENT_3D('',#62793,#41027,#41028);
#34187=AXIS2_PLACEMENT_3D('',#62795,#41029,#41030);
#34188=AXIS2_PLACEMENT_3D('',#62796,#41031,#41032);
#34189=AXIS2_PLACEMENT_3D('',#62797,#41033,#41034);
#34190=AXIS2_PLACEMENT_3D('',#62799,#41035,#41036);
#34191=AXIS2_PLACEMENT_3D('',#62801,#41037,#41038);
#34192=AXIS2_PLACEMENT_3D('',#62802,#41039,#41040);
#34193=AXIS2_PLACEMENT_3D('',#62803,#41041,#41042);
#34194=AXIS2_PLACEMENT_3D('',#62805,#41043,#41044);
#34195=AXIS2_PLACEMENT_3D('',#62807,#41045,#41046);
#34196=AXIS2_PLACEMENT_3D('',#62808,#41047,#41048);
#34197=AXIS2_PLACEMENT_3D('',#62809,#41049,#41050);
#34198=AXIS2_PLACEMENT_3D('',#62811,#41051,#41052);
#34199=AXIS2_PLACEMENT_3D('',#62813,#41053,#41054);
#34200=AXIS2_PLACEMENT_3D('',#62814,#41055,#41056);
#34201=AXIS2_PLACEMENT_3D('',#62815,#41057,#41058);
#34202=AXIS2_PLACEMENT_3D('',#62817,#41059,#41060);
#34203=AXIS2_PLACEMENT_3D('',#62819,#41061,#41062);
#34204=AXIS2_PLACEMENT_3D('',#62820,#41063,#41064);
#34205=AXIS2_PLACEMENT_3D('',#62821,#41065,#41066);
#34206=AXIS2_PLACEMENT_3D('',#62823,#41067,#41068);
#34207=AXIS2_PLACEMENT_3D('',#62825,#41069,#41070);
#34208=AXIS2_PLACEMENT_3D('',#62826,#41071,#41072);
#34209=AXIS2_PLACEMENT_3D('',#62827,#41073,#41074);
#34210=AXIS2_PLACEMENT_3D('',#62829,#41075,#41076);
#34211=AXIS2_PLACEMENT_3D('',#62831,#41077,#41078);
#34212=AXIS2_PLACEMENT_3D('',#62832,#41079,#41080);
#34213=AXIS2_PLACEMENT_3D('',#62833,#41081,#41082);
#34214=AXIS2_PLACEMENT_3D('',#62835,#41083,#41084);
#34215=AXIS2_PLACEMENT_3D('',#62837,#41085,#41086);
#34216=AXIS2_PLACEMENT_3D('',#62838,#41087,#41088);
#34217=AXIS2_PLACEMENT_3D('',#62839,#41089,#41090);
#34218=AXIS2_PLACEMENT_3D('',#62841,#41091,#41092);
#34219=AXIS2_PLACEMENT_3D('',#62843,#41093,#41094);
#34220=AXIS2_PLACEMENT_3D('',#62844,#41095,#41096);
#34221=AXIS2_PLACEMENT_3D('',#62845,#41097,#41098);
#34222=AXIS2_PLACEMENT_3D('',#62847,#41099,#41100);
#34223=AXIS2_PLACEMENT_3D('',#62849,#41101,#41102);
#34224=AXIS2_PLACEMENT_3D('',#62850,#41103,#41104);
#34225=AXIS2_PLACEMENT_3D('',#62851,#41105,#41106);
#34226=AXIS2_PLACEMENT_3D('',#62853,#41107,#41108);
#34227=AXIS2_PLACEMENT_3D('',#62855,#41109,#41110);
#34228=AXIS2_PLACEMENT_3D('',#62856,#41111,#41112);
#34229=AXIS2_PLACEMENT_3D('',#62857,#41113,#41114);
#34230=AXIS2_PLACEMENT_3D('',#62859,#41115,#41116);
#34231=AXIS2_PLACEMENT_3D('',#62861,#41117,#41118);
#34232=AXIS2_PLACEMENT_3D('',#62862,#41119,#41120);
#34233=AXIS2_PLACEMENT_3D('',#62863,#41121,#41122);
#34234=AXIS2_PLACEMENT_3D('',#62865,#41123,#41124);
#34235=AXIS2_PLACEMENT_3D('',#62867,#41125,#41126);
#34236=AXIS2_PLACEMENT_3D('',#62868,#41127,#41128);
#34237=AXIS2_PLACEMENT_3D('',#62869,#41129,#41130);
#34238=AXIS2_PLACEMENT_3D('',#62871,#41131,#41132);
#34239=AXIS2_PLACEMENT_3D('',#62873,#41133,#41134);
#34240=AXIS2_PLACEMENT_3D('',#62874,#41135,#41136);
#34241=AXIS2_PLACEMENT_3D('',#62875,#41137,#41138);
#34242=AXIS2_PLACEMENT_3D('',#62877,#41139,#41140);
#34243=AXIS2_PLACEMENT_3D('',#62879,#41141,#41142);
#34244=AXIS2_PLACEMENT_3D('',#62880,#41143,#41144);
#34245=AXIS2_PLACEMENT_3D('',#62881,#41145,#41146);
#34246=AXIS2_PLACEMENT_3D('',#62883,#41147,#41148);
#34247=AXIS2_PLACEMENT_3D('',#62885,#41149,#41150);
#34248=AXIS2_PLACEMENT_3D('',#62886,#41151,#41152);
#34249=AXIS2_PLACEMENT_3D('',#62887,#41153,#41154);
#34250=AXIS2_PLACEMENT_3D('',#62889,#41155,#41156);
#34251=AXIS2_PLACEMENT_3D('',#62891,#41157,#41158);
#34252=AXIS2_PLACEMENT_3D('',#62892,#41159,#41160);
#34253=AXIS2_PLACEMENT_3D('',#62893,#41161,#41162);
#34254=AXIS2_PLACEMENT_3D('',#62895,#41163,#41164);
#34255=AXIS2_PLACEMENT_3D('',#62897,#41165,#41166);
#34256=AXIS2_PLACEMENT_3D('',#62898,#41167,#41168);
#34257=AXIS2_PLACEMENT_3D('',#62899,#41169,#41170);
#34258=AXIS2_PLACEMENT_3D('',#62901,#41171,#41172);
#34259=AXIS2_PLACEMENT_3D('',#62903,#41173,#41174);
#34260=AXIS2_PLACEMENT_3D('',#62904,#41175,#41176);
#34261=AXIS2_PLACEMENT_3D('',#62905,#41177,#41178);
#34262=AXIS2_PLACEMENT_3D('',#62907,#41179,#41180);
#34263=AXIS2_PLACEMENT_3D('',#62909,#41181,#41182);
#34264=AXIS2_PLACEMENT_3D('',#62910,#41183,#41184);
#34265=AXIS2_PLACEMENT_3D('',#62911,#41185,#41186);
#34266=AXIS2_PLACEMENT_3D('',#62913,#41187,#41188);
#34267=AXIS2_PLACEMENT_3D('',#62915,#41189,#41190);
#34268=AXIS2_PLACEMENT_3D('',#62916,#41191,#41192);
#34269=AXIS2_PLACEMENT_3D('',#62917,#41193,#41194);
#34270=AXIS2_PLACEMENT_3D('',#62919,#41195,#41196);
#34271=AXIS2_PLACEMENT_3D('',#62921,#41197,#41198);
#34272=AXIS2_PLACEMENT_3D('',#62922,#41199,#41200);
#34273=AXIS2_PLACEMENT_3D('',#62923,#41201,#41202);
#34274=AXIS2_PLACEMENT_3D('',#62925,#41203,#41204);
#34275=AXIS2_PLACEMENT_3D('',#62927,#41205,#41206);
#34276=AXIS2_PLACEMENT_3D('',#62928,#41207,#41208);
#34277=AXIS2_PLACEMENT_3D('',#62929,#41209,#41210);
#34278=AXIS2_PLACEMENT_3D('',#62931,#41211,#41212);
#34279=AXIS2_PLACEMENT_3D('',#62933,#41213,#41214);
#34280=AXIS2_PLACEMENT_3D('',#62934,#41215,#41216);
#34281=AXIS2_PLACEMENT_3D('',#62935,#41217,#41218);
#34282=AXIS2_PLACEMENT_3D('',#62937,#41219,#41220);
#34283=AXIS2_PLACEMENT_3D('',#62939,#41221,#41222);
#34284=AXIS2_PLACEMENT_3D('',#62940,#41223,#41224);
#34285=AXIS2_PLACEMENT_3D('',#62941,#41225,#41226);
#34286=AXIS2_PLACEMENT_3D('',#62943,#41227,#41228);
#34287=AXIS2_PLACEMENT_3D('',#62945,#41229,#41230);
#34288=AXIS2_PLACEMENT_3D('',#62946,#41231,#41232);
#34289=AXIS2_PLACEMENT_3D('',#62947,#41233,#41234);
#34290=AXIS2_PLACEMENT_3D('',#62949,#41235,#41236);
#34291=AXIS2_PLACEMENT_3D('',#62951,#41237,#41238);
#34292=AXIS2_PLACEMENT_3D('',#62952,#41239,#41240);
#34293=AXIS2_PLACEMENT_3D('',#62953,#41241,#41242);
#34294=AXIS2_PLACEMENT_3D('',#62955,#41243,#41244);
#34295=AXIS2_PLACEMENT_3D('',#62957,#41245,#41246);
#34296=AXIS2_PLACEMENT_3D('',#62958,#41247,#41248);
#34297=AXIS2_PLACEMENT_3D('',#62959,#41249,#41250);
#34298=AXIS2_PLACEMENT_3D('',#62961,#41251,#41252);
#34299=AXIS2_PLACEMENT_3D('',#62963,#41253,#41254);
#34300=AXIS2_PLACEMENT_3D('',#62964,#41255,#41256);
#34301=AXIS2_PLACEMENT_3D('',#62965,#41257,#41258);
#34302=AXIS2_PLACEMENT_3D('',#62967,#41259,#41260);
#34303=AXIS2_PLACEMENT_3D('',#62969,#41261,#41262);
#34304=AXIS2_PLACEMENT_3D('',#62970,#41263,#41264);
#34305=AXIS2_PLACEMENT_3D('',#62971,#41265,#41266);
#34306=AXIS2_PLACEMENT_3D('',#62973,#41267,#41268);
#34307=AXIS2_PLACEMENT_3D('',#62975,#41269,#41270);
#34308=AXIS2_PLACEMENT_3D('',#62976,#41271,#41272);
#34309=AXIS2_PLACEMENT_3D('',#62977,#41273,#41274);
#34310=AXIS2_PLACEMENT_3D('',#62979,#41275,#41276);
#34311=AXIS2_PLACEMENT_3D('',#62981,#41277,#41278);
#34312=AXIS2_PLACEMENT_3D('',#62982,#41279,#41280);
#34313=AXIS2_PLACEMENT_3D('',#62983,#41281,#41282);
#34314=AXIS2_PLACEMENT_3D('',#62985,#41283,#41284);
#34315=AXIS2_PLACEMENT_3D('',#62987,#41285,#41286);
#34316=AXIS2_PLACEMENT_3D('',#62988,#41287,#41288);
#34317=AXIS2_PLACEMENT_3D('',#62989,#41289,#41290);
#34318=AXIS2_PLACEMENT_3D('',#62993,#41292,#41293);
#34319=AXIS2_PLACEMENT_3D('',#62995,#41295,#41296);
#34320=AXIS2_PLACEMENT_3D('',#63000,#41299,#41300);
#34321=AXIS2_PLACEMENT_3D('',#63001,#41301,#41302);
#34322=AXIS2_PLACEMENT_3D('',#63006,#41305,#41306);
#34323=AXIS2_PLACEMENT_3D('',#63007,#41307,#41308);
#34324=AXIS2_PLACEMENT_3D('',#63012,#41311,#41312);
#34325=AXIS2_PLACEMENT_3D('',#63013,#41313,#41314);
#34326=AXIS2_PLACEMENT_3D('',#63018,#41317,#41318);
#34327=AXIS2_PLACEMENT_3D('',#63019,#41319,#41320);
#34328=AXIS2_PLACEMENT_3D('',#63024,#41323,#41324);
#34329=AXIS2_PLACEMENT_3D('',#63025,#41325,#41326);
#34330=AXIS2_PLACEMENT_3D('',#63030,#41329,#41330);
#34331=AXIS2_PLACEMENT_3D('',#63031,#41331,#41332);
#34332=AXIS2_PLACEMENT_3D('',#63036,#41335,#41336);
#34333=AXIS2_PLACEMENT_3D('',#63037,#41337,#41338);
#34334=AXIS2_PLACEMENT_3D('',#63042,#41341,#41342);
#34335=AXIS2_PLACEMENT_3D('',#63043,#41343,#41344);
#34336=AXIS2_PLACEMENT_3D('',#63048,#41347,#41348);
#34337=AXIS2_PLACEMENT_3D('',#63049,#41349,#41350);
#34338=AXIS2_PLACEMENT_3D('',#63054,#41353,#41354);
#34339=AXIS2_PLACEMENT_3D('',#63055,#41355,#41356);
#34340=AXIS2_PLACEMENT_3D('',#63060,#41359,#41360);
#34341=AXIS2_PLACEMENT_3D('',#63061,#41361,#41362);
#34342=AXIS2_PLACEMENT_3D('',#63066,#41365,#41366);
#34343=AXIS2_PLACEMENT_3D('',#63067,#41367,#41368);
#34344=AXIS2_PLACEMENT_3D('',#63072,#41371,#41372);
#34345=AXIS2_PLACEMENT_3D('',#63073,#41373,#41374);
#34346=AXIS2_PLACEMENT_3D('',#63078,#41377,#41378);
#34347=AXIS2_PLACEMENT_3D('',#63079,#41379,#41380);
#34348=AXIS2_PLACEMENT_3D('',#63084,#41383,#41384);
#34349=AXIS2_PLACEMENT_3D('',#63085,#41385,#41386);
#34350=AXIS2_PLACEMENT_3D('',#63090,#41389,#41390);
#34351=AXIS2_PLACEMENT_3D('',#63091,#41391,#41392);
#34352=AXIS2_PLACEMENT_3D('',#63096,#41395,#41396);
#34353=AXIS2_PLACEMENT_3D('',#63097,#41397,#41398);
#34354=AXIS2_PLACEMENT_3D('',#63102,#41401,#41402);
#34355=AXIS2_PLACEMENT_3D('',#63103,#41403,#41404);
#34356=AXIS2_PLACEMENT_3D('',#63108,#41407,#41408);
#34357=AXIS2_PLACEMENT_3D('',#63109,#41409,#41410);
#34358=AXIS2_PLACEMENT_3D('',#63114,#41413,#41414);
#34359=AXIS2_PLACEMENT_3D('',#63115,#41415,#41416);
#34360=AXIS2_PLACEMENT_3D('',#63120,#41419,#41420);
#34361=AXIS2_PLACEMENT_3D('',#63121,#41421,#41422);
#34362=AXIS2_PLACEMENT_3D('',#63126,#41425,#41426);
#34363=AXIS2_PLACEMENT_3D('',#63127,#41427,#41428);
#34364=AXIS2_PLACEMENT_3D('',#63132,#41431,#41432);
#34365=AXIS2_PLACEMENT_3D('',#63133,#41433,#41434);
#34366=AXIS2_PLACEMENT_3D('',#63138,#41437,#41438);
#34367=AXIS2_PLACEMENT_3D('',#63139,#41439,#41440);
#34368=AXIS2_PLACEMENT_3D('',#63144,#41443,#41444);
#34369=AXIS2_PLACEMENT_3D('',#63145,#41445,#41446);
#34370=AXIS2_PLACEMENT_3D('',#63150,#41449,#41450);
#34371=AXIS2_PLACEMENT_3D('',#63151,#41451,#41452);
#34372=AXIS2_PLACEMENT_3D('',#63156,#41455,#41456);
#34373=AXIS2_PLACEMENT_3D('',#63157,#41457,#41458);
#34374=AXIS2_PLACEMENT_3D('',#63162,#41461,#41462);
#34375=AXIS2_PLACEMENT_3D('',#63163,#41463,#41464);
#34376=AXIS2_PLACEMENT_3D('',#63168,#41467,#41468);
#34377=AXIS2_PLACEMENT_3D('',#63169,#41469,#41470);
#34378=AXIS2_PLACEMENT_3D('',#63174,#41473,#41474);
#34379=AXIS2_PLACEMENT_3D('',#63175,#41475,#41476);
#34380=AXIS2_PLACEMENT_3D('',#63180,#41479,#41480);
#34381=AXIS2_PLACEMENT_3D('',#63181,#41481,#41482);
#34382=AXIS2_PLACEMENT_3D('',#63186,#41485,#41486);
#34383=AXIS2_PLACEMENT_3D('',#63187,#41487,#41488);
#34384=AXIS2_PLACEMENT_3D('',#63192,#41491,#41492);
#34385=AXIS2_PLACEMENT_3D('',#63193,#41493,#41494);
#34386=AXIS2_PLACEMENT_3D('',#63198,#41497,#41498);
#34387=AXIS2_PLACEMENT_3D('',#63199,#41499,#41500);
#34388=AXIS2_PLACEMENT_3D('',#63204,#41503,#41504);
#34389=AXIS2_PLACEMENT_3D('',#63205,#41505,#41506);
#34390=AXIS2_PLACEMENT_3D('',#63210,#41509,#41510);
#34391=AXIS2_PLACEMENT_3D('',#63211,#41511,#41512);
#34392=AXIS2_PLACEMENT_3D('',#63216,#41515,#41516);
#34393=AXIS2_PLACEMENT_3D('',#63217,#41517,#41518);
#34394=AXIS2_PLACEMENT_3D('',#63222,#41521,#41522);
#34395=AXIS2_PLACEMENT_3D('',#63223,#41523,#41524);
#34396=AXIS2_PLACEMENT_3D('',#63228,#41527,#41528);
#34397=AXIS2_PLACEMENT_3D('',#63229,#41529,#41530);
#34398=AXIS2_PLACEMENT_3D('',#63234,#41533,#41534);
#34399=AXIS2_PLACEMENT_3D('',#63235,#41535,#41536);
#34400=AXIS2_PLACEMENT_3D('',#63240,#41539,#41540);
#34401=AXIS2_PLACEMENT_3D('',#63241,#41541,#41542);
#34402=AXIS2_PLACEMENT_3D('',#63246,#41545,#41546);
#34403=AXIS2_PLACEMENT_3D('',#63247,#41547,#41548);
#34404=AXIS2_PLACEMENT_3D('',#63252,#41551,#41552);
#34405=AXIS2_PLACEMENT_3D('',#63253,#41553,#41554);
#34406=AXIS2_PLACEMENT_3D('',#63258,#41557,#41558);
#34407=AXIS2_PLACEMENT_3D('',#63259,#41559,#41560);
#34408=AXIS2_PLACEMENT_3D('',#63264,#41563,#41564);
#34409=AXIS2_PLACEMENT_3D('',#63265,#41565,#41566);
#34410=AXIS2_PLACEMENT_3D('',#63270,#41569,#41570);
#34411=AXIS2_PLACEMENT_3D('',#63271,#41571,#41572);
#34412=AXIS2_PLACEMENT_3D('',#63276,#41575,#41576);
#34413=AXIS2_PLACEMENT_3D('',#63277,#41577,#41578);
#34414=AXIS2_PLACEMENT_3D('',#63282,#41581,#41582);
#34415=AXIS2_PLACEMENT_3D('',#63283,#41583,#41584);
#34416=AXIS2_PLACEMENT_3D('',#63288,#41587,#41588);
#34417=AXIS2_PLACEMENT_3D('',#63289,#41589,#41590);
#34418=AXIS2_PLACEMENT_3D('',#63294,#41593,#41594);
#34419=AXIS2_PLACEMENT_3D('',#63295,#41595,#41596);
#34420=AXIS2_PLACEMENT_3D('',#63300,#41599,#41600);
#34421=AXIS2_PLACEMENT_3D('',#63301,#41601,#41602);
#34422=AXIS2_PLACEMENT_3D('',#63306,#41605,#41606);
#34423=AXIS2_PLACEMENT_3D('',#63307,#41607,#41608);
#34424=AXIS2_PLACEMENT_3D('',#63312,#41611,#41612);
#34425=AXIS2_PLACEMENT_3D('',#63313,#41613,#41614);
#34426=AXIS2_PLACEMENT_3D('',#63318,#41617,#41618);
#34427=AXIS2_PLACEMENT_3D('',#63319,#41619,#41620);
#34428=AXIS2_PLACEMENT_3D('',#63324,#41623,#41624);
#34429=AXIS2_PLACEMENT_3D('',#63325,#41625,#41626);
#34430=AXIS2_PLACEMENT_3D('',#63330,#41629,#41630);
#34431=AXIS2_PLACEMENT_3D('',#63331,#41631,#41632);
#34432=AXIS2_PLACEMENT_3D('',#63336,#41635,#41636);
#34433=AXIS2_PLACEMENT_3D('',#63337,#41637,#41638);
#34434=AXIS2_PLACEMENT_3D('',#63342,#41641,#41642);
#34435=AXIS2_PLACEMENT_3D('',#63343,#41643,#41644);
#34436=AXIS2_PLACEMENT_3D('',#63348,#41647,#41648);
#34437=AXIS2_PLACEMENT_3D('',#63349,#41649,#41650);
#34438=AXIS2_PLACEMENT_3D('',#63354,#41653,#41654);
#34439=AXIS2_PLACEMENT_3D('',#63355,#41655,#41656);
#34440=AXIS2_PLACEMENT_3D('',#63360,#41659,#41660);
#34441=AXIS2_PLACEMENT_3D('',#63361,#41661,#41662);
#34442=AXIS2_PLACEMENT_3D('',#63366,#41665,#41666);
#34443=AXIS2_PLACEMENT_3D('',#63367,#41667,#41668);
#34444=AXIS2_PLACEMENT_3D('',#63372,#41671,#41672);
#34445=AXIS2_PLACEMENT_3D('',#63373,#41673,#41674);
#34446=AXIS2_PLACEMENT_3D('',#63377,#41676,#41677);
#34447=AXIS2_PLACEMENT_3D('',#63379,#41679,#41680);
#34448=AXIS2_PLACEMENT_3D('',#63383,#41682,#41683);
#34449=AXIS2_PLACEMENT_3D('',#63385,#41685,#41686);
#34450=AXIS2_PLACEMENT_3D('',#63389,#41688,#41689);
#34451=AXIS2_PLACEMENT_3D('',#63391,#41691,#41692);
#34452=AXIS2_PLACEMENT_3D('',#63395,#41694,#41695);
#34453=AXIS2_PLACEMENT_3D('',#63397,#41697,#41698);
#34454=AXIS2_PLACEMENT_3D('',#63401,#41700,#41701);
#34455=AXIS2_PLACEMENT_3D('',#63403,#41703,#41704);
#34456=AXIS2_PLACEMENT_3D('',#63407,#41706,#41707);
#34457=AXIS2_PLACEMENT_3D('',#63409,#41709,#41710);
#34458=AXIS2_PLACEMENT_3D('',#63413,#41712,#41713);
#34459=AXIS2_PLACEMENT_3D('',#63415,#41715,#41716);
#34460=AXIS2_PLACEMENT_3D('',#63419,#41718,#41719);
#34461=AXIS2_PLACEMENT_3D('',#63421,#41721,#41722);
#34462=AXIS2_PLACEMENT_3D('',#63425,#41724,#41725);
#34463=AXIS2_PLACEMENT_3D('',#63427,#41727,#41728);
#34464=AXIS2_PLACEMENT_3D('',#63431,#41730,#41731);
#34465=AXIS2_PLACEMENT_3D('',#63433,#41733,#41734);
#34466=AXIS2_PLACEMENT_3D('',#63437,#41736,#41737);
#34467=AXIS2_PLACEMENT_3D('',#63439,#41739,#41740);
#34468=AXIS2_PLACEMENT_3D('',#63443,#41742,#41743);
#34469=AXIS2_PLACEMENT_3D('',#63445,#41745,#41746);
#34470=AXIS2_PLACEMENT_3D('',#63449,#41748,#41749);
#34471=AXIS2_PLACEMENT_3D('',#63451,#41751,#41752);
#34472=AXIS2_PLACEMENT_3D('',#63455,#41754,#41755);
#34473=AXIS2_PLACEMENT_3D('',#63457,#41757,#41758);
#34474=AXIS2_PLACEMENT_3D('',#63462,#41761,#41762);
#34475=AXIS2_PLACEMENT_3D('',#63463,#41763,#41764);
#34476=AXIS2_PLACEMENT_3D('',#63464,#41765,#41766);
#34477=AXIS2_PLACEMENT_3D('',#63465,#41767,#41768);
#34478=AXIS2_PLACEMENT_3D('',#63466,#41769,#41770);
#34479=AXIS2_PLACEMENT_3D('',#63467,#41771,#41772);
#34480=AXIS2_PLACEMENT_3D('',#63468,#41773,#41774);
#34481=AXIS2_PLACEMENT_3D('',#63469,#41775,#41776);
#34482=AXIS2_PLACEMENT_3D('',#63470,#41777,#41778);
#34483=AXIS2_PLACEMENT_3D('',#63471,#41779,#41780);
#34484=AXIS2_PLACEMENT_3D('',#63472,#41781,#41782);
#34485=AXIS2_PLACEMENT_3D('',#63473,#41783,#41784);
#34486=AXIS2_PLACEMENT_3D('',#63474,#41785,#41786);
#34487=AXIS2_PLACEMENT_3D('',#63475,#41787,#41788);
#34488=AXIS2_PLACEMENT_3D('',#63476,#41789,#41790);
#34489=AXIS2_PLACEMENT_3D('',#63477,#41791,#41792);
#34490=AXIS2_PLACEMENT_3D('',#63478,#41793,#41794);
#34491=AXIS2_PLACEMENT_3D('',#63479,#41795,#41796);
#34492=AXIS2_PLACEMENT_3D('',#63480,#41797,#41798);
#34493=AXIS2_PLACEMENT_3D('',#63481,#41799,#41800);
#34494=AXIS2_PLACEMENT_3D('',#63482,#41801,#41802);
#34495=AXIS2_PLACEMENT_3D('',#63483,#41803,#41804);
#34496=AXIS2_PLACEMENT_3D('',#63484,#41805,#41806);
#34497=AXIS2_PLACEMENT_3D('',#63485,#41807,#41808);
#34498=AXIS2_PLACEMENT_3D('',#63486,#41809,#41810);
#34499=AXIS2_PLACEMENT_3D('',#63487,#41811,#41812);
#34500=AXIS2_PLACEMENT_3D('',#63488,#41813,#41814);
#34501=AXIS2_PLACEMENT_3D('',#63489,#41815,#41816);
#34502=AXIS2_PLACEMENT_3D('',#63490,#41817,#41818);
#34503=AXIS2_PLACEMENT_3D('',#63491,#41819,#41820);
#34504=AXIS2_PLACEMENT_3D('',#63492,#41821,#41822);
#34505=AXIS2_PLACEMENT_3D('',#63493,#41823,#41824);
#34506=AXIS2_PLACEMENT_3D('',#63494,#41825,#41826);
#34507=AXIS2_PLACEMENT_3D('',#63495,#41827,#41828);
#34508=AXIS2_PLACEMENT_3D('',#63496,#41829,#41830);
#34509=AXIS2_PLACEMENT_3D('',#63497,#41831,#41832);
#34510=AXIS2_PLACEMENT_3D('',#63498,#41833,#41834);
#34511=AXIS2_PLACEMENT_3D('',#63499,#41835,#41836);
#34512=AXIS2_PLACEMENT_3D('',#63500,#41837,#41838);
#34513=AXIS2_PLACEMENT_3D('',#63501,#41839,#41840);
#34514=AXIS2_PLACEMENT_3D('',#63502,#41841,#41842);
#34515=AXIS2_PLACEMENT_3D('',#63503,#41843,#41844);
#34516=AXIS2_PLACEMENT_3D('',#63504,#41845,#41846);
#34517=AXIS2_PLACEMENT_3D('',#63505,#41847,#41848);
#34518=AXIS2_PLACEMENT_3D('',#63506,#41849,#41850);
#34519=AXIS2_PLACEMENT_3D('',#63507,#41851,#41852);
#34520=AXIS2_PLACEMENT_3D('',#63508,#41853,#41854);
#34521=AXIS2_PLACEMENT_3D('',#63509,#41855,#41856);
#34522=AXIS2_PLACEMENT_3D('',#63510,#41857,#41858);
#34523=AXIS2_PLACEMENT_3D('',#63511,#41859,#41860);
#34524=AXIS2_PLACEMENT_3D('',#63512,#41861,#41862);
#34525=AXIS2_PLACEMENT_3D('',#63513,#41863,#41864);
#34526=AXIS2_PLACEMENT_3D('',#63514,#41865,#41866);
#34527=AXIS2_PLACEMENT_3D('',#63515,#41867,#41868);
#34528=AXIS2_PLACEMENT_3D('',#63516,#41869,#41870);
#34529=AXIS2_PLACEMENT_3D('',#63517,#41871,#41872);
#34530=AXIS2_PLACEMENT_3D('',#63518,#41873,#41874);
#34531=AXIS2_PLACEMENT_3D('',#63519,#41875,#41876);
#34532=AXIS2_PLACEMENT_3D('',#63520,#41877,#41878);
#34533=AXIS2_PLACEMENT_3D('',#63521,#41879,#41880);
#34534=AXIS2_PLACEMENT_3D('',#63522,#41881,#41882);
#34535=AXIS2_PLACEMENT_3D('',#63523,#41883,#41884);
#34536=AXIS2_PLACEMENT_3D('',#63524,#41885,#41886);
#34537=AXIS2_PLACEMENT_3D('',#63525,#41887,#41888);
#34538=AXIS2_PLACEMENT_3D('',#63526,#41889,#41890);
#34539=AXIS2_PLACEMENT_3D('',#63527,#41891,#41892);
#34540=AXIS2_PLACEMENT_3D('',#63528,#41893,#41894);
#34541=AXIS2_PLACEMENT_3D('',#63529,#41895,#41896);
#34542=AXIS2_PLACEMENT_3D('',#63530,#41897,#41898);
#34543=AXIS2_PLACEMENT_3D('',#63531,#41899,#41900);
#34544=AXIS2_PLACEMENT_3D('',#63532,#41901,#41902);
#34545=AXIS2_PLACEMENT_3D('',#63533,#41903,#41904);
#34546=AXIS2_PLACEMENT_3D('',#63534,#41905,#41906);
#34547=AXIS2_PLACEMENT_3D('',#63535,#41907,#41908);
#34548=AXIS2_PLACEMENT_3D('',#63536,#41909,#41910);
#34549=AXIS2_PLACEMENT_3D('',#63537,#41911,#41912);
#34550=AXIS2_PLACEMENT_3D('',#63538,#41913,#41914);
#34551=AXIS2_PLACEMENT_3D('',#63539,#41915,#41916);
#34552=AXIS2_PLACEMENT_3D('',#63540,#41917,#41918);
#34553=AXIS2_PLACEMENT_3D('',#63541,#41919,#41920);
#34554=AXIS2_PLACEMENT_3D('',#63542,#41921,#41922);
#34555=AXIS2_PLACEMENT_3D('',#63543,#41923,#41924);
#34556=AXIS2_PLACEMENT_3D('',#63544,#41925,#41926);
#34557=AXIS2_PLACEMENT_3D('',#63545,#41927,#41928);
#34558=AXIS2_PLACEMENT_3D('',#63546,#41929,#41930);
#34559=AXIS2_PLACEMENT_3D('',#63547,#41931,#41932);
#34560=AXIS2_PLACEMENT_3D('',#63548,#41933,#41934);
#34561=AXIS2_PLACEMENT_3D('',#63549,#41935,#41936);
#34562=AXIS2_PLACEMENT_3D('',#63550,#41937,#41938);
#34563=AXIS2_PLACEMENT_3D('',#63551,#41939,#41940);
#34564=AXIS2_PLACEMENT_3D('',#63552,#41941,#41942);
#34565=AXIS2_PLACEMENT_3D('',#63553,#41943,#41944);
#34566=AXIS2_PLACEMENT_3D('',#63554,#41945,#41946);
#34567=AXIS2_PLACEMENT_3D('',#63555,#41947,#41948);
#34568=AXIS2_PLACEMENT_3D('',#63556,#41949,#41950);
#34569=AXIS2_PLACEMENT_3D('',#63557,#41951,#41952);
#34570=AXIS2_PLACEMENT_3D('',#63558,#41953,#41954);
#34571=AXIS2_PLACEMENT_3D('',#63559,#41955,#41956);
#34572=AXIS2_PLACEMENT_3D('',#63560,#41957,#41958);
#34573=AXIS2_PLACEMENT_3D('',#63561,#41959,#41960);
#34574=AXIS2_PLACEMENT_3D('',#63562,#41961,#41962);
#34575=AXIS2_PLACEMENT_3D('',#63563,#41963,#41964);
#34576=AXIS2_PLACEMENT_3D('',#63564,#41965,#41966);
#34577=AXIS2_PLACEMENT_3D('',#63565,#41967,#41968);
#34578=AXIS2_PLACEMENT_3D('',#63566,#41969,#41970);
#34579=AXIS2_PLACEMENT_3D('',#63567,#41971,#41972);
#34580=AXIS2_PLACEMENT_3D('',#63568,#41973,#41974);
#34581=AXIS2_PLACEMENT_3D('',#63569,#41975,#41976);
#34582=AXIS2_PLACEMENT_3D('',#63570,#41977,#41978);
#34583=AXIS2_PLACEMENT_3D('',#63571,#41979,#41980);
#34584=AXIS2_PLACEMENT_3D('',#63572,#41981,#41982);
#34585=AXIS2_PLACEMENT_3D('',#63573,#41983,#41984);
#34586=AXIS2_PLACEMENT_3D('',#63574,#41985,#41986);
#34587=AXIS2_PLACEMENT_3D('',#63575,#41987,#41988);
#34588=AXIS2_PLACEMENT_3D('',#63576,#41989,#41990);
#34589=AXIS2_PLACEMENT_3D('',#63577,#41991,#41992);
#34590=AXIS2_PLACEMENT_3D('',#63578,#41993,#41994);
#34591=AXIS2_PLACEMENT_3D('',#63579,#41995,#41996);
#34592=AXIS2_PLACEMENT_3D('',#63580,#41997,#41998);
#34593=AXIS2_PLACEMENT_3D('',#63581,#41999,#42000);
#34594=AXIS2_PLACEMENT_3D('',#63582,#42001,#42002);
#34595=AXIS2_PLACEMENT_3D('',#63583,#42003,#42004);
#34596=AXIS2_PLACEMENT_3D('',#63584,#42005,#42006);
#34597=AXIS2_PLACEMENT_3D('',#63585,#42007,#42008);
#34598=AXIS2_PLACEMENT_3D('',#63586,#42009,#42010);
#34599=AXIS2_PLACEMENT_3D('',#63587,#42011,#42012);
#34600=AXIS2_PLACEMENT_3D('',#63588,#42013,#42014);
#34601=AXIS2_PLACEMENT_3D('',#63589,#42015,#42016);
#34602=AXIS2_PLACEMENT_3D('',#63590,#42017,#42018);
#34603=AXIS2_PLACEMENT_3D('',#63591,#42019,#42020);
#34604=AXIS2_PLACEMENT_3D('',#63592,#42021,#42022);
#34605=AXIS2_PLACEMENT_3D('',#63593,#42023,#42024);
#34606=AXIS2_PLACEMENT_3D('',#63594,#42025,#42026);
#34607=AXIS2_PLACEMENT_3D('',#63595,#42027,#42028);
#34608=AXIS2_PLACEMENT_3D('',#63596,#42029,#42030);
#34609=AXIS2_PLACEMENT_3D('',#63597,#42031,#42032);
#34610=AXIS2_PLACEMENT_3D('',#63598,#42033,#42034);
#34611=AXIS2_PLACEMENT_3D('',#63599,#42035,#42036);
#34612=AXIS2_PLACEMENT_3D('',#63600,#42037,#42038);
#34613=AXIS2_PLACEMENT_3D('',#63601,#42039,#42040);
#34614=AXIS2_PLACEMENT_3D('',#63602,#42041,#42042);
#34615=AXIS2_PLACEMENT_3D('',#63603,#42043,#42044);
#34616=AXIS2_PLACEMENT_3D('',#63604,#42045,#42046);
#34617=AXIS2_PLACEMENT_3D('',#63605,#42047,#42048);
#34618=AXIS2_PLACEMENT_3D('',#63606,#42049,#42050);
#34619=AXIS2_PLACEMENT_3D('',#63607,#42051,#42052);
#34620=AXIS2_PLACEMENT_3D('',#63608,#42053,#42054);
#34621=AXIS2_PLACEMENT_3D('',#63609,#42055,#42056);
#34622=AXIS2_PLACEMENT_3D('',#63610,#42057,#42058);
#34623=AXIS2_PLACEMENT_3D('',#63611,#42059,#42060);
#34624=AXIS2_PLACEMENT_3D('',#63612,#42061,#42062);
#34625=AXIS2_PLACEMENT_3D('',#63613,#42063,#42064);
#34626=AXIS2_PLACEMENT_3D('',#63614,#42065,#42066);
#34627=AXIS2_PLACEMENT_3D('',#63615,#42067,#42068);
#34628=AXIS2_PLACEMENT_3D('',#63616,#42069,#42070);
#34629=AXIS2_PLACEMENT_3D('',#63617,#42071,#42072);
#34630=AXIS2_PLACEMENT_3D('',#63618,#42073,#42074);
#34631=AXIS2_PLACEMENT_3D('',#63619,#42075,#42076);
#34632=AXIS2_PLACEMENT_3D('',#63620,#42077,#42078);
#34633=AXIS2_PLACEMENT_3D('',#63621,#42079,#42080);
#34634=AXIS2_PLACEMENT_3D('',#63622,#42081,#42082);
#34635=AXIS2_PLACEMENT_3D('',#63623,#42083,#42084);
#34636=AXIS2_PLACEMENT_3D('',#63624,#42085,#42086);
#34637=AXIS2_PLACEMENT_3D('',#63625,#42087,#42088);
#34638=AXIS2_PLACEMENT_3D('',#63626,#42089,#42090);
#34639=AXIS2_PLACEMENT_3D('',#63627,#42091,#42092);
#34640=AXIS2_PLACEMENT_3D('',#63628,#42093,#42094);
#34641=AXIS2_PLACEMENT_3D('',#63629,#42095,#42096);
#34642=AXIS2_PLACEMENT_3D('',#63630,#42097,#42098);
#34643=AXIS2_PLACEMENT_3D('',#63631,#42099,#42100);
#34644=AXIS2_PLACEMENT_3D('',#63632,#42101,#42102);
#34645=AXIS2_PLACEMENT_3D('',#63633,#42103,#42104);
#34646=AXIS2_PLACEMENT_3D('',#63634,#42105,#42106);
#34647=AXIS2_PLACEMENT_3D('',#63635,#42107,#42108);
#34648=AXIS2_PLACEMENT_3D('',#63636,#42109,#42110);
#34649=AXIS2_PLACEMENT_3D('',#63637,#42111,#42112);
#34650=AXIS2_PLACEMENT_3D('',#63638,#42113,#42114);
#34651=AXIS2_PLACEMENT_3D('',#63639,#42115,#42116);
#34652=AXIS2_PLACEMENT_3D('',#63640,#42117,#42118);
#34653=AXIS2_PLACEMENT_3D('',#63641,#42119,#42120);
#34654=AXIS2_PLACEMENT_3D('',#63642,#42121,#42122);
#34655=AXIS2_PLACEMENT_3D('',#63643,#42123,#42124);
#34656=AXIS2_PLACEMENT_3D('',#63644,#42125,#42126);
#34657=AXIS2_PLACEMENT_3D('',#63645,#42127,#42128);
#34658=AXIS2_PLACEMENT_3D('',#63646,#42129,#42130);
#34659=AXIS2_PLACEMENT_3D('',#63647,#42131,#42132);
#34660=AXIS2_PLACEMENT_3D('',#63648,#42133,#42134);
#34661=AXIS2_PLACEMENT_3D('',#63649,#42135,#42136);
#34662=AXIS2_PLACEMENT_3D('',#63650,#42137,#42138);
#34663=AXIS2_PLACEMENT_3D('',#63651,#42139,#42140);
#34664=AXIS2_PLACEMENT_3D('',#63652,#42141,#42142);
#34665=AXIS2_PLACEMENT_3D('',#63653,#42143,#42144);
#34666=AXIS2_PLACEMENT_3D('',#63654,#42145,#42146);
#34667=AXIS2_PLACEMENT_3D('',#63655,#42147,#42148);
#34668=AXIS2_PLACEMENT_3D('',#63656,#42149,#42150);
#34669=AXIS2_PLACEMENT_3D('',#63657,#42151,#42152);
#34670=AXIS2_PLACEMENT_3D('',#63658,#42153,#42154);
#34671=AXIS2_PLACEMENT_3D('',#63659,#42155,#42156);
#34672=AXIS2_PLACEMENT_3D('',#63660,#42157,#42158);
#34673=AXIS2_PLACEMENT_3D('',#63661,#42159,#42160);
#34674=AXIS2_PLACEMENT_3D('',#63662,#42161,#42162);
#34675=AXIS2_PLACEMENT_3D('',#63663,#42163,#42164);
#34676=AXIS2_PLACEMENT_3D('',#63664,#42165,#42166);
#34677=AXIS2_PLACEMENT_3D('',#63665,#42167,#42168);
#34678=AXIS2_PLACEMENT_3D('',#63666,#42169,#42170);
#34679=AXIS2_PLACEMENT_3D('',#63667,#42171,#42172);
#34680=AXIS2_PLACEMENT_3D('',#63668,#42173,#42174);
#34681=AXIS2_PLACEMENT_3D('',#63669,#42175,#42176);
#34682=AXIS2_PLACEMENT_3D('',#63670,#42177,#42178);
#34683=AXIS2_PLACEMENT_3D('',#63671,#42179,#42180);
#34684=AXIS2_PLACEMENT_3D('',#63672,#42181,#42182);
#34685=AXIS2_PLACEMENT_3D('',#63673,#42183,#42184);
#34686=AXIS2_PLACEMENT_3D('',#63674,#42185,#42186);
#34687=AXIS2_PLACEMENT_3D('',#63675,#42187,#42188);
#34688=AXIS2_PLACEMENT_3D('',#63676,#42189,#42190);
#34689=AXIS2_PLACEMENT_3D('',#63677,#42191,#42192);
#34690=AXIS2_PLACEMENT_3D('',#63678,#42193,#42194);
#34691=AXIS2_PLACEMENT_3D('',#63679,#42195,#42196);
#34692=AXIS2_PLACEMENT_3D('',#63680,#42197,#42198);
#34693=AXIS2_PLACEMENT_3D('',#63681,#42199,#42200);
#34694=AXIS2_PLACEMENT_3D('',#63682,#42201,#42202);
#34695=AXIS2_PLACEMENT_3D('',#63683,#42203,#42204);
#34696=AXIS2_PLACEMENT_3D('',#63684,#42205,#42206);
#34697=AXIS2_PLACEMENT_3D('',#63685,#42207,#42208);
#34698=AXIS2_PLACEMENT_3D('',#63686,#42209,#42210);
#34699=AXIS2_PLACEMENT_3D('',#63687,#42211,#42212);
#34700=AXIS2_PLACEMENT_3D('',#63688,#42213,#42214);
#34701=AXIS2_PLACEMENT_3D('',#63689,#42215,#42216);
#34702=AXIS2_PLACEMENT_3D('',#63690,#42217,#42218);
#34703=AXIS2_PLACEMENT_3D('',#63691,#42219,#42220);
#34704=AXIS2_PLACEMENT_3D('',#63692,#42221,#42222);
#34705=AXIS2_PLACEMENT_3D('',#63693,#42223,#42224);
#34706=AXIS2_PLACEMENT_3D('',#63694,#42225,#42226);
#34707=AXIS2_PLACEMENT_3D('',#63695,#42227,#42228);
#34708=AXIS2_PLACEMENT_3D('',#63696,#42229,#42230);
#34709=AXIS2_PLACEMENT_3D('',#63697,#42231,#42232);
#34710=AXIS2_PLACEMENT_3D('',#63698,#42233,#42234);
#34711=AXIS2_PLACEMENT_3D('',#63699,#42235,#42236);
#34712=AXIS2_PLACEMENT_3D('',#63700,#42237,#42238);
#34713=AXIS2_PLACEMENT_3D('',#63701,#42239,#42240);
#34714=AXIS2_PLACEMENT_3D('',#63702,#42241,#42242);
#34715=AXIS2_PLACEMENT_3D('',#63704,#42243,#42244);
#34716=AXIS2_PLACEMENT_3D('',#63706,#42245,#42246);
#34717=AXIS2_PLACEMENT_3D('',#63707,#42247,#42248);
#34718=AXIS2_PLACEMENT_3D('',#63708,#42249,#42250);
#34719=AXIS2_PLACEMENT_3D('',#63713,#42253,#42254);
#34720=AXIS2_PLACEMENT_3D('',#63714,#42255,#42256);
#34721=AXIS2_PLACEMENT_3D('',#63715,#42257,#42258);
#34722=AXIS2_PLACEMENT_3D('',#63716,#42259,#42260);
#34723=AXIS2_PLACEMENT_3D('',#63717,#42261,#42262);
#34724=AXIS2_PLACEMENT_3D('',#63718,#42263,#42264);
#34725=AXIS2_PLACEMENT_3D('',#63731,#42271,#42272);
#34726=AXIS2_PLACEMENT_3D('',#63734,#42275,#42276);
#34727=AXIS2_PLACEMENT_3D('',#63736,#42278,#42279);
#34728=AXIS2_PLACEMENT_3D('',#63738,#42281,#42282);
#34729=AXIS2_PLACEMENT_3D('',#63740,#42284,#42285);
#34730=AXIS2_PLACEMENT_3D('',#63742,#42287,#42288);
#34731=AXIS2_PLACEMENT_3D('',#65264,#42290,#42291);
#34732=AXIS2_PLACEMENT_3D('',#65265,#42292,#42293);
#34733=AXIS2_PLACEMENT_3D('',#65267,#42295,#42296);
#34734=AXIS2_PLACEMENT_3D('',#65269,#42298,#42299);
#34735=AXIS2_PLACEMENT_3D('',#65270,#42300,#42301);
#34736=AXIS2_PLACEMENT_3D('',#65272,#42303,#42304);
#34737=AXIS2_PLACEMENT_3D('',#65274,#42306,#42307);
#34738=AXIS2_PLACEMENT_3D('',#65275,#42308,#42309);
#34739=AXIS2_PLACEMENT_3D('',#65277,#42311,#42312);
#34740=AXIS2_PLACEMENT_3D('',#65279,#42314,#42315);
#34741=AXIS2_PLACEMENT_3D('',#65280,#42316,#42317);
#34742=AXIS2_PLACEMENT_3D('',#65282,#42319,#42320);
#34743=AXIS2_PLACEMENT_3D('',#65284,#42322,#42323);
#34744=AXIS2_PLACEMENT_3D('',#65285,#42324,#42325);
#34745=AXIS2_PLACEMENT_3D('',#65287,#42327,#42328);
#34746=AXIS2_PLACEMENT_3D('',#65289,#42330,#42331);
#34747=AXIS2_PLACEMENT_3D('',#65290,#42332,#42333);
#34748=AXIS2_PLACEMENT_3D('',#65292,#42335,#42336);
#34749=AXIS2_PLACEMENT_3D('',#65294,#42338,#42339);
#34750=AXIS2_PLACEMENT_3D('',#65295,#42340,#42341);
#34751=AXIS2_PLACEMENT_3D('',#65297,#42343,#42344);
#34752=AXIS2_PLACEMENT_3D('',#65299,#42346,#42347);
#34753=AXIS2_PLACEMENT_3D('',#65300,#42348,#42349);
#34754=AXIS2_PLACEMENT_3D('',#65301,#42350,#42351);
#34755=AXIS2_PLACEMENT_3D('',#65302,#42352,#42353);
#34756=AXIS2_PLACEMENT_3D('',#65303,#42354,#42355);
#34757=AXIS2_PLACEMENT_3D('',#65304,#42356,#42357);
#34758=AXIS2_PLACEMENT_3D('',#65305,#42358,#42359);
#34759=AXIS2_PLACEMENT_3D('',#65306,#42360,#42361);
#34760=AXIS2_PLACEMENT_3D('',#65307,#42362,#42363);
#34761=AXIS2_PLACEMENT_3D('',#65308,#42364,#42365);
#34762=AXIS2_PLACEMENT_3D('',#65309,#42366,#42367);
#34763=AXIS2_PLACEMENT_3D('',#65310,#42368,#42369);
#34764=AXIS2_PLACEMENT_3D('',#65311,#42370,#42371);
#34765=AXIS2_PLACEMENT_3D('',#65312,#42372,#42373);
#34766=AXIS2_PLACEMENT_3D('',#65313,#42374,#42375);
#34767=AXIS2_PLACEMENT_3D('',#65314,#42376,#42377);
#34768=AXIS2_PLACEMENT_3D('',#65315,#42378,#42379);
#34769=AXIS2_PLACEMENT_3D('',#65316,#42380,#42381);
#34770=AXIS2_PLACEMENT_3D('',#65317,#42382,#42383);
#34771=AXIS2_PLACEMENT_3D('',#65318,#42384,#42385);
#34772=AXIS2_PLACEMENT_3D('',#65320,#42387,#42388);
#34773=AXIS2_PLACEMENT_3D('',#65322,#42390,#42391);
#34774=AXIS2_PLACEMENT_3D('',#65323,#42392,#42393);
#34775=AXIS2_PLACEMENT_3D('',#65325,#42395,#42396);
#34776=AXIS2_PLACEMENT_3D('',#65327,#42398,#42399);
#34777=AXIS2_PLACEMENT_3D('',#65328,#42400,#42401);
#34778=AXIS2_PLACEMENT_3D('',#65330,#42403,#42404);
#34779=AXIS2_PLACEMENT_3D('',#65332,#42406,#42407);
#34780=AXIS2_PLACEMENT_3D('',#65333,#42408,#42409);
#34781=AXIS2_PLACEMENT_3D('',#65335,#42411,#42412);
#34782=AXIS2_PLACEMENT_3D('',#65337,#42414,#42415);
#34783=AXIS2_PLACEMENT_3D('',#65338,#42416,#42417);
#34784=AXIS2_PLACEMENT_3D('',#65340,#42419,#42420);
#34785=AXIS2_PLACEMENT_3D('',#65342,#42422,#42423);
#34786=AXIS2_PLACEMENT_3D('',#65343,#42424,#42425);
#34787=AXIS2_PLACEMENT_3D('',#65345,#42427,#42428);
#34788=AXIS2_PLACEMENT_3D('',#65347,#42430,#42431);
#34789=AXIS2_PLACEMENT_3D('',#65348,#42432,#42433);
#34790=AXIS2_PLACEMENT_3D('',#65350,#42435,#42436);
#34791=AXIS2_PLACEMENT_3D('',#65352,#42438,#42439);
#34792=AXIS2_PLACEMENT_3D('',#65353,#42440,#42441);
#34793=AXIS2_PLACEMENT_3D('',#65355,#42443,#42444);
#34794=AXIS2_PLACEMENT_3D('',#65357,#42446,#42447);
#34795=AXIS2_PLACEMENT_3D('',#65358,#42448,#42449);
#34796=AXIS2_PLACEMENT_3D('',#65360,#42451,#42452);
#34797=AXIS2_PLACEMENT_3D('',#65362,#42454,#42455);
#34798=AXIS2_PLACEMENT_3D('',#65363,#42456,#42457);
#34799=AXIS2_PLACEMENT_3D('',#65365,#42459,#42460);
#34800=AXIS2_PLACEMENT_3D('',#65367,#42462,#42463);
#34801=AXIS2_PLACEMENT_3D('',#65368,#42464,#42465);
#34802=AXIS2_PLACEMENT_3D('',#65370,#42467,#42468);
#34803=AXIS2_PLACEMENT_3D('',#65372,#42470,#42471);
#34804=AXIS2_PLACEMENT_3D('',#65373,#42472,#42473);
#34805=AXIS2_PLACEMENT_3D('',#65375,#42475,#42476);
#34806=AXIS2_PLACEMENT_3D('',#65377,#42478,#42479);
#34807=AXIS2_PLACEMENT_3D('',#65378,#42480,#42481);
#34808=AXIS2_PLACEMENT_3D('',#65380,#42483,#42484);
#34809=AXIS2_PLACEMENT_3D('',#65382,#42486,#42487);
#34810=AXIS2_PLACEMENT_3D('',#65383,#42488,#42489);
#34811=AXIS2_PLACEMENT_3D('',#65385,#42491,#42492);
#34812=AXIS2_PLACEMENT_3D('',#65387,#42494,#42495);
#34813=AXIS2_PLACEMENT_3D('',#65388,#42496,#42497);
#34814=AXIS2_PLACEMENT_3D('',#65390,#42499,#42500);
#34815=AXIS2_PLACEMENT_3D('',#65392,#42502,#42503);
#34816=AXIS2_PLACEMENT_3D('',#65393,#42504,#42505);
#34817=AXIS2_PLACEMENT_3D('',#65395,#42507,#42508);
#34818=AXIS2_PLACEMENT_3D('',#65397,#42510,#42511);
#34819=AXIS2_PLACEMENT_3D('',#65398,#42512,#42513);
#34820=AXIS2_PLACEMENT_3D('',#65400,#42515,#42516);
#34821=AXIS2_PLACEMENT_3D('',#65402,#42518,#42519);
#34822=AXIS2_PLACEMENT_3D('',#65403,#42520,#42521);
#34823=AXIS2_PLACEMENT_3D('',#65405,#42523,#42524);
#34824=AXIS2_PLACEMENT_3D('',#65407,#42526,#42527);
#34825=AXIS2_PLACEMENT_3D('',#65408,#42528,#42529);
#34826=AXIS2_PLACEMENT_3D('',#65410,#42531,#42532);
#34827=AXIS2_PLACEMENT_3D('',#65412,#42534,#42535);
#34828=AXIS2_PLACEMENT_3D('',#65413,#42536,#42537);
#34829=AXIS2_PLACEMENT_3D('',#65415,#42539,#42540);
#34830=AXIS2_PLACEMENT_3D('',#65417,#42542,#42543);
#34831=AXIS2_PLACEMENT_3D('',#65418,#42544,#42545);
#34832=AXIS2_PLACEMENT_3D('',#65420,#42547,#42548);
#34833=AXIS2_PLACEMENT_3D('',#65422,#42550,#42551);
#34834=AXIS2_PLACEMENT_3D('',#65423,#42552,#42553);
#34835=AXIS2_PLACEMENT_3D('',#65425,#42555,#42556);
#34836=AXIS2_PLACEMENT_3D('',#65427,#42558,#42559);
#34837=AXIS2_PLACEMENT_3D('',#65428,#42560,#42561);
#34838=AXIS2_PLACEMENT_3D('',#65430,#42563,#42564);
#34839=AXIS2_PLACEMENT_3D('',#65432,#42566,#42567);
#34840=AXIS2_PLACEMENT_3D('',#65433,#42568,#42569);
#34841=AXIS2_PLACEMENT_3D('',#65435,#42571,#42572);
#34842=AXIS2_PLACEMENT_3D('',#65437,#42574,#42575);
#34843=AXIS2_PLACEMENT_3D('',#65438,#42576,#42577);
#34844=AXIS2_PLACEMENT_3D('',#65440,#42579,#42580);
#34845=AXIS2_PLACEMENT_3D('',#65442,#42582,#42583);
#34846=AXIS2_PLACEMENT_3D('',#65443,#42584,#42585);
#34847=AXIS2_PLACEMENT_3D('',#65445,#42587,#42588);
#34848=AXIS2_PLACEMENT_3D('',#65447,#42590,#42591);
#34849=AXIS2_PLACEMENT_3D('',#65448,#42592,#42593);
#34850=AXIS2_PLACEMENT_3D('',#65450,#42595,#42596);
#34851=AXIS2_PLACEMENT_3D('',#65452,#42598,#42599);
#34852=AXIS2_PLACEMENT_3D('',#65453,#42600,#42601);
#34853=AXIS2_PLACEMENT_3D('',#65455,#42603,#42604);
#34854=AXIS2_PLACEMENT_3D('',#65457,#42606,#42607);
#34855=AXIS2_PLACEMENT_3D('',#65458,#42608,#42609);
#34856=AXIS2_PLACEMENT_3D('',#65460,#42611,#42612);
#34857=AXIS2_PLACEMENT_3D('',#65462,#42614,#42615);
#34858=AXIS2_PLACEMENT_3D('',#65463,#42616,#42617);
#34859=AXIS2_PLACEMENT_3D('',#65465,#42619,#42620);
#34860=AXIS2_PLACEMENT_3D('',#65467,#42622,#42623);
#34861=AXIS2_PLACEMENT_3D('',#65468,#42624,#42625);
#34862=AXIS2_PLACEMENT_3D('',#65470,#42627,#42628);
#34863=AXIS2_PLACEMENT_3D('',#65472,#42630,#42631);
#34864=AXIS2_PLACEMENT_3D('',#65473,#42632,#42633);
#34865=AXIS2_PLACEMENT_3D('',#65475,#42635,#42636);
#34866=AXIS2_PLACEMENT_3D('',#65477,#42638,#42639);
#34867=AXIS2_PLACEMENT_3D('',#65478,#42640,#42641);
#34868=AXIS2_PLACEMENT_3D('',#65480,#42643,#42644);
#34869=AXIS2_PLACEMENT_3D('',#65482,#42646,#42647);
#34870=AXIS2_PLACEMENT_3D('',#65483,#42648,#42649);
#34871=AXIS2_PLACEMENT_3D('',#65485,#42651,#42652);
#34872=AXIS2_PLACEMENT_3D('',#65487,#42654,#42655);
#34873=AXIS2_PLACEMENT_3D('',#65488,#42656,#42657);
#34874=AXIS2_PLACEMENT_3D('',#65490,#42659,#42660);
#34875=AXIS2_PLACEMENT_3D('',#65492,#42662,#42663);
#34876=AXIS2_PLACEMENT_3D('',#65493,#42664,#42665);
#34877=AXIS2_PLACEMENT_3D('',#65495,#42667,#42668);
#34878=AXIS2_PLACEMENT_3D('',#65497,#42670,#42671);
#34879=AXIS2_PLACEMENT_3D('',#65498,#42672,#42673);
#34880=AXIS2_PLACEMENT_3D('',#65500,#42675,#42676);
#34881=AXIS2_PLACEMENT_3D('',#65502,#42678,#42679);
#34882=AXIS2_PLACEMENT_3D('',#65503,#42680,#42681);
#34883=AXIS2_PLACEMENT_3D('',#65505,#42683,#42684);
#34884=AXIS2_PLACEMENT_3D('',#65507,#42686,#42687);
#34885=AXIS2_PLACEMENT_3D('',#65508,#42688,#42689);
#34886=AXIS2_PLACEMENT_3D('',#65510,#42691,#42692);
#34887=AXIS2_PLACEMENT_3D('',#65512,#42694,#42695);
#34888=AXIS2_PLACEMENT_3D('',#65513,#42696,#42697);
#34889=AXIS2_PLACEMENT_3D('',#65515,#42699,#42700);
#34890=AXIS2_PLACEMENT_3D('',#65517,#42702,#42703);
#34891=AXIS2_PLACEMENT_3D('',#65518,#42704,#42705);
#34892=AXIS2_PLACEMENT_3D('',#65520,#42707,#42708);
#34893=AXIS2_PLACEMENT_3D('',#65522,#42710,#42711);
#34894=AXIS2_PLACEMENT_3D('',#65523,#42712,#42713);
#34895=AXIS2_PLACEMENT_3D('',#65525,#42715,#42716);
#34896=AXIS2_PLACEMENT_3D('',#65527,#42718,#42719);
#34897=AXIS2_PLACEMENT_3D('',#65528,#42720,#42721);
#34898=AXIS2_PLACEMENT_3D('',#65530,#42723,#42724);
#34899=AXIS2_PLACEMENT_3D('',#65532,#42726,#42727);
#34900=AXIS2_PLACEMENT_3D('',#65533,#42728,#42729);
#34901=AXIS2_PLACEMENT_3D('',#65535,#42731,#42732);
#34902=AXIS2_PLACEMENT_3D('',#65537,#42734,#42735);
#34903=AXIS2_PLACEMENT_3D('',#65538,#42736,#42737);
#34904=AXIS2_PLACEMENT_3D('',#65540,#42739,#42740);
#34905=AXIS2_PLACEMENT_3D('',#65542,#42742,#42743);
#34906=AXIS2_PLACEMENT_3D('',#65543,#42744,#42745);
#34907=AXIS2_PLACEMENT_3D('',#65545,#42747,#42748);
#34908=AXIS2_PLACEMENT_3D('',#65547,#42750,#42751);
#34909=AXIS2_PLACEMENT_3D('',#65548,#42752,#42753);
#34910=AXIS2_PLACEMENT_3D('',#65550,#42755,#42756);
#34911=AXIS2_PLACEMENT_3D('',#65552,#42758,#42759);
#34912=AXIS2_PLACEMENT_3D('',#65553,#42760,#42761);
#34913=AXIS2_PLACEMENT_3D('',#65555,#42763,#42764);
#34914=AXIS2_PLACEMENT_3D('',#65557,#42766,#42767);
#34915=AXIS2_PLACEMENT_3D('',#65558,#42768,#42769);
#34916=AXIS2_PLACEMENT_3D('',#65560,#42771,#42772);
#34917=AXIS2_PLACEMENT_3D('',#65562,#42774,#42775);
#34918=AXIS2_PLACEMENT_3D('',#65563,#42776,#42777);
#34919=AXIS2_PLACEMENT_3D('',#65565,#42779,#42780);
#34920=AXIS2_PLACEMENT_3D('',#65567,#42782,#42783);
#34921=AXIS2_PLACEMENT_3D('',#65568,#42784,#42785);
#34922=AXIS2_PLACEMENT_3D('',#65570,#42787,#42788);
#34923=AXIS2_PLACEMENT_3D('',#65572,#42790,#42791);
#34924=AXIS2_PLACEMENT_3D('',#65573,#42792,#42793);
#34925=AXIS2_PLACEMENT_3D('',#65575,#42795,#42796);
#34926=AXIS2_PLACEMENT_3D('',#65577,#42798,#42799);
#34927=AXIS2_PLACEMENT_3D('',#65578,#42800,#42801);
#34928=AXIS2_PLACEMENT_3D('',#65580,#42803,#42804);
#34929=AXIS2_PLACEMENT_3D('',#65582,#42806,#42807);
#34930=AXIS2_PLACEMENT_3D('',#65583,#42808,#42809);
#34931=AXIS2_PLACEMENT_3D('',#65585,#42811,#42812);
#34932=AXIS2_PLACEMENT_3D('',#65587,#42814,#42815);
#34933=AXIS2_PLACEMENT_3D('',#65588,#42816,#42817);
#34934=AXIS2_PLACEMENT_3D('',#65590,#42819,#42820);
#34935=AXIS2_PLACEMENT_3D('',#65592,#42822,#42823);
#34936=AXIS2_PLACEMENT_3D('',#65593,#42824,#42825);
#34937=AXIS2_PLACEMENT_3D('',#65595,#42827,#42828);
#34938=AXIS2_PLACEMENT_3D('',#65597,#42830,#42831);
#34939=AXIS2_PLACEMENT_3D('',#65598,#42832,#42833);
#34940=AXIS2_PLACEMENT_3D('',#65600,#42835,#42836);
#34941=AXIS2_PLACEMENT_3D('',#65602,#42838,#42839);
#34942=AXIS2_PLACEMENT_3D('',#65603,#42840,#42841);
#34943=AXIS2_PLACEMENT_3D('',#65605,#42843,#42844);
#34944=AXIS2_PLACEMENT_3D('',#65607,#42846,#42847);
#34945=AXIS2_PLACEMENT_3D('',#65608,#42848,#42849);
#34946=AXIS2_PLACEMENT_3D('',#65609,#42850,#42851);
#34947=AXIS2_PLACEMENT_3D('',#65610,#42852,#42853);
#34948=AXIS2_PLACEMENT_3D('',#65611,#42854,#42855);
#34949=AXIS2_PLACEMENT_3D('',#65612,#42856,#42857);
#34950=AXIS2_PLACEMENT_3D('',#65613,#42858,#42859);
#34951=AXIS2_PLACEMENT_3D('',#65614,#42860,#42861);
#34952=AXIS2_PLACEMENT_3D('',#65615,#42862,#42863);
#34953=AXIS2_PLACEMENT_3D('',#65616,#42864,#42865);
#34954=AXIS2_PLACEMENT_3D('',#65617,#42866,#42867);
#34955=AXIS2_PLACEMENT_3D('',#65618,#42868,#42869);
#34956=AXIS2_PLACEMENT_3D('',#65619,#42870,#42871);
#34957=AXIS2_PLACEMENT_3D('',#65620,#42872,#42873);
#34958=AXIS2_PLACEMENT_3D('',#65621,#42874,#42875);
#34959=AXIS2_PLACEMENT_3D('',#65664,#42878,#42879);
#34960=AXIS2_PLACEMENT_3D('',#65666,#42880,#42881);
#34961=AXIS2_PLACEMENT_3D('',#65701,#42882,#42883);
#34962=AXIS2_PLACEMENT_3D('',#65777,#42885,#42886);
#34963=AXIS2_PLACEMENT_3D('',#65855,#42888,#42889);
#34964=AXIS2_PLACEMENT_3D('',#65931,#42891,#42892);
#34965=AXIS2_PLACEMENT_3D('',#66007,#42894,#42895);
#34966=AXIS2_PLACEMENT_3D('',#66083,#42897,#42898);
#34967=AXIS2_PLACEMENT_3D('',#66159,#42900,#42901);
#34968=AXIS2_PLACEMENT_3D('',#66237,#42903,#42904);
#34969=AXIS2_PLACEMENT_3D('',#66315,#42906,#42907);
#34970=AXIS2_PLACEMENT_3D('',#66391,#42909,#42910);
#34971=AXIS2_PLACEMENT_3D('',#66467,#42912,#42913);
#34972=AXIS2_PLACEMENT_3D('',#66543,#42915,#42916);
#34973=AXIS2_PLACEMENT_3D('',#66619,#42918,#42919);
#34974=AXIS2_PLACEMENT_3D('',#66697,#42921,#42922);
#34975=AXIS2_PLACEMENT_3D('',#66773,#42924,#42925);
#34976=AXIS2_PLACEMENT_3D('',#66851,#42927,#42928);
#34977=AXIS2_PLACEMENT_3D('',#66927,#42930,#42931);
#34978=AXIS2_PLACEMENT_3D('',#67003,#42933,#42934);
#34979=AXIS2_PLACEMENT_3D('',#67079,#42936,#42937);
#34980=AXIS2_PLACEMENT_3D('',#67155,#42939,#42940);
#34981=AXIS2_PLACEMENT_3D('',#67233,#42942,#42943);
#34982=AXIS2_PLACEMENT_3D('',#67311,#42945,#42946);
#34983=AXIS2_PLACEMENT_3D('',#67387,#42948,#42949);
#34984=AXIS2_PLACEMENT_3D('',#67463,#42951,#42952);
#34985=AXIS2_PLACEMENT_3D('',#67539,#42954,#42955);
#34986=AXIS2_PLACEMENT_3D('',#67615,#42957,#42958);
#34987=AXIS2_PLACEMENT_3D('',#67693,#42960,#42961);
#34988=AXIS2_PLACEMENT_3D('',#67769,#42963,#42964);
#34989=AXIS2_PLACEMENT_3D('',#67794,#42966,#42967);
#34990=AXIS2_PLACEMENT_3D('',#67795,#42968,#42969);
#34991=AXIS2_PLACEMENT_3D('',#67807,#42971,#42972);
#34992=AXIS2_PLACEMENT_3D('',#67808,#42973,#42974);
#34993=AXIS2_PLACEMENT_3D('',#67884,#42976,#42977);
#34994=AXIS2_PLACEMENT_3D('',#67960,#42979,#42980);
#34995=AXIS2_PLACEMENT_3D('',#68038,#42982,#42983);
#34996=AXIS2_PLACEMENT_3D('',#68114,#42985,#42986);
#34997=AXIS2_PLACEMENT_3D('',#68192,#42988,#42989);
#34998=AXIS2_PLACEMENT_3D('',#68268,#42991,#42992);
#34999=AXIS2_PLACEMENT_3D('',#68344,#42994,#42995);
#35000=AXIS2_PLACEMENT_3D('',#68420,#42997,#42998);
#35001=AXIS2_PLACEMENT_3D('',#68496,#43000,#43001);
#35002=AXIS2_PLACEMENT_3D('',#68574,#43003,#43004);
#35003=AXIS2_PLACEMENT_3D('',#68650,#43006,#43007);
#35004=AXIS2_PLACEMENT_3D('',#68728,#43009,#43010);
#35005=AXIS2_PLACEMENT_3D('',#68804,#43012,#43013);
#35006=AXIS2_PLACEMENT_3D('',#68880,#43015,#43016);
#35007=AXIS2_PLACEMENT_3D('',#68956,#43018,#43019);
#35008=AXIS2_PLACEMENT_3D('',#69032,#43021,#43022);
#35009=AXIS2_PLACEMENT_3D('',#69108,#43024,#43025);
#35010=AXIS2_PLACEMENT_3D('',#69186,#43027,#43028);
#35011=AXIS2_PLACEMENT_3D('',#69262,#43030,#43031);
#35012=AXIS2_PLACEMENT_3D('',#69340,#43033,#43034);
#35013=AXIS2_PLACEMENT_3D('',#69416,#43036,#43037);
#35014=AXIS2_PLACEMENT_3D('',#69492,#43039,#43040);
#35015=AXIS2_PLACEMENT_3D('',#69568,#43042,#43043);
#35016=AXIS2_PLACEMENT_3D('',#69644,#43045,#43046);
#35017=AXIS2_PLACEMENT_3D('',#69722,#43048,#43049);
#35018=AXIS2_PLACEMENT_3D('',#69798,#43051,#43052);
#35019=AXIS2_PLACEMENT_3D('',#69876,#43054,#43055);
#35020=AXIS2_PLACEMENT_3D('',#69952,#43057,#43058);
#35021=AXIS2_PLACEMENT_3D('',#70028,#43060,#43061);
#35022=AXIS2_PLACEMENT_3D('',#70038,#43062,#43063);
#35023=AXIS2_PLACEMENT_3D('',#70039,#43064,#43065);
#35024=AXIS2_PLACEMENT_3D('',#70040,#43066,#43067);
#35025=AXIS2_PLACEMENT_3D('',#70055,#43068,#43069);
#35026=AXIS2_PLACEMENT_3D('',#70078,#43070,#43071);
#35027=AXIS2_PLACEMENT_3D('',#70145,#43072,#43073);
#35028=AXIS2_PLACEMENT_3D('',#70148,#43074,#43075);
#35029=AXIS2_PLACEMENT_3D('',#70152,#43077,#43078);
#35030=AXIS2_PLACEMENT_3D('',#70154,#43080,#43081);
#35031=AXIS2_PLACEMENT_3D('',#70157,#43082,#43083);
#35032=AXIS2_PLACEMENT_3D('',#70161,#43085,#43086);
#35033=AXIS2_PLACEMENT_3D('',#70163,#43088,#43089);
#35034=AXIS2_PLACEMENT_3D('',#70166,#43090,#43091);
#35035=AXIS2_PLACEMENT_3D('',#70170,#43093,#43094);
#35036=AXIS2_PLACEMENT_3D('',#70172,#43096,#43097);
#35037=AXIS2_PLACEMENT_3D('',#70175,#43098,#43099);
#35038=AXIS2_PLACEMENT_3D('',#70179,#43101,#43102);
#35039=AXIS2_PLACEMENT_3D('',#70181,#43104,#43105);
#35040=AXIS2_PLACEMENT_3D('',#70184,#43106,#43107);
#35041=AXIS2_PLACEMENT_3D('',#70188,#43109,#43110);
#35042=AXIS2_PLACEMENT_3D('',#70190,#43112,#43113);
#35043=AXIS2_PLACEMENT_3D('',#70193,#43114,#43115);
#35044=AXIS2_PLACEMENT_3D('',#70197,#43117,#43118);
#35045=AXIS2_PLACEMENT_3D('',#70199,#43120,#43121);
#35046=AXIS2_PLACEMENT_3D('',#70202,#43122,#43123);
#35047=AXIS2_PLACEMENT_3D('',#70206,#43125,#43126);
#35048=AXIS2_PLACEMENT_3D('',#70208,#43128,#43129);
#35049=AXIS2_PLACEMENT_3D('',#70211,#43130,#43131);
#35050=AXIS2_PLACEMENT_3D('',#70215,#43133,#43134);
#35051=AXIS2_PLACEMENT_3D('',#70217,#43136,#43137);
#35052=AXIS2_PLACEMENT_3D('',#70220,#43138,#43139);
#35053=AXIS2_PLACEMENT_3D('',#70224,#43141,#43142);
#35054=AXIS2_PLACEMENT_3D('',#70226,#43144,#43145);
#35055=AXIS2_PLACEMENT_3D('',#70229,#43146,#43147);
#35056=AXIS2_PLACEMENT_3D('',#70233,#43149,#43150);
#35057=AXIS2_PLACEMENT_3D('',#70235,#43152,#43153);
#35058=AXIS2_PLACEMENT_3D('',#70238,#43154,#43155);
#35059=AXIS2_PLACEMENT_3D('',#70242,#43157,#43158);
#35060=AXIS2_PLACEMENT_3D('',#70244,#43160,#43161);
#35061=AXIS2_PLACEMENT_3D('',#70247,#43162,#43163);
#35062=AXIS2_PLACEMENT_3D('',#70251,#43165,#43166);
#35063=AXIS2_PLACEMENT_3D('',#70253,#43168,#43169);
#35064=AXIS2_PLACEMENT_3D('',#70256,#43170,#43171);
#35065=AXIS2_PLACEMENT_3D('',#70260,#43173,#43174);
#35066=AXIS2_PLACEMENT_3D('',#70262,#43176,#43177);
#35067=AXIS2_PLACEMENT_3D('',#70265,#43178,#43179);
#35068=AXIS2_PLACEMENT_3D('',#70269,#43181,#43182);
#35069=AXIS2_PLACEMENT_3D('',#70271,#43184,#43185);
#35070=AXIS2_PLACEMENT_3D('',#70274,#43186,#43187);
#35071=AXIS2_PLACEMENT_3D('',#70278,#43189,#43190);
#35072=AXIS2_PLACEMENT_3D('',#70280,#43192,#43193);
#35073=AXIS2_PLACEMENT_3D('',#70311,#43195,#43196);
#35074=AXIS2_PLACEMENT_3D('',#70312,#43197,#43198);
#35075=AXIS2_PLACEMENT_3D('',#70314,#43199,#43200);
#35076=AXIS2_PLACEMENT_3D('',#70316,#43201,#43202);
#35077=AXIS2_PLACEMENT_3D('',#70317,#43203,#43204);
#35078=AXIS2_PLACEMENT_3D('',#70318,#43205,#43206);
#35079=AXIS2_PLACEMENT_3D('',#70334,#43207,#43208);
#35080=AXIS2_PLACEMENT_3D('',#70340,#43209,#43210);
#35081=AXIS2_PLACEMENT_3D('',#70346,#43211,#43212);
#35082=AXIS2_PLACEMENT_3D('',#70352,#43213,#43214);
#35083=AXIS2_PLACEMENT_3D('',#70358,#43215,#43216);
#35084=AXIS2_PLACEMENT_3D('',#70364,#43217,#43218);
#35085=AXIS2_PLACEMENT_3D('',#70370,#43219,#43220);
#35086=AXIS2_PLACEMENT_3D('',#70376,#43221,#43222);
#35087=AXIS2_PLACEMENT_3D('',#70382,#43223,#43224);
#35088=AXIS2_PLACEMENT_3D('',#70388,#43225,#43226);
#35089=AXIS2_PLACEMENT_3D('',#70394,#43227,#43228);
#35090=AXIS2_PLACEMENT_3D('',#70400,#43229,#43230);
#35091=AXIS2_PLACEMENT_3D('',#70406,#43231,#43232);
#35092=AXIS2_PLACEMENT_3D('',#70412,#43233,#43234);
#35093=AXIS2_PLACEMENT_3D('',#70418,#43235,#43236);
#35094=AXIS2_PLACEMENT_3D('',#70424,#43237,#43238);
#35095=AXIS2_PLACEMENT_3D('',#70430,#43239,#43240);
#35096=AXIS2_PLACEMENT_3D('',#70436,#43241,#43242);
#35097=AXIS2_PLACEMENT_3D('',#70442,#43243,#43244);
#35098=AXIS2_PLACEMENT_3D('',#70448,#43245,#43246);
#35099=AXIS2_PLACEMENT_3D('',#70454,#43247,#43248);
#35100=AXIS2_PLACEMENT_3D('',#70460,#43249,#43250);
#35101=AXIS2_PLACEMENT_3D('',#70466,#43251,#43252);
#35102=AXIS2_PLACEMENT_3D('',#70472,#43253,#43254);
#35103=AXIS2_PLACEMENT_3D('',#70478,#43255,#43256);
#35104=AXIS2_PLACEMENT_3D('',#70484,#43257,#43258);
#35105=AXIS2_PLACEMENT_3D('',#70490,#43259,#43260);
#35106=AXIS2_PLACEMENT_3D('',#70496,#43261,#43262);
#35107=AXIS2_PLACEMENT_3D('',#70502,#43263,#43264);
#35108=AXIS2_PLACEMENT_3D('',#70508,#43265,#43266);
#35109=AXIS2_PLACEMENT_3D('',#70514,#43267,#43268);
#35110=AXIS2_PLACEMENT_3D('',#70520,#43269,#43270);
#35111=AXIS2_PLACEMENT_3D('',#70526,#43271,#43272);
#35112=AXIS2_PLACEMENT_3D('',#70532,#43273,#43274);
#35113=AXIS2_PLACEMENT_3D('',#70538,#43275,#43276);
#35114=AXIS2_PLACEMENT_3D('',#70544,#43277,#43278);
#35115=AXIS2_PLACEMENT_3D('',#70550,#43279,#43280);
#35116=AXIS2_PLACEMENT_3D('',#70556,#43281,#43282);
#35117=AXIS2_PLACEMENT_3D('',#70562,#43283,#43284);
#35118=AXIS2_PLACEMENT_3D('',#70568,#43285,#43286);
#35119=AXIS2_PLACEMENT_3D('',#70574,#43287,#43288);
#35120=AXIS2_PLACEMENT_3D('',#70580,#43289,#43290);
#35121=AXIS2_PLACEMENT_3D('',#70586,#43291,#43292);
#35122=AXIS2_PLACEMENT_3D('',#70592,#43293,#43294);
#35123=AXIS2_PLACEMENT_3D('',#70598,#43295,#43296);
#35124=AXIS2_PLACEMENT_3D('',#70604,#43297,#43298);
#35125=AXIS2_PLACEMENT_3D('',#70610,#43299,#43300);
#35126=AXIS2_PLACEMENT_3D('',#70616,#43301,#43302);
#35127=AXIS2_PLACEMENT_3D('',#70622,#43303,#43304);
#35128=AXIS2_PLACEMENT_3D('',#70628,#43305,#43306);
#35129=AXIS2_PLACEMENT_3D('',#70634,#43307,#43308);
#35130=AXIS2_PLACEMENT_3D('',#70640,#43309,#43310);
#35131=AXIS2_PLACEMENT_3D('',#70646,#43311,#43312);
#35132=AXIS2_PLACEMENT_3D('',#70652,#43313,#43314);
#35133=AXIS2_PLACEMENT_3D('',#70658,#43315,#43316);
#35134=AXIS2_PLACEMENT_3D('',#70664,#43317,#43318);
#35135=AXIS2_PLACEMENT_3D('',#70670,#43319,#43320);
#35136=AXIS2_PLACEMENT_3D('',#70676,#43321,#43322);
#35137=AXIS2_PLACEMENT_3D('',#70682,#43323,#43324);
#35138=AXIS2_PLACEMENT_3D('',#70688,#43325,#43326);
#35139=AXIS2_PLACEMENT_3D('',#70694,#43327,#43328);
#35140=AXIS2_PLACEMENT_3D('',#70700,#43329,#43330);
#35141=AXIS2_PLACEMENT_3D('',#70706,#43331,#43332);
#35142=AXIS2_PLACEMENT_3D('',#70712,#43333,#43334);
#35143=AXIS2_PLACEMENT_3D('',#70718,#43335,#43336);
#35144=AXIS2_PLACEMENT_3D('',#70724,#43337,#43338);
#35145=AXIS2_PLACEMENT_3D('',#70730,#43339,#43340);
#35146=AXIS2_PLACEMENT_3D('',#70736,#43341,#43342);
#35147=AXIS2_PLACEMENT_3D('',#70742,#43343,#43344);
#35148=AXIS2_PLACEMENT_3D('',#70748,#43345,#43346);
#35149=AXIS2_PLACEMENT_3D('',#70754,#43347,#43348);
#35150=AXIS2_PLACEMENT_3D('',#70760,#43349,#43350);
#35151=AXIS2_PLACEMENT_3D('',#70766,#43351,#43352);
#35152=AXIS2_PLACEMENT_3D('',#70772,#43353,#43354);
#35153=AXIS2_PLACEMENT_3D('',#70778,#43355,#43356);
#35154=AXIS2_PLACEMENT_3D('',#70784,#43357,#43358);
#35155=AXIS2_PLACEMENT_3D('',#70790,#43359,#43360);
#35156=AXIS2_PLACEMENT_3D('',#70796,#43361,#43362);
#35157=AXIS2_PLACEMENT_3D('',#70802,#43363,#43364);
#35158=AXIS2_PLACEMENT_3D('',#70808,#43365,#43366);
#35159=AXIS2_PLACEMENT_3D('',#70814,#43367,#43368);
#35160=AXIS2_PLACEMENT_3D('',#70820,#43369,#43370);
#35161=AXIS2_PLACEMENT_3D('',#70826,#43371,#43372);
#35162=AXIS2_PLACEMENT_3D('',#70832,#43373,#43374);
#35163=AXIS2_PLACEMENT_3D('',#70838,#43375,#43376);
#35164=AXIS2_PLACEMENT_3D('',#70844,#43377,#43378);
#35165=AXIS2_PLACEMENT_3D('',#70850,#43379,#43380);
#35166=AXIS2_PLACEMENT_3D('',#70856,#43381,#43382);
#35167=AXIS2_PLACEMENT_3D('',#70862,#43383,#43384);
#35168=AXIS2_PLACEMENT_3D('',#70868,#43385,#43386);
#35169=AXIS2_PLACEMENT_3D('',#70874,#43387,#43388);
#35170=AXIS2_PLACEMENT_3D('',#70883,#43389,#43390);
#35171=AXIS2_PLACEMENT_3D('',#70892,#43391,#43392);
#35172=AXIS2_PLACEMENT_3D('',#70901,#43393,#43394);
#35173=AXIS2_PLACEMENT_3D('',#70910,#43395,#43396);
#35174=AXIS2_PLACEMENT_3D('',#70919,#43397,#43398);
#35175=AXIS2_PLACEMENT_3D('',#70928,#43399,#43400);
#35176=AXIS2_PLACEMENT_3D('',#70937,#43401,#43402);
#35177=AXIS2_PLACEMENT_3D('',#70946,#43403,#43404);
#35178=AXIS2_PLACEMENT_3D('',#70955,#43405,#43406);
#35179=AXIS2_PLACEMENT_3D('',#70964,#43407,#43408);
#35180=AXIS2_PLACEMENT_3D('',#70973,#43409,#43410);
#35181=AXIS2_PLACEMENT_3D('',#70982,#43411,#43412);
#35182=AXIS2_PLACEMENT_3D('',#70991,#43413,#43414);
#35183=AXIS2_PLACEMENT_3D('',#71000,#43415,#43416);
#35184=AXIS2_PLACEMENT_3D('',#71009,#43417,#43418);
#35185=AXIS2_PLACEMENT_3D('',#71015,#43419,#43420);
#35186=AXIS2_PLACEMENT_3D('',#71021,#43421,#43422);
#35187=AXIS2_PLACEMENT_3D('',#71027,#43423,#43424);
#35188=AXIS2_PLACEMENT_3D('',#71033,#43425,#43426);
#35189=AXIS2_PLACEMENT_3D('',#71039,#43427,#43428);
#35190=AXIS2_PLACEMENT_3D('',#71045,#43429,#43430);
#35191=AXIS2_PLACEMENT_3D('',#71051,#43431,#43432);
#35192=AXIS2_PLACEMENT_3D('',#71057,#43433,#43434);
#35193=AXIS2_PLACEMENT_3D('',#71063,#43435,#43436);
#35194=AXIS2_PLACEMENT_3D('',#71069,#43437,#43438);
#35195=AXIS2_PLACEMENT_3D('',#71075,#43439,#43440);
#35196=AXIS2_PLACEMENT_3D('',#71081,#43441,#43442);
#35197=AXIS2_PLACEMENT_3D('',#71087,#43443,#43444);
#35198=AXIS2_PLACEMENT_3D('',#71093,#43445,#43446);
#35199=AXIS2_PLACEMENT_3D('',#71099,#43447,#43448);
#35200=AXIS2_PLACEMENT_3D('',#71105,#43449,#43450);
#35201=AXIS2_PLACEMENT_3D('',#71111,#43451,#43452);
#35202=AXIS2_PLACEMENT_3D('',#71117,#43453,#43454);
#35203=AXIS2_PLACEMENT_3D('',#71123,#43455,#43456);
#35204=AXIS2_PLACEMENT_3D('',#71129,#43457,#43458);
#35205=AXIS2_PLACEMENT_3D('',#71135,#43459,#43460);
#35206=AXIS2_PLACEMENT_3D('',#71141,#43461,#43462);
#35207=AXIS2_PLACEMENT_3D('',#71147,#43463,#43464);
#35208=AXIS2_PLACEMENT_3D('',#71153,#43465,#43466);
#35209=AXIS2_PLACEMENT_3D('',#71159,#43467,#43468);
#35210=AXIS2_PLACEMENT_3D('',#71165,#43469,#43470);
#35211=AXIS2_PLACEMENT_3D('',#71171,#43471,#43472);
#35212=AXIS2_PLACEMENT_3D('',#71177,#43473,#43474);
#35213=AXIS2_PLACEMENT_3D('',#71183,#43475,#43476);
#35214=AXIS2_PLACEMENT_3D('',#71189,#43477,#43478);
#35215=AXIS2_PLACEMENT_3D('',#71195,#43479,#43480);
#35216=AXIS2_PLACEMENT_3D('',#71201,#43481,#43482);
#35217=AXIS2_PLACEMENT_3D('',#71207,#43483,#43484);
#35218=AXIS2_PLACEMENT_3D('',#71213,#43485,#43486);
#35219=AXIS2_PLACEMENT_3D('',#71219,#43487,#43488);
#35220=AXIS2_PLACEMENT_3D('',#71225,#43489,#43490);
#35221=AXIS2_PLACEMENT_3D('',#71231,#43491,#43492);
#35222=AXIS2_PLACEMENT_3D('',#71237,#43493,#43494);
#35223=AXIS2_PLACEMENT_3D('',#71251,#43496,#43497);
#35224=AXIS2_PLACEMENT_3D('',#71267,#43498,#43499);
#35225=AXIS2_PLACEMENT_3D('',#71273,#43500,#43501);
#35226=AXIS2_PLACEMENT_3D('',#71279,#43502,#43503);
#35227=AXIS2_PLACEMENT_3D('',#71285,#43504,#43505);
#35228=AXIS2_PLACEMENT_3D('',#71291,#43506,#43507);
#35229=AXIS2_PLACEMENT_3D('',#71297,#43508,#43509);
#35230=AXIS2_PLACEMENT_3D('',#71303,#43510,#43511);
#35231=AXIS2_PLACEMENT_3D('',#71309,#43512,#43513);
#35232=AXIS2_PLACEMENT_3D('',#71315,#43514,#43515);
#35233=AXIS2_PLACEMENT_3D('',#71321,#43516,#43517);
#35234=AXIS2_PLACEMENT_3D('',#71327,#43518,#43519);
#35235=AXIS2_PLACEMENT_3D('',#71333,#43520,#43521);
#35236=AXIS2_PLACEMENT_3D('',#71339,#43522,#43523);
#35237=AXIS2_PLACEMENT_3D('',#71345,#43524,#43525);
#35238=AXIS2_PLACEMENT_3D('',#71351,#43526,#43527);
#35239=AXIS2_PLACEMENT_3D('',#71357,#43528,#43529);
#35240=AXIS2_PLACEMENT_3D('',#71363,#43530,#43531);
#35241=AXIS2_PLACEMENT_3D('',#71369,#43532,#43533);
#35242=AXIS2_PLACEMENT_3D('',#71375,#43534,#43535);
#35243=AXIS2_PLACEMENT_3D('',#71381,#43536,#43537);
#35244=AXIS2_PLACEMENT_3D('',#71387,#43538,#43539);
#35245=AXIS2_PLACEMENT_3D('',#71393,#43540,#43541);
#35246=AXIS2_PLACEMENT_3D('',#71399,#43542,#43543);
#35247=AXIS2_PLACEMENT_3D('',#71405,#43544,#43545);
#35248=AXIS2_PLACEMENT_3D('',#71411,#43546,#43547);
#35249=AXIS2_PLACEMENT_3D('',#71417,#43548,#43549);
#35250=AXIS2_PLACEMENT_3D('',#71423,#43550,#43551);
#35251=AXIS2_PLACEMENT_3D('',#71429,#43552,#43553);
#35252=AXIS2_PLACEMENT_3D('',#71435,#43554,#43555);
#35253=AXIS2_PLACEMENT_3D('',#71441,#43556,#43557);
#35254=AXIS2_PLACEMENT_3D('',#71447,#43558,#43559);
#35255=AXIS2_PLACEMENT_3D('',#71453,#43560,#43561);
#35256=AXIS2_PLACEMENT_3D('',#71459,#43562,#43563);
#35257=AXIS2_PLACEMENT_3D('',#71465,#43564,#43565);
#35258=AXIS2_PLACEMENT_3D('',#71471,#43566,#43567);
#35259=AXIS2_PLACEMENT_3D('',#71477,#43568,#43569);
#35260=AXIS2_PLACEMENT_3D('',#71483,#43570,#43571);
#35261=AXIS2_PLACEMENT_3D('',#71489,#43572,#43573);
#35262=AXIS2_PLACEMENT_3D('',#71495,#43574,#43575);
#35263=AXIS2_PLACEMENT_3D('',#71501,#43576,#43577);
#35264=AXIS2_PLACEMENT_3D('',#71507,#43578,#43579);
#35265=AXIS2_PLACEMENT_3D('',#71513,#43580,#43581);
#35266=AXIS2_PLACEMENT_3D('',#71519,#43582,#43583);
#35267=AXIS2_PLACEMENT_3D('',#71525,#43584,#43585);
#35268=AXIS2_PLACEMENT_3D('',#71531,#43586,#43587);
#35269=AXIS2_PLACEMENT_3D('',#71537,#43588,#43589);
#35270=AXIS2_PLACEMENT_3D('',#71543,#43590,#43591);
#35271=AXIS2_PLACEMENT_3D('',#71549,#43592,#43593);
#35272=AXIS2_PLACEMENT_3D('',#71555,#43594,#43595);
#35273=AXIS2_PLACEMENT_3D('',#71561,#43596,#43597);
#35274=AXIS2_PLACEMENT_3D('',#71567,#43598,#43599);
#35275=AXIS2_PLACEMENT_3D('',#71573,#43600,#43601);
#35276=AXIS2_PLACEMENT_3D('',#71579,#43602,#43603);
#35277=AXIS2_PLACEMENT_3D('',#71585,#43604,#43605);
#35278=AXIS2_PLACEMENT_3D('',#71591,#43606,#43607);
#35279=AXIS2_PLACEMENT_3D('',#71597,#43608,#43609);
#35280=AXIS2_PLACEMENT_3D('',#71603,#43610,#43611);
#35281=AXIS2_PLACEMENT_3D('',#71609,#43612,#43613);
#35282=AXIS2_PLACEMENT_3D('',#71615,#43614,#43615);
#35283=AXIS2_PLACEMENT_3D('',#71621,#43616,#43617);
#35284=AXIS2_PLACEMENT_3D('',#71627,#43618,#43619);
#35285=AXIS2_PLACEMENT_3D('',#71633,#43620,#43621);
#35286=AXIS2_PLACEMENT_3D('',#71639,#43622,#43623);
#35287=AXIS2_PLACEMENT_3D('',#71645,#43624,#43625);
#35288=AXIS2_PLACEMENT_3D('',#71651,#43626,#43627);
#35289=AXIS2_PLACEMENT_3D('',#71657,#43628,#43629);
#35290=AXIS2_PLACEMENT_3D('',#71663,#43630,#43631);
#35291=AXIS2_PLACEMENT_3D('',#71669,#43632,#43633);
#35292=AXIS2_PLACEMENT_3D('',#71675,#43634,#43635);
#35293=AXIS2_PLACEMENT_3D('',#71681,#43636,#43637);
#35294=AXIS2_PLACEMENT_3D('',#71687,#43638,#43639);
#35295=AXIS2_PLACEMENT_3D('',#71693,#43640,#43641);
#35296=AXIS2_PLACEMENT_3D('',#71699,#43642,#43643);
#35297=AXIS2_PLACEMENT_3D('',#71705,#43644,#43645);
#35298=AXIS2_PLACEMENT_3D('',#71711,#43646,#43647);
#35299=AXIS2_PLACEMENT_3D('',#71717,#43648,#43649);
#35300=AXIS2_PLACEMENT_3D('',#71723,#43650,#43651);
#35301=AXIS2_PLACEMENT_3D('',#71729,#43652,#43653);
#35302=AXIS2_PLACEMENT_3D('',#71735,#43654,#43655);
#35303=AXIS2_PLACEMENT_3D('',#71741,#43656,#43657);
#35304=AXIS2_PLACEMENT_3D('',#71747,#43658,#43659);
#35305=AXIS2_PLACEMENT_3D('',#71753,#43660,#43661);
#35306=AXIS2_PLACEMENT_3D('',#71759,#43662,#43663);
#35307=AXIS2_PLACEMENT_3D('',#71765,#43664,#43665);
#35308=AXIS2_PLACEMENT_3D('',#71771,#43666,#43667);
#35309=AXIS2_PLACEMENT_3D('',#71777,#43668,#43669);
#35310=AXIS2_PLACEMENT_3D('',#71783,#43670,#43671);
#35311=AXIS2_PLACEMENT_3D('',#71789,#43672,#43673);
#35312=AXIS2_PLACEMENT_3D('',#71795,#43674,#43675);
#35313=AXIS2_PLACEMENT_3D('',#71801,#43676,#43677);
#35314=AXIS2_PLACEMENT_3D('',#71807,#43678,#43679);
#35315=AXIS2_PLACEMENT_3D('',#71813,#43680,#43681);
#35316=AXIS2_PLACEMENT_3D('',#71819,#43682,#43683);
#35317=AXIS2_PLACEMENT_3D('',#71825,#43684,#43685);
#35318=AXIS2_PLACEMENT_3D('',#71831,#43686,#43687);
#35319=AXIS2_PLACEMENT_3D('',#71837,#43688,#43689);
#35320=AXIS2_PLACEMENT_3D('',#71843,#43690,#43691);
#35321=AXIS2_PLACEMENT_3D('',#71849,#43692,#43693);
#35322=AXIS2_PLACEMENT_3D('',#71855,#43694,#43695);
#35323=AXIS2_PLACEMENT_3D('',#71861,#43696,#43697);
#35324=AXIS2_PLACEMENT_3D('',#71867,#43698,#43699);
#35325=AXIS2_PLACEMENT_3D('',#71873,#43700,#43701);
#35326=AXIS2_PLACEMENT_3D('',#71879,#43702,#43703);
#35327=AXIS2_PLACEMENT_3D('',#71885,#43704,#43705);
#35328=AXIS2_PLACEMENT_3D('',#71891,#43706,#43707);
#35329=AXIS2_PLACEMENT_3D('',#71897,#43708,#43709);
#35330=AXIS2_PLACEMENT_3D('',#71903,#43710,#43711);
#35331=AXIS2_PLACEMENT_3D('',#71909,#43712,#43713);
#35332=AXIS2_PLACEMENT_3D('',#71915,#43714,#43715);
#35333=AXIS2_PLACEMENT_3D('',#71921,#43716,#43717);
#35334=AXIS2_PLACEMENT_3D('',#71927,#43718,#43719);
#35335=AXIS2_PLACEMENT_3D('',#71933,#43720,#43721);
#35336=AXIS2_PLACEMENT_3D('',#71939,#43722,#43723);
#35337=AXIS2_PLACEMENT_3D('',#71945,#43724,#43725);
#35338=AXIS2_PLACEMENT_3D('',#71951,#43726,#43727);
#35339=AXIS2_PLACEMENT_3D('',#71957,#43728,#43729);
#35340=AXIS2_PLACEMENT_3D('',#71963,#43730,#43731);
#35341=AXIS2_PLACEMENT_3D('',#71969,#43732,#43733);
#35342=AXIS2_PLACEMENT_3D('',#71975,#43734,#43735);
#35343=AXIS2_PLACEMENT_3D('',#71984,#43736,#43737);
#35344=AXIS2_PLACEMENT_3D('',#71993,#43738,#43739);
#35345=AXIS2_PLACEMENT_3D('',#72002,#43740,#43741);
#35346=AXIS2_PLACEMENT_3D('',#72011,#43742,#43743);
#35347=AXIS2_PLACEMENT_3D('',#72020,#43744,#43745);
#35348=AXIS2_PLACEMENT_3D('',#72029,#43746,#43747);
#35349=AXIS2_PLACEMENT_3D('',#72038,#43748,#43749);
#35350=AXIS2_PLACEMENT_3D('',#72047,#43750,#43751);
#35351=AXIS2_PLACEMENT_3D('',#72056,#43752,#43753);
#35352=AXIS2_PLACEMENT_3D('',#72065,#43754,#43755);
#35353=AXIS2_PLACEMENT_3D('',#72074,#43756,#43757);
#35354=AXIS2_PLACEMENT_3D('',#72083,#43758,#43759);
#35355=AXIS2_PLACEMENT_3D('',#72092,#43760,#43761);
#35356=AXIS2_PLACEMENT_3D('',#72101,#43762,#43763);
#35357=AXIS2_PLACEMENT_3D('',#72110,#43764,#43765);
#35358=AXIS2_PLACEMENT_3D('',#72116,#43766,#43767);
#35359=AXIS2_PLACEMENT_3D('',#72122,#43768,#43769);
#35360=AXIS2_PLACEMENT_3D('',#72128,#43770,#43771);
#35361=AXIS2_PLACEMENT_3D('',#72134,#43772,#43773);
#35362=AXIS2_PLACEMENT_3D('',#72140,#43774,#43775);
#35363=AXIS2_PLACEMENT_3D('',#72146,#43776,#43777);
#35364=AXIS2_PLACEMENT_3D('',#72152,#43778,#43779);
#35365=AXIS2_PLACEMENT_3D('',#72158,#43780,#43781);
#35366=AXIS2_PLACEMENT_3D('',#72164,#43782,#43783);
#35367=AXIS2_PLACEMENT_3D('',#72170,#43784,#43785);
#35368=AXIS2_PLACEMENT_3D('',#72186,#43787,#43788);
#35369=AXIS2_PLACEMENT_3D('',#72187,#43789,#43790);
#35370=AXIS2_PLACEMENT_3D('',#72188,#43791,#43792);
#35371=AXIS2_PLACEMENT_3D('',#72190,#43793,#43794);
#35372=AXIS2_PLACEMENT_3D('',#72191,#43795,#43796);
#35373=AXIS2_PLACEMENT_3D('',#72192,#43797,#43798);
#35374=AXIS2_PLACEMENT_3D('',#72194,#43799,#43800);
#35375=AXIS2_PLACEMENT_3D('',#72196,#43802,#43803);
#35376=AXIS2_PLACEMENT_3D('',#72198,#43804,#43805);
#35377=AXIS2_PLACEMENT_3D('',#72199,#43806,#43807);
#35378=AXIS2_PLACEMENT_3D('',#72200,#43808,#43809);
#35379=AXIS2_PLACEMENT_3D('',#72202,#43810,#43811);
#35380=AXIS2_PLACEMENT_3D('',#72203,#43812,#43813);
#35381=AXIS2_PLACEMENT_3D('',#72204,#43814,#43815);
#35382=AXIS2_PLACEMENT_3D('',#72206,#43816,#43817);
#35383=AXIS2_PLACEMENT_3D('',#72208,#43818,#43819);
#35384=AXIS2_PLACEMENT_3D('',#72209,#43820,#43821);
#35385=AXIS2_PLACEMENT_3D('',#72210,#43822,#43823);
#35386=AXIS2_PLACEMENT_3D('',#72212,#43824,#43825);
#35387=AXIS2_PLACEMENT_3D('',#72214,#43826,#43827);
#35388=AXIS2_PLACEMENT_3D('',#72215,#43828,#43829);
#35389=AXIS2_PLACEMENT_3D('',#72216,#43830,#43831);
#35390=AXIS2_PLACEMENT_3D('',#72218,#43832,#43833);
#35391=AXIS2_PLACEMENT_3D('',#72220,#43834,#43835);
#35392=AXIS2_PLACEMENT_3D('',#72221,#43836,#43837);
#35393=AXIS2_PLACEMENT_3D('',#72222,#43838,#43839);
#35394=AXIS2_PLACEMENT_3D('',#72224,#43840,#43841);
#35395=AXIS2_PLACEMENT_3D('',#72226,#43842,#43843);
#35396=AXIS2_PLACEMENT_3D('',#72227,#43844,#43845);
#35397=AXIS2_PLACEMENT_3D('',#72228,#43846,#43847);
#35398=AXIS2_PLACEMENT_3D('',#72230,#43848,#43849);
#35399=AXIS2_PLACEMENT_3D('',#72232,#43850,#43851);
#35400=AXIS2_PLACEMENT_3D('',#72233,#43852,#43853);
#35401=AXIS2_PLACEMENT_3D('',#72234,#43854,#43855);
#35402=AXIS2_PLACEMENT_3D('',#72236,#43856,#43857);
#35403=AXIS2_PLACEMENT_3D('',#72238,#43858,#43859);
#35404=AXIS2_PLACEMENT_3D('',#72239,#43860,#43861);
#35405=AXIS2_PLACEMENT_3D('',#72240,#43862,#43863);
#35406=AXIS2_PLACEMENT_3D('',#72242,#43864,#43865);
#35407=AXIS2_PLACEMENT_3D('',#72244,#43866,#43867);
#35408=AXIS2_PLACEMENT_3D('',#72245,#43868,#43869);
#35409=AXIS2_PLACEMENT_3D('',#72246,#43870,#43871);
#35410=AXIS2_PLACEMENT_3D('',#72248,#43872,#43873);
#35411=AXIS2_PLACEMENT_3D('',#72250,#43874,#43875);
#35412=AXIS2_PLACEMENT_3D('',#72251,#43876,#43877);
#35413=AXIS2_PLACEMENT_3D('',#72252,#43878,#43879);
#35414=AXIS2_PLACEMENT_3D('',#72254,#43880,#43881);
#35415=AXIS2_PLACEMENT_3D('',#72256,#43882,#43883);
#35416=AXIS2_PLACEMENT_3D('',#72257,#43884,#43885);
#35417=AXIS2_PLACEMENT_3D('',#72258,#43886,#43887);
#35418=AXIS2_PLACEMENT_3D('',#72260,#43888,#43889);
#35419=AXIS2_PLACEMENT_3D('',#72262,#43890,#43891);
#35420=AXIS2_PLACEMENT_3D('',#72263,#43892,#43893);
#35421=AXIS2_PLACEMENT_3D('',#72264,#43894,#43895);
#35422=AXIS2_PLACEMENT_3D('',#72266,#43896,#43897);
#35423=AXIS2_PLACEMENT_3D('',#72268,#43898,#43899);
#35424=AXIS2_PLACEMENT_3D('',#72269,#43900,#43901);
#35425=AXIS2_PLACEMENT_3D('',#72270,#43902,#43903);
#35426=AXIS2_PLACEMENT_3D('',#72272,#43904,#43905);
#35427=AXIS2_PLACEMENT_3D('',#72274,#43906,#43907);
#35428=AXIS2_PLACEMENT_3D('',#72275,#43908,#43909);
#35429=AXIS2_PLACEMENT_3D('',#72276,#43910,#43911);
#35430=AXIS2_PLACEMENT_3D('',#72278,#43912,#43913);
#35431=AXIS2_PLACEMENT_3D('',#72280,#43914,#43915);
#35432=AXIS2_PLACEMENT_3D('',#72281,#43916,#43917);
#35433=AXIS2_PLACEMENT_3D('',#72282,#43918,#43919);
#35434=AXIS2_PLACEMENT_3D('',#72284,#43920,#43921);
#35435=AXIS2_PLACEMENT_3D('',#72286,#43922,#43923);
#35436=AXIS2_PLACEMENT_3D('',#72287,#43924,#43925);
#35437=AXIS2_PLACEMENT_3D('',#72288,#43926,#43927);
#35438=AXIS2_PLACEMENT_3D('',#72290,#43928,#43929);
#35439=AXIS2_PLACEMENT_3D('',#72292,#43930,#43931);
#35440=AXIS2_PLACEMENT_3D('',#72293,#43932,#43933);
#35441=AXIS2_PLACEMENT_3D('',#72294,#43934,#43935);
#35442=AXIS2_PLACEMENT_3D('',#72296,#43936,#43937);
#35443=AXIS2_PLACEMENT_3D('',#72298,#43938,#43939);
#35444=AXIS2_PLACEMENT_3D('',#72299,#43940,#43941);
#35445=AXIS2_PLACEMENT_3D('',#72300,#43942,#43943);
#35446=AXIS2_PLACEMENT_3D('',#72302,#43944,#43945);
#35447=AXIS2_PLACEMENT_3D('',#72304,#43946,#43947);
#35448=AXIS2_PLACEMENT_3D('',#72305,#43948,#43949);
#35449=AXIS2_PLACEMENT_3D('',#72306,#43950,#43951);
#35450=AXIS2_PLACEMENT_3D('',#72308,#43952,#43953);
#35451=AXIS2_PLACEMENT_3D('',#72310,#43954,#43955);
#35452=AXIS2_PLACEMENT_3D('',#72311,#43956,#43957);
#35453=AXIS2_PLACEMENT_3D('',#72312,#43958,#43959);
#35454=AXIS2_PLACEMENT_3D('',#72314,#43960,#43961);
#35455=AXIS2_PLACEMENT_3D('',#72316,#43962,#43963);
#35456=AXIS2_PLACEMENT_3D('',#72317,#43964,#43965);
#35457=AXIS2_PLACEMENT_3D('',#72318,#43966,#43967);
#35458=AXIS2_PLACEMENT_3D('',#72320,#43968,#43969);
#35459=AXIS2_PLACEMENT_3D('',#72322,#43970,#43971);
#35460=AXIS2_PLACEMENT_3D('',#72323,#43972,#43973);
#35461=AXIS2_PLACEMENT_3D('',#72324,#43974,#43975);
#35462=AXIS2_PLACEMENT_3D('',#72326,#43976,#43977);
#35463=AXIS2_PLACEMENT_3D('',#72328,#43978,#43979);
#35464=AXIS2_PLACEMENT_3D('',#72329,#43980,#43981);
#35465=AXIS2_PLACEMENT_3D('',#72330,#43982,#43983);
#35466=AXIS2_PLACEMENT_3D('',#72332,#43984,#43985);
#35467=AXIS2_PLACEMENT_3D('',#72334,#43986,#43987);
#35468=AXIS2_PLACEMENT_3D('',#72335,#43988,#43989);
#35469=AXIS2_PLACEMENT_3D('',#72336,#43990,#43991);
#35470=AXIS2_PLACEMENT_3D('',#72338,#43992,#43993);
#35471=AXIS2_PLACEMENT_3D('',#72340,#43994,#43995);
#35472=AXIS2_PLACEMENT_3D('',#72341,#43996,#43997);
#35473=AXIS2_PLACEMENT_3D('',#72342,#43998,#43999);
#35474=AXIS2_PLACEMENT_3D('',#72344,#44000,#44001);
#35475=AXIS2_PLACEMENT_3D('',#72346,#44002,#44003);
#35476=AXIS2_PLACEMENT_3D('',#72347,#44004,#44005);
#35477=AXIS2_PLACEMENT_3D('',#72348,#44006,#44007);
#35478=AXIS2_PLACEMENT_3D('',#72350,#44008,#44009);
#35479=AXIS2_PLACEMENT_3D('',#72352,#44010,#44011);
#35480=AXIS2_PLACEMENT_3D('',#72353,#44012,#44013);
#35481=AXIS2_PLACEMENT_3D('',#72354,#44014,#44015);
#35482=AXIS2_PLACEMENT_3D('',#72356,#44016,#44017);
#35483=AXIS2_PLACEMENT_3D('',#72358,#44018,#44019);
#35484=AXIS2_PLACEMENT_3D('',#72359,#44020,#44021);
#35485=AXIS2_PLACEMENT_3D('',#72360,#44022,#44023);
#35486=AXIS2_PLACEMENT_3D('',#72362,#44024,#44025);
#35487=AXIS2_PLACEMENT_3D('',#72364,#44026,#44027);
#35488=AXIS2_PLACEMENT_3D('',#72365,#44028,#44029);
#35489=AXIS2_PLACEMENT_3D('',#72366,#44030,#44031);
#35490=AXIS2_PLACEMENT_3D('',#72368,#44032,#44033);
#35491=AXIS2_PLACEMENT_3D('',#72370,#44034,#44035);
#35492=AXIS2_PLACEMENT_3D('',#72371,#44036,#44037);
#35493=AXIS2_PLACEMENT_3D('',#72372,#44038,#44039);
#35494=AXIS2_PLACEMENT_3D('',#72374,#44040,#44041);
#35495=AXIS2_PLACEMENT_3D('',#72376,#44042,#44043);
#35496=AXIS2_PLACEMENT_3D('',#72377,#44044,#44045);
#35497=AXIS2_PLACEMENT_3D('',#72378,#44046,#44047);
#35498=AXIS2_PLACEMENT_3D('',#72380,#44048,#44049);
#35499=AXIS2_PLACEMENT_3D('',#72382,#44050,#44051);
#35500=AXIS2_PLACEMENT_3D('',#72383,#44052,#44053);
#35501=AXIS2_PLACEMENT_3D('',#72384,#44054,#44055);
#35502=AXIS2_PLACEMENT_3D('',#72386,#44056,#44057);
#35503=AXIS2_PLACEMENT_3D('',#72388,#44058,#44059);
#35504=AXIS2_PLACEMENT_3D('',#72389,#44060,#44061);
#35505=AXIS2_PLACEMENT_3D('',#72390,#44062,#44063);
#35506=AXIS2_PLACEMENT_3D('',#72392,#44064,#44065);
#35507=AXIS2_PLACEMENT_3D('',#72394,#44066,#44067);
#35508=AXIS2_PLACEMENT_3D('',#72395,#44068,#44069);
#35509=AXIS2_PLACEMENT_3D('',#72396,#44070,#44071);
#35510=AXIS2_PLACEMENT_3D('',#72398,#44072,#44073);
#35511=AXIS2_PLACEMENT_3D('',#72400,#44074,#44075);
#35512=AXIS2_PLACEMENT_3D('',#72401,#44076,#44077);
#35513=AXIS2_PLACEMENT_3D('',#72402,#44078,#44079);
#35514=AXIS2_PLACEMENT_3D('',#72404,#44080,#44081);
#35515=AXIS2_PLACEMENT_3D('',#72406,#44082,#44083);
#35516=AXIS2_PLACEMENT_3D('',#72407,#44084,#44085);
#35517=AXIS2_PLACEMENT_3D('',#72408,#44086,#44087);
#35518=AXIS2_PLACEMENT_3D('',#72410,#44088,#44089);
#35519=AXIS2_PLACEMENT_3D('',#72412,#44090,#44091);
#35520=AXIS2_PLACEMENT_3D('',#72413,#44092,#44093);
#35521=AXIS2_PLACEMENT_3D('',#72414,#44094,#44095);
#35522=AXIS2_PLACEMENT_3D('',#72416,#44096,#44097);
#35523=AXIS2_PLACEMENT_3D('',#72418,#44098,#44099);
#35524=AXIS2_PLACEMENT_3D('',#72419,#44100,#44101);
#35525=AXIS2_PLACEMENT_3D('',#72420,#44102,#44103);
#35526=AXIS2_PLACEMENT_3D('',#72422,#44104,#44105);
#35527=AXIS2_PLACEMENT_3D('',#72424,#44106,#44107);
#35528=AXIS2_PLACEMENT_3D('',#72425,#44108,#44109);
#35529=AXIS2_PLACEMENT_3D('',#72426,#44110,#44111);
#35530=AXIS2_PLACEMENT_3D('',#72428,#44112,#44113);
#35531=AXIS2_PLACEMENT_3D('',#72430,#44114,#44115);
#35532=AXIS2_PLACEMENT_3D('',#72431,#44116,#44117);
#35533=AXIS2_PLACEMENT_3D('',#72432,#44118,#44119);
#35534=AXIS2_PLACEMENT_3D('',#72434,#44120,#44121);
#35535=AXIS2_PLACEMENT_3D('',#72436,#44122,#44123);
#35536=AXIS2_PLACEMENT_3D('',#72437,#44124,#44125);
#35537=AXIS2_PLACEMENT_3D('',#72438,#44126,#44127);
#35538=AXIS2_PLACEMENT_3D('',#72440,#44128,#44129);
#35539=AXIS2_PLACEMENT_3D('',#72442,#44130,#44131);
#35540=AXIS2_PLACEMENT_3D('',#72443,#44132,#44133);
#35541=AXIS2_PLACEMENT_3D('',#72444,#44134,#44135);
#35542=AXIS2_PLACEMENT_3D('',#72446,#44136,#44137);
#35543=AXIS2_PLACEMENT_3D('',#72448,#44138,#44139);
#35544=AXIS2_PLACEMENT_3D('',#72449,#44140,#44141);
#35545=AXIS2_PLACEMENT_3D('',#72450,#44142,#44143);
#35546=AXIS2_PLACEMENT_3D('',#72452,#44144,#44145);
#35547=AXIS2_PLACEMENT_3D('',#72454,#44146,#44147);
#35548=AXIS2_PLACEMENT_3D('',#72455,#44148,#44149);
#35549=AXIS2_PLACEMENT_3D('',#72456,#44150,#44151);
#35550=AXIS2_PLACEMENT_3D('',#72458,#44152,#44153);
#35551=AXIS2_PLACEMENT_3D('',#72460,#44154,#44155);
#35552=AXIS2_PLACEMENT_3D('',#72461,#44156,#44157);
#35553=AXIS2_PLACEMENT_3D('',#72462,#44158,#44159);
#35554=AXIS2_PLACEMENT_3D('',#72464,#44160,#44161);
#35555=AXIS2_PLACEMENT_3D('',#72466,#44162,#44163);
#35556=AXIS2_PLACEMENT_3D('',#72467,#44164,#44165);
#35557=AXIS2_PLACEMENT_3D('',#72468,#44166,#44167);
#35558=AXIS2_PLACEMENT_3D('',#72470,#44168,#44169);
#35559=AXIS2_PLACEMENT_3D('',#72472,#44170,#44171);
#35560=AXIS2_PLACEMENT_3D('',#72473,#44172,#44173);
#35561=AXIS2_PLACEMENT_3D('',#72474,#44174,#44175);
#35562=AXIS2_PLACEMENT_3D('',#72476,#44176,#44177);
#35563=AXIS2_PLACEMENT_3D('',#72478,#44178,#44179);
#35564=AXIS2_PLACEMENT_3D('',#72479,#44180,#44181);
#35565=AXIS2_PLACEMENT_3D('',#72480,#44182,#44183);
#35566=AXIS2_PLACEMENT_3D('',#72482,#44184,#44185);
#35567=AXIS2_PLACEMENT_3D('',#72484,#44186,#44187);
#35568=AXIS2_PLACEMENT_3D('',#72485,#44188,#44189);
#35569=AXIS2_PLACEMENT_3D('',#72486,#44190,#44191);
#35570=AXIS2_PLACEMENT_3D('',#72488,#44192,#44193);
#35571=AXIS2_PLACEMENT_3D('',#72490,#44194,#44195);
#35572=AXIS2_PLACEMENT_3D('',#72491,#44196,#44197);
#35573=AXIS2_PLACEMENT_3D('',#72492,#44198,#44199);
#35574=AXIS2_PLACEMENT_3D('',#72494,#44200,#44201);
#35575=AXIS2_PLACEMENT_3D('',#72496,#44202,#44203);
#35576=AXIS2_PLACEMENT_3D('',#72497,#44204,#44205);
#35577=AXIS2_PLACEMENT_3D('',#72498,#44206,#44207);
#35578=AXIS2_PLACEMENT_3D('',#72500,#44208,#44209);
#35579=AXIS2_PLACEMENT_3D('',#72502,#44210,#44211);
#35580=AXIS2_PLACEMENT_3D('',#72503,#44212,#44213);
#35581=AXIS2_PLACEMENT_3D('',#72504,#44214,#44215);
#35582=AXIS2_PLACEMENT_3D('',#72506,#44216,#44217);
#35583=AXIS2_PLACEMENT_3D('',#72508,#44218,#44219);
#35584=AXIS2_PLACEMENT_3D('',#72509,#44220,#44221);
#35585=AXIS2_PLACEMENT_3D('',#72510,#44222,#44223);
#35586=AXIS2_PLACEMENT_3D('',#72512,#44224,#44225);
#35587=AXIS2_PLACEMENT_3D('',#72514,#44226,#44227);
#35588=AXIS2_PLACEMENT_3D('',#72515,#44228,#44229);
#35589=AXIS2_PLACEMENT_3D('',#72516,#44230,#44231);
#35590=AXIS2_PLACEMENT_3D('',#72518,#44232,#44233);
#35591=AXIS2_PLACEMENT_3D('',#72520,#44234,#44235);
#35592=AXIS2_PLACEMENT_3D('',#72521,#44236,#44237);
#35593=AXIS2_PLACEMENT_3D('',#72522,#44238,#44239);
#35594=AXIS2_PLACEMENT_3D('',#72524,#44240,#44241);
#35595=AXIS2_PLACEMENT_3D('',#72526,#44242,#44243);
#35596=AXIS2_PLACEMENT_3D('',#72527,#44244,#44245);
#35597=AXIS2_PLACEMENT_3D('',#72528,#44246,#44247);
#35598=AXIS2_PLACEMENT_3D('',#72530,#44248,#44249);
#35599=AXIS2_PLACEMENT_3D('',#72532,#44250,#44251);
#35600=AXIS2_PLACEMENT_3D('',#72533,#44252,#44253);
#35601=AXIS2_PLACEMENT_3D('',#72534,#44254,#44255);
#35602=AXIS2_PLACEMENT_3D('',#72536,#44256,#44257);
#35603=AXIS2_PLACEMENT_3D('',#72538,#44258,#44259);
#35604=AXIS2_PLACEMENT_3D('',#72539,#44260,#44261);
#35605=AXIS2_PLACEMENT_3D('',#72540,#44262,#44263);
#35606=AXIS2_PLACEMENT_3D('',#72542,#44264,#44265);
#35607=AXIS2_PLACEMENT_3D('',#72544,#44266,#44267);
#35608=AXIS2_PLACEMENT_3D('',#72545,#44268,#44269);
#35609=AXIS2_PLACEMENT_3D('',#72546,#44270,#44271);
#35610=AXIS2_PLACEMENT_3D('',#72548,#44272,#44273);
#35611=AXIS2_PLACEMENT_3D('',#72550,#44274,#44275);
#35612=AXIS2_PLACEMENT_3D('',#72551,#44276,#44277);
#35613=AXIS2_PLACEMENT_3D('',#72552,#44278,#44279);
#35614=AXIS2_PLACEMENT_3D('',#72554,#44280,#44281);
#35615=AXIS2_PLACEMENT_3D('',#72556,#44282,#44283);
#35616=AXIS2_PLACEMENT_3D('',#72557,#44284,#44285);
#35617=AXIS2_PLACEMENT_3D('',#72558,#44286,#44287);
#35618=AXIS2_PLACEMENT_3D('',#72560,#44288,#44289);
#35619=AXIS2_PLACEMENT_3D('',#72562,#44290,#44291);
#35620=AXIS2_PLACEMENT_3D('',#72563,#44292,#44293);
#35621=AXIS2_PLACEMENT_3D('',#72564,#44294,#44295);
#35622=AXIS2_PLACEMENT_3D('',#72566,#44296,#44297);
#35623=AXIS2_PLACEMENT_3D('',#72568,#44298,#44299);
#35624=AXIS2_PLACEMENT_3D('',#72569,#44300,#44301);
#35625=AXIS2_PLACEMENT_3D('',#72570,#44302,#44303);
#35626=AXIS2_PLACEMENT_3D('',#72572,#44304,#44305);
#35627=AXIS2_PLACEMENT_3D('',#72574,#44306,#44307);
#35628=AXIS2_PLACEMENT_3D('',#72575,#44308,#44309);
#35629=AXIS2_PLACEMENT_3D('',#72576,#44310,#44311);
#35630=AXIS2_PLACEMENT_3D('',#72578,#44312,#44313);
#35631=AXIS2_PLACEMENT_3D('',#72580,#44314,#44315);
#35632=AXIS2_PLACEMENT_3D('',#72581,#44316,#44317);
#35633=AXIS2_PLACEMENT_3D('',#72582,#44318,#44319);
#35634=AXIS2_PLACEMENT_3D('',#72584,#44320,#44321);
#35635=AXIS2_PLACEMENT_3D('',#72586,#44322,#44323);
#35636=AXIS2_PLACEMENT_3D('',#72587,#44324,#44325);
#35637=AXIS2_PLACEMENT_3D('',#72588,#44326,#44327);
#35638=AXIS2_PLACEMENT_3D('',#72590,#44328,#44329);
#35639=AXIS2_PLACEMENT_3D('',#72592,#44330,#44331);
#35640=AXIS2_PLACEMENT_3D('',#72593,#44332,#44333);
#35641=AXIS2_PLACEMENT_3D('',#72594,#44334,#44335);
#35642=AXIS2_PLACEMENT_3D('',#72596,#44336,#44337);
#35643=AXIS2_PLACEMENT_3D('',#72598,#44338,#44339);
#35644=AXIS2_PLACEMENT_3D('',#72599,#44340,#44341);
#35645=AXIS2_PLACEMENT_3D('',#72600,#44342,#44343);
#35646=AXIS2_PLACEMENT_3D('',#72602,#44344,#44345);
#35647=AXIS2_PLACEMENT_3D('',#72604,#44346,#44347);
#35648=AXIS2_PLACEMENT_3D('',#72605,#44348,#44349);
#35649=AXIS2_PLACEMENT_3D('',#72606,#44350,#44351);
#35650=AXIS2_PLACEMENT_3D('',#72608,#44352,#44353);
#35651=AXIS2_PLACEMENT_3D('',#72610,#44354,#44355);
#35652=AXIS2_PLACEMENT_3D('',#72611,#44356,#44357);
#35653=AXIS2_PLACEMENT_3D('',#72612,#44358,#44359);
#35654=AXIS2_PLACEMENT_3D('',#72614,#44360,#44361);
#35655=AXIS2_PLACEMENT_3D('',#72616,#44362,#44363);
#35656=AXIS2_PLACEMENT_3D('',#72617,#44364,#44365);
#35657=AXIS2_PLACEMENT_3D('',#72618,#44366,#44367);
#35658=AXIS2_PLACEMENT_3D('',#72620,#44368,#44369);
#35659=AXIS2_PLACEMENT_3D('',#72622,#44370,#44371);
#35660=AXIS2_PLACEMENT_3D('',#72623,#44372,#44373);
#35661=AXIS2_PLACEMENT_3D('',#72624,#44374,#44375);
#35662=AXIS2_PLACEMENT_3D('',#72626,#44376,#44377);
#35663=AXIS2_PLACEMENT_3D('',#72628,#44378,#44379);
#35664=AXIS2_PLACEMENT_3D('',#72629,#44380,#44381);
#35665=AXIS2_PLACEMENT_3D('',#72630,#44382,#44383);
#35666=AXIS2_PLACEMENT_3D('',#72632,#44384,#44385);
#35667=AXIS2_PLACEMENT_3D('',#72634,#44386,#44387);
#35668=AXIS2_PLACEMENT_3D('',#72635,#44388,#44389);
#35669=AXIS2_PLACEMENT_3D('',#72636,#44390,#44391);
#35670=AXIS2_PLACEMENT_3D('',#72638,#44392,#44393);
#35671=AXIS2_PLACEMENT_3D('',#72640,#44394,#44395);
#35672=AXIS2_PLACEMENT_3D('',#72641,#44396,#44397);
#35673=AXIS2_PLACEMENT_3D('',#72642,#44398,#44399);
#35674=AXIS2_PLACEMENT_3D('',#72644,#44400,#44401);
#35675=AXIS2_PLACEMENT_3D('',#72646,#44402,#44403);
#35676=AXIS2_PLACEMENT_3D('',#72647,#44404,#44405);
#35677=AXIS2_PLACEMENT_3D('',#72648,#44406,#44407);
#35678=AXIS2_PLACEMENT_3D('',#72650,#44408,#44409);
#35679=AXIS2_PLACEMENT_3D('',#72652,#44410,#44411);
#35680=AXIS2_PLACEMENT_3D('',#72653,#44412,#44413);
#35681=AXIS2_PLACEMENT_3D('',#72654,#44414,#44415);
#35682=AXIS2_PLACEMENT_3D('',#72656,#44416,#44417);
#35683=AXIS2_PLACEMENT_3D('',#72658,#44418,#44419);
#35684=AXIS2_PLACEMENT_3D('',#72659,#44420,#44421);
#35685=AXIS2_PLACEMENT_3D('',#72660,#44422,#44423);
#35686=AXIS2_PLACEMENT_3D('',#72662,#44424,#44425);
#35687=AXIS2_PLACEMENT_3D('',#72664,#44426,#44427);
#35688=AXIS2_PLACEMENT_3D('',#72665,#44428,#44429);
#35689=AXIS2_PLACEMENT_3D('',#72666,#44430,#44431);
#35690=AXIS2_PLACEMENT_3D('',#72668,#44432,#44433);
#35691=AXIS2_PLACEMENT_3D('',#72670,#44434,#44435);
#35692=AXIS2_PLACEMENT_3D('',#72671,#44436,#44437);
#35693=AXIS2_PLACEMENT_3D('',#72672,#44438,#44439);
#35694=AXIS2_PLACEMENT_3D('',#72674,#44440,#44441);
#35695=AXIS2_PLACEMENT_3D('',#72676,#44442,#44443);
#35696=AXIS2_PLACEMENT_3D('',#72677,#44444,#44445);
#35697=AXIS2_PLACEMENT_3D('',#72678,#44446,#44447);
#35698=AXIS2_PLACEMENT_3D('',#72682,#44449,#44450);
#35699=AXIS2_PLACEMENT_3D('',#72684,#44452,#44453);
#35700=AXIS2_PLACEMENT_3D('',#72689,#44456,#44457);
#35701=AXIS2_PLACEMENT_3D('',#72690,#44458,#44459);
#35702=AXIS2_PLACEMENT_3D('',#72695,#44462,#44463);
#35703=AXIS2_PLACEMENT_3D('',#72696,#44464,#44465);
#35704=AXIS2_PLACEMENT_3D('',#72701,#44468,#44469);
#35705=AXIS2_PLACEMENT_3D('',#72702,#44470,#44471);
#35706=AXIS2_PLACEMENT_3D('',#72707,#44474,#44475);
#35707=AXIS2_PLACEMENT_3D('',#72708,#44476,#44477);
#35708=AXIS2_PLACEMENT_3D('',#72713,#44480,#44481);
#35709=AXIS2_PLACEMENT_3D('',#72714,#44482,#44483);
#35710=AXIS2_PLACEMENT_3D('',#72719,#44486,#44487);
#35711=AXIS2_PLACEMENT_3D('',#72720,#44488,#44489);
#35712=AXIS2_PLACEMENT_3D('',#72725,#44492,#44493);
#35713=AXIS2_PLACEMENT_3D('',#72726,#44494,#44495);
#35714=AXIS2_PLACEMENT_3D('',#72731,#44498,#44499);
#35715=AXIS2_PLACEMENT_3D('',#72732,#44500,#44501);
#35716=AXIS2_PLACEMENT_3D('',#72737,#44504,#44505);
#35717=AXIS2_PLACEMENT_3D('',#72738,#44506,#44507);
#35718=AXIS2_PLACEMENT_3D('',#72743,#44510,#44511);
#35719=AXIS2_PLACEMENT_3D('',#72744,#44512,#44513);
#35720=AXIS2_PLACEMENT_3D('',#72749,#44516,#44517);
#35721=AXIS2_PLACEMENT_3D('',#72750,#44518,#44519);
#35722=AXIS2_PLACEMENT_3D('',#72755,#44522,#44523);
#35723=AXIS2_PLACEMENT_3D('',#72756,#44524,#44525);
#35724=AXIS2_PLACEMENT_3D('',#72761,#44528,#44529);
#35725=AXIS2_PLACEMENT_3D('',#72762,#44530,#44531);
#35726=AXIS2_PLACEMENT_3D('',#72767,#44534,#44535);
#35727=AXIS2_PLACEMENT_3D('',#72768,#44536,#44537);
#35728=AXIS2_PLACEMENT_3D('',#72773,#44540,#44541);
#35729=AXIS2_PLACEMENT_3D('',#72774,#44542,#44543);
#35730=AXIS2_PLACEMENT_3D('',#72779,#44546,#44547);
#35731=AXIS2_PLACEMENT_3D('',#72780,#44548,#44549);
#35732=AXIS2_PLACEMENT_3D('',#72785,#44552,#44553);
#35733=AXIS2_PLACEMENT_3D('',#72786,#44554,#44555);
#35734=AXIS2_PLACEMENT_3D('',#72791,#44558,#44559);
#35735=AXIS2_PLACEMENT_3D('',#72792,#44560,#44561);
#35736=AXIS2_PLACEMENT_3D('',#72797,#44564,#44565);
#35737=AXIS2_PLACEMENT_3D('',#72798,#44566,#44567);
#35738=AXIS2_PLACEMENT_3D('',#72803,#44570,#44571);
#35739=AXIS2_PLACEMENT_3D('',#72804,#44572,#44573);
#35740=AXIS2_PLACEMENT_3D('',#72809,#44576,#44577);
#35741=AXIS2_PLACEMENT_3D('',#72810,#44578,#44579);
#35742=AXIS2_PLACEMENT_3D('',#72815,#44582,#44583);
#35743=AXIS2_PLACEMENT_3D('',#72816,#44584,#44585);
#35744=AXIS2_PLACEMENT_3D('',#72821,#44588,#44589);
#35745=AXIS2_PLACEMENT_3D('',#72822,#44590,#44591);
#35746=AXIS2_PLACEMENT_3D('',#72827,#44594,#44595);
#35747=AXIS2_PLACEMENT_3D('',#72828,#44596,#44597);
#35748=AXIS2_PLACEMENT_3D('',#72833,#44600,#44601);
#35749=AXIS2_PLACEMENT_3D('',#72834,#44602,#44603);
#35750=AXIS2_PLACEMENT_3D('',#72839,#44606,#44607);
#35751=AXIS2_PLACEMENT_3D('',#72840,#44608,#44609);
#35752=AXIS2_PLACEMENT_3D('',#72845,#44612,#44613);
#35753=AXIS2_PLACEMENT_3D('',#72846,#44614,#44615);
#35754=AXIS2_PLACEMENT_3D('',#72851,#44618,#44619);
#35755=AXIS2_PLACEMENT_3D('',#72852,#44620,#44621);
#35756=AXIS2_PLACEMENT_3D('',#72857,#44624,#44625);
#35757=AXIS2_PLACEMENT_3D('',#72858,#44626,#44627);
#35758=AXIS2_PLACEMENT_3D('',#72863,#44630,#44631);
#35759=AXIS2_PLACEMENT_3D('',#72864,#44632,#44633);
#35760=AXIS2_PLACEMENT_3D('',#72869,#44636,#44637);
#35761=AXIS2_PLACEMENT_3D('',#72870,#44638,#44639);
#35762=AXIS2_PLACEMENT_3D('',#72875,#44642,#44643);
#35763=AXIS2_PLACEMENT_3D('',#72876,#44644,#44645);
#35764=AXIS2_PLACEMENT_3D('',#72881,#44648,#44649);
#35765=AXIS2_PLACEMENT_3D('',#72882,#44650,#44651);
#35766=AXIS2_PLACEMENT_3D('',#72887,#44654,#44655);
#35767=AXIS2_PLACEMENT_3D('',#72888,#44656,#44657);
#35768=AXIS2_PLACEMENT_3D('',#72893,#44660,#44661);
#35769=AXIS2_PLACEMENT_3D('',#72894,#44662,#44663);
#35770=AXIS2_PLACEMENT_3D('',#72899,#44666,#44667);
#35771=AXIS2_PLACEMENT_3D('',#72900,#44668,#44669);
#35772=AXIS2_PLACEMENT_3D('',#72905,#44672,#44673);
#35773=AXIS2_PLACEMENT_3D('',#72906,#44674,#44675);
#35774=AXIS2_PLACEMENT_3D('',#72911,#44678,#44679);
#35775=AXIS2_PLACEMENT_3D('',#72912,#44680,#44681);
#35776=AXIS2_PLACEMENT_3D('',#72917,#44684,#44685);
#35777=AXIS2_PLACEMENT_3D('',#72918,#44686,#44687);
#35778=AXIS2_PLACEMENT_3D('',#72923,#44690,#44691);
#35779=AXIS2_PLACEMENT_3D('',#72924,#44692,#44693);
#35780=AXIS2_PLACEMENT_3D('',#72929,#44696,#44697);
#35781=AXIS2_PLACEMENT_3D('',#72930,#44698,#44699);
#35782=AXIS2_PLACEMENT_3D('',#72935,#44702,#44703);
#35783=AXIS2_PLACEMENT_3D('',#72936,#44704,#44705);
#35784=AXIS2_PLACEMENT_3D('',#72941,#44708,#44709);
#35785=AXIS2_PLACEMENT_3D('',#72942,#44710,#44711);
#35786=AXIS2_PLACEMENT_3D('',#72947,#44714,#44715);
#35787=AXIS2_PLACEMENT_3D('',#72948,#44716,#44717);
#35788=AXIS2_PLACEMENT_3D('',#72953,#44720,#44721);
#35789=AXIS2_PLACEMENT_3D('',#72954,#44722,#44723);
#35790=AXIS2_PLACEMENT_3D('',#72959,#44726,#44727);
#35791=AXIS2_PLACEMENT_3D('',#72960,#44728,#44729);
#35792=AXIS2_PLACEMENT_3D('',#72965,#44732,#44733);
#35793=AXIS2_PLACEMENT_3D('',#72966,#44734,#44735);
#35794=AXIS2_PLACEMENT_3D('',#72971,#44738,#44739);
#35795=AXIS2_PLACEMENT_3D('',#72972,#44740,#44741);
#35796=AXIS2_PLACEMENT_3D('',#72977,#44744,#44745);
#35797=AXIS2_PLACEMENT_3D('',#72978,#44746,#44747);
#35798=AXIS2_PLACEMENT_3D('',#72983,#44750,#44751);
#35799=AXIS2_PLACEMENT_3D('',#72984,#44752,#44753);
#35800=AXIS2_PLACEMENT_3D('',#72989,#44756,#44757);
#35801=AXIS2_PLACEMENT_3D('',#72990,#44758,#44759);
#35802=AXIS2_PLACEMENT_3D('',#72995,#44762,#44763);
#35803=AXIS2_PLACEMENT_3D('',#72996,#44764,#44765);
#35804=AXIS2_PLACEMENT_3D('',#73001,#44768,#44769);
#35805=AXIS2_PLACEMENT_3D('',#73002,#44770,#44771);
#35806=AXIS2_PLACEMENT_3D('',#73007,#44774,#44775);
#35807=AXIS2_PLACEMENT_3D('',#73008,#44776,#44777);
#35808=AXIS2_PLACEMENT_3D('',#73013,#44780,#44781);
#35809=AXIS2_PLACEMENT_3D('',#73014,#44782,#44783);
#35810=AXIS2_PLACEMENT_3D('',#73019,#44786,#44787);
#35811=AXIS2_PLACEMENT_3D('',#73020,#44788,#44789);
#35812=AXIS2_PLACEMENT_3D('',#73025,#44792,#44793);
#35813=AXIS2_PLACEMENT_3D('',#73026,#44794,#44795);
#35814=AXIS2_PLACEMENT_3D('',#73031,#44798,#44799);
#35815=AXIS2_PLACEMENT_3D('',#73032,#44800,#44801);
#35816=AXIS2_PLACEMENT_3D('',#73037,#44804,#44805);
#35817=AXIS2_PLACEMENT_3D('',#73038,#44806,#44807);
#35818=AXIS2_PLACEMENT_3D('',#73043,#44810,#44811);
#35819=AXIS2_PLACEMENT_3D('',#73044,#44812,#44813);
#35820=AXIS2_PLACEMENT_3D('',#73049,#44816,#44817);
#35821=AXIS2_PLACEMENT_3D('',#73050,#44818,#44819);
#35822=AXIS2_PLACEMENT_3D('',#73055,#44822,#44823);
#35823=AXIS2_PLACEMENT_3D('',#73056,#44824,#44825);
#35824=AXIS2_PLACEMENT_3D('',#73061,#44828,#44829);
#35825=AXIS2_PLACEMENT_3D('',#73062,#44830,#44831);
#35826=AXIS2_PLACEMENT_3D('',#73066,#44833,#44834);
#35827=AXIS2_PLACEMENT_3D('',#73068,#44836,#44837);
#35828=AXIS2_PLACEMENT_3D('',#73072,#44839,#44840);
#35829=AXIS2_PLACEMENT_3D('',#73074,#44842,#44843);
#35830=AXIS2_PLACEMENT_3D('',#73078,#44845,#44846);
#35831=AXIS2_PLACEMENT_3D('',#73080,#44848,#44849);
#35832=AXIS2_PLACEMENT_3D('',#73084,#44851,#44852);
#35833=AXIS2_PLACEMENT_3D('',#73086,#44854,#44855);
#35834=AXIS2_PLACEMENT_3D('',#73090,#44857,#44858);
#35835=AXIS2_PLACEMENT_3D('',#73092,#44860,#44861);
#35836=AXIS2_PLACEMENT_3D('',#73096,#44863,#44864);
#35837=AXIS2_PLACEMENT_3D('',#73098,#44866,#44867);
#35838=AXIS2_PLACEMENT_3D('',#73102,#44869,#44870);
#35839=AXIS2_PLACEMENT_3D('',#73104,#44872,#44873);
#35840=AXIS2_PLACEMENT_3D('',#73108,#44875,#44876);
#35841=AXIS2_PLACEMENT_3D('',#73110,#44878,#44879);
#35842=AXIS2_PLACEMENT_3D('',#73114,#44881,#44882);
#35843=AXIS2_PLACEMENT_3D('',#73116,#44884,#44885);
#35844=AXIS2_PLACEMENT_3D('',#73120,#44887,#44888);
#35845=AXIS2_PLACEMENT_3D('',#73122,#44890,#44891);
#35846=AXIS2_PLACEMENT_3D('',#73126,#44893,#44894);
#35847=AXIS2_PLACEMENT_3D('',#73128,#44896,#44897);
#35848=AXIS2_PLACEMENT_3D('',#73132,#44899,#44900);
#35849=AXIS2_PLACEMENT_3D('',#73134,#44902,#44903);
#35850=AXIS2_PLACEMENT_3D('',#73138,#44905,#44906);
#35851=AXIS2_PLACEMENT_3D('',#73140,#44908,#44909);
#35852=AXIS2_PLACEMENT_3D('',#73144,#44911,#44912);
#35853=AXIS2_PLACEMENT_3D('',#73146,#44914,#44915);
#35854=AXIS2_PLACEMENT_3D('',#73151,#44918,#44919);
#35855=AXIS2_PLACEMENT_3D('',#73152,#44920,#44921);
#35856=AXIS2_PLACEMENT_3D('',#73153,#44922,#44923);
#35857=AXIS2_PLACEMENT_3D('',#73154,#44924,#44925);
#35858=AXIS2_PLACEMENT_3D('',#73155,#44926,#44927);
#35859=AXIS2_PLACEMENT_3D('',#73156,#44928,#44929);
#35860=AXIS2_PLACEMENT_3D('',#73157,#44930,#44931);
#35861=AXIS2_PLACEMENT_3D('',#73158,#44932,#44933);
#35862=AXIS2_PLACEMENT_3D('',#73159,#44934,#44935);
#35863=AXIS2_PLACEMENT_3D('',#73160,#44936,#44937);
#35864=AXIS2_PLACEMENT_3D('',#73161,#44938,#44939);
#35865=AXIS2_PLACEMENT_3D('',#73162,#44940,#44941);
#35866=AXIS2_PLACEMENT_3D('',#73163,#44942,#44943);
#35867=AXIS2_PLACEMENT_3D('',#73164,#44944,#44945);
#35868=AXIS2_PLACEMENT_3D('',#73165,#44946,#44947);
#35869=AXIS2_PLACEMENT_3D('',#73166,#44948,#44949);
#35870=AXIS2_PLACEMENT_3D('',#73167,#44950,#44951);
#35871=AXIS2_PLACEMENT_3D('',#73168,#44952,#44953);
#35872=AXIS2_PLACEMENT_3D('',#73169,#44954,#44955);
#35873=AXIS2_PLACEMENT_3D('',#73170,#44956,#44957);
#35874=AXIS2_PLACEMENT_3D('',#73171,#44958,#44959);
#35875=AXIS2_PLACEMENT_3D('',#73172,#44960,#44961);
#35876=AXIS2_PLACEMENT_3D('',#73173,#44962,#44963);
#35877=AXIS2_PLACEMENT_3D('',#73174,#44964,#44965);
#35878=AXIS2_PLACEMENT_3D('',#73175,#44966,#44967);
#35879=AXIS2_PLACEMENT_3D('',#73176,#44968,#44969);
#35880=AXIS2_PLACEMENT_3D('',#73177,#44970,#44971);
#35881=AXIS2_PLACEMENT_3D('',#73178,#44972,#44973);
#35882=AXIS2_PLACEMENT_3D('',#73179,#44974,#44975);
#35883=AXIS2_PLACEMENT_3D('',#73180,#44976,#44977);
#35884=AXIS2_PLACEMENT_3D('',#73181,#44978,#44979);
#35885=AXIS2_PLACEMENT_3D('',#73182,#44980,#44981);
#35886=AXIS2_PLACEMENT_3D('',#73183,#44982,#44983);
#35887=AXIS2_PLACEMENT_3D('',#73184,#44984,#44985);
#35888=AXIS2_PLACEMENT_3D('',#73185,#44986,#44987);
#35889=AXIS2_PLACEMENT_3D('',#73186,#44988,#44989);
#35890=AXIS2_PLACEMENT_3D('',#73187,#44990,#44991);
#35891=AXIS2_PLACEMENT_3D('',#73188,#44992,#44993);
#35892=AXIS2_PLACEMENT_3D('',#73189,#44994,#44995);
#35893=AXIS2_PLACEMENT_3D('',#73190,#44996,#44997);
#35894=AXIS2_PLACEMENT_3D('',#73191,#44998,#44999);
#35895=AXIS2_PLACEMENT_3D('',#73192,#45000,#45001);
#35896=AXIS2_PLACEMENT_3D('',#73193,#45002,#45003);
#35897=AXIS2_PLACEMENT_3D('',#73194,#45004,#45005);
#35898=AXIS2_PLACEMENT_3D('',#73195,#45006,#45007);
#35899=AXIS2_PLACEMENT_3D('',#73196,#45008,#45009);
#35900=AXIS2_PLACEMENT_3D('',#73197,#45010,#45011);
#35901=AXIS2_PLACEMENT_3D('',#73198,#45012,#45013);
#35902=AXIS2_PLACEMENT_3D('',#73199,#45014,#45015);
#35903=AXIS2_PLACEMENT_3D('',#73200,#45016,#45017);
#35904=AXIS2_PLACEMENT_3D('',#73201,#45018,#45019);
#35905=AXIS2_PLACEMENT_3D('',#73202,#45020,#45021);
#35906=AXIS2_PLACEMENT_3D('',#73203,#45022,#45023);
#35907=AXIS2_PLACEMENT_3D('',#73204,#45024,#45025);
#35908=AXIS2_PLACEMENT_3D('',#73205,#45026,#45027);
#35909=AXIS2_PLACEMENT_3D('',#73206,#45028,#45029);
#35910=AXIS2_PLACEMENT_3D('',#73207,#45030,#45031);
#35911=AXIS2_PLACEMENT_3D('',#73208,#45032,#45033);
#35912=AXIS2_PLACEMENT_3D('',#73209,#45034,#45035);
#35913=AXIS2_PLACEMENT_3D('',#73210,#45036,#45037);
#35914=AXIS2_PLACEMENT_3D('',#73211,#45038,#45039);
#35915=AXIS2_PLACEMENT_3D('',#73212,#45040,#45041);
#35916=AXIS2_PLACEMENT_3D('',#73213,#45042,#45043);
#35917=AXIS2_PLACEMENT_3D('',#73214,#45044,#45045);
#35918=AXIS2_PLACEMENT_3D('',#73215,#45046,#45047);
#35919=AXIS2_PLACEMENT_3D('',#73216,#45048,#45049);
#35920=AXIS2_PLACEMENT_3D('',#73217,#45050,#45051);
#35921=AXIS2_PLACEMENT_3D('',#73218,#45052,#45053);
#35922=AXIS2_PLACEMENT_3D('',#73219,#45054,#45055);
#35923=AXIS2_PLACEMENT_3D('',#73220,#45056,#45057);
#35924=AXIS2_PLACEMENT_3D('',#73221,#45058,#45059);
#35925=AXIS2_PLACEMENT_3D('',#73222,#45060,#45061);
#35926=AXIS2_PLACEMENT_3D('',#73223,#45062,#45063);
#35927=AXIS2_PLACEMENT_3D('',#73224,#45064,#45065);
#35928=AXIS2_PLACEMENT_3D('',#73225,#45066,#45067);
#35929=AXIS2_PLACEMENT_3D('',#73226,#45068,#45069);
#35930=AXIS2_PLACEMENT_3D('',#73227,#45070,#45071);
#35931=AXIS2_PLACEMENT_3D('',#73228,#45072,#45073);
#35932=AXIS2_PLACEMENT_3D('',#73229,#45074,#45075);
#35933=AXIS2_PLACEMENT_3D('',#73230,#45076,#45077);
#35934=AXIS2_PLACEMENT_3D('',#73231,#45078,#45079);
#35935=AXIS2_PLACEMENT_3D('',#73232,#45080,#45081);
#35936=AXIS2_PLACEMENT_3D('',#73233,#45082,#45083);
#35937=AXIS2_PLACEMENT_3D('',#73234,#45084,#45085);
#35938=AXIS2_PLACEMENT_3D('',#73235,#45086,#45087);
#35939=AXIS2_PLACEMENT_3D('',#73236,#45088,#45089);
#35940=AXIS2_PLACEMENT_3D('',#73237,#45090,#45091);
#35941=AXIS2_PLACEMENT_3D('',#73238,#45092,#45093);
#35942=AXIS2_PLACEMENT_3D('',#73239,#45094,#45095);
#35943=AXIS2_PLACEMENT_3D('',#73240,#45096,#45097);
#35944=AXIS2_PLACEMENT_3D('',#73241,#45098,#45099);
#35945=AXIS2_PLACEMENT_3D('',#73242,#45100,#45101);
#35946=AXIS2_PLACEMENT_3D('',#73243,#45102,#45103);
#35947=AXIS2_PLACEMENT_3D('',#73244,#45104,#45105);
#35948=AXIS2_PLACEMENT_3D('',#73245,#45106,#45107);
#35949=AXIS2_PLACEMENT_3D('',#73246,#45108,#45109);
#35950=AXIS2_PLACEMENT_3D('',#73247,#45110,#45111);
#35951=AXIS2_PLACEMENT_3D('',#73248,#45112,#45113);
#35952=AXIS2_PLACEMENT_3D('',#73249,#45114,#45115);
#35953=AXIS2_PLACEMENT_3D('',#73250,#45116,#45117);
#35954=AXIS2_PLACEMENT_3D('',#73251,#45118,#45119);
#35955=AXIS2_PLACEMENT_3D('',#73252,#45120,#45121);
#35956=AXIS2_PLACEMENT_3D('',#73253,#45122,#45123);
#35957=AXIS2_PLACEMENT_3D('',#73254,#45124,#45125);
#35958=AXIS2_PLACEMENT_3D('',#73255,#45126,#45127);
#35959=AXIS2_PLACEMENT_3D('',#73256,#45128,#45129);
#35960=AXIS2_PLACEMENT_3D('',#73257,#45130,#45131);
#35961=AXIS2_PLACEMENT_3D('',#73258,#45132,#45133);
#35962=AXIS2_PLACEMENT_3D('',#73259,#45134,#45135);
#35963=AXIS2_PLACEMENT_3D('',#73260,#45136,#45137);
#35964=AXIS2_PLACEMENT_3D('',#73261,#45138,#45139);
#35965=AXIS2_PLACEMENT_3D('',#73262,#45140,#45141);
#35966=AXIS2_PLACEMENT_3D('',#73263,#45142,#45143);
#35967=AXIS2_PLACEMENT_3D('',#73264,#45144,#45145);
#35968=AXIS2_PLACEMENT_3D('',#73265,#45146,#45147);
#35969=AXIS2_PLACEMENT_3D('',#73266,#45148,#45149);
#35970=AXIS2_PLACEMENT_3D('',#73267,#45150,#45151);
#35971=AXIS2_PLACEMENT_3D('',#73268,#45152,#45153);
#35972=AXIS2_PLACEMENT_3D('',#73269,#45154,#45155);
#35973=AXIS2_PLACEMENT_3D('',#73270,#45156,#45157);
#35974=AXIS2_PLACEMENT_3D('',#73271,#45158,#45159);
#35975=AXIS2_PLACEMENT_3D('',#73272,#45160,#45161);
#35976=AXIS2_PLACEMENT_3D('',#73273,#45162,#45163);
#35977=AXIS2_PLACEMENT_3D('',#73274,#45164,#45165);
#35978=AXIS2_PLACEMENT_3D('',#73275,#45166,#45167);
#35979=AXIS2_PLACEMENT_3D('',#73276,#45168,#45169);
#35980=AXIS2_PLACEMENT_3D('',#73277,#45170,#45171);
#35981=AXIS2_PLACEMENT_3D('',#73278,#45172,#45173);
#35982=AXIS2_PLACEMENT_3D('',#73279,#45174,#45175);
#35983=AXIS2_PLACEMENT_3D('',#73280,#45176,#45177);
#35984=AXIS2_PLACEMENT_3D('',#73281,#45178,#45179);
#35985=AXIS2_PLACEMENT_3D('',#73282,#45180,#45181);
#35986=AXIS2_PLACEMENT_3D('',#73283,#45182,#45183);
#35987=AXIS2_PLACEMENT_3D('',#73284,#45184,#45185);
#35988=AXIS2_PLACEMENT_3D('',#73285,#45186,#45187);
#35989=AXIS2_PLACEMENT_3D('',#73286,#45188,#45189);
#35990=AXIS2_PLACEMENT_3D('',#73287,#45190,#45191);
#35991=AXIS2_PLACEMENT_3D('',#73288,#45192,#45193);
#35992=AXIS2_PLACEMENT_3D('',#73289,#45194,#45195);
#35993=AXIS2_PLACEMENT_3D('',#73290,#45196,#45197);
#35994=AXIS2_PLACEMENT_3D('',#73291,#45198,#45199);
#35995=AXIS2_PLACEMENT_3D('',#73292,#45200,#45201);
#35996=AXIS2_PLACEMENT_3D('',#73293,#45202,#45203);
#35997=AXIS2_PLACEMENT_3D('',#73294,#45204,#45205);
#35998=AXIS2_PLACEMENT_3D('',#73295,#45206,#45207);
#35999=AXIS2_PLACEMENT_3D('',#73296,#45208,#45209);
#36000=AXIS2_PLACEMENT_3D('',#73297,#45210,#45211);
#36001=AXIS2_PLACEMENT_3D('',#73298,#45212,#45213);
#36002=AXIS2_PLACEMENT_3D('',#73299,#45214,#45215);
#36003=AXIS2_PLACEMENT_3D('',#73300,#45216,#45217);
#36004=AXIS2_PLACEMENT_3D('',#73301,#45218,#45219);
#36005=AXIS2_PLACEMENT_3D('',#73302,#45220,#45221);
#36006=AXIS2_PLACEMENT_3D('',#73303,#45222,#45223);
#36007=AXIS2_PLACEMENT_3D('',#73304,#45224,#45225);
#36008=AXIS2_PLACEMENT_3D('',#73305,#45226,#45227);
#36009=AXIS2_PLACEMENT_3D('',#73306,#45228,#45229);
#36010=AXIS2_PLACEMENT_3D('',#73307,#45230,#45231);
#36011=AXIS2_PLACEMENT_3D('',#73308,#45232,#45233);
#36012=AXIS2_PLACEMENT_3D('',#73309,#45234,#45235);
#36013=AXIS2_PLACEMENT_3D('',#73310,#45236,#45237);
#36014=AXIS2_PLACEMENT_3D('',#73311,#45238,#45239);
#36015=AXIS2_PLACEMENT_3D('',#73312,#45240,#45241);
#36016=AXIS2_PLACEMENT_3D('',#73313,#45242,#45243);
#36017=AXIS2_PLACEMENT_3D('',#73314,#45244,#45245);
#36018=AXIS2_PLACEMENT_3D('',#73315,#45246,#45247);
#36019=AXIS2_PLACEMENT_3D('',#73316,#45248,#45249);
#36020=AXIS2_PLACEMENT_3D('',#73317,#45250,#45251);
#36021=AXIS2_PLACEMENT_3D('',#73318,#45252,#45253);
#36022=AXIS2_PLACEMENT_3D('',#73319,#45254,#45255);
#36023=AXIS2_PLACEMENT_3D('',#73320,#45256,#45257);
#36024=AXIS2_PLACEMENT_3D('',#73321,#45258,#45259);
#36025=AXIS2_PLACEMENT_3D('',#73322,#45260,#45261);
#36026=AXIS2_PLACEMENT_3D('',#73323,#45262,#45263);
#36027=AXIS2_PLACEMENT_3D('',#73324,#45264,#45265);
#36028=AXIS2_PLACEMENT_3D('',#73325,#45266,#45267);
#36029=AXIS2_PLACEMENT_3D('',#73326,#45268,#45269);
#36030=AXIS2_PLACEMENT_3D('',#73327,#45270,#45271);
#36031=AXIS2_PLACEMENT_3D('',#73328,#45272,#45273);
#36032=AXIS2_PLACEMENT_3D('',#73329,#45274,#45275);
#36033=AXIS2_PLACEMENT_3D('',#73330,#45276,#45277);
#36034=AXIS2_PLACEMENT_3D('',#73331,#45278,#45279);
#36035=AXIS2_PLACEMENT_3D('',#73332,#45280,#45281);
#36036=AXIS2_PLACEMENT_3D('',#73333,#45282,#45283);
#36037=AXIS2_PLACEMENT_3D('',#73334,#45284,#45285);
#36038=AXIS2_PLACEMENT_3D('',#73335,#45286,#45287);
#36039=AXIS2_PLACEMENT_3D('',#73336,#45288,#45289);
#36040=AXIS2_PLACEMENT_3D('',#73337,#45290,#45291);
#36041=AXIS2_PLACEMENT_3D('',#73338,#45292,#45293);
#36042=AXIS2_PLACEMENT_3D('',#73339,#45294,#45295);
#36043=AXIS2_PLACEMENT_3D('',#73340,#45296,#45297);
#36044=AXIS2_PLACEMENT_3D('',#73341,#45298,#45299);
#36045=AXIS2_PLACEMENT_3D('',#73342,#45300,#45301);
#36046=AXIS2_PLACEMENT_3D('',#73343,#45302,#45303);
#36047=AXIS2_PLACEMENT_3D('',#73344,#45304,#45305);
#36048=AXIS2_PLACEMENT_3D('',#73345,#45306,#45307);
#36049=AXIS2_PLACEMENT_3D('',#73346,#45308,#45309);
#36050=AXIS2_PLACEMENT_3D('',#73347,#45310,#45311);
#36051=AXIS2_PLACEMENT_3D('',#73348,#45312,#45313);
#36052=AXIS2_PLACEMENT_3D('',#73349,#45314,#45315);
#36053=AXIS2_PLACEMENT_3D('',#73350,#45316,#45317);
#36054=AXIS2_PLACEMENT_3D('',#73351,#45318,#45319);
#36055=AXIS2_PLACEMENT_3D('',#73352,#45320,#45321);
#36056=AXIS2_PLACEMENT_3D('',#73353,#45322,#45323);
#36057=AXIS2_PLACEMENT_3D('',#73354,#45324,#45325);
#36058=AXIS2_PLACEMENT_3D('',#73355,#45326,#45327);
#36059=AXIS2_PLACEMENT_3D('',#73356,#45328,#45329);
#36060=AXIS2_PLACEMENT_3D('',#73357,#45330,#45331);
#36061=AXIS2_PLACEMENT_3D('',#73358,#45332,#45333);
#36062=AXIS2_PLACEMENT_3D('',#73359,#45334,#45335);
#36063=AXIS2_PLACEMENT_3D('',#73360,#45336,#45337);
#36064=AXIS2_PLACEMENT_3D('',#73361,#45338,#45339);
#36065=AXIS2_PLACEMENT_3D('',#73362,#45340,#45341);
#36066=AXIS2_PLACEMENT_3D('',#73363,#45342,#45343);
#36067=AXIS2_PLACEMENT_3D('',#73364,#45344,#45345);
#36068=AXIS2_PLACEMENT_3D('',#73365,#45346,#45347);
#36069=AXIS2_PLACEMENT_3D('',#73366,#45348,#45349);
#36070=AXIS2_PLACEMENT_3D('',#73367,#45350,#45351);
#36071=AXIS2_PLACEMENT_3D('',#73368,#45352,#45353);
#36072=AXIS2_PLACEMENT_3D('',#73369,#45354,#45355);
#36073=AXIS2_PLACEMENT_3D('',#73370,#45356,#45357);
#36074=AXIS2_PLACEMENT_3D('',#73371,#45358,#45359);
#36075=AXIS2_PLACEMENT_3D('',#73372,#45360,#45361);
#36076=AXIS2_PLACEMENT_3D('',#73373,#45362,#45363);
#36077=AXIS2_PLACEMENT_3D('',#73374,#45364,#45365);
#36078=AXIS2_PLACEMENT_3D('',#73375,#45366,#45367);
#36079=AXIS2_PLACEMENT_3D('',#73376,#45368,#45369);
#36080=AXIS2_PLACEMENT_3D('',#73377,#45370,#45371);
#36081=AXIS2_PLACEMENT_3D('',#73378,#45372,#45373);
#36082=AXIS2_PLACEMENT_3D('',#73379,#45374,#45375);
#36083=AXIS2_PLACEMENT_3D('',#73380,#45376,#45377);
#36084=AXIS2_PLACEMENT_3D('',#73381,#45378,#45379);
#36085=AXIS2_PLACEMENT_3D('',#73382,#45380,#45381);
#36086=AXIS2_PLACEMENT_3D('',#73383,#45382,#45383);
#36087=AXIS2_PLACEMENT_3D('',#73384,#45384,#45385);
#36088=AXIS2_PLACEMENT_3D('',#73385,#45386,#45387);
#36089=AXIS2_PLACEMENT_3D('',#73386,#45388,#45389);
#36090=AXIS2_PLACEMENT_3D('',#73387,#45390,#45391);
#36091=AXIS2_PLACEMENT_3D('',#73388,#45392,#45393);
#36092=AXIS2_PLACEMENT_3D('',#73389,#45394,#45395);
#36093=AXIS2_PLACEMENT_3D('',#73390,#45396,#45397);
#36094=AXIS2_PLACEMENT_3D('',#73391,#45398,#45399);
#36095=AXIS2_PLACEMENT_3D('',#73393,#45400,#45401);
#36096=AXIS2_PLACEMENT_3D('',#73395,#45402,#45403);
#36097=AXIS2_PLACEMENT_3D('',#73396,#45404,#45405);
#36098=AXIS2_PLACEMENT_3D('',#73397,#45406,#45407);
#36099=AXIS2_PLACEMENT_3D('',#73402,#45410,#45411);
#36100=AXIS2_PLACEMENT_3D('',#73403,#45412,#45413);
#36101=AXIS2_PLACEMENT_3D('',#73404,#45414,#45415);
#36102=AXIS2_PLACEMENT_3D('',#73405,#45416,#45417);
#36103=AXIS2_PLACEMENT_3D('',#73406,#45418,#45419);
#36104=AXIS2_PLACEMENT_3D('',#73407,#45420,#45421);
#36105=AXIS2_PLACEMENT_3D('',#73420,#45428,#45429);
#36106=AXIS2_PLACEMENT_3D('',#73423,#45432,#45433);
#36107=AXIS2_PLACEMENT_3D('',#73425,#45435,#45436);
#36108=AXIS2_PLACEMENT_3D('',#73427,#45438,#45439);
#36109=AXIS2_PLACEMENT_3D('',#73429,#45441,#45442);
#36110=AXIS2_PLACEMENT_3D('',#73431,#45444,#45445);
#36111=AXIS2_PLACEMENT_3D('',#74953,#45447,#45448);
#36112=AXIS2_PLACEMENT_3D('',#74954,#45449,#45450);
#36113=AXIS2_PLACEMENT_3D('',#74956,#45452,#45453);
#36114=AXIS2_PLACEMENT_3D('',#74958,#45455,#45456);
#36115=AXIS2_PLACEMENT_3D('',#74959,#45457,#45458);
#36116=AXIS2_PLACEMENT_3D('',#74961,#45460,#45461);
#36117=AXIS2_PLACEMENT_3D('',#74963,#45463,#45464);
#36118=AXIS2_PLACEMENT_3D('',#74964,#45465,#45466);
#36119=AXIS2_PLACEMENT_3D('',#74966,#45468,#45469);
#36120=AXIS2_PLACEMENT_3D('',#74968,#45471,#45472);
#36121=AXIS2_PLACEMENT_3D('',#74969,#45473,#45474);
#36122=AXIS2_PLACEMENT_3D('',#74971,#45476,#45477);
#36123=AXIS2_PLACEMENT_3D('',#74973,#45479,#45480);
#36124=AXIS2_PLACEMENT_3D('',#74974,#45481,#45482);
#36125=AXIS2_PLACEMENT_3D('',#74976,#45484,#45485);
#36126=AXIS2_PLACEMENT_3D('',#74978,#45487,#45488);
#36127=AXIS2_PLACEMENT_3D('',#74979,#45489,#45490);
#36128=AXIS2_PLACEMENT_3D('',#74981,#45492,#45493);
#36129=AXIS2_PLACEMENT_3D('',#74983,#45495,#45496);
#36130=AXIS2_PLACEMENT_3D('',#74984,#45497,#45498);
#36131=AXIS2_PLACEMENT_3D('',#74986,#45500,#45501);
#36132=AXIS2_PLACEMENT_3D('',#74988,#45503,#45504);
#36133=AXIS2_PLACEMENT_3D('',#74989,#45505,#45506);
#36134=AXIS2_PLACEMENT_3D('',#74990,#45507,#45508);
#36135=AXIS2_PLACEMENT_3D('',#74991,#45509,#45510);
#36136=AXIS2_PLACEMENT_3D('',#74992,#45511,#45512);
#36137=AXIS2_PLACEMENT_3D('',#74993,#45513,#45514);
#36138=AXIS2_PLACEMENT_3D('',#74994,#45515,#45516);
#36139=AXIS2_PLACEMENT_3D('',#74995,#45517,#45518);
#36140=AXIS2_PLACEMENT_3D('',#74996,#45519,#45520);
#36141=AXIS2_PLACEMENT_3D('',#74997,#45521,#45522);
#36142=AXIS2_PLACEMENT_3D('',#74998,#45523,#45524);
#36143=AXIS2_PLACEMENT_3D('',#74999,#45525,#45526);
#36144=AXIS2_PLACEMENT_3D('',#75000,#45527,#45528);
#36145=AXIS2_PLACEMENT_3D('',#75001,#45529,#45530);
#36146=AXIS2_PLACEMENT_3D('',#75002,#45531,#45532);
#36147=AXIS2_PLACEMENT_3D('',#75003,#45533,#45534);
#36148=AXIS2_PLACEMENT_3D('',#75004,#45535,#45536);
#36149=AXIS2_PLACEMENT_3D('',#75005,#45537,#45538);
#36150=AXIS2_PLACEMENT_3D('',#75006,#45539,#45540);
#36151=AXIS2_PLACEMENT_3D('',#75007,#45541,#45542);
#36152=AXIS2_PLACEMENT_3D('',#75009,#45544,#45545);
#36153=AXIS2_PLACEMENT_3D('',#75011,#45547,#45548);
#36154=AXIS2_PLACEMENT_3D('',#75012,#45549,#45550);
#36155=AXIS2_PLACEMENT_3D('',#75014,#45552,#45553);
#36156=AXIS2_PLACEMENT_3D('',#75016,#45555,#45556);
#36157=AXIS2_PLACEMENT_3D('',#75017,#45557,#45558);
#36158=AXIS2_PLACEMENT_3D('',#75019,#45560,#45561);
#36159=AXIS2_PLACEMENT_3D('',#75021,#45563,#45564);
#36160=AXIS2_PLACEMENT_3D('',#75022,#45565,#45566);
#36161=AXIS2_PLACEMENT_3D('',#75024,#45568,#45569);
#36162=AXIS2_PLACEMENT_3D('',#75026,#45571,#45572);
#36163=AXIS2_PLACEMENT_3D('',#75027,#45573,#45574);
#36164=AXIS2_PLACEMENT_3D('',#75029,#45576,#45577);
#36165=AXIS2_PLACEMENT_3D('',#75031,#45579,#45580);
#36166=AXIS2_PLACEMENT_3D('',#75032,#45581,#45582);
#36167=AXIS2_PLACEMENT_3D('',#75034,#45584,#45585);
#36168=AXIS2_PLACEMENT_3D('',#75036,#45587,#45588);
#36169=AXIS2_PLACEMENT_3D('',#75037,#45589,#45590);
#36170=AXIS2_PLACEMENT_3D('',#75039,#45592,#45593);
#36171=AXIS2_PLACEMENT_3D('',#75041,#45595,#45596);
#36172=AXIS2_PLACEMENT_3D('',#75042,#45597,#45598);
#36173=AXIS2_PLACEMENT_3D('',#75044,#45600,#45601);
#36174=AXIS2_PLACEMENT_3D('',#75046,#45603,#45604);
#36175=AXIS2_PLACEMENT_3D('',#75047,#45605,#45606);
#36176=AXIS2_PLACEMENT_3D('',#75049,#45608,#45609);
#36177=AXIS2_PLACEMENT_3D('',#75051,#45611,#45612);
#36178=AXIS2_PLACEMENT_3D('',#75052,#45613,#45614);
#36179=AXIS2_PLACEMENT_3D('',#75054,#45616,#45617);
#36180=AXIS2_PLACEMENT_3D('',#75056,#45619,#45620);
#36181=AXIS2_PLACEMENT_3D('',#75057,#45621,#45622);
#36182=AXIS2_PLACEMENT_3D('',#75059,#45624,#45625);
#36183=AXIS2_PLACEMENT_3D('',#75061,#45627,#45628);
#36184=AXIS2_PLACEMENT_3D('',#75062,#45629,#45630);
#36185=AXIS2_PLACEMENT_3D('',#75064,#45632,#45633);
#36186=AXIS2_PLACEMENT_3D('',#75066,#45635,#45636);
#36187=AXIS2_PLACEMENT_3D('',#75067,#45637,#45638);
#36188=AXIS2_PLACEMENT_3D('',#75069,#45640,#45641);
#36189=AXIS2_PLACEMENT_3D('',#75071,#45643,#45644);
#36190=AXIS2_PLACEMENT_3D('',#75072,#45645,#45646);
#36191=AXIS2_PLACEMENT_3D('',#75074,#45648,#45649);
#36192=AXIS2_PLACEMENT_3D('',#75076,#45651,#45652);
#36193=AXIS2_PLACEMENT_3D('',#75077,#45653,#45654);
#36194=AXIS2_PLACEMENT_3D('',#75079,#45656,#45657);
#36195=AXIS2_PLACEMENT_3D('',#75081,#45659,#45660);
#36196=AXIS2_PLACEMENT_3D('',#75082,#45661,#45662);
#36197=AXIS2_PLACEMENT_3D('',#75084,#45664,#45665);
#36198=AXIS2_PLACEMENT_3D('',#75086,#45667,#45668);
#36199=AXIS2_PLACEMENT_3D('',#75087,#45669,#45670);
#36200=AXIS2_PLACEMENT_3D('',#75089,#45672,#45673);
#36201=AXIS2_PLACEMENT_3D('',#75091,#45675,#45676);
#36202=AXIS2_PLACEMENT_3D('',#75092,#45677,#45678);
#36203=AXIS2_PLACEMENT_3D('',#75094,#45680,#45681);
#36204=AXIS2_PLACEMENT_3D('',#75096,#45683,#45684);
#36205=AXIS2_PLACEMENT_3D('',#75097,#45685,#45686);
#36206=AXIS2_PLACEMENT_3D('',#75099,#45688,#45689);
#36207=AXIS2_PLACEMENT_3D('',#75101,#45691,#45692);
#36208=AXIS2_PLACEMENT_3D('',#75102,#45693,#45694);
#36209=AXIS2_PLACEMENT_3D('',#75104,#45696,#45697);
#36210=AXIS2_PLACEMENT_3D('',#75106,#45699,#45700);
#36211=AXIS2_PLACEMENT_3D('',#75107,#45701,#45702);
#36212=AXIS2_PLACEMENT_3D('',#75109,#45704,#45705);
#36213=AXIS2_PLACEMENT_3D('',#75111,#45707,#45708);
#36214=AXIS2_PLACEMENT_3D('',#75112,#45709,#45710);
#36215=AXIS2_PLACEMENT_3D('',#75114,#45712,#45713);
#36216=AXIS2_PLACEMENT_3D('',#75116,#45715,#45716);
#36217=AXIS2_PLACEMENT_3D('',#75117,#45717,#45718);
#36218=AXIS2_PLACEMENT_3D('',#75119,#45720,#45721);
#36219=AXIS2_PLACEMENT_3D('',#75121,#45723,#45724);
#36220=AXIS2_PLACEMENT_3D('',#75122,#45725,#45726);
#36221=AXIS2_PLACEMENT_3D('',#75124,#45728,#45729);
#36222=AXIS2_PLACEMENT_3D('',#75126,#45731,#45732);
#36223=AXIS2_PLACEMENT_3D('',#75127,#45733,#45734);
#36224=AXIS2_PLACEMENT_3D('',#75129,#45736,#45737);
#36225=AXIS2_PLACEMENT_3D('',#75131,#45739,#45740);
#36226=AXIS2_PLACEMENT_3D('',#75132,#45741,#45742);
#36227=AXIS2_PLACEMENT_3D('',#75134,#45744,#45745);
#36228=AXIS2_PLACEMENT_3D('',#75136,#45747,#45748);
#36229=AXIS2_PLACEMENT_3D('',#75137,#45749,#45750);
#36230=AXIS2_PLACEMENT_3D('',#75139,#45752,#45753);
#36231=AXIS2_PLACEMENT_3D('',#75141,#45755,#45756);
#36232=AXIS2_PLACEMENT_3D('',#75142,#45757,#45758);
#36233=AXIS2_PLACEMENT_3D('',#75144,#45760,#45761);
#36234=AXIS2_PLACEMENT_3D('',#75146,#45763,#45764);
#36235=AXIS2_PLACEMENT_3D('',#75147,#45765,#45766);
#36236=AXIS2_PLACEMENT_3D('',#75149,#45768,#45769);
#36237=AXIS2_PLACEMENT_3D('',#75151,#45771,#45772);
#36238=AXIS2_PLACEMENT_3D('',#75152,#45773,#45774);
#36239=AXIS2_PLACEMENT_3D('',#75154,#45776,#45777);
#36240=AXIS2_PLACEMENT_3D('',#75156,#45779,#45780);
#36241=AXIS2_PLACEMENT_3D('',#75157,#45781,#45782);
#36242=AXIS2_PLACEMENT_3D('',#75159,#45784,#45785);
#36243=AXIS2_PLACEMENT_3D('',#75161,#45787,#45788);
#36244=AXIS2_PLACEMENT_3D('',#75162,#45789,#45790);
#36245=AXIS2_PLACEMENT_3D('',#75164,#45792,#45793);
#36246=AXIS2_PLACEMENT_3D('',#75166,#45795,#45796);
#36247=AXIS2_PLACEMENT_3D('',#75167,#45797,#45798);
#36248=AXIS2_PLACEMENT_3D('',#75169,#45800,#45801);
#36249=AXIS2_PLACEMENT_3D('',#75171,#45803,#45804);
#36250=AXIS2_PLACEMENT_3D('',#75172,#45805,#45806);
#36251=AXIS2_PLACEMENT_3D('',#75174,#45808,#45809);
#36252=AXIS2_PLACEMENT_3D('',#75176,#45811,#45812);
#36253=AXIS2_PLACEMENT_3D('',#75177,#45813,#45814);
#36254=AXIS2_PLACEMENT_3D('',#75179,#45816,#45817);
#36255=AXIS2_PLACEMENT_3D('',#75181,#45819,#45820);
#36256=AXIS2_PLACEMENT_3D('',#75182,#45821,#45822);
#36257=AXIS2_PLACEMENT_3D('',#75184,#45824,#45825);
#36258=AXIS2_PLACEMENT_3D('',#75186,#45827,#45828);
#36259=AXIS2_PLACEMENT_3D('',#75187,#45829,#45830);
#36260=AXIS2_PLACEMENT_3D('',#75189,#45832,#45833);
#36261=AXIS2_PLACEMENT_3D('',#75191,#45835,#45836);
#36262=AXIS2_PLACEMENT_3D('',#75192,#45837,#45838);
#36263=AXIS2_PLACEMENT_3D('',#75194,#45840,#45841);
#36264=AXIS2_PLACEMENT_3D('',#75196,#45843,#45844);
#36265=AXIS2_PLACEMENT_3D('',#75197,#45845,#45846);
#36266=AXIS2_PLACEMENT_3D('',#75199,#45848,#45849);
#36267=AXIS2_PLACEMENT_3D('',#75201,#45851,#45852);
#36268=AXIS2_PLACEMENT_3D('',#75202,#45853,#45854);
#36269=AXIS2_PLACEMENT_3D('',#75204,#45856,#45857);
#36270=AXIS2_PLACEMENT_3D('',#75206,#45859,#45860);
#36271=AXIS2_PLACEMENT_3D('',#75207,#45861,#45862);
#36272=AXIS2_PLACEMENT_3D('',#75209,#45864,#45865);
#36273=AXIS2_PLACEMENT_3D('',#75211,#45867,#45868);
#36274=AXIS2_PLACEMENT_3D('',#75212,#45869,#45870);
#36275=AXIS2_PLACEMENT_3D('',#75214,#45872,#45873);
#36276=AXIS2_PLACEMENT_3D('',#75216,#45875,#45876);
#36277=AXIS2_PLACEMENT_3D('',#75217,#45877,#45878);
#36278=AXIS2_PLACEMENT_3D('',#75219,#45880,#45881);
#36279=AXIS2_PLACEMENT_3D('',#75221,#45883,#45884);
#36280=AXIS2_PLACEMENT_3D('',#75222,#45885,#45886);
#36281=AXIS2_PLACEMENT_3D('',#75224,#45888,#45889);
#36282=AXIS2_PLACEMENT_3D('',#75226,#45891,#45892);
#36283=AXIS2_PLACEMENT_3D('',#75227,#45893,#45894);
#36284=AXIS2_PLACEMENT_3D('',#75229,#45896,#45897);
#36285=AXIS2_PLACEMENT_3D('',#75231,#45899,#45900);
#36286=AXIS2_PLACEMENT_3D('',#75232,#45901,#45902);
#36287=AXIS2_PLACEMENT_3D('',#75234,#45904,#45905);
#36288=AXIS2_PLACEMENT_3D('',#75236,#45907,#45908);
#36289=AXIS2_PLACEMENT_3D('',#75237,#45909,#45910);
#36290=AXIS2_PLACEMENT_3D('',#75239,#45912,#45913);
#36291=AXIS2_PLACEMENT_3D('',#75241,#45915,#45916);
#36292=AXIS2_PLACEMENT_3D('',#75242,#45917,#45918);
#36293=AXIS2_PLACEMENT_3D('',#75244,#45920,#45921);
#36294=AXIS2_PLACEMENT_3D('',#75246,#45923,#45924);
#36295=AXIS2_PLACEMENT_3D('',#75247,#45925,#45926);
#36296=AXIS2_PLACEMENT_3D('',#75249,#45928,#45929);
#36297=AXIS2_PLACEMENT_3D('',#75251,#45931,#45932);
#36298=AXIS2_PLACEMENT_3D('',#75252,#45933,#45934);
#36299=AXIS2_PLACEMENT_3D('',#75254,#45936,#45937);
#36300=AXIS2_PLACEMENT_3D('',#75256,#45939,#45940);
#36301=AXIS2_PLACEMENT_3D('',#75257,#45941,#45942);
#36302=AXIS2_PLACEMENT_3D('',#75259,#45944,#45945);
#36303=AXIS2_PLACEMENT_3D('',#75261,#45947,#45948);
#36304=AXIS2_PLACEMENT_3D('',#75262,#45949,#45950);
#36305=AXIS2_PLACEMENT_3D('',#75264,#45952,#45953);
#36306=AXIS2_PLACEMENT_3D('',#75266,#45955,#45956);
#36307=AXIS2_PLACEMENT_3D('',#75267,#45957,#45958);
#36308=AXIS2_PLACEMENT_3D('',#75269,#45960,#45961);
#36309=AXIS2_PLACEMENT_3D('',#75271,#45963,#45964);
#36310=AXIS2_PLACEMENT_3D('',#75272,#45965,#45966);
#36311=AXIS2_PLACEMENT_3D('',#75274,#45968,#45969);
#36312=AXIS2_PLACEMENT_3D('',#75276,#45971,#45972);
#36313=AXIS2_PLACEMENT_3D('',#75277,#45973,#45974);
#36314=AXIS2_PLACEMENT_3D('',#75279,#45976,#45977);
#36315=AXIS2_PLACEMENT_3D('',#75281,#45979,#45980);
#36316=AXIS2_PLACEMENT_3D('',#75282,#45981,#45982);
#36317=AXIS2_PLACEMENT_3D('',#75284,#45984,#45985);
#36318=AXIS2_PLACEMENT_3D('',#75286,#45987,#45988);
#36319=AXIS2_PLACEMENT_3D('',#75287,#45989,#45990);
#36320=AXIS2_PLACEMENT_3D('',#75289,#45992,#45993);
#36321=AXIS2_PLACEMENT_3D('',#75291,#45995,#45996);
#36322=AXIS2_PLACEMENT_3D('',#75292,#45997,#45998);
#36323=AXIS2_PLACEMENT_3D('',#75294,#46000,#46001);
#36324=AXIS2_PLACEMENT_3D('',#75296,#46003,#46004);
#36325=AXIS2_PLACEMENT_3D('',#75297,#46005,#46006);
#36326=AXIS2_PLACEMENT_3D('',#75298,#46007,#46008);
#36327=AXIS2_PLACEMENT_3D('',#75299,#46009,#46010);
#36328=AXIS2_PLACEMENT_3D('',#75300,#46011,#46012);
#36329=AXIS2_PLACEMENT_3D('',#75301,#46013,#46014);
#36330=AXIS2_PLACEMENT_3D('',#75302,#46015,#46016);
#36331=AXIS2_PLACEMENT_3D('',#75303,#46017,#46018);
#36332=AXIS2_PLACEMENT_3D('',#75304,#46019,#46020);
#36333=AXIS2_PLACEMENT_3D('',#75305,#46021,#46022);
#36334=AXIS2_PLACEMENT_3D('',#75306,#46023,#46024);
#36335=AXIS2_PLACEMENT_3D('',#75307,#46025,#46026);
#36336=AXIS2_PLACEMENT_3D('',#75308,#46027,#46028);
#36337=AXIS2_PLACEMENT_3D('',#75309,#46029,#46030);
#36338=AXIS2_PLACEMENT_3D('',#75310,#46031,#46032);
#36339=AXIS2_PLACEMENT_3D('',#75311,#46033,#46034);
#36340=AXIS2_PLACEMENT_3D('',#75312,#46035,#46036);
#36341=AXIS2_PLACEMENT_3D('',#75313,#46037,#46038);
#36342=AXIS2_PLACEMENT_3D('',#75314,#46039,#46040);
#36343=AXIS2_PLACEMENT_3D('',#75315,#46041,#46042);
#36344=AXIS2_PLACEMENT_3D('',#75316,#46043,#46044);
#36345=DIRECTION('axis',(0.,0.,1.));
#36346=DIRECTION('refdir',(1.,0.,0.));
#36347=DIRECTION('axis',(0.,0.,1.));
#36348=DIRECTION('refdir',(1.,0.,0.));
#36349=DIRECTION('center_axis',(0.496731764892154,0.286788218175523,-0.819152044288992));
#36350=DIRECTION('ref_axis',(-0.709406479916223,-0.409576022144496,-0.573576436351046));
#36351=DIRECTION('',(-0.427535056636437,-0.740512440111147,-0.51851239270389));
#36352=DIRECTION('',(0.5,-0.866025403784439,0.));
#36353=DIRECTION('',(-0.709406479916223,-0.409576022144496,-0.573576436351046));
#36354=DIRECTION('',(-0.5,0.866025403784439,0.));
#36355=DIRECTION('center_axis',(-0.496731764892154,0.286788218175523,-0.819152044288992));
#36356=DIRECTION('ref_axis',(0.709406479916223,-0.409576022144496,-0.573576436351046));
#36357=DIRECTION('',(-0.855070113272875,2.22044604925031E-16,0.51851239270389));
#36358=DIRECTION('',(0.5,0.866025403784439,0.));
#36359=DIRECTION('',(0.709406479916223,-0.409576022144496,-0.573576436351045));
#36360=DIRECTION('',(-0.5,-0.866025403784439,0.));
#36361=DIRECTION('center_axis',(0.496731764892154,-0.286788218175523,-0.819152044288992));
#36362=DIRECTION('ref_axis',(0.709406479916223,-0.409576022144496,0.573576436351046));
#36363=DIRECTION('',(0.427535056636437,-0.740512440111147,0.518512392703891));
#36364=DIRECTION('',(0.709406479916223,-0.409576022144496,0.573576436351045));
#36365=DIRECTION('',(-0.5,-0.866025403784439,0.));
#36366=DIRECTION('center_axis',(-0.500000000000001,-0.866025403784438,0.));
#36367=DIRECTION('ref_axis',(0.,0.,-1.));
#36368=DIRECTION('',(-0.866025403784438,0.5,0.));
#36369=DIRECTION('center_axis',(-0.496731764892154,-0.286788218175523,-0.819152044288992));
#36370=DIRECTION('ref_axis',(-0.709406479916223,-0.409576022144496,0.573576436351046));
#36371=DIRECTION('',(-0.709406479916223,-0.409576022144496,0.573576436351046));
#36372=DIRECTION('',(-0.5,0.866025403784439,0.));
#36373=DIRECTION('center_axis',(-0.5,0.866025403784439,0.));
#36374=DIRECTION('ref_axis',(0.,0.,-1.));
#36375=DIRECTION('',(0.866025403784439,0.5,0.));
#36376=DIRECTION('center_axis',(0.,0.573576436351046,-0.819152044288992));
#36377=DIRECTION('ref_axis',(0.,0.819152044288992,0.573576436351046));
#36378=DIRECTION('',(1.,0.,0.));
#36379=DIRECTION('',(0.,0.819152044288992,0.573576436351046));
#36380=DIRECTION('',(1.,0.,0.));
#36381=DIRECTION('center_axis',(0.,-0.573576436351046,-0.819152044288992));
#36382=DIRECTION('ref_axis',(0.,0.819152044288992,-0.573576436351046));
#36383=DIRECTION('',(-1.,0.,0.));
#36384=DIRECTION('',(0.,0.819152044288992,-0.573576436351046));
#36385=DIRECTION('center_axis',(1.,0.,0.));
#36386=DIRECTION('ref_axis',(0.,0.,-1.));
#36387=DIRECTION('',(0.,-1.,0.));
#36388=DIRECTION('center_axis',(0.,0.,1.));
#36389=DIRECTION('ref_axis',(1.,0.,0.));
#36390=DIRECTION('center_axis',(0.,0.,1.));
#36391=DIRECTION('ref_axis',(1.,0.,0.));
#36392=DIRECTION('',(0.,0.,-1.));
#36393=DIRECTION('center_axis',(0.,0.,1.));
#36394=DIRECTION('ref_axis',(1.,0.,0.));
#36395=DIRECTION('center_axis',(0.,0.,1.));
#36396=DIRECTION('ref_axis',(1.,0.,0.));
#36397=DIRECTION('center_axis',(0.,0.,1.));
#36398=DIRECTION('ref_axis',(1.,0.,0.));
#36399=DIRECTION('axis',(0.,0.,1.));
#36400=DIRECTION('refdir',(1.,0.,0.));
#36401=DIRECTION('center_axis',(0.,0.,1.));
#36402=DIRECTION('ref_axis',(1.,0.,0.));
#36403=DIRECTION('center_axis',(1.22464679914735E-16,-1.,0.));
#36404=DIRECTION('ref_axis',(-1.,-1.22464679914735E-16,0.));
#36405=DIRECTION('axis',(0.,0.,1.));
#36406=DIRECTION('refdir',(1.,0.,0.));
#36407=DIRECTION('center_axis',(0.,0.,1.));
#36408=DIRECTION('ref_axis',(-0.5,0.866025403784439,0.));
#36409=DIRECTION('center_axis',(0.866025403784439,0.5,0.));
#36410=DIRECTION('ref_axis',(0.5,-0.866025403784439,0.));
#36411=DIRECTION('axis',(0.,0.,1.));
#36412=DIRECTION('refdir',(1.,0.,0.));
#36413=DIRECTION('center_axis',(0.,0.,1.));
#36414=DIRECTION('ref_axis',(-0.5,-0.866025403784438,0.));
#36415=DIRECTION('center_axis',(-0.866025403784439,0.5,0.));
#36416=DIRECTION('ref_axis',(0.5,0.866025403784439,0.));
#36417=DIRECTION('axis',(0.,0.,1.));
#36418=DIRECTION('refdir',(1.,0.,0.));
#36419=DIRECTION('center_axis',(0.,0.,-1.));
#36420=DIRECTION('ref_axis',(0.5,0.866025403784438,0.));
#36421=DIRECTION('center_axis',(0.,0.,-1.));
#36422=DIRECTION('ref_axis',(0.5,0.866025403784438,0.));
#36423=DIRECTION('',(0.,0.,-1.));
#36424=DIRECTION('center_axis',(0.,0.,1.));
#36425=DIRECTION('ref_axis',(0.5,0.866025403784438,0.));
#36426=DIRECTION('center_axis',(0.,0.,-1.));
#36427=DIRECTION('ref_axis',(0.5,-0.866025403784439,0.));
#36428=DIRECTION('center_axis',(0.,0.,-1.));
#36429=DIRECTION('ref_axis',(0.5,-0.866025403784439,0.));
#36430=DIRECTION('',(0.,0.,-1.));
#36431=DIRECTION('center_axis',(0.,0.,1.));
#36432=DIRECTION('ref_axis',(0.5,-0.866025403784439,0.));
#36433=DIRECTION('center_axis',(0.,0.,-1.));
#36434=DIRECTION('ref_axis',(-1.,0.,0.));
#36435=DIRECTION('center_axis',(0.,0.,-1.));
#36436=DIRECTION('ref_axis',(-1.,0.,0.));
#36437=DIRECTION('',(0.,0.,-1.));
#36438=DIRECTION('center_axis',(0.,0.,1.));
#36439=DIRECTION('ref_axis',(-1.,0.,0.));
#36440=DIRECTION('center_axis',(0.,0.,1.));
#36441=DIRECTION('ref_axis',(-0.5,-0.866025403784439,0.));
#36442=DIRECTION('center_axis',(0.,0.,-1.));
#36443=DIRECTION('ref_axis',(-0.5,-0.866025403784439,0.));
#36444=DIRECTION('',(0.,0.,1.));
#36445=DIRECTION('center_axis',(0.,0.,1.));
#36446=DIRECTION('ref_axis',(-0.5,-0.866025403784439,0.));
#36447=DIRECTION('',(0.,0.,-1.));
#36448=DIRECTION('center_axis',(0.866025403784439,0.5,0.));
#36449=DIRECTION('ref_axis',(-0.5,0.866025403784439,0.));
#36450=DIRECTION('',(-0.5,0.866025403784439,0.));
#36451=DIRECTION('',(0.,0.,-1.));
#36452=DIRECTION('',(-0.5,0.866025403784439,0.));
#36453=DIRECTION('center_axis',(0.,0.,1.));
#36454=DIRECTION('ref_axis',(-0.5,0.866025403784439,0.));
#36455=DIRECTION('center_axis',(0.,0.,-1.));
#36456=DIRECTION('ref_axis',(-0.5,0.866025403784439,0.));
#36457=DIRECTION('',(0.,0.,1.));
#36458=DIRECTION('center_axis',(0.,0.,1.));
#36459=DIRECTION('ref_axis',(-0.5,0.866025403784439,0.));
#36460=DIRECTION('',(0.,0.,-1.));
#36461=DIRECTION('center_axis',(0.,-1.,0.));
#36462=DIRECTION('ref_axis',(1.,0.,0.));
#36463=DIRECTION('',(1.,0.,0.));
#36464=DIRECTION('',(0.,0.,-1.));
#36465=DIRECTION('',(1.,0.,0.));
#36466=DIRECTION('center_axis',(0.,0.,1.));
#36467=DIRECTION('ref_axis',(1.,-1.92296268638356E-16,0.));
#36468=DIRECTION('center_axis',(0.,0.,-1.));
#36469=DIRECTION('ref_axis',(1.,-1.92296268638356E-16,0.));
#36470=DIRECTION('',(0.,0.,1.));
#36471=DIRECTION('center_axis',(0.,0.,1.));
#36472=DIRECTION('ref_axis',(1.,-1.92296268638356E-16,0.));
#36473=DIRECTION('',(0.,0.,-1.));
#36474=DIRECTION('center_axis',(-0.866025403784438,0.5,0.));
#36475=DIRECTION('ref_axis',(-0.5,-0.866025403784438,0.));
#36476=DIRECTION('',(-0.5,-0.866025403784439,0.));
#36477=DIRECTION('',(0.,0.,-1.));
#36478=DIRECTION('',(-0.5,-0.866025403784439,0.));
#36479=DIRECTION('center_axis',(0.,0.,1.));
#36480=DIRECTION('ref_axis',(0.327326835353988,-0.944911182523068,0.));
#36481=DIRECTION('center_axis',(0.,0.,-1.));
#36482=DIRECTION('ref_axis',(0.327326835353988,-0.944911182523068,0.));
#36483=DIRECTION('',(0.,0.,-1.));
#36484=DIRECTION('center_axis',(0.,0.,1.));
#36485=DIRECTION('ref_axis',(0.327326835353988,-0.944911182523068,0.));
#36486=DIRECTION('',(0.,0.,1.));
#36487=DIRECTION('center_axis',(0.,0.,1.));
#36488=DIRECTION('ref_axis',(-1.,0.,0.));
#36489=DIRECTION('center_axis',(0.,0.,1.));
#36490=DIRECTION('ref_axis',(-1.,0.,0.));
#36491=DIRECTION('',(0.,0.,1.));
#36492=DIRECTION('center_axis',(0.,0.,1.));
#36493=DIRECTION('ref_axis',(-1.,0.,0.));
#36494=DIRECTION('center_axis',(0.,0.,1.));
#36495=DIRECTION('ref_axis',(-1.,0.,0.));
#36496=DIRECTION('',(0.5,0.866025403784439,0.));
#36497=DIRECTION('center_axis',(0.,0.,-1.));
#36498=DIRECTION('ref_axis',(0.654653670707978,-0.755928946018454,0.));
#36499=DIRECTION('center_axis',(0.,0.,1.));
#36500=DIRECTION('ref_axis',(-1.,0.,0.));
#36501=DIRECTION('center_axis',(0.,0.,-1.));
#36502=DIRECTION('ref_axis',(0.654653670707978,0.755928946018454,0.));
#36503=DIRECTION('',(-1.,0.,0.));
#36504=DIRECTION('center_axis',(0.,0.,-1.));
#36505=DIRECTION('ref_axis',(0.327326835353989,0.944911182523068,0.));
#36506=DIRECTION('center_axis',(0.,0.,1.));
#36507=DIRECTION('ref_axis',(-1.,0.,0.));
#36508=DIRECTION('center_axis',(0.,0.,-1.));
#36509=DIRECTION('ref_axis',(-0.981980506061966,0.188982236504613,0.));
#36510=DIRECTION('',(0.5,-0.866025403784439,0.));
#36511=DIRECTION('center_axis',(0.,0.,-1.));
#36512=DIRECTION('ref_axis',(-0.981980506061966,-0.188982236504613,0.));
#36513=DIRECTION('center_axis',(0.,0.,1.));
#36514=DIRECTION('ref_axis',(0.654653670707978,-0.755928946018454,0.));
#36515=DIRECTION('center_axis',(0.,0.,1.));
#36516=DIRECTION('ref_axis',(0.654653670707978,-0.755928946018454,0.));
#36517=DIRECTION('',(0.,0.,1.));
#36518=DIRECTION('center_axis',(0.,0.,1.));
#36519=DIRECTION('ref_axis',(1.,-1.22464679914735E-16,0.));
#36520=DIRECTION('center_axis',(0.,0.,1.));
#36521=DIRECTION('ref_axis',(-1.,0.,0.));
#36522=DIRECTION('',(0.,0.,-1.));
#36523=DIRECTION('center_axis',(0.,0.,1.));
#36524=DIRECTION('ref_axis',(0.654653670707978,0.755928946018454,0.));
#36525=DIRECTION('center_axis',(0.,0.,1.));
#36526=DIRECTION('ref_axis',(0.654653670707978,0.755928946018454,0.));
#36527=DIRECTION('',(0.,0.,1.));
#36528=DIRECTION('center_axis',(0.,0.,1.));
#36529=DIRECTION('ref_axis',(0.327326835353989,0.944911182523068,0.));
#36530=DIRECTION('center_axis',(0.,0.,1.));
#36531=DIRECTION('ref_axis',(0.327326835353989,0.944911182523068,0.));
#36532=DIRECTION('',(0.,0.,1.));
#36533=DIRECTION('center_axis',(0.,0.,1.));
#36534=DIRECTION('ref_axis',(-0.981980506061966,-0.188982236504613,0.));
#36535=DIRECTION('center_axis',(0.,0.,1.));
#36536=DIRECTION('ref_axis',(-0.981980506061966,-0.188982236504613,0.));
#36537=DIRECTION('center_axis',(0.,0.,1.));
#36538=DIRECTION('ref_axis',(-0.981980506061966,0.188982236504613,0.));
#36539=DIRECTION('',(0.,0.,-1.));
#36540=DIRECTION('center_axis',(0.,0.,1.));
#36541=DIRECTION('ref_axis',(-0.981980506061966,0.188982236504613,0.));
#36542=DIRECTION('',(0.,0.,1.));
#36543=DIRECTION('center_axis',(-0.866025403784439,-0.5,0.));
#36544=DIRECTION('ref_axis',(0.5,-0.866025403784439,0.));
#36545=DIRECTION('',(0.5,-0.866025403784439,0.));
#36546=DIRECTION('center_axis',(0.,0.,1.));
#36547=DIRECTION('ref_axis',(-1.,0.,0.));
#36548=DIRECTION('center_axis',(0.,0.,1.));
#36549=DIRECTION('ref_axis',(-1.,0.,0.));
#36550=DIRECTION('center_axis',(0.,1.,0.));
#36551=DIRECTION('ref_axis',(-1.,0.,0.));
#36552=DIRECTION('',(-1.,0.,0.));
#36553=DIRECTION('center_axis',(0.866025403784438,-0.5,0.));
#36554=DIRECTION('ref_axis',(0.5,0.866025403784438,0.));
#36555=DIRECTION('',(0.5,0.866025403784439,0.));
#36556=DIRECTION('center_axis',(0.,0.,1.));
#36557=DIRECTION('ref_axis',(-1.,0.,0.));
#36558=DIRECTION('axis',(0.,0.,1.));
#36559=DIRECTION('refdir',(1.,0.,0.));
#36560=DIRECTION('center_axis',(5.15167520928809E-67,-1.18789542670764E-48,
-1.));
#36561=DIRECTION('ref_axis',(-4.33680868994202E-19,1.,-1.18789542670764E-48));
#36562=DIRECTION('',(-5.15167520928809E-67,1.18789542670764E-48,1.));
#36563=DIRECTION('',(-5.15167520928809E-67,1.18789542670764E-48,1.));
#36564=DIRECTION('center_axis',(5.15167520928809E-67,-1.18789542670764E-48,
-1.));
#36565=DIRECTION('ref_axis',(-4.33680868994202E-19,1.,-1.18789542670764E-48));
#36566=DIRECTION('center_axis',(-4.70261923768679E-35,1.08435016942139E-16,
-1.));
#36567=DIRECTION('ref_axis',(-4.33680868994202E-19,1.,1.08435016942139E-16));
#36568=DIRECTION('center_axis',(5.15167520928809E-67,-1.18789542670764E-48,
-1.));
#36569=DIRECTION('ref_axis',(-4.33680868994202E-19,1.,-1.18789542670764E-48));
#36570=DIRECTION('',(-5.15167520928809E-67,1.18789542670764E-48,1.));
#36571=DIRECTION('center_axis',(5.15167520928809E-67,-1.18789542670764E-48,
-1.));
#36572=DIRECTION('ref_axis',(-4.33680868994202E-19,1.,-1.18789542670764E-48));
#36573=DIRECTION('',(-5.15167520928809E-67,1.18789542670764E-48,1.));
#36574=DIRECTION('center_axis',(5.15167520928809E-67,-1.18789542670764E-48,
-1.));
#36575=DIRECTION('ref_axis',(-4.33680868994202E-19,1.,-1.18789542670764E-48));
#36576=DIRECTION('',(-5.15167520928809E-67,1.18789542670764E-48,1.));
#36577=DIRECTION('center_axis',(5.15167520928809E-67,-1.18789542670764E-48,
-1.));
#36578=DIRECTION('ref_axis',(-4.33680868994202E-19,1.,-1.18789542670764E-48));
#36579=DIRECTION('',(-5.15167520928809E-67,1.18789542670764E-48,1.));
#36580=DIRECTION('center_axis',(5.15167520928809E-67,-1.18789542670764E-48,
-1.));
#36581=DIRECTION('ref_axis',(-4.33680868994202E-19,1.,-1.18789542670764E-48));
#36582=DIRECTION('',(-5.15167520928809E-67,1.18789542670764E-48,1.));
#36583=DIRECTION('center_axis',(5.15167520928809E-67,-1.18789542670764E-48,
-1.));
#36584=DIRECTION('ref_axis',(-4.33680868994202E-19,1.,-1.18789542670764E-48));
#36585=DIRECTION('',(-5.15167520928809E-67,1.18789542670764E-48,1.));
#36586=DIRECTION('center_axis',(5.15167520928809E-67,-1.18789542670764E-48,
-1.));
#36587=DIRECTION('ref_axis',(-4.33680868994202E-19,1.,-1.18789542670764E-48));
#36588=DIRECTION('',(-5.15167520928809E-67,1.18789542670764E-48,1.));
#36589=DIRECTION('center_axis',(5.15167520928809E-67,-1.18789542670764E-48,
-1.));
#36590=DIRECTION('ref_axis',(-4.33680868994202E-19,1.,-1.18789542670764E-48));
#36591=DIRECTION('',(-5.15167520928809E-67,1.18789542670764E-48,1.));
#36592=DIRECTION('center_axis',(5.15167520928809E-67,-1.18789542670764E-48,
-1.));
#36593=DIRECTION('ref_axis',(-4.33680868994202E-19,1.,-1.18789542670764E-48));
#36594=DIRECTION('',(-5.15167520928809E-67,1.18789542670764E-48,1.));
#36595=DIRECTION('center_axis',(5.15167520928809E-67,-1.18789542670764E-48,
-1.));
#36596=DIRECTION('ref_axis',(-4.33680868994202E-19,1.,-1.18789542670764E-48));
#36597=DIRECTION('',(-5.15167520928809E-67,1.18789542670764E-48,1.));
#36598=DIRECTION('center_axis',(5.15167520928809E-67,-1.18789542670764E-48,
-1.));
#36599=DIRECTION('ref_axis',(-4.33680868994202E-19,1.,-1.18789542670764E-48));
#36600=DIRECTION('',(-5.15167520928809E-67,1.18789542670764E-48,1.));
#36601=DIRECTION('center_axis',(5.15167520928809E-67,-1.18789542670764E-48,
-1.));
#36602=DIRECTION('ref_axis',(-4.33680868994202E-19,1.,-1.18789542670764E-48));
#36603=DIRECTION('',(-5.15167520928809E-67,1.18789542670764E-48,1.));
#36604=DIRECTION('center_axis',(5.15167520928809E-67,-1.18789542670764E-48,
-1.));
#36605=DIRECTION('ref_axis',(-4.33680868994202E-19,1.,-1.18789542670764E-48));
#36606=DIRECTION('',(-5.15167520928809E-67,1.18789542670764E-48,1.));
#36607=DIRECTION('center_axis',(5.15167520928809E-67,-1.18789542670764E-48,
-1.));
#36608=DIRECTION('ref_axis',(-4.33680868994202E-19,1.,-1.18789542670764E-48));
#36609=DIRECTION('',(-5.15167520928809E-67,1.18789542670764E-48,1.));
#36610=DIRECTION('center_axis',(5.15167520928809E-67,-1.18789542670764E-48,
-1.));
#36611=DIRECTION('ref_axis',(-4.33680868994202E-19,1.,-1.18789542670764E-48));
#36612=DIRECTION('',(-5.15167520928809E-67,1.18789542670764E-48,1.));
#36613=DIRECTION('center_axis',(5.15167520928809E-67,-1.18789542670764E-48,
-1.));
#36614=DIRECTION('ref_axis',(-4.33680868994202E-19,1.,-1.18789542670764E-48));
#36615=DIRECTION('',(-5.15167520928809E-67,1.18789542670764E-48,1.));
#36616=DIRECTION('center_axis',(5.15167520928809E-67,-1.18789542670764E-48,
-1.));
#36617=DIRECTION('ref_axis',(-4.33680868994202E-19,1.,-1.18789542670764E-48));
#36618=DIRECTION('',(-5.15167520928809E-67,1.18789542670764E-48,1.));
#36619=DIRECTION('center_axis',(5.15167520928809E-67,-1.18789542670764E-48,
-1.));
#36620=DIRECTION('ref_axis',(-4.33680868994202E-19,1.,-1.18789542670764E-48));
#36621=DIRECTION('',(-5.15167520928809E-67,1.18789542670764E-48,1.));
#36622=DIRECTION('center_axis',(5.15167520928809E-67,-1.18789542670764E-48,
-1.));
#36623=DIRECTION('ref_axis',(-4.33680868994202E-19,1.,-1.18789542670764E-48));
#36624=DIRECTION('',(-5.15167520928809E-67,1.18789542670764E-48,1.));
#36625=DIRECTION('center_axis',(5.15167520928809E-67,-1.18789542670764E-48,
-1.));
#36626=DIRECTION('ref_axis',(-4.33680868994202E-19,1.,-1.18789542670764E-48));
#36627=DIRECTION('',(-5.15167520928809E-67,1.18789542670764E-48,1.));
#36628=DIRECTION('center_axis',(5.15167520928809E-67,-1.18789542670764E-48,
-1.));
#36629=DIRECTION('ref_axis',(-4.33680868994202E-19,1.,-1.18789542670764E-48));
#36630=DIRECTION('',(-5.15167520928809E-67,1.18789542670764E-48,1.));
#36631=DIRECTION('center_axis',(5.15167520928809E-67,-1.18789542670764E-48,
-1.));
#36632=DIRECTION('ref_axis',(-4.33680868994202E-19,1.,-1.18789542670764E-48));
#36633=DIRECTION('',(-5.15167520928809E-67,1.18789542670764E-48,1.));
#36634=DIRECTION('center_axis',(5.15167520928809E-67,-1.18789542670764E-48,
-1.));
#36635=DIRECTION('ref_axis',(-4.33680868994202E-19,1.,-1.18789542670764E-48));
#36636=DIRECTION('',(-5.15167520928809E-67,1.18789542670764E-48,1.));
#36637=DIRECTION('center_axis',(5.15167520928809E-67,-1.18789542670764E-48,
-1.));
#36638=DIRECTION('ref_axis',(-4.33680868994202E-19,1.,-1.18789542670764E-48));
#36639=DIRECTION('',(-5.15167520928809E-67,1.18789542670764E-48,1.));
#36640=DIRECTION('center_axis',(5.15167520928809E-67,-1.18789542670764E-48,
-1.));
#36641=DIRECTION('ref_axis',(-4.33680868994202E-19,1.,-1.18789542670764E-48));
#36642=DIRECTION('',(-5.15167520928809E-67,1.18789542670764E-48,1.));
#36643=DIRECTION('center_axis',(5.15167520928809E-67,-1.18789542670764E-48,
-1.));
#36644=DIRECTION('ref_axis',(-4.33680868994202E-19,1.,-1.18789542670764E-48));
#36645=DIRECTION('',(-5.15167520928809E-67,1.18789542670764E-48,1.));
#36646=DIRECTION('center_axis',(5.15167520928809E-67,-1.18789542670764E-48,
-1.));
#36647=DIRECTION('ref_axis',(-4.33680868994202E-19,1.,-1.18789542670764E-48));
#36648=DIRECTION('',(-5.15167520928809E-67,1.18789542670764E-48,1.));
#36649=DIRECTION('center_axis',(-5.15167520928809E-67,1.18789542670764E-48,
1.));
#36650=DIRECTION('ref_axis',(4.33680868994202E-19,-1.,1.18789542670764E-48));
#36651=DIRECTION('',(8.69022643068855E-17,-0.707106781186544,-0.707106781186551));
#36652=DIRECTION('center_axis',(5.15167520928809E-67,-1.18789542670764E-48,
-1.));
#36653=DIRECTION('ref_axis',(-4.33680868994202E-19,1.,-1.18789542670764E-48));
#36654=DIRECTION('center_axis',(0.,0.,1.));
#36655=DIRECTION('ref_axis',(5.30947313395831E-16,1.,0.));
#36656=DIRECTION('',(0.,0.,-1.));
#36657=DIRECTION('center_axis',(5.15167520928809E-67,-1.18789542670764E-48,
-1.));
#36658=DIRECTION('ref_axis',(-4.33680868994202E-19,1.,-1.18789542670764E-48));
#36659=DIRECTION('center_axis',(0.,0.,1.));
#36660=DIRECTION('ref_axis',(5.30947313395831E-16,1.,0.));
#36661=DIRECTION('',(0.,0.,-1.));
#36662=DIRECTION('center_axis',(0.,0.,1.));
#36663=DIRECTION('ref_axis',(5.30947313395831E-16,1.,0.));
#36664=DIRECTION('',(0.,0.,-1.));
#36665=DIRECTION('center_axis',(0.,0.,1.));
#36666=DIRECTION('ref_axis',(5.30947313395831E-16,1.,0.));
#36667=DIRECTION('',(0.,0.,-1.));
#36668=DIRECTION('center_axis',(0.,0.,1.));
#36669=DIRECTION('ref_axis',(5.30947313395831E-16,1.,0.));
#36670=DIRECTION('',(0.,0.,-1.));
#36671=DIRECTION('center_axis',(0.,0.,1.));
#36672=DIRECTION('ref_axis',(5.30947313395831E-16,1.,0.));
#36673=DIRECTION('',(0.,0.,-1.));
#36674=DIRECTION('center_axis',(0.,0.,1.));
#36675=DIRECTION('ref_axis',(5.30947313395831E-16,1.,0.));
#36676=DIRECTION('',(0.,0.,-1.));
#36677=DIRECTION('center_axis',(0.,0.,1.));
#36678=DIRECTION('ref_axis',(5.30947313395831E-16,1.,0.));
#36679=DIRECTION('',(0.,0.,-1.));
#36680=DIRECTION('center_axis',(0.,0.,1.));
#36681=DIRECTION('ref_axis',(5.30947313395831E-16,1.,0.));
#36682=DIRECTION('',(0.,0.,-1.));
#36683=DIRECTION('center_axis',(0.,0.,1.));
#36684=DIRECTION('ref_axis',(5.30947313395831E-16,1.,0.));
#36685=DIRECTION('',(0.,0.,-1.));
#36686=DIRECTION('center_axis',(0.,0.,1.));
#36687=DIRECTION('ref_axis',(5.30947313395831E-16,1.,0.));
#36688=DIRECTION('',(0.,0.,-1.));
#36689=DIRECTION('center_axis',(0.,0.,1.));
#36690=DIRECTION('ref_axis',(5.30947313395831E-16,1.,0.));
#36691=DIRECTION('',(0.,0.,-1.));
#36692=DIRECTION('center_axis',(0.,0.,1.));
#36693=DIRECTION('ref_axis',(5.30947313395831E-16,1.,0.));
#36694=DIRECTION('',(0.,0.,-1.));
#36695=DIRECTION('center_axis',(0.,0.,1.));
#36696=DIRECTION('ref_axis',(5.30947313395831E-16,1.,0.));
#36697=DIRECTION('',(0.,0.,-1.));
#36698=DIRECTION('center_axis',(0.,0.,1.));
#36699=DIRECTION('ref_axis',(5.30947313395831E-16,1.,0.));
#36700=DIRECTION('',(0.,0.,-1.));
#36701=DIRECTION('center_axis',(0.,0.,1.));
#36702=DIRECTION('ref_axis',(5.30947313395831E-16,1.,0.));
#36703=DIRECTION('',(0.,0.,-1.));
#36704=DIRECTION('center_axis',(0.,0.,1.));
#36705=DIRECTION('ref_axis',(5.30947313395831E-16,1.,0.));
#36706=DIRECTION('',(0.,0.,-1.));
#36707=DIRECTION('center_axis',(0.,0.,1.));
#36708=DIRECTION('ref_axis',(5.30947313395831E-16,1.,0.));
#36709=DIRECTION('',(0.,0.,-1.));
#36710=DIRECTION('center_axis',(0.,0.,1.));
#36711=DIRECTION('ref_axis',(5.30947313395831E-16,1.,0.));
#36712=DIRECTION('',(0.,0.,-1.));
#36713=DIRECTION('center_axis',(0.,0.,1.));
#36714=DIRECTION('ref_axis',(5.30947313395831E-16,1.,0.));
#36715=DIRECTION('',(0.,0.,-1.));
#36716=DIRECTION('center_axis',(0.,0.,1.));
#36717=DIRECTION('ref_axis',(5.30947313395831E-16,1.,0.));
#36718=DIRECTION('',(0.,0.,-1.));
#36719=DIRECTION('center_axis',(0.,0.,1.));
#36720=DIRECTION('ref_axis',(5.30947313395831E-16,1.,0.));
#36721=DIRECTION('',(0.,0.,-1.));
#36722=DIRECTION('center_axis',(0.,0.,1.));
#36723=DIRECTION('ref_axis',(5.30947313395831E-16,1.,0.));
#36724=DIRECTION('',(0.,0.,-1.));
#36725=DIRECTION('center_axis',(0.,0.,1.));
#36726=DIRECTION('ref_axis',(5.30947313395831E-16,1.,0.));
#36727=DIRECTION('',(0.,0.,-1.));
#36728=DIRECTION('center_axis',(0.,0.,1.));
#36729=DIRECTION('ref_axis',(5.30947313395831E-16,1.,0.));
#36730=DIRECTION('',(0.,0.,-1.));
#36731=DIRECTION('center_axis',(0.,0.,1.));
#36732=DIRECTION('ref_axis',(5.30947313395831E-16,1.,0.));
#36733=DIRECTION('',(0.,0.,-1.));
#36734=DIRECTION('center_axis',(0.,0.,1.));
#36735=DIRECTION('ref_axis',(5.30947313395831E-16,1.,0.));
#36736=DIRECTION('',(0.,0.,-1.));
#36737=DIRECTION('center_axis',(0.,0.,1.));
#36738=DIRECTION('ref_axis',(5.30947313395831E-16,1.,0.));
#36739=DIRECTION('',(0.,0.,-1.));
#36740=DIRECTION('center_axis',(0.,0.,1.));
#36741=DIRECTION('ref_axis',(5.30947313395831E-16,1.,0.));
#36742=DIRECTION('',(0.,0.,-1.));
#36743=DIRECTION('center_axis',(0.,0.,1.));
#36744=DIRECTION('ref_axis',(5.30947313395831E-16,1.,0.));
#36745=DIRECTION('',(0.,0.,-1.));
#36746=DIRECTION('center_axis',(0.,0.,1.));
#36747=DIRECTION('ref_axis',(5.30947313395831E-16,1.,0.));
#36748=DIRECTION('center_axis',(0.,0.,1.));
#36749=DIRECTION('ref_axis',(0.700629269222058,-0.7135254915624,0.));
#36750=DIRECTION('center_axis',(-5.15167520928809E-67,1.18789542670764E-48,
1.));
#36751=DIRECTION('ref_axis',(4.33680868994202E-19,-1.,1.18789542670764E-48));
#36752=DIRECTION('center_axis',(5.15167520928809E-67,-1.18789542670764E-48,
-1.));
#36753=DIRECTION('ref_axis',(-4.33680868994202E-19,1.,-1.18789542670764E-48));
#36754=DIRECTION('center_axis',(5.15167520928809E-67,-1.18789542670764E-48,
-1.));
#36755=DIRECTION('ref_axis',(-4.33680868994202E-19,1.,-1.18789542670764E-48));
#36756=DIRECTION('center_axis',(5.15167520928809E-67,-1.18789542670764E-48,
-1.));
#36757=DIRECTION('ref_axis',(-4.33680868994202E-19,1.,-1.18789542670764E-48));
#36758=DIRECTION('center_axis',(1.09747227149895E-48,7.33307527524356E-49,
1.));
#36759=DIRECTION('ref_axis',(1.,4.33680868994202E-19,-1.09747227149895E-48));
#36760=DIRECTION('center_axis',(-0.654448706060852,0.271081529927754,-0.705841126081008));
#36761=DIRECTION('ref_axis',(0.652112169591586,-0.270113704831613,-0.708370174931649));
#36762=DIRECTION('',(1.09747227149895E-48,7.33307527524356E-49,1.));
#36763=DIRECTION('center_axis',(-0.654448706060939,0.271081529927973,0.705841126080843));
#36764=DIRECTION('ref_axis',(0.652112169592024,-0.270113704830126,0.708370174931813));
#36765=DIRECTION('',(1.09747227149895E-48,7.33307527524356E-49,1.));
#36766=DIRECTION('center_axis',(1.12975568624751E-48,8.20815552314688E-49,
1.));
#36767=DIRECTION('ref_axis',(1.,4.33680868994202E-19,-1.12975568624751E-48));
#36768=DIRECTION('center_axis',(-0.673700070814156,0.218898422362917,-0.705841126084352));
#36769=DIRECTION('ref_axis',(0.671294802430975,-0.218116903290839,-0.708370174928316));
#36770=DIRECTION('',(1.12975568624751E-48,8.20815552314688E-49,1.));
#36771=DIRECTION('center_axis',(-0.673700070814201,0.218898422363249,0.705841126084207));
#36772=DIRECTION('ref_axis',(0.671294802430673,-0.218116903291296,0.708370174928462));
#36773=DIRECTION('',(1.12975568624751E-48,8.20815552314688E-49,1.));
#36774=DIRECTION('center_axis',(1.15507378150847E-48,9.10586746597098E-49,
1.));
#36775=DIRECTION('ref_axis',(1.,4.33680868994202E-19,-1.15507378150847E-48));
#36776=DIRECTION('center_axis',(-0.688797850611722,0.165365733230951,-0.705841126079843));
#36777=DIRECTION('ref_axis',(0.686338679579581,-0.164775338502517,-0.708370174932809));
#36778=DIRECTION('',(1.15507378150847E-48,9.10586746597098E-49,1.));
#36779=DIRECTION('center_axis',(-0.688797850609436,0.165365733233163,0.705841126081556));
#36780=DIRECTION('ref_axis',(0.68633867958204,-0.164775338499612,0.708370174931102));
#36781=DIRECTION('',(1.15507378150847E-48,9.10586746597098E-49,1.));
#36782=DIRECTION('center_axis',(1.17327046280542E-48,1.00206764110688E-48,
1.));
#36783=DIRECTION('ref_axis',(1.,4.33680868994202E-19,-1.17327046280542E-48));
#36784=DIRECTION('center_axis',(-0.699648962604041,0.110813509366852,-0.705841126082132));
#36785=DIRECTION('ref_axis',(0.697151050543932,-0.11041787896162,-0.708370174930529));
#36786=DIRECTION('',(1.17327046280542E-48,1.00206764110688E-48,1.));
#36787=DIRECTION('center_axis',(-0.699648962604175,0.110813509367011,0.705841126081974));
#36788=DIRECTION('ref_axis',(0.697151050543496,-0.110417878963368,0.708370174930686));
#36789=DIRECTION('',(1.17327046280542E-48,1.00206764110688E-48,1.));
#36790=DIRECTION('center_axis',(1.18423354154716E-48,1.09469422570891E-48,
1.));
#36791=DIRECTION('ref_axis',(1.,4.33680868994202E-19,-1.18423354154716E-48));
#36792=DIRECTION('center_axis',(-0.706186506088737,0.0555780833649064,-0.705841126081264));
#36793=DIRECTION('ref_axis',(0.703665253451942,-0.0553796564821394,-0.708370174931394));
#36794=DIRECTION('',(1.18423354154716E-48,1.09469422570891E-48,1.));
#36795=DIRECTION('center_axis',(-0.706186506088284,0.0555780833648712,0.705841126081719));
#36796=DIRECTION('ref_axis',(0.703665253452317,-0.0553796564831855,0.70837017493094));
#36797=DIRECTION('',(1.18423354154716E-48,1.09469422570891E-48,1.));
#36798=DIRECTION('center_axis',(1.18789542670764E-48,1.18789542670763E-48,
1.));
#36799=DIRECTION('ref_axis',(1.,4.33680868994202E-19,-1.18789542670764E-48));
#36800=DIRECTION('center_axis',(-0.70837017493089,-1.25340662871076E-13,
-0.70584112608177));
#36801=DIRECTION('ref_axis',(0.70584112608177,-2.88506822019813E-13,-0.708370174930889));
#36802=DIRECTION('',(1.18789542670764E-48,1.18789542670763E-48,1.));
#36803=DIRECTION('center_axis',(-0.70837017493089,1.25340662871076E-13,
0.70584112608177));
#36804=DIRECTION('ref_axis',(0.70584112608177,2.61497947465894E-13,0.708370174930889));
#36805=DIRECTION('',(1.18789542670764E-48,1.18789542670763E-48,1.));
#36806=DIRECTION('center_axis',(1.05842257525003E-48,6.48602188298306E-49,
1.));
#36807=DIRECTION('ref_axis',(1.,4.33680868994202E-19,-1.05842257525003E-48));
#36808=DIRECTION('center_axis',(-0.631162447404585,0.321593329715507,-0.70584112608203));
#36809=DIRECTION('ref_axis',(0.628909048379288,-0.320445165567225,-0.708370174930631));
#36810=DIRECTION('',(1.05842257525003E-48,6.48602188298306E-49,1.));
#36811=DIRECTION('center_axis',(-0.631162447404969,0.32159332971786,0.705841126080614));
#36812=DIRECTION('ref_axis',(0.628909048378923,-0.320445165564824,0.708370174932041));
#36813=DIRECTION('',(1.05842257525003E-48,6.48602188298306E-49,1.));
#36814=DIRECTION('center_axis',(1.01284735186347E-48,5.67221771220248E-49,
1.));
#36815=DIRECTION('ref_axis',(1.,4.33680868994202E-19,-1.01284735186347E-48));
#36816=DIRECTION('center_axis',(-0.603984862377595,0.370122399687911,-0.705841126081486));
#36817=DIRECTION('ref_axis',(0.601828493750374,-0.368800975294447,-0.708370174931173));
#36818=DIRECTION('',(1.01284735186347E-48,5.67221771220248E-49,1.));
#36819=DIRECTION('center_axis',(-0.603984862377492,0.370122399687834,0.705841126081615));
#36820=DIRECTION('ref_axis',(0.60182849375054,-0.368800975294424,0.708370174931044));
#36821=DIRECTION('',(1.01284735186347E-48,5.67221771220248E-49,1.));
#36822=DIRECTION('center_axis',(9.61027587746754E-49,4.89668013623204E-49,
1.));
#36823=DIRECTION('ref_axis',(1.,4.33680868994202E-19,-9.61027587746754E-49));
#36824=DIRECTION('center_axis',(-0.57308350982942,0.416369541987989,-0.705841126080299));
#36825=DIRECTION('ref_axis',(-0.571037466327478,0.414883004371834,0.708370174932355));
#36826=DIRECTION('',(9.61027587746754E-49,4.89668013623204E-49,1.));
#36827=DIRECTION('center_axis',(-0.573083509826005,0.416369541988967,0.705841126082495));
#36828=DIRECTION('ref_axis',(0.571037466331126,-0.41488300437055,0.708370174930167));
#36829=DIRECTION('',(9.61027587746754E-49,4.89668013623204E-49,1.));
#36830=DIRECTION('center_axis',(9.03282768977476E-49,4.16419060212002E-49,
1.));
#36831=DIRECTION('ref_axis',(1.,4.33680868994202E-19,-9.03282768977476E-49));
#36832=DIRECTION('center_axis',(-0.538648906869708,0.460049627603881,-0.705841126082633));
#36833=DIRECTION('ref_axis',(-0.536725803041031,0.458407141763258,0.70837017493003));
#36834=DIRECTION('',(9.03282768977476E-49,4.16419060212002E-49,1.));
#36835=DIRECTION('center_axis',(-0.53864890686968,0.460049627604191,0.705841126082452));
#36836=DIRECTION('ref_axis',(0.536725803040381,-0.45840714176374,0.70837017493021));
#36837=DIRECTION('',(9.03282768977476E-49,4.16419060212002E-49,1.));
#36838=DIRECTION('center_axis',(8.39968911565451E-49,3.47926515142171E-49,
1.));
#36839=DIRECTION('ref_axis',(1.,4.33680868994202E-19,-8.39968911565451E-49));
#36840=DIRECTION('center_axis',(-0.500893354284786,0.500893354283015,-0.705841126081816));
#36841=DIRECTION('ref_axis',(-0.499105046691526,0.499105046694076,0.708370174930843));
#36842=DIRECTION('',(8.39968911565451E-49,3.47926515142171E-49,1.));
#36843=DIRECTION('center_axis',(-0.500893354285066,0.500893354283687,0.70584112608114));
#36844=DIRECTION('ref_axis',(0.49910504669045,-0.499105046694196,0.708370174931517));
#36845=DIRECTION('',(8.39968911565451E-49,3.47926515142171E-49,1.));
#36846=DIRECTION('center_axis',(7.71476366495618E-49,2.84612657730147E-49,
1.));
#36847=DIRECTION('ref_axis',(1.,4.33680868994202E-19,-7.71476366495618E-49));
#36848=DIRECTION('center_axis',(-0.460049627606723,0.538648906869542,-0.705841126080907));
#36849=DIRECTION('ref_axis',(-0.458407141764148,0.536725803038001,0.708370174931749));
#36850=DIRECTION('',(7.71476366495618E-49,2.84612657730147E-49,1.));
#36851=DIRECTION('center_axis',(-0.460049627603276,0.538648906871872,0.705841126081376));
#36852=DIRECTION('ref_axis',(0.458407141768044,-0.53672580303529,0.708370174931282));
#36853=DIRECTION('',(7.71476366495618E-49,2.84612657730147E-49,1.));
#36854=DIRECTION('center_axis',(6.98227413084414E-49,2.26867838960871E-49,
1.));
#36855=DIRECTION('ref_axis',(1.,4.33680868994202E-19,-6.98227413084414E-49));
#36856=DIRECTION('center_axis',(-0.416369541989573,0.573083509826983,-0.705841126081344));
#36857=DIRECTION('ref_axis',(-0.414883004369422,0.571037466330522,0.708370174931314));
#36858=DIRECTION('',(6.98227413084414E-49,2.26867838960871E-49,1.));
#36859=DIRECTION('center_axis',(-0.416369541986537,0.573083509827722,0.705841126082535));
#36860=DIRECTION('ref_axis',(0.414883004374377,-0.571037466328393,0.708370174930127));
#36861=DIRECTION('',(6.98227413084414E-49,2.26867838960871E-49,1.));
#36862=DIRECTION('center_axis',(6.2067365548737E-49,1.75048074844156E-49,
1.));
#36863=DIRECTION('ref_axis',(1.,4.33680868994202E-19,-6.2067365548737E-49));
#36864=DIRECTION('center_axis',(-0.370122399687787,0.603984862376041,-0.70584112608288));
#36865=DIRECTION('ref_axis',(-0.368800975294937,0.60182849375171,0.708370174929783));
#36866=DIRECTION('',(6.2067365548737E-49,1.75048074844156E-49,1.));
#36867=DIRECTION('center_axis',(-0.370122399687792,0.603984862376936,0.705841126082112));
#36868=DIRECTION('ref_axis',(0.368800975294942,-0.601828493750806,0.708370174930549));
#36869=DIRECTION('',(6.2067365548737E-49,1.75048074844156E-49,1.));
#36870=DIRECTION('center_axis',(5.39293238409311E-49,1.29472851457601E-49,
1.));
#36871=DIRECTION('ref_axis',(1.,4.33680868994202E-19,-5.39293238409311E-49));
#36872=DIRECTION('center_axis',(-0.321593329717153,0.63116244740346,-0.705841126082286));
#36873=DIRECTION('ref_axis',(-0.320445165567263,0.628909048379556,0.708370174930376));
#36874=DIRECTION('',(5.39293238409311E-49,1.29472851457601E-49,1.));
#36875=DIRECTION('center_axis',(-0.321593329716558,0.631162447403966,0.705841126082104));
#36876=DIRECTION('ref_axis',(0.320445165566995,-0.628909048379489,0.708370174930556));
#36877=DIRECTION('',(5.39293238409311E-49,1.29472851457601E-49,1.));
#36878=DIRECTION('center_axis',(0.,0.,1.));
#36879=DIRECTION('ref_axis',(1.,4.33680868994202E-19,0.));
#36880=DIRECTION('',(-0.707106781186549,-8.69022643068862E-17,0.707106781186546));
#36881=DIRECTION('center_axis',(0.,0.,1.));
#36882=DIRECTION('ref_axis',(1.,4.33680868994202E-19,0.));
#36883=DIRECTION('center_axis',(5.15167520928809E-67,-1.18789542670764E-48,
-1.));
#36884=DIRECTION('ref_axis',(0.,1.,0.));
#36885=DIRECTION('center_axis',(5.15167520928809E-67,-1.18789542670764E-48,
-1.));
#36886=DIRECTION('ref_axis',(-4.33680868994202E-19,1.,-1.18789542670764E-48));
#36887=DIRECTION('center_axis',(-1.,0.,-5.15167520928809E-67));
#36888=DIRECTION('ref_axis',(0.,-1.,0.));
#36889=DIRECTION('center_axis',(5.15167520928809E-67,-1.18789542670764E-48,
-1.));
#36890=DIRECTION('ref_axis',(-4.33680868994202E-19,1.,-1.18789542670764E-48));
#36891=DIRECTION('center_axis',(5.15167520928809E-67,-1.18789542670764E-48,
-1.));
#36892=DIRECTION('ref_axis',(-4.33680868994202E-19,1.,-1.18789542670764E-48));
#36893=DIRECTION('center_axis',(5.15167520928809E-67,-1.18789542670764E-48,
-1.));
#36894=DIRECTION('ref_axis',(-4.33680868994202E-19,1.,-1.18789542670764E-48));
#36895=DIRECTION('center_axis',(0.0555758110363288,-0.706157633406642,0.705870190622316));
#36896=DIRECTION('ref_axis',(0.0553775799352608,-0.703694571287346,-0.708341212962532));
#36897=DIRECTION('center_axis',(5.15167520928809E-67,-1.18789542670764E-48,
-1.));
#36898=DIRECTION('ref_axis',(-4.33680868994202E-19,1.,-1.18789542670764E-48));
#36899=DIRECTION('center_axis',(0.11080862020158,-0.699618093636883,0.705872490429338));
#36900=DIRECTION('ref_axis',(0.110419233095995,-0.697182591373234,-0.708338921173046));
#36901=DIRECTION('center_axis',(5.15167520928809E-67,-1.18789542670764E-48,
-1.));
#36902=DIRECTION('ref_axis',(-4.33680868994202E-19,1.,-1.18789542670764E-48));
#36903=DIRECTION('center_axis',(0.165358045050138,-0.688765827029971,0.705874176077378));
#36904=DIRECTION('ref_axis',(0.164780094681068,-0.686371526838389,-0.708337241391723));
#36905=DIRECTION('center_axis',(5.15167520928809E-67,-1.18789542670764E-48,
-1.));
#36906=DIRECTION('ref_axis',(-4.33680868994202E-19,1.,-1.18789542670764E-48));
#36907=DIRECTION('center_axis',(0.218887852522913,-0.673667540197498,0.705875451692549));
#36908=DIRECTION('ref_axis',(0.218125006053852,-0.671328261761447,-0.708335970210719));
#36909=DIRECTION('center_axis',(5.15167520928809E-67,-1.18789542670764E-48,
-1.));
#36910=DIRECTION('ref_axis',(-4.33680868994202E-19,1.,-1.18789542670764E-48));
#36911=DIRECTION('center_axis',(0.271068063822855,-0.654416196007407,0.705876439030603));
#36912=DIRECTION('ref_axis',(0.270125073931967,-0.65214568281518,-0.708334986301518));
#36913=DIRECTION('center_axis',(5.15167520928809E-67,-1.18789542670764E-48,
-1.));
#36914=DIRECTION('ref_axis',(-4.33680868994202E-19,1.,-1.18789542670764E-48));
#36915=DIRECTION('center_axis',(0.321577003370555,-0.631130405143931,0.705877214964523));
#36916=DIRECTION('ref_axis',(0.320459697262731,-0.628942147608601,-0.708334213060304));
#36917=DIRECTION('center_axis',(5.15167520928809E-67,-1.18789542670764E-48,
-1.));
#36918=DIRECTION('ref_axis',(-4.33680868994202E-19,1.,-1.18789542670764E-48));
#36919=DIRECTION('center_axis',(0.370103289326652,-0.603953677099404,0.705877830185721));
#36920=DIRECTION('ref_axis',(0.368818543504099,-0.601860775526205,-0.708333599972859));
#36921=DIRECTION('center_axis',(5.15167520928809E-67,-1.18789542670764E-48,
-1.));
#36922=DIRECTION('ref_axis',(-4.33680868994202E-19,1.,-1.18789542670764E-48));
#36923=DIRECTION('center_axis',(0.416347757295498,-0.573053525770462,0.705878319256975));
#36924=DIRECTION('ref_axis',(0.414903461782555,-0.571068576441932,-0.708333112597058));
#36925=DIRECTION('center_axis',(5.15167520928809E-67,-1.18789542670764E-48,
-1.));
#36926=DIRECTION('ref_axis',(-4.33680868994202E-19,1.,-1.18789542670764E-48));
#36927=DIRECTION('center_axis',(0.460025307051016,-0.538620431161506,0.705878706300177));
#36928=DIRECTION('ref_axis',(0.458430320957564,-0.536755427393206,-0.708332726895123));
#36929=DIRECTION('center_axis',(5.15167520928809E-67,-1.18789542670764E-48,
-1.));
#36930=DIRECTION('ref_axis',(-4.33680868994202E-19,1.,-1.18789542670764E-48));
#36931=DIRECTION('center_axis',(0.500866661619323,-0.500866661619323,0.705879008440277));
#36932=DIRECTION('ref_axis',(0.499130761357991,-0.499132905771573,-0.708332425801768));
#36933=DIRECTION('center_axis',(5.15167520928809E-67,-1.18789542670764E-48,
-1.));
#36934=DIRECTION('ref_axis',(-4.33680868994202E-19,1.,-1.18789542670764E-48));
#36935=DIRECTION('center_axis',(0.53862002836901,-0.46002496303376,0.705879237848482));
#36936=DIRECTION('ref_axis',(0.536753849182443,-0.458432987266868,-0.708332197188161));
#36937=DIRECTION('center_axis',(5.15167520928809E-67,-1.18789542670764E-48,
-1.));
#36938=DIRECTION('ref_axis',(-4.33680868994202E-19,1.,-1.18789542670764E-48));
#36939=DIRECTION('center_axis',(0.573052651970297,-0.416347122442612,0.705879403087785));
#36940=DIRECTION('ref_axis',(0.571067623542823,-0.414906617259439,-0.708332032521106));
#36941=DIRECTION('center_axis',(5.15167520928809E-67,-1.18789542670764E-48,
-1.));
#36942=DIRECTION('ref_axis',(-4.33680868994202E-19,1.,-1.18789542670764E-48));
#36943=DIRECTION('center_axis',(0.603952249837211,-0.370102414699222,0.705879509938047));
#36944=DIRECTION('ref_axis',(0.601860526500507,-0.368822164724135,-0.708331926040847));
#36945=DIRECTION('center_axis',(5.15167520928809E-67,-1.18789542670764E-48,
-1.));
#36946=DIRECTION('ref_axis',(-4.33680868994202E-19,1.,-1.18789542670764E-48));
#36947=DIRECTION('center_axis',(0.631128321247012,-0.321575941572045,0.705879561909807));
#36948=DIRECTION('ref_axis',(0.628942707293582,-0.320463768412346,-0.708331874249054));
#36949=DIRECTION('center_axis',(5.15167520928809E-67,-1.18789542670764E-48,
-1.));
#36950=DIRECTION('ref_axis',(-4.33680868994202E-19,1.,-1.18789542670764E-48));
#36951=DIRECTION('center_axis',(0.654413322126613,-0.271066873422487,0.70587956051735));
#36952=DIRECTION('ref_axis',(0.652147192704133,-0.270129585579022,-0.708331875636714));
#36953=DIRECTION('center_axis',(5.15167520928809E-67,-1.18789542670764E-48,
-1.));
#36954=DIRECTION('ref_axis',(-4.33680868994202E-19,1.,-1.18789542670764E-48));
#36955=DIRECTION('center_axis',(0.673663698306673,-0.218886604216949,0.705879505353533));
#36956=DIRECTION('ref_axis',(0.671330916306432,-0.218129954133086,-0.708331930609559));
#36957=DIRECTION('center_axis',(5.15167520928809E-67,-1.18789542670764E-48,
-1.));
#36958=DIRECTION('ref_axis',(-4.33680868994202E-19,1.,-1.18789542670764E-48));
#36959=DIRECTION('center_axis',(0.688760770927107,-0.165356831187235,0.705879393955946));
#36960=DIRECTION('ref_axis',(0.686375600198304,-0.164785479532649,-0.708332041621451));
#36961=DIRECTION('center_axis',(5.15167520928809E-67,-1.18789542670764E-48,
-1.));
#36962=DIRECTION('ref_axis',(-4.33680868994202E-19,1.,-1.18789542670764E-48));
#36963=DIRECTION('center_axis',(0.699611468639781,-0.110807570905153,0.705879221381242));
#36964=DIRECTION('ref_axis',(0.697188483633051,-0.110425058152577,-0.708332213598567));
#36965=DIRECTION('center_axis',(5.15167520928809E-67,-1.18789542670764E-48,
-1.));
#36966=DIRECTION('ref_axis',(-4.33680868994202E-19,1.,-1.18789542670764E-48));
#36967=DIRECTION('center_axis',(0.706148902304913,-0.0555751238837372,0.705878979272562));
#36968=DIRECTION('ref_axis',(0.703702893729778,-0.0553838490533553,-0.708332454868737));
#36969=DIRECTION('center_axis',(5.15167520928809E-67,-1.18789542670764E-48,
-1.));
#36970=DIRECTION('ref_axis',(-4.33680868994202E-19,1.,-1.18789542670764E-48));
#36971=DIRECTION('center_axis',(0.708332577472403,3.07190287735134E-19,
0.705878856243267));
#36972=DIRECTION('ref_axis',(0.705878856242412,-1.55615277571261E-6,-0.708332577471545));
#36973=DIRECTION('center_axis',(5.15167520928809E-67,-1.18789542670764E-48,
-1.));
#36974=DIRECTION('ref_axis',(-4.33680868994202E-19,1.,-1.18789542670764E-48));
#36975=DIRECTION('center_axis',(0.706157633406551,0.0555758110364317,0.705870190622399));
#36976=DIRECTION('ref_axis',(0.703694571287442,0.0553775799351074,-0.70834121296245));
#36977=DIRECTION('center_axis',(5.15167520928809E-67,-1.18789542670764E-48,
-1.));
#36978=DIRECTION('ref_axis',(-4.33680868994202E-19,1.,-1.18789542670764E-48));
#36979=DIRECTION('center_axis',(0.699618093637069,0.110808620201609,0.705872490429149));
#36980=DIRECTION('ref_axis',(0.697182591372912,0.11041923309682,-0.708338921173234));
#36981=DIRECTION('center_axis',(5.15167520928809E-67,-1.18789542670764E-48,
-1.));
#36982=DIRECTION('ref_axis',(-4.33680868994202E-19,1.,-1.18789542670764E-48));
#36983=DIRECTION('center_axis',(0.688765827030135,0.165358045050174,0.705874176077209));
#36984=DIRECTION('ref_axis',(0.686371526838244,0.16478009468095,-0.708337241391891));
#36985=DIRECTION('center_axis',(5.15167520928809E-67,-1.18789542670764E-48,
-1.));
#36986=DIRECTION('ref_axis',(-4.33680868994202E-19,1.,-1.18789542670764E-48));
#36987=DIRECTION('center_axis',(0.673667540197388,0.21888785252289,0.705875451692661));
#36988=DIRECTION('ref_axis',(0.671328261761852,0.21812500605297,-0.708335970210607));
#36989=DIRECTION('center_axis',(5.15167520928809E-67,-1.18789542670764E-48,
-1.));
#36990=DIRECTION('ref_axis',(-4.33680868994202E-19,1.,-1.18789542670764E-48));
#36991=DIRECTION('center_axis',(0.654416196007382,0.271068063822859,0.705876439030624));
#36992=DIRECTION('ref_axis',(0.652145682814771,0.270125073933009,-0.708334986301497));
#36993=DIRECTION('center_axis',(5.15167520928809E-67,-1.18789542670764E-48,
-1.));
#36994=DIRECTION('ref_axis',(-4.33680868994202E-19,1.,-1.18789542670764E-48));
#36995=DIRECTION('center_axis',(0.631130405143941,0.321577003370555,0.705877214964514));
#36996=DIRECTION('ref_axis',(0.628942147608526,0.320459697262857,-0.708334213060313));
#36997=DIRECTION('center_axis',(5.15167520928809E-67,-1.18789542670764E-48,
-1.));
#36998=DIRECTION('ref_axis',(-4.33680868994202E-19,1.,-1.18789542670764E-48));
#36999=DIRECTION('center_axis',(0.603953677099555,0.370103289326611,0.705877830185613));
#37000=DIRECTION('ref_axis',(0.601860775525942,0.368818543504321,-0.708333599972967));
#37001=DIRECTION('center_axis',(5.15167520928809E-67,-1.18789542670764E-48,
-1.));
#37002=DIRECTION('ref_axis',(-4.33680868994202E-19,1.,-1.18789542670764E-48));
#37003=DIRECTION('center_axis',(0.573053525770564,0.41634775729573,0.705878319256755));
#37004=DIRECTION('ref_axis',(-0.571068576442187,-0.414903461781831,0.708333112597277));
#37005=DIRECTION('center_axis',(5.15167520928809E-67,-1.18789542670764E-48,
-1.));
#37006=DIRECTION('ref_axis',(-4.33680868994202E-19,1.,-1.18789542670764E-48));
#37007=DIRECTION('center_axis',(0.538620431161647,0.46002530705115,0.705878706299982));
#37008=DIRECTION('ref_axis',(-0.536755427393011,-0.458430320957492,0.708332726895318));
#37009=DIRECTION('center_axis',(5.15167520928809E-67,-1.18789542670764E-48,
-1.));
#37010=DIRECTION('ref_axis',(-4.33680868994202E-19,1.,-1.18789542670764E-48));
#37011=DIRECTION('center_axis',(0.500866661619527,0.500866661619527,0.705879008439988));
#37012=DIRECTION('ref_axis',(-0.49913290577155,-0.499130761357605,0.708332425802057));
#37013=DIRECTION('center_axis',(5.15167520928809E-67,-1.18789542670764E-48,
-1.));
#37014=DIRECTION('ref_axis',(-4.33680868994202E-19,1.,-1.18789542670764E-48));
#37015=DIRECTION('center_axis',(0.460024963033642,0.538620028368862,0.705879237848672));
#37016=DIRECTION('ref_axis',(-0.45843298726639,-0.536753849183101,0.708332197187972));
#37017=DIRECTION('center_axis',(5.15167520928809E-67,-1.18789542670764E-48,
-1.));
#37018=DIRECTION('ref_axis',(-4.33680868994202E-19,1.,-1.18789542670764E-48));
#37019=DIRECTION('center_axis',(0.416347122442686,0.573052651970292,0.705879403087744));
#37020=DIRECTION('ref_axis',(-0.414906617258984,-0.571067623543104,0.708332032521146));
#37021=DIRECTION('center_axis',(5.15167520928809E-67,-1.18789542670764E-48,
-1.));
#37022=DIRECTION('ref_axis',(-4.33680868994202E-19,1.,-1.18789542670764E-48));
#37023=DIRECTION('center_axis',(0.370102414699172,0.603952249837277,0.705879509938016));
#37024=DIRECTION('ref_axis',(-0.368822164724246,-0.601860526500403,0.708331926040877));
#37025=DIRECTION('center_axis',(5.15167520928809E-67,-1.18789542670764E-48,
-1.));
#37026=DIRECTION('ref_axis',(-4.33680868994202E-19,1.,-1.18789542670764E-48));
#37027=DIRECTION('center_axis',(0.321575941571924,0.631128321246917,0.705879561909948));
#37028=DIRECTION('ref_axis',(-0.320463768412656,-0.628942707293582,0.708331874248914));
#37029=DIRECTION('center_axis',(5.15167520928809E-67,-1.18789542670764E-48,
-1.));
#37030=DIRECTION('ref_axis',(-4.33680868994202E-19,1.,-1.18789542670764E-48));
#37031=DIRECTION('center_axis',(0.271066873422485,0.654413322126598,0.705879560517365));
#37032=DIRECTION('ref_axis',(-0.270129585579224,-0.652147192704065,0.708331875636699));
#37033=DIRECTION('center_axis',(5.15167520928809E-67,-1.18789542670764E-48,
-1.));
#37034=DIRECTION('ref_axis',(-4.33680868994202E-19,1.,-1.18789542670764E-48));
#37035=DIRECTION('center_axis',(0.218886604216952,0.67366369830668,0.705879505353526));
#37036=DIRECTION('ref_axis',(-0.218129954132996,-0.671330916306453,0.708331930609566));
#37037=DIRECTION('center_axis',(5.15167520928809E-67,-1.18789542670764E-48,
-1.));
#37038=DIRECTION('ref_axis',(-4.33680868994202E-19,1.,-1.18789542670764E-48));
#37039=DIRECTION('center_axis',(0.16535683118711,0.68876077092705,0.705879393956031));
#37040=DIRECTION('ref_axis',(-0.164785479532882,-0.686375600198336,0.708332041621366));
#37041=DIRECTION('center_axis',(5.15167520928809E-67,-1.18789542670764E-48,
-1.));
#37042=DIRECTION('ref_axis',(-4.33680868994202E-19,1.,-1.18789542670764E-48));
#37043=DIRECTION('center_axis',(0.110807570905159,0.699611468639805,0.705879221381218));
#37044=DIRECTION('ref_axis',(-0.11042505815257,-0.697188483633028,0.708332213598592));
#37045=DIRECTION('center_axis',(5.15167520928809E-67,-1.18789542670764E-48,
-1.));
#37046=DIRECTION('ref_axis',(-4.33680868994202E-19,1.,-1.18789542670764E-48));
#37047=DIRECTION('center_axis',(0.055575123883674,0.706148902304893,0.705878979272587));
#37048=DIRECTION('ref_axis',(-0.0553838490533958,-0.7037028937298,0.708332454868712));
#37049=DIRECTION('center_axis',(5.15167520928809E-67,-1.18789542670764E-48,
-1.));
#37050=DIRECTION('ref_axis',(-4.33680868994202E-19,1.,-1.18789542670764E-48));
#37051=DIRECTION('center_axis',(4.84352581305682E-13,0.70837017493119,0.705841126081468));
#37052=DIRECTION('ref_axis',(-1.41156745807278E-12,-0.705841126081468,0.70837017493119));
#37053=DIRECTION('center_axis',(5.15167520928809E-67,-1.18789542670764E-48,
-1.));
#37054=DIRECTION('ref_axis',(-4.33680868994202E-19,1.,-1.18789542670764E-48));
#37055=DIRECTION('center_axis',(-0.0555758110363152,0.706157633406656,0.705870190622303));
#37056=DIRECTION('ref_axis',(0.0553775799350914,-0.703694571287347,0.708341212962545));
#37057=DIRECTION('center_axis',(5.15167520928809E-67,-1.18789542670764E-48,
-1.));
#37058=DIRECTION('ref_axis',(-4.33680868994202E-19,1.,-1.18789542670764E-48));
#37059=DIRECTION('center_axis',(-0.110808620201596,0.699618093636976,0.705872490429243));
#37060=DIRECTION('ref_axis',(0.11041923309583,-0.697182591373165,0.70833892117314));
#37061=DIRECTION('center_axis',(5.15167520928809E-67,-1.18789542670764E-48,
-1.));
#37062=DIRECTION('ref_axis',(-4.33680868994202E-19,1.,-1.18789542670764E-48));
#37063=DIRECTION('center_axis',(-0.165358045050154,0.688765827030126,0.705874176077223));
#37064=DIRECTION('ref_axis',(0.164780094680844,-0.686371526838284,0.708337241391878));
#37065=DIRECTION('center_axis',(5.15167520928809E-67,-1.18789542670764E-48,
-1.));
#37066=DIRECTION('ref_axis',(-4.33680868994202E-19,1.,-1.18789542670764E-48));
#37067=DIRECTION('center_axis',(-0.218887852522867,0.673667540197309,0.705875451692744));
#37068=DIRECTION('ref_axis',(0.218125006054104,-0.67132826176157,0.708335970210525));
#37069=DIRECTION('center_axis',(5.15167520928809E-67,-1.18789542670764E-48,
-1.));
#37070=DIRECTION('ref_axis',(-4.33680868994202E-19,1.,-1.18789542670764E-48));
#37071=DIRECTION('center_axis',(-0.271068063822887,0.654416196007496,0.705876439030507));
#37072=DIRECTION('ref_axis',(0.270125073932604,-0.652145682814813,0.708334986301614));
#37073=DIRECTION('center_axis',(5.15167520928809E-67,-1.18789542670764E-48,
-1.));
#37074=DIRECTION('ref_axis',(-4.33680868994202E-19,1.,-1.18789542670764E-48));
#37075=DIRECTION('center_axis',(5.15167520928809E-67,-1.18789542670764E-48,
-1.));
#37076=DIRECTION('ref_axis',(-4.33680868994202E-19,1.,-1.18789542670764E-48));
#37077=DIRECTION('center_axis',(5.15167520928809E-67,-1.18789542670764E-48,
-1.));
#37078=DIRECTION('ref_axis',(-4.33680868994202E-19,1.,-1.18789542670764E-48));
#37079=DIRECTION('center_axis',(5.15167520928809E-67,-1.18789542670764E-48,
-1.));
#37080=DIRECTION('ref_axis',(-4.33680868994202E-19,1.,-1.18789542670764E-48));
#37081=DIRECTION('center_axis',(5.15167520928809E-67,-1.18789542670764E-48,
-1.));
#37082=DIRECTION('ref_axis',(-4.33680868994202E-19,1.,-1.18789542670764E-48));
#37083=DIRECTION('center_axis',(5.15167520928809E-67,-1.18789542670764E-48,
-1.));
#37084=DIRECTION('ref_axis',(-4.33680868994202E-19,1.,-1.18789542670764E-48));
#37085=DIRECTION('center_axis',(5.15167520928809E-67,-1.18789542670764E-48,
-1.));
#37086=DIRECTION('ref_axis',(-4.33680868994202E-19,1.,-1.18789542670764E-48));
#37087=DIRECTION('center_axis',(5.15167520928809E-67,-1.18789542670764E-48,
-1.));
#37088=DIRECTION('ref_axis',(-4.33680868994202E-19,1.,-1.18789542670764E-48));
#37089=DIRECTION('center_axis',(5.15167520928809E-67,-1.18789542670764E-48,
-1.));
#37090=DIRECTION('ref_axis',(-4.33680868994202E-19,1.,-1.18789542670764E-48));
#37091=DIRECTION('center_axis',(5.15167520928809E-67,-1.18789542670764E-48,
-1.));
#37092=DIRECTION('ref_axis',(-4.33680868994202E-19,1.,-1.18789542670764E-48));
#37093=DIRECTION('center_axis',(5.15167520928809E-67,-1.18789542670764E-48,
-1.));
#37094=DIRECTION('ref_axis',(-4.33680868994202E-19,1.,-1.18789542670764E-48));
#37095=DIRECTION('center_axis',(5.15167520928809E-67,-1.18789542670764E-48,
-1.));
#37096=DIRECTION('ref_axis',(-4.33680868994202E-19,1.,-1.18789542670764E-48));
#37097=DIRECTION('center_axis',(5.15167520928809E-67,-1.18789542670764E-48,
-1.));
#37098=DIRECTION('ref_axis',(-4.33680868994202E-19,1.,-1.18789542670764E-48));
#37099=DIRECTION('center_axis',(5.15167520928809E-67,-1.18789542670764E-48,
-1.));
#37100=DIRECTION('ref_axis',(-4.33680868994202E-19,1.,-1.18789542670764E-48));
#37101=DIRECTION('center_axis',(5.15167520928809E-67,-1.18789542670764E-48,
-1.));
#37102=DIRECTION('ref_axis',(-4.33680868994202E-19,1.,-1.18789542670764E-48));
#37103=DIRECTION('center_axis',(5.15167520928809E-67,-1.18789542670764E-48,
-1.));
#37104=DIRECTION('ref_axis',(-4.33680868994202E-19,1.,-1.18789542670764E-48));
#37105=DIRECTION('center_axis',(-0.7061576334064,-0.0555758110363729,0.705870190622555));
#37106=DIRECTION('ref_axis',(0.703694571287618,0.0553775799348557,0.708341212962294));
#37107=DIRECTION('center_axis',(5.15167520928809E-67,-1.18789542670764E-48,
-1.));
#37108=DIRECTION('ref_axis',(-4.33680868994202E-19,1.,-1.18789542670764E-48));
#37109=DIRECTION('center_axis',(-0.699618093637056,-0.110808620201623,0.70587249042916));
#37110=DIRECTION('ref_axis',(0.697182591373085,0.110419233095803,0.708338921173223));
#37111=DIRECTION('center_axis',(5.15167520928809E-67,-1.18789542670764E-48,
-1.));
#37112=DIRECTION('ref_axis',(-4.33680868994202E-19,1.,-1.18789542670764E-48));
#37113=DIRECTION('center_axis',(-0.68876582703002,-0.165358045050145,0.705874176077329));
#37114=DIRECTION('ref_axis',(0.686371526838198,0.164780094681657,0.708337241391772));
#37115=DIRECTION('center_axis',(5.15167520928809E-67,-1.18789542670764E-48,
-1.));
#37116=DIRECTION('ref_axis',(-4.33680868994202E-19,1.,-1.18789542670764E-48));
#37117=DIRECTION('center_axis',(-0.673667540197642,-0.218887852522971,0.705875451692394));
#37118=DIRECTION('ref_axis',(0.671328261761337,0.218125006053688,0.708335970210874));
#37119=DIRECTION('center_axis',(5.15167520928809E-67,-1.18789542670764E-48,
-1.));
#37120=DIRECTION('ref_axis',(-4.33680868994202E-19,1.,-1.18789542670764E-48));
#37121=DIRECTION('center_axis',(-0.654416196007479,-0.271068063822885,0.705876439030525));
#37122=DIRECTION('ref_axis',(0.652145682815046,0.270125073932086,0.708334986301596));
#37123=DIRECTION('center_axis',(5.15167520928809E-67,-1.18789542670764E-48,
-1.));
#37124=DIRECTION('ref_axis',(-4.33680868994202E-19,1.,-1.18789542670764E-48));
#37125=DIRECTION('center_axis',(-0.631130405143739,-0.321577003370466,0.705877214964735));
#37126=DIRECTION('ref_axis',(0.628942147608447,0.3204596972635,0.708334213060093));
#37127=DIRECTION('center_axis',(5.15167520928809E-67,-1.18789542670764E-48,
-1.));
#37128=DIRECTION('ref_axis',(-4.33680868994202E-19,1.,-1.18789542670764E-48));
#37129=DIRECTION('center_axis',(-0.603953677099563,-0.37010328932661,0.705877830185607));
#37130=DIRECTION('ref_axis',(0.601860775526009,0.3688185435042,0.708333599972973));
#37131=DIRECTION('center_axis',(5.15167520928809E-67,-1.18789542670764E-48,
-1.));
#37132=DIRECTION('ref_axis',(-4.33680868994202E-19,1.,-1.18789542670764E-48));
#37133=DIRECTION('center_axis',(-0.573053525770468,-0.416347757295655,0.705878319256877));
#37134=DIRECTION('ref_axis',(-0.571068576442267,-0.414903461781928,-0.708333112597156));
#37135=DIRECTION('center_axis',(5.15167520928809E-67,-1.18789542670764E-48,
-1.));
#37136=DIRECTION('ref_axis',(-4.33680868994202E-19,1.,-1.18789542670764E-48));
#37137=DIRECTION('center_axis',(-0.5386204311615,-0.460025307051025,0.705878706300176));
#37138=DIRECTION('ref_axis',(-0.53675542739315,-0.458430320957627,-0.708332726895124));
#37139=DIRECTION('center_axis',(5.15167520928809E-67,-1.18789542670764E-48,
-1.));
#37140=DIRECTION('ref_axis',(-4.33680868994202E-19,1.,-1.18789542670764E-48));
#37141=DIRECTION('center_axis',(-0.500866661619536,-0.500866661619512,0.705879008439992));
#37142=DIRECTION('ref_axis',(-0.499132905770748,-0.499130761358414,-0.708332425802052));
#37143=DIRECTION('center_axis',(5.15167520928809E-67,-1.18789542670764E-48,
-1.));
#37144=DIRECTION('ref_axis',(-4.33680868994202E-19,1.,-1.18789542670764E-48));
#37145=DIRECTION('center_axis',(-0.460024963033767,-0.538620028369008,0.70587923784848));
#37146=DIRECTION('ref_axis',(-0.45843298726701,-0.536753849182318,-0.708332197188163));
#37147=DIRECTION('center_axis',(5.15167520928809E-67,-1.18789542670764E-48,
-1.));
#37148=DIRECTION('ref_axis',(-4.33680868994202E-19,1.,-1.18789542670764E-48));
#37149=DIRECTION('center_axis',(-0.416347122442742,-0.573052651970378,0.705879403087642));
#37150=DIRECTION('ref_axis',(-0.414906617259033,-0.571067623542942,-0.708332032521248));
#37151=DIRECTION('center_axis',(5.15167520928809E-67,-1.18789542670764E-48,
-1.));
#37152=DIRECTION('ref_axis',(-4.33680868994202E-19,1.,-1.18789542670764E-48));
#37153=DIRECTION('center_axis',(-0.370102414699178,-0.603952249837274,0.705879509938015));
#37154=DIRECTION('ref_axis',(-0.368822164723695,-0.601860526500739,-0.708331926040878));
#37155=DIRECTION('center_axis',(5.15167520928809E-67,-1.18789542670764E-48,
-1.));
#37156=DIRECTION('ref_axis',(-4.33680868994202E-19,1.,-1.18789542670764E-48));
#37157=DIRECTION('center_axis',(-0.321575941572111,-0.631128321247095,0.705879561909702));
#37158=DIRECTION('ref_axis',(-0.320463768412258,-0.628942707293509,-0.708331874249159));
#37159=DIRECTION('center_axis',(5.15167520928809E-67,-1.18789542670764E-48,
-1.));
#37160=DIRECTION('ref_axis',(-4.33680868994202E-19,1.,-1.18789542670764E-48));
#37161=DIRECTION('center_axis',(-0.271066873422704,-0.654413322126826,0.70587956051707));
#37162=DIRECTION('ref_axis',(-0.270129585579653,-0.652147192703568,-0.708331875636993));
#37163=DIRECTION('center_axis',(5.15167520928809E-67,-1.18789542670764E-48,
-1.));
#37164=DIRECTION('ref_axis',(-4.33680868994202E-19,1.,-1.18789542670764E-48));
#37165=DIRECTION('center_axis',(-0.218886604216915,-0.673663698306575,0.705879505353637));
#37166=DIRECTION('ref_axis',(-0.218129954131654,-0.671330916307006,-0.708331930609455));
#37167=DIRECTION('center_axis',(5.15167520928809E-67,-1.18789542670764E-48,
-1.));
#37168=DIRECTION('ref_axis',(-4.33680868994202E-19,1.,-1.18789542670764E-48));
#37169=DIRECTION('center_axis',(-0.165356831187205,-0.688760770926913,0.705879393956142));
#37170=DIRECTION('ref_axis',(-0.164785479532657,-0.686375600198504,-0.708332041621255));
#37171=DIRECTION('center_axis',(5.15167520928809E-67,-1.18789542670764E-48,
-1.));
#37172=DIRECTION('ref_axis',(-4.33680868994202E-19,1.,-1.18789542670764E-48));
#37173=DIRECTION('center_axis',(-0.110807570905278,-0.699611468639872,0.705879221381132));
#37174=DIRECTION('ref_axis',(-0.110425058152835,-0.697188483632899,-0.708332213598677));
#37175=DIRECTION('center_axis',(5.15167520928809E-67,-1.18789542670764E-48,
-1.));
#37176=DIRECTION('ref_axis',(-4.33680868994202E-19,1.,-1.18789542670764E-48));
#37177=DIRECTION('center_axis',(-0.0555751238837442,-0.706148902305009,
0.705878979272465));
#37178=DIRECTION('ref_axis',(-0.0553838490528384,-0.703702893729722,-0.708332454868834));
#37179=DIRECTION('center_axis',(5.15167520928809E-67,-1.18789542670764E-48,
-1.));
#37180=DIRECTION('ref_axis',(-4.33680868994202E-19,1.,-1.18789542670764E-48));
#37181=DIRECTION('',(8.62889469402126E-17,0.707106781186547,0.707106781186548));
#37182=DIRECTION('center_axis',(-5.15167520928809E-67,1.18789542670764E-48,
1.));
#37183=DIRECTION('ref_axis',(4.33680868994202E-19,-1.,1.18789542670764E-48));
#37184=DIRECTION('center_axis',(5.15167520928809E-67,-1.18789542670764E-48,
-1.));
#37185=DIRECTION('ref_axis',(-4.33680868994202E-19,1.,-1.18789542670764E-48));
#37186=DIRECTION('center_axis',(0.0555758110363494,0.706157633406676,-0.705870190622281));
#37187=DIRECTION('ref_axis',(0.0553775799347821,0.703694571287349,0.708341212962568));
#37188=DIRECTION('center_axis',(5.15167520928809E-67,-1.18789542670764E-48,
-1.));
#37189=DIRECTION('ref_axis',(-4.33680868994202E-19,1.,-1.18789542670764E-48));
#37190=DIRECTION('center_axis',(0.110808620201597,0.699618093636782,-0.705872490429435));
#37191=DIRECTION('ref_axis',(0.110419233096536,0.697182591373247,0.708338921172949));
#37192=DIRECTION('center_axis',(5.15167520928809E-67,-1.18789542670764E-48,
-1.));
#37193=DIRECTION('ref_axis',(-4.33680868994202E-19,1.,-1.18789542670764E-48));
#37194=DIRECTION('center_axis',(0.165358045050176,0.688765827030065,-0.705874176077277));
#37195=DIRECTION('ref_axis',(0.164780094681565,0.686371526838166,0.708337241391824));
#37196=DIRECTION('center_axis',(5.15167520928809E-67,-1.18789542670764E-48,
-1.));
#37197=DIRECTION('ref_axis',(-4.33680868994202E-19,1.,-1.18789542670764E-48));
#37198=DIRECTION('center_axis',(0.218887852522828,0.673667540197125,-0.705875451692931));
#37199=DIRECTION('ref_axis',(0.218125006053502,0.671328261761963,0.708335970210338));
#37200=DIRECTION('center_axis',(5.15167520928809E-67,-1.18789542670764E-48,
-1.));
#37201=DIRECTION('ref_axis',(-4.33680868994202E-19,1.,-1.18789542670764E-48));
#37202=DIRECTION('center_axis',(0.271068063822916,0.654416196007463,-0.705876439030527));
#37203=DIRECTION('ref_axis',(0.270125073931817,0.65214568281516,0.708334986301594));
#37204=DIRECTION('center_axis',(5.15167520928809E-67,-1.18789542670764E-48,
-1.));
#37205=DIRECTION('ref_axis',(-4.33680868994202E-19,1.,-1.18789542670764E-48));
#37206=DIRECTION('center_axis',(0.321577003370433,0.631130405143686,-0.705877214964798));
#37207=DIRECTION('ref_axis',(0.320459697263181,0.62894214760868,0.70833421306003));
#37208=DIRECTION('center_axis',(5.15167520928809E-67,-1.18789542670764E-48,
-1.));
#37209=DIRECTION('ref_axis',(-4.33680868994202E-19,1.,-1.18789542670764E-48));
#37210=DIRECTION('center_axis',(0.37010328932647,0.603953677099309,-0.705877830185898));
#37211=DIRECTION('ref_axis',(0.368818543504439,0.601860775526204,0.708333599972683));
#37212=DIRECTION('center_axis',(5.15167520928809E-67,-1.18789542670764E-48,
-1.));
#37213=DIRECTION('ref_axis',(-4.33680868994202E-19,1.,-1.18789542670764E-48));
#37214=DIRECTION('center_axis',(0.416347757295563,0.573053525770315,-0.705878319257056));
#37215=DIRECTION('ref_axis',(0.414903461782186,0.5710685764423,0.708333112596977));
#37216=DIRECTION('center_axis',(5.15167520928809E-67,-1.18789542670764E-48,
-1.));
#37217=DIRECTION('ref_axis',(-4.33680868994202E-19,1.,-1.18789542670764E-48));
#37218=DIRECTION('center_axis',(0.46002530705103,0.538620431161473,-0.705878706300193));
#37219=DIRECTION('ref_axis',(0.458430320957387,0.536755427393379,0.708332726895108));
#37220=DIRECTION('center_axis',(5.15167520928809E-67,-1.18789542670764E-48,
-1.));
#37221=DIRECTION('ref_axis',(-4.33680868994202E-19,1.,-1.18789542670764E-48));
#37222=DIRECTION('center_axis',(0.500866661619595,0.500866661619595,-0.705879008439891));
#37223=DIRECTION('ref_axis',(0.499130761358023,0.499132905770996,0.708332425802153));
#37224=DIRECTION('center_axis',(5.15167520928809E-67,-1.18789542670764E-48,
-1.));
#37225=DIRECTION('ref_axis',(-4.33680868994202E-19,1.,-1.18789542670764E-48));
#37226=DIRECTION('center_axis',(0.538620028368889,0.460024963033635,-0.705879237848656));
#37227=DIRECTION('ref_axis',(0.536753849182959,0.458432987266531,0.708332197187987));
#37228=DIRECTION('center_axis',(5.15167520928809E-67,-1.18789542670764E-48,
-1.));
#37229=DIRECTION('ref_axis',(-4.33680868994202E-19,1.,-1.18789542670764E-48));
#37230=DIRECTION('center_axis',(0.573052651970233,0.416347122442629,-0.705879403087826));
#37231=DIRECTION('ref_axis',(0.57106762354309,0.414906617259142,0.708332032521065));
#37232=DIRECTION('center_axis',(5.15167520928809E-67,-1.18789542670764E-48,
-1.));
#37233=DIRECTION('ref_axis',(-4.33680868994202E-19,1.,-1.18789542670764E-48));
#37234=DIRECTION('center_axis',(0.603952249837032,0.370102414699012,-0.70587950993831));
#37235=DIRECTION('ref_axis',(0.601860526500475,0.36882216472469,0.708331926040585));
#37236=DIRECTION('center_axis',(5.15167520928809E-67,-1.18789542670764E-48,
-1.));
#37237=DIRECTION('ref_axis',(-4.33680868994202E-19,1.,-1.18789542670764E-48));
#37238=DIRECTION('center_axis',(0.631128321246922,0.32157594157199,-0.705879561909913));
#37239=DIRECTION('ref_axis',(0.628942707293632,0.32046376841248,0.708331874248949));
#37240=DIRECTION('center_axis',(5.15167520928809E-67,-1.18789542670764E-48,
-1.));
#37241=DIRECTION('ref_axis',(-4.33680868994202E-19,1.,-1.18789542670764E-48));
#37242=DIRECTION('center_axis',(0.654413322126609,0.271066873422466,-0.705879560517362));
#37243=DIRECTION('ref_axis',(0.652147192704168,0.270129585578968,0.708331875636702));
#37244=DIRECTION('center_axis',(5.15167520928809E-67,-1.18789542670764E-48,
-1.));
#37245=DIRECTION('ref_axis',(-4.33680868994202E-19,1.,-1.18789542670764E-48));
#37246=DIRECTION('center_axis',(0.673663698306398,0.218886604216837,-0.70587950535383));
#37247=DIRECTION('ref_axis',(0.671330916306662,0.218129954133339,0.708331930609263));
#37248=DIRECTION('center_axis',(5.15167520928809E-67,-1.18789542670764E-48,
-1.));
#37249=DIRECTION('ref_axis',(-4.33680868994202E-19,1.,-1.18789542670764E-48));
#37250=DIRECTION('center_axis',(0.688760770927087,0.165356831187229,-0.705879393955967));
#37251=DIRECTION('ref_axis',(0.686375600198292,0.164785479532791,0.70833204162143));
#37252=DIRECTION('center_axis',(5.15167520928809E-67,-1.18789542670764E-48,
-1.));
#37253=DIRECTION('ref_axis',(-4.33680868994202E-19,1.,-1.18789542670764E-48));
#37254=DIRECTION('center_axis',(0.699611468639904,0.110807570905141,-0.705879221381122));
#37255=DIRECTION('ref_axis',(0.697188483632864,0.11042505815299,0.708332213598687));
#37256=DIRECTION('center_axis',(5.15167520928809E-67,-1.18789542670764E-48,
-1.));
#37257=DIRECTION('ref_axis',(-4.33680868994202E-19,1.,-1.18789542670764E-48));
#37258=DIRECTION('center_axis',(0.706148902304704,0.0555751238836885,-0.705878979272775));
#37259=DIRECTION('ref_axis',(0.703702893729991,0.0553838490533688,0.708332454868525));
#37260=DIRECTION('center_axis',(5.15167520928809E-67,-1.18789542670764E-48,
-1.));
#37261=DIRECTION('ref_axis',(-4.33680868994202E-19,1.,-1.18789542670764E-48));
#37262=DIRECTION('center_axis',(0.708332577472139,3.0719028773502E-19,-0.705878856243532));
#37263=DIRECTION('ref_axis',(0.705878856242677,1.5561538090606E-6,0.708332577471281));
#37264=DIRECTION('center_axis',(5.15167520928809E-67,-1.18789542670764E-48,
-1.));
#37265=DIRECTION('ref_axis',(-4.33680868994202E-19,1.,-1.18789542670764E-48));
#37266=DIRECTION('center_axis',(0.706157633406651,-0.0555758110363464,-0.705870190622306));
#37267=DIRECTION('ref_axis',(0.703694571287399,-0.0553775799344575,0.708341212962543));
#37268=DIRECTION('center_axis',(5.15167520928809E-67,-1.18789542670764E-48,
-1.));
#37269=DIRECTION('ref_axis',(-4.33680868994202E-19,1.,-1.18789542670764E-48));
#37270=DIRECTION('center_axis',(0.699618093636944,-0.110808620201621,-0.705872490429271));
#37271=DIRECTION('ref_axis',(0.697182591373154,-0.110419233096072,0.708338921173112));
#37272=DIRECTION('center_axis',(5.15167520928809E-67,-1.18789542670764E-48,
-1.));
#37273=DIRECTION('ref_axis',(-4.33680868994202E-19,1.,-1.18789542670764E-48));
#37274=DIRECTION('center_axis',(0.688765827030149,-0.165358045050179,-0.705874176077195));
#37275=DIRECTION('ref_axis',(0.686371526838092,-0.164780094681522,0.708337241391906));
#37276=DIRECTION('center_axis',(5.15167520928809E-67,-1.18789542670764E-48,
-1.));
#37277=DIRECTION('ref_axis',(-4.33680868994202E-19,1.,-1.18789542670764E-48));
#37278=DIRECTION('center_axis',(0.673667540197491,-0.218887852522947,-0.705875451692545));
#37279=DIRECTION('ref_axis',(0.671328261761432,-0.218125006053886,0.708335970210723));
#37280=DIRECTION('center_axis',(5.15167520928809E-67,-1.18789542670764E-48,
-1.));
#37281=DIRECTION('ref_axis',(-4.33680868994202E-19,1.,-1.18789542670764E-48));
#37282=DIRECTION('center_axis',(0.654416196007489,-0.271068063822922,-0.705876439030501));
#37283=DIRECTION('ref_axis',(0.652145682814786,-0.270125073932652,0.70833498630162));
#37284=DIRECTION('center_axis',(5.15167520928809E-67,-1.18789542670764E-48,
-1.));
#37285=DIRECTION('ref_axis',(-4.33680868994202E-19,1.,-1.18789542670764E-48));
#37286=DIRECTION('center_axis',(0.631130405143858,-0.321577003370522,-0.705877214964604));
#37287=DIRECTION('ref_axis',(0.628942147608515,-0.320459697263077,0.708334213060224));
#37288=DIRECTION('center_axis',(5.15167520928809E-67,-1.18789542670764E-48,
-1.));
#37289=DIRECTION('ref_axis',(-4.33680868994202E-19,1.,-1.18789542670764E-48));
#37290=DIRECTION('center_axis',(0.603953677099314,-0.37010328932649,-0.705877830185883));
#37291=DIRECTION('ref_axis',(0.60186077552563,-0.368818543505346,0.708333599972698));
#37292=DIRECTION('center_axis',(5.15167520928809E-67,-1.18789542670764E-48,
-1.));
#37293=DIRECTION('ref_axis',(-4.33680868994202E-19,1.,-1.18789542670764E-48));
#37294=DIRECTION('center_axis',(0.573053525770311,-0.416347757295561,-0.70587831925706));
#37295=DIRECTION('ref_axis',(-0.571068576442179,0.41490346178236,-0.708333112596973));
#37296=DIRECTION('center_axis',(5.15167520928809E-67,-1.18789542670764E-48,
-1.));
#37297=DIRECTION('ref_axis',(-4.33680868994202E-19,1.,-1.18789542670764E-48));
#37298=DIRECTION('center_axis',(0.53862043116148,-0.460025307051029,-0.705878706300189));
#37299=DIRECTION('ref_axis',(-0.536755427393413,0.45843032095734,-0.708332726895112));
#37300=DIRECTION('center_axis',(5.15167520928809E-67,-1.18789542670764E-48,
-1.));
#37301=DIRECTION('ref_axis',(-4.33680868994202E-19,1.,-1.18789542670764E-48));
#37302=DIRECTION('center_axis',(0.500866661619453,-0.500866661619453,-0.705879008440093));
#37303=DIRECTION('ref_axis',(-0.499132905770974,0.49913076135833,-0.708332425801952));
#37304=DIRECTION('center_axis',(5.15167520928809E-67,-1.18789542670764E-48,
-1.));
#37305=DIRECTION('ref_axis',(-4.33680868994202E-19,1.,-1.18789542670764E-48));
#37306=DIRECTION('center_axis',(0.460024963033751,-0.538620028369041,-0.705879237848464));
#37307=DIRECTION('ref_axis',(-0.458432987266724,0.536753849182542,-0.708332197188179));
#37308=DIRECTION('center_axis',(5.15167520928809E-67,-1.18789542670764E-48,
-1.));
#37309=DIRECTION('ref_axis',(-4.33680868994202E-19,1.,-1.18789542670764E-48));
#37310=DIRECTION('center_axis',(0.416347122442499,-0.573052651970059,-0.705879403088044));
#37311=DIRECTION('ref_axis',(-0.414906617258677,0.571067623543698,-0.708332032520848));
#37312=DIRECTION('center_axis',(5.15167520928809E-67,-1.18789542670764E-48,
-1.));
#37313=DIRECTION('ref_axis',(-4.33680868994202E-19,1.,-1.18789542670764E-48));
#37314=DIRECTION('center_axis',(0.370102414698996,-0.603952249837027,-0.705879509938322));
#37315=DIRECTION('ref_axis',(-0.36882216472453,0.601860526500588,-0.708331926040572));
#37316=DIRECTION('center_axis',(5.15167520928809E-67,-1.18789542670764E-48,
-1.));
#37317=DIRECTION('ref_axis',(-4.33680868994202E-19,1.,-1.18789542670764E-48));
#37318=DIRECTION('center_axis',(0.321575941571994,-0.631128321246919,-0.705879561909914));
#37319=DIRECTION('ref_axis',(-0.320463768412686,0.628942707293528,-0.708331874248948));
#37320=DIRECTION('center_axis',(5.15167520928809E-67,-1.18789542670764E-48,
-1.));
#37321=DIRECTION('ref_axis',(-4.33680868994202E-19,1.,-1.18789542670764E-48));
#37322=DIRECTION('center_axis',(0.27106687342253,-0.654413322126797,-0.705879560517163));
#37323=DIRECTION('ref_axis',(-0.270129585579053,0.652147192703917,-0.7083318756369));
#37324=DIRECTION('center_axis',(5.15167520928809E-67,-1.18789542670764E-48,
-1.));
#37325=DIRECTION('ref_axis',(-4.33680868994202E-19,1.,-1.18789542670764E-48));
#37326=DIRECTION('center_axis',(0.218886604216888,-0.673663698306596,-0.705879505353626));
#37327=DIRECTION('ref_axis',(-0.218129954133397,0.671330916306428,-0.708331930609466));
#37328=DIRECTION('center_axis',(5.15167520928809E-67,-1.18789542670764E-48,
-1.));
#37329=DIRECTION('ref_axis',(-4.33680868994202E-19,1.,-1.18789542670764E-48));
#37330=DIRECTION('center_axis',(0.165356831187193,-0.688760770926925,-0.705879393956133));
#37331=DIRECTION('ref_axis',(-0.164785479532379,0.686375600198561,-0.708332041621264));
#37332=DIRECTION('center_axis',(5.15167520928809E-67,-1.18789542670764E-48,
-1.));
#37333=DIRECTION('ref_axis',(-4.33680868994202E-19,1.,-1.18789542670764E-48));
#37334=DIRECTION('center_axis',(0.110807570905112,-0.699611468639716,-0.705879221381312));
#37335=DIRECTION('ref_axis',(-0.110425058152835,0.697188483633082,-0.708332213598497));
#37336=DIRECTION('center_axis',(5.15167520928809E-67,-1.18789542670764E-48,
-1.));
#37337=DIRECTION('ref_axis',(-4.33680868994202E-19,1.,-1.18789542670764E-48));
#37338=DIRECTION('center_axis',(0.0555751238837179,-0.706148902304883,-0.705878979272593));
#37339=DIRECTION('ref_axis',(-0.0553838490533129,0.703702893729813,-0.708332454868706));
#37340=DIRECTION('center_axis',(5.15167520928809E-67,-1.18789542670764E-48,
-1.));
#37341=DIRECTION('ref_axis',(-4.33680868994202E-19,1.,-1.18789542670764E-48));
#37342=DIRECTION('center_axis',(4.22129745643424E-13,-0.708370174930854,
-0.705841126081805));
#37343=DIRECTION('ref_axis',(-3.47233154276107E-12,0.705841126081805,-0.708370174930854));
#37344=DIRECTION('center_axis',(5.15167520928809E-67,-1.18789542670764E-48,
-1.));
#37345=DIRECTION('ref_axis',(-4.33680868994202E-19,1.,-1.18789542670764E-48));
#37346=DIRECTION('center_axis',(-0.0555758110363383,-0.706157633406556,
-0.705870190622402));
#37347=DIRECTION('ref_axis',(0.0553775799352142,0.703694571287436,-0.708341212962447));
#37348=DIRECTION('center_axis',(5.15167520928809E-67,-1.18789542670764E-48,
-1.));
#37349=DIRECTION('ref_axis',(-4.33680868994202E-19,1.,-1.18789542670764E-48));
#37350=DIRECTION('center_axis',(-0.110808620201578,-0.699618093636773,-0.705872490429447));
#37351=DIRECTION('ref_axis',(0.110419233096311,0.697182591373295,-0.708338921172937));
#37352=DIRECTION('center_axis',(5.15167520928809E-67,-1.18789542670764E-48,
-1.));
#37353=DIRECTION('ref_axis',(-4.33680868994202E-19,1.,-1.18789542670764E-48));
#37354=DIRECTION('center_axis',(-0.165358045050148,-0.688765827029952,-0.705874176077394));
#37355=DIRECTION('ref_axis',(0.164780094682061,0.686371526838168,-0.708337241391707));
#37356=DIRECTION('center_axis',(5.15167520928809E-67,-1.18789542670764E-48,
-1.));
#37357=DIRECTION('ref_axis',(-4.33680868994202E-19,1.,-1.18789542670764E-48));
#37358=DIRECTION('center_axis',(-0.218887852522884,-0.673667540197305,-0.705875451692742));
#37359=DIRECTION('ref_axis',(0.218125006053241,0.671328261761849,-0.708335970210527));
#37360=DIRECTION('center_axis',(5.15167520928809E-67,-1.18789542670764E-48,
-1.));
#37361=DIRECTION('ref_axis',(-4.33680868994202E-19,1.,-1.18789542670764E-48));
#37362=DIRECTION('center_axis',(-0.271068063822912,-0.654416196007481,-0.705876439030512));
#37363=DIRECTION('ref_axis',(0.270125073931987,0.652145682815073,-0.708334986301609));
#37364=DIRECTION('center_axis',(5.15167520928809E-67,-1.18789542670764E-48,
-1.));
#37365=DIRECTION('ref_axis',(-4.33680868994202E-19,1.,-1.18789542670764E-48));
#37366=DIRECTION('center_axis',(-0.321577003370454,-0.631130405143677,-0.705877214964797));
#37367=DIRECTION('ref_axis',(0.32045969726294,0.628942147608801,-0.708334213060031));
#37368=DIRECTION('center_axis',(5.15167520928809E-67,-1.18789542670764E-48,
-1.));
#37369=DIRECTION('ref_axis',(-4.33680868994202E-19,1.,-1.18789542670764E-48));
#37370=DIRECTION('center_axis',(-0.370103289326527,-0.60395367709939,-0.705877830185799));
#37371=DIRECTION('ref_axis',(0.368818543504467,0.601860775526071,-0.708333599972782));
#37372=DIRECTION('center_axis',(5.15167520928809E-67,-1.18789542670764E-48,
-1.));
#37373=DIRECTION('ref_axis',(-4.33680868994202E-19,1.,-1.18789542670764E-48));
#37374=DIRECTION('center_axis',(-0.41634775729562,-0.5730535257704,-0.705878319256953));
#37375=DIRECTION('ref_axis',(0.414903461781904,0.571068576442378,-0.70833311259708));
#37376=DIRECTION('center_axis',(5.15167520928809E-67,-1.18789542670764E-48,
-1.));
#37377=DIRECTION('ref_axis',(-4.33680868994202E-19,1.,-1.18789542670764E-48));
#37378=DIRECTION('center_axis',(-0.460025307050912,-0.538620431161332,-0.705878706300378));
#37379=DIRECTION('ref_axis',(0.458430320957773,0.536755427393291,-0.708332726894923));
#37380=DIRECTION('center_axis',(5.15167520928809E-67,-1.18789542670764E-48,
-1.));
#37381=DIRECTION('ref_axis',(-4.33680868994202E-19,1.,-1.18789542670764E-48));
#37382=DIRECTION('center_axis',(-0.500866661619468,-0.500866661619444,-0.705879008440089));
#37383=DIRECTION('ref_axis',(0.499130761358181,0.499132905771117,-0.708332425801956));
#37384=DIRECTION('center_axis',(5.15167520928809E-67,-1.18789542670764E-48,
-1.));
#37385=DIRECTION('ref_axis',(-4.33680868994202E-19,1.,-1.18789542670764E-48));
#37386=DIRECTION('center_axis',(-0.538620028368883,-0.46002496303363,-0.705879237848664));
#37387=DIRECTION('ref_axis',(0.536753849182796,0.458432987266734,-0.70833219718798));
#37388=DIRECTION('center_axis',(5.15167520928809E-67,-1.18789542670764E-48,
-1.));
#37389=DIRECTION('ref_axis',(-4.33680868994202E-19,1.,-1.18789542670764E-48));
#37390=DIRECTION('center_axis',(-0.573052651970218,-0.416347122442612,-0.705879403087848));
#37391=DIRECTION('ref_axis',(0.571067623543181,0.414906617259055,-0.708332032521043));
#37392=DIRECTION('center_axis',(5.15167520928809E-67,-1.18789542670764E-48,
-1.));
#37393=DIRECTION('ref_axis',(-4.33680868994202E-19,1.,-1.18789542670764E-48));
#37394=DIRECTION('center_axis',(-0.603952249837038,-0.37010241469901,-0.705879509938305));
#37395=DIRECTION('ref_axis',(0.601860526500551,0.368822164724558,-0.708331926040589));
#37396=DIRECTION('center_axis',(5.15167520928809E-67,-1.18789542670764E-48,
-1.));
#37397=DIRECTION('ref_axis',(-4.33680868994202E-19,1.,-1.18789542670764E-48));
#37398=DIRECTION('center_axis',(-0.631128321246897,-0.32157594157199,-0.705879561909935));
#37399=DIRECTION('ref_axis',(0.628942707294004,0.320463768411799,-0.708331874248927));
#37400=DIRECTION('center_axis',(5.15167520928809E-67,-1.18789542670764E-48,
-1.));
#37401=DIRECTION('ref_axis',(-4.33680868994202E-19,1.,-1.18789542670764E-48));
#37402=DIRECTION('center_axis',(-0.654413322126778,-0.271066873422522,-0.705879560517184));
#37403=DIRECTION('ref_axis',(0.65214719270402,0.270129585578859,-0.708331875636879));
#37404=DIRECTION('center_axis',(5.15167520928809E-67,-1.18789542670764E-48,
-1.));
#37405=DIRECTION('ref_axis',(-4.33680868994202E-19,1.,-1.18789542670764E-48));
#37406=DIRECTION('center_axis',(-0.673663698306464,-0.218886604216857,-0.705879505353761));
#37407=DIRECTION('ref_axis',(0.671330916306719,0.218129954132939,-0.708331930609331));
#37408=DIRECTION('center_axis',(5.15167520928809E-67,-1.18789542670764E-48,
-1.));
#37409=DIRECTION('ref_axis',(-4.33680868994202E-19,1.,-1.18789542670764E-48));
#37410=DIRECTION('center_axis',(-0.688760770927255,-0.165356831187267,-0.705879393955794));
#37411=DIRECTION('ref_axis',(0.686375600198197,0.164785479532444,-0.708332041621602));
#37412=DIRECTION('center_axis',(5.15167520928809E-67,-1.18789542670764E-48,
-1.));
#37413=DIRECTION('ref_axis',(-4.33680868994202E-19,1.,-1.18789542670764E-48));
#37414=DIRECTION('center_axis',(-0.699611468639891,-0.110807570905155,-0.705879221381132));
#37415=DIRECTION('ref_axis',(0.697188483632974,0.110425058152362,-0.708332213598677));
#37416=DIRECTION('center_axis',(5.15167520928809E-67,-1.18789542670764E-48,
-1.));
#37417=DIRECTION('ref_axis',(-4.33680868994202E-19,1.,-1.18789542670764E-48));
#37418=DIRECTION('center_axis',(-0.706148902304619,-0.0555751238836977,
-0.705878979272859));
#37419=DIRECTION('ref_axis',(0.703702893730101,0.0553838490530483,-0.708332454868441));
#37420=DIRECTION('center_axis',(5.15167520928809E-67,-1.18789542670764E-48,
-1.));
#37421=DIRECTION('ref_axis',(-4.33680868994202E-19,1.,-1.18789542670764E-48));
#37422=DIRECTION('center_axis',(5.15167520928809E-67,-1.18789542670764E-48,
-1.));
#37423=DIRECTION('ref_axis',(-4.33680868994202E-19,1.,-1.18789542670764E-48));
#37424=DIRECTION('center_axis',(5.15167520928809E-67,-1.18789542670764E-48,
-1.));
#37425=DIRECTION('ref_axis',(-4.33680868994202E-19,1.,-1.18789542670764E-48));
#37426=DIRECTION('center_axis',(5.15167520928809E-67,-1.18789542670764E-48,
-1.));
#37427=DIRECTION('ref_axis',(-4.33680868994202E-19,1.,-1.18789542670764E-48));
#37428=DIRECTION('center_axis',(5.15167520928809E-67,-1.18789542670764E-48,
-1.));
#37429=DIRECTION('ref_axis',(-4.33680868994202E-19,1.,-1.18789542670764E-48));
#37430=DIRECTION('center_axis',(5.15167520928809E-67,-1.18789542670764E-48,
-1.));
#37431=DIRECTION('ref_axis',(-4.33680868994202E-19,1.,-1.18789542670764E-48));
#37432=DIRECTION('center_axis',(5.15167520928809E-67,-1.18789542670764E-48,
-1.));
#37433=DIRECTION('ref_axis',(-4.33680868994202E-19,1.,-1.18789542670764E-48));
#37434=DIRECTION('center_axis',(5.15167520928809E-67,-1.18789542670764E-48,
-1.));
#37435=DIRECTION('ref_axis',(-4.33680868994202E-19,1.,-1.18789542670764E-48));
#37436=DIRECTION('center_axis',(5.15167520928809E-67,-1.18789542670764E-48,
-1.));
#37437=DIRECTION('ref_axis',(-4.33680868994202E-19,1.,-1.18789542670764E-48));
#37438=DIRECTION('center_axis',(5.15167520928809E-67,-1.18789542670764E-48,
-1.));
#37439=DIRECTION('ref_axis',(-4.33680868994202E-19,1.,-1.18789542670764E-48));
#37440=DIRECTION('center_axis',(5.15167520928809E-67,-1.18789542670764E-48,
-1.));
#37441=DIRECTION('ref_axis',(-4.33680868994202E-19,1.,-1.18789542670764E-48));
#37442=DIRECTION('center_axis',(5.15167520928809E-67,-1.18789542670764E-48,
-1.));
#37443=DIRECTION('ref_axis',(-4.33680868994202E-19,1.,-1.18789542670764E-48));
#37444=DIRECTION('center_axis',(5.15167520928809E-67,-1.18789542670764E-48,
-1.));
#37445=DIRECTION('ref_axis',(-4.33680868994202E-19,1.,-1.18789542670764E-48));
#37446=DIRECTION('center_axis',(5.15167520928809E-67,-1.18789542670764E-48,
-1.));
#37447=DIRECTION('ref_axis',(-4.33680868994202E-19,1.,-1.18789542670764E-48));
#37448=DIRECTION('center_axis',(5.15167520928809E-67,-1.18789542670764E-48,
-1.));
#37449=DIRECTION('ref_axis',(-4.33680868994202E-19,1.,-1.18789542670764E-48));
#37450=DIRECTION('center_axis',(5.15167520928809E-67,-1.18789542670764E-48,
-1.));
#37451=DIRECTION('ref_axis',(-4.33680868994202E-19,1.,-1.18789542670764E-48));
#37452=DIRECTION('center_axis',(-0.271066873422527,0.654413322126802,-0.70587956051716));
#37453=DIRECTION('ref_axis',(-0.270129585578839,0.652147192704003,0.708331875636903));
#37454=DIRECTION('center_axis',(5.15167520928809E-67,-1.18789542670764E-48,
-1.));
#37455=DIRECTION('ref_axis',(-4.33680868994202E-19,1.,-1.18789542670764E-48));
#37456=DIRECTION('center_axis',(-0.218886604216929,0.673663698306674,-0.705879505353539));
#37457=DIRECTION('ref_axis',(-0.218129954131946,0.671330916306808,0.708331930609553));
#37458=DIRECTION('center_axis',(5.15167520928809E-67,-1.18789542670764E-48,
-1.));
#37459=DIRECTION('ref_axis',(-4.33680868994202E-19,1.,-1.18789542670764E-48));
#37460=DIRECTION('center_axis',(-0.16535683118721,0.688760770927084,-0.705879393955974));
#37461=DIRECTION('ref_axis',(-0.164785479532737,0.686375600198312,0.708332041621423));
#37462=DIRECTION('center_axis',(5.15167520928809E-67,-1.18789542670764E-48,
-1.));
#37463=DIRECTION('ref_axis',(-4.33680868994202E-19,1.,-1.18789542670764E-48));
#37464=DIRECTION('center_axis',(-0.110807570905113,0.699611468639715,-0.705879221381313));
#37465=DIRECTION('ref_axis',(-0.110425058151779,0.69718848363325,0.708332213598496));
#37466=DIRECTION('center_axis',(5.15167520928809E-67,-1.18789542670764E-48,
-1.));
#37467=DIRECTION('ref_axis',(-4.33680868994202E-19,1.,-1.18789542670764E-48));
#37468=DIRECTION('center_axis',(-0.0555751238836985,0.706148902304822,-0.705878979272656));
#37469=DIRECTION('ref_axis',(-0.0553838490532064,0.703702893729884,0.708332454868643));
#37470=DIRECTION('center_axis',(5.15167520928809E-67,-1.18789542670764E-48,
-1.));
#37471=DIRECTION('ref_axis',(-4.33680868994202E-19,1.,-1.18789542670764E-48));
#37472=DIRECTION('',(8.69022643068848E-17,-0.707106781186538,-0.707106781186557));
#37473=DIRECTION('center_axis',(5.15167520928809E-67,-1.18789542670764E-48,
-1.));
#37474=DIRECTION('ref_axis',(-4.33680868994202E-19,1.,-1.18789542670764E-48));
#37475=DIRECTION('center_axis',(5.15167520928809E-67,-1.18789542670764E-48,
-1.));
#37476=DIRECTION('ref_axis',(-4.33680868994202E-19,1.,-1.18789542670764E-48));
#37477=DIRECTION('center_axis',(5.15167520928809E-67,-1.18789542670764E-48,
-1.));
#37478=DIRECTION('ref_axis',(0.,1.,0.));
#37479=DIRECTION('center_axis',(5.15167520928809E-67,-1.18789542670764E-48,
-1.));
#37480=DIRECTION('ref_axis',(-4.33680868994202E-19,1.,-1.18789542670764E-48));
#37481=DIRECTION('center_axis',(1.,0.,5.15167520928809E-67));
#37482=DIRECTION('ref_axis',(0.,-1.,0.));
#37483=DIRECTION('center_axis',(5.15167520928809E-67,-1.18789542670764E-48,
-1.));
#37484=DIRECTION('ref_axis',(-4.33680868994202E-19,1.,-1.18789542670764E-48));
#37485=DIRECTION('center_axis',(5.15167520928809E-67,-1.18789542670764E-48,
-1.));
#37486=DIRECTION('ref_axis',(-4.33680868994202E-19,1.,-1.18789542670764E-48));
#37487=DIRECTION('',(-5.15167520928809E-67,1.18789542670764E-48,1.));
#37488=DIRECTION('center_axis',(5.15167520928809E-67,-1.18789542670764E-48,
-1.));
#37489=DIRECTION('ref_axis',(0.,1.,0.));
#37490=DIRECTION('center_axis',(5.15167520928809E-67,-1.18789542670764E-48,
-1.));
#37491=DIRECTION('ref_axis',(-4.33680868994202E-19,1.,-1.18789542670764E-48));
#37492=DIRECTION('center_axis',(-1.,0.,-5.15167520928809E-67));
#37493=DIRECTION('ref_axis',(0.,-1.,0.));
#37494=DIRECTION('center_axis',(5.15167520928809E-67,-1.18789542670764E-48,
-1.));
#37495=DIRECTION('ref_axis',(0.,1.,0.));
#37496=DIRECTION('center_axis',(1.,0.,5.15167520928809E-67));
#37497=DIRECTION('ref_axis',(0.,-1.,0.));
#37498=DIRECTION('center_axis',(5.15167520928809E-67,-1.18789542670764E-48,
-1.));
#37499=DIRECTION('ref_axis',(-4.33680868994202E-19,1.,-1.18789542670764E-48));
#37500=DIRECTION('center_axis',(5.15167520928809E-67,-1.18789542670764E-48,
-1.));
#37501=DIRECTION('ref_axis',(0.,1.,0.));
#37502=DIRECTION('center_axis',(-0.726741019926939,-0.686911553067863,9.06501466507717E-5));
#37503=DIRECTION('ref_axis',(0.686840456252471,-0.726663889286196,0.0144837723800636));
#37504=DIRECTION('center_axis',(5.15167520928809E-67,-1.18789542670764E-48,
-1.));
#37505=DIRECTION('ref_axis',(-4.33680868994202E-19,1.,-1.18789542670764E-48));
#37506=DIRECTION('center_axis',(0.0503838293498797,0.99872992276226,0.000105448247773495));
#37507=DIRECTION('ref_axis',(0.998655285166785,-0.0503813543085061,0.012220496982052));
#37508=DIRECTION('center_axis',(5.15167520928809E-67,-1.18789542670764E-48,
-1.));
#37509=DIRECTION('ref_axis',(0.,1.,0.));
#37510=DIRECTION('center_axis',(-0.0281309337977199,0.999604241409737,0.000105448247664664));
#37511=DIRECTION('ref_axis',(0.999529639708461,0.0281275452111534,0.0122204969076063));
#37512=DIRECTION('center_axis',(-0.670606260601171,-0.741813477246852,9.06501467500846E-5));
#37513=DIRECTION('ref_axis',(0.741736547998884,-0.670534945920291,0.0144837723805249));
#37514=DIRECTION('center_axis',(5.15167520928809E-67,-1.18789542670764E-48,
-1.));
#37515=DIRECTION('ref_axis',(-4.33680868994202E-19,1.,-1.18789542670764E-48));
#37516=DIRECTION('center_axis',(5.15167520928809E-67,-1.18789542670764E-48,
-1.));
#37517=DIRECTION('ref_axis',(0.,1.,0.));
#37518=DIRECTION('center_axis',(-0.106472260383779,0.994315667506771,0.000105448247699395));
#37519=DIRECTION('ref_axis',(0.99424156164256,0.106463029061011,0.0122204969504906));
#37520=DIRECTION('center_axis',(-0.610336990679751,-0.792141874660428,9.06501467512865E-5));
#37521=DIRECTION('ref_axis',(0.792059587274889,-0.610271931637935,0.0144837723275367));
#37522=DIRECTION('center_axis',(5.15167520928809E-67,-1.18789542670764E-48,
-1.));
#37523=DIRECTION('ref_axis',(-4.33680868994202E-19,1.,-1.18789542670764E-48));
#37524=DIRECTION('center_axis',(5.15167520928809E-67,-1.18789542670764E-48,
-1.));
#37525=DIRECTION('ref_axis',(0.,1.,0.));
#37526=DIRECTION('center_axis',(-0.18415715007879,0.982896806870144,0.000105448247763879));
#37527=DIRECTION('ref_axis',(0.982823653730846,0.18414213293402,0.0122204969481005));
#37528=DIRECTION('center_axis',(-0.546304790252955,-0.837586454002944,9.06501468511952E-5));
#37529=DIRECTION('ref_axis',(0.837499315807933,-0.546246387960026,0.0144837723631749));
#37530=DIRECTION('center_axis',(5.15167520928809E-67,-1.18789542670764E-48,
-1.));
#37531=DIRECTION('ref_axis',(-4.33680868994202E-19,1.,-1.18789542670764E-48));
#37532=DIRECTION('center_axis',(5.15167520928809E-67,-1.18789542670764E-48,
-1.));
#37533=DIRECTION('ref_axis',(0.,1.,0.));
#37534=DIRECTION('center_axis',(-0.260706649705391,0.965418060572754,0.000105448247684059));
#37535=DIRECTION('ref_axis',(0.965346311171948,0.260685939324359,0.0122204969329739));
#37536=DIRECTION('center_axis',(-0.478904439129961,-0.877867034330466,9.06501466909999E-5));
#37537=DIRECTION('ref_axis',(0.877775582562065,-0.478853053655646,0.0144837723846339));
#37538=DIRECTION('center_axis',(5.15167520928809E-67,-1.18789542670764E-48,
-1.));
#37539=DIRECTION('ref_axis',(-4.33680868994202E-19,1.,-1.18789542670764E-48));
#37540=DIRECTION('center_axis',(5.15167520928809E-67,-1.18789542670764E-48,
-1.));
#37541=DIRECTION('ref_axis',(0.,1.,0.));
#37542=DIRECTION('center_axis',(-0.33564880614276,0.941987190897842,0.000105448247631265));
#37543=DIRECTION('ref_axis',(0.941917287593993,0.335622530211717,0.0122204969563928));
#37544=DIRECTION('center_axis',(-0.408551482887427,-0.912735272471178,9.06501467675252E-5));
#37545=DIRECTION('ref_axis',(0.91264007095957,-0.408507431040139,0.0144837724331839));
#37546=DIRECTION('center_axis',(5.15167520928809E-67,-1.18789542670764E-48,
-1.));
#37547=DIRECTION('ref_axis',(-4.33680868994202E-19,1.,-1.18789542670764E-48));
#37548=DIRECTION('center_axis',(5.15167520928809E-67,-1.18789542670764E-48,
-1.));
#37549=DIRECTION('ref_axis',(0.,1.,0.));
#37550=DIRECTION('center_axis',(-0.408521576075341,0.912748656948662,0.000105448247753309));
#37551=DIRECTION('ref_axis',(0.912681030719062,0.40848989659417,0.0122204969651243));
#37552=DIRECTION('center_axis',(-0.335679670896088,-0.941976194141681,9.06501466394305E-5));
#37553=DIRECTION('ref_axis',(0.941877829837658,-0.335643224270894,0.0144837723450194));
#37554=DIRECTION('center_axis',(5.15167520928809E-67,-1.18789542670764E-48,
-1.));
#37555=DIRECTION('ref_axis',(-4.33680868994202E-19,1.,-1.18789542670764E-48));
#37556=DIRECTION('center_axis',(5.15167520928809E-67,-1.18789542670764E-48,
-1.));
#37557=DIRECTION('ref_axis',(0.,1.,0.));
#37558=DIRECTION('center_axis',(-0.478875674645407,0.877882724009063,0.000105448247283112));
#37559=DIRECTION('ref_axis',(0.877817791790398,0.478838786927794,0.012220497115417));
#37560=DIRECTION('center_axis',(-0.260738282108194,-0.965409519336649,9.06501468435925E-5));
#37561=DIRECTION('ref_axis',(0.965308598687812,-0.260709665410158,0.0144837723364994));
#37562=DIRECTION('center_axis',(5.15167520928809E-67,-1.18789542670764E-48,
-1.));
#37563=DIRECTION('ref_axis',(-4.33680868994202E-19,1.,-1.18789542670764E-48));
#37564=DIRECTION('center_axis',(5.15167520928809E-67,-1.18789542670764E-48,
-1.));
#37565=DIRECTION('ref_axis',(0.,1.,0.));
#37566=DIRECTION('center_axis',(-0.546277345437336,0.837604352151184,0.000105448247639474));
#37567=DIRECTION('ref_axis',(0.837542514276272,0.546235476910692,0.0122204968773897));
#37568=DIRECTION('center_axis',(-0.184189355107295,-0.982890773813505,9.06501468099581E-5));
#37569=DIRECTION('ref_axis',(0.982787919029019,-0.184168744767822,0.0144837723419927));
#37570=DIRECTION('center_axis',(5.15167520928809E-67,-1.18789542670764E-48,
-1.));
#37571=DIRECTION('ref_axis',(-4.33680868994202E-19,1.,-1.18789542670764E-48));
#37572=DIRECTION('center_axis',(5.15167520928809E-67,-1.18789542670764E-48,
-1.));
#37573=DIRECTION('ref_axis',(0.,1.,0.));
#37574=DIRECTION('center_axis',(-0.610311034740724,0.792161870929404,0.000105448247072483));
#37575=DIRECTION('ref_axis',(0.792103508642798,0.610264443533926,0.0122204972891987));
#37576=DIRECTION('center_axis',(-0.106504839483277,-0.994312179825427,9.06501466463657E-5));
#37577=DIRECTION('ref_axis',(0.994208025037708,-0.106492362571804,0.014483772453865));
#37578=DIRECTION('center_axis',(5.15167520928809E-67,-1.18789542670764E-48,
-1.));
#37579=DIRECTION('ref_axis',(-4.33680868994202E-19,1.,-1.18789542670764E-48));
#37580=DIRECTION('center_axis',(5.15167520928809E-67,-1.18789542670764E-48,
-1.));
#37581=DIRECTION('ref_axis',(0.,1.,0.));
#37582=DIRECTION('center_axis',(-0.670581953563772,0.74183544835446,0.000105448247723866));
#37583=DIRECTION('ref_axis',(0.741780921486778,0.670530926933108,0.012220496898794));
#37584=DIRECTION('center_axis',(-0.0281636861068304,-0.999603320606443,
9.06501467794172E-5));
#37585=DIRECTION('ref_axis',(0.999498507966719,-0.0281594195479949,0.0144837724030356));
#37586=DIRECTION('center_axis',(5.15167520928809E-67,-1.18789542670764E-48,
-1.));
#37587=DIRECTION('ref_axis',(-4.33680868994202E-19,1.,-1.18789542670764E-48));
#37588=DIRECTION('center_axis',(5.15167520928809E-67,-1.18789542670764E-48,
-1.));
#37589=DIRECTION('ref_axis',(0.,1.,0.));
#37590=DIRECTION('center_axis',(-0.726718511653027,0.686935363554299,0.000105448247728815));
#37591=DIRECTION('ref_axis',(0.686885008277766,0.726663364191397,0.0122204969332444));
#37592=DIRECTION('center_axis',(0.050351105759542,-0.998731574514065,9.06501467573609E-5));
#37593=DIRECTION('ref_axis',(0.998626750226961,0.0503471356610921,0.014483772362966));
#37594=DIRECTION('center_axis',(5.15167520928809E-67,-1.18789542670764E-48,
-1.));
#37595=DIRECTION('ref_axis',(-4.33680868994202E-19,1.,-1.18789542670764E-48));
#37596=DIRECTION('center_axis',(5.15167520928809E-67,-1.18789542670764E-48,
-1.));
#37597=DIRECTION('ref_axis',(0.,1.,0.));
#37598=DIRECTION('center_axis',(-0.778374608459537,0.627800093808634,0.000105448247783041));
#37599=DIRECTION('ref_axis',(0.627754220580437,0.778315680169477,0.01222049695274));
#37600=DIRECTION('center_axis',(0.128555466315269,-0.991702316152894,9.06501465984867E-5));
#37601=DIRECTION('ref_axis',(0.99159812649388,0.128543284036463,0.0144837724004731));
#37602=DIRECTION('center_axis',(5.15167520928809E-67,-1.18789542670764E-48,
-1.));
#37603=DIRECTION('ref_axis',(-4.33680868994202E-19,1.,-1.18789542670764E-48));
#37604=DIRECTION('center_axis',(5.15167520928809E-67,-1.18789542670764E-48,
-1.));
#37605=DIRECTION('ref_axis',(0.,1.,0.));
#37606=DIRECTION('center_axis',(-0.825231766969855,0.564794227718802,0.000105448247237627));
#37607=DIRECTION('ref_axis',(0.564753119361559,0.825169421162197,0.0122204971352771));
#37608=DIRECTION('center_axis',(0.205967239672467,-0.97855888323813,9.06501466256469E-5));
#37609=DIRECTION('ref_axis',(0.978455970572454,0.205946920321296,0.0144837723432324));
#37610=DIRECTION('center_axis',(5.15167520928809E-67,-1.18789542670764E-48,
-1.));
#37611=DIRECTION('ref_axis',(-4.33680868994202E-19,1.,-1.18789542670764E-48));
#37612=DIRECTION('center_axis',(5.15167520928809E-67,-1.18789542670764E-48,
-1.));
#37613=DIRECTION('ref_axis',(0.,1.,0.));
#37614=DIRECTION('center_axis',(-0.867001097222074,0.498306217396881,0.00010544824406792));
#37615=DIRECTION('ref_axis',(0.498270127350421,0.866935718266621,0.0122204985059196));
#37616=DIRECTION('center_axis',(0.282109156506117,-0.959382309404316,9.06501467341775E-5));
#37617=DIRECTION('ref_axis',(0.959281308220891,0.282080825357731,0.0144837724201092));
#37618=DIRECTION('center_axis',(5.15167520928809E-67,-1.18789542670764E-48,
-1.));
#37619=DIRECTION('ref_axis',(-4.33680868994202E-19,1.,-1.18789542670764E-48));
#37620=DIRECTION('center_axis',(5.15167520928809E-67,-1.18789542670764E-48,
-1.));
#37621=DIRECTION('ref_axis',(0.,1.,0.));
#37622=DIRECTION('center_axis',(-0.903425077395399,0.428745983554114,0.00010544824771057));
#37623=DIRECTION('ref_axis',(0.42871513434286,0.903357068405985,0.0122204969754959));
#37624=DIRECTION('center_axis',(0.356511776578972,-0.934290824606052,9.06501467185522E-5));
#37625=DIRECTION('ref_axis',(0.934192357612503,0.356475608304786,0.0144837723720686));
#37626=DIRECTION('center_axis',(5.15167520928809E-67,-1.18789542670764E-48,
-1.));
#37627=DIRECTION('ref_axis',(-4.33680868994202E-19,1.,-1.18789542670764E-48));
#37628=DIRECTION('center_axis',(5.15167520928809E-67,-1.18789542670764E-48,
-1.));
#37629=DIRECTION('ref_axis',(0.,1.,0.));
#37630=DIRECTION('center_axis',(-0.934279141551227,0.35654238814336,0.000105448247725771));
#37631=DIRECTION('ref_axis',(0.356516969954114,0.934208921810617,0.0122204968876431));
#37632=DIRECTION('center_axis',(0.428716382996855,-0.903439126190938,9.06501466905075E-5));
#37633=DIRECTION('ref_axis',(0.903343800467886,0.428672600585895,0.0144837724078269));
#37634=DIRECTION('center_axis',(5.15167520928809E-67,-1.18789542670764E-48,
-1.));
#37635=DIRECTION('ref_axis',(-4.33680868994202E-19,1.,-1.18789542670764E-48));
#37636=DIRECTION('center_axis',(5.15167520928809E-67,-1.18789542670764E-48,
-1.));
#37637=DIRECTION('ref_axis',(0.,1.,0.));
#37638=DIRECTION('center_axis',(-0.959373064120116,0.282140590347166,0.000105448247704078));
#37639=DIRECTION('ref_axis',(0.282120759890668,0.959301066553995,0.0122204970062476));
#37640=DIRECTION('center_axis',(0.498277810351468,-0.867017425138559,9.06501469271671E-5));
#37641=DIRECTION('ref_axis',(0.86692582840188,0.498226683737388,0.0144837723593644));
#37642=DIRECTION('center_axis',(5.15167520928809E-67,-1.18789542670764E-48,
-1.));
#37643=DIRECTION('ref_axis',(-4.33680868994202E-19,1.,-1.18789542670764E-48));
#37644=DIRECTION('center_axis',(5.15167520928809E-67,-1.18789542670764E-48,
-1.));
#37645=DIRECTION('ref_axis',(0.,1.,0.));
#37646=DIRECTION('center_axis',(-0.978552132724721,0.205999301990486,0.000105448247790145));
#37647=DIRECTION('ref_axis',(0.205985181528783,0.978478801224291,0.0122204969305395));
#37648=DIRECTION('center_axis',(0.564767189310343,-0.825250273348059,9.06501467424166E-5));
#37649=DIRECTION('ref_axis',(0.825162970321744,0.56470903370561,0.0144837723356968));
#37650=DIRECTION('center_axis',(5.15167520928809E-67,-1.18789542670764E-48,
-1.));
#37651=DIRECTION('ref_axis',(-4.33680868994202E-19,1.,-1.18789542670764E-48));
#37652=DIRECTION('center_axis',(5.15167520928809E-67,-1.18789542670764E-48,
-1.));
#37653=DIRECTION('ref_axis',(0.,1.,0.));
#37654=DIRECTION('center_axis',(-0.991698102029505,0.128587959435343,0.000105448247905715));
#37655=DIRECTION('ref_axis',(0.12857963602553,0.991623888707005,0.0122204969268892));
#37656=DIRECTION('center_axis',(0.627774590743107,-0.778395179198763,9.06501466692162E-5));
#37657=DIRECTION('ref_axis',(0.778312708134479,0.627709764696018,0.0144837723553914));
#37658=DIRECTION('center_axis',(5.15167520928809E-67,-1.18789542670764E-48,
-1.));
#37659=DIRECTION('ref_axis',(-4.33680868994202E-19,1.,-1.18789542670764E-48));
#37660=DIRECTION('center_axis',(5.15167520928809E-67,-1.18789542670764E-48,
-1.));
#37661=DIRECTION('ref_axis',(0.,1.,0.));
#37662=DIRECTION('center_axis',(-0.998729922762266,0.05038382934976,0.000105448247701369));
#37663=DIRECTION('ref_axis',(0.0503813543083786,0.998655285166624,0.0122204969957313));
#37664=DIRECTION('center_axis',(0.686911553067687,-0.726741019927105,9.06501465529425E-5));
#37665=DIRECTION('ref_axis',(0.726663889286156,0.686840456252101,0.0144837723995786));
#37666=DIRECTION('center_axis',(5.15167520928809E-67,-1.18789542670764E-48,
-1.));
#37667=DIRECTION('ref_axis',(-4.33680868994202E-19,1.,-1.18789542670764E-48));
#37668=DIRECTION('center_axis',(5.15167520928809E-67,-1.18789542670764E-48,
-1.));
#37669=DIRECTION('ref_axis',(0.,1.,0.));
#37670=DIRECTION('center_axis',(-0.999604241409733,-0.0281309337978441,
0.000105448247608528));
#37671=DIRECTION('ref_axis',(0.0281275452112647,-0.999529639708088,-0.0122204969378127));
#37672=DIRECTION('center_axis',(0.741813477246663,-0.67060626060138,9.06501466416355E-5));
#37673=DIRECTION('ref_axis',(0.670534945920398,0.741736547998582,0.0144837723910712));
#37674=DIRECTION('center_axis',(5.15167520928809E-67,-1.18789542670764E-48,
-1.));
#37675=DIRECTION('ref_axis',(-4.33680868994202E-19,1.,-1.18789542670764E-48));
#37676=DIRECTION('center_axis',(5.15167520928809E-67,-1.18789542670764E-48,
-1.));
#37677=DIRECTION('ref_axis',(0.,1.,0.));
#37678=DIRECTION('center_axis',(-0.994315667506803,-0.106472260383486,0.000105448247832577));
#37679=DIRECTION('ref_axis',(0.10646302906079,-0.994241561643227,-0.0122204968981425));
#37680=DIRECTION('center_axis',(0.792141874660394,-0.610336990679795,9.06501467163515E-5));
#37681=DIRECTION('ref_axis',(0.610271931637984,0.792059587274861,0.0144837723269713));
#37682=DIRECTION('center_axis',(5.15167520928809E-67,-1.18789542670764E-48,
-1.));
#37683=DIRECTION('ref_axis',(-4.33680868994202E-19,1.,-1.18789542670764E-48));
#37684=DIRECTION('center_axis',(5.15167520928809E-67,-1.18789542670764E-48,
-1.));
#37685=DIRECTION('ref_axis',(0.,1.,0.));
#37686=DIRECTION('center_axis',(-0.982896806870098,-0.184157150079038,0.000105448247610839));
#37687=DIRECTION('ref_axis',(0.184142132934261,-0.982823653730751,-0.0122204969521754));
#37688=DIRECTION('center_axis',(0.837586454002892,-0.546304790253034,9.06501468389122E-5));
#37689=DIRECTION('ref_axis',(0.546246387959946,0.837499315807641,0.014483772383082));
#37690=DIRECTION('center_axis',(5.15167520928809E-67,-1.18789542670764E-48,
-1.));
#37691=DIRECTION('ref_axis',(-4.33680868994202E-19,1.,-1.18789542670764E-48));
#37692=DIRECTION('center_axis',(5.15167520928809E-67,-1.18789542670764E-48,
-1.));
#37693=DIRECTION('ref_axis',(0.,1.,0.));
#37694=DIRECTION('center_axis',(-0.965418060572767,-0.260706649705342,0.000105448247695262));
#37695=DIRECTION('ref_axis',(0.260685939324476,-0.965346311172558,-0.0122204968822783));
#37696=DIRECTION('center_axis',(0.877867034330398,-0.478904439130086,9.06501466177592E-5));
#37697=DIRECTION('ref_axis',(0.478853053655353,0.877775582561241,0.0144837724443041));
#37698=DIRECTION('center_axis',(5.15167520928809E-67,-1.18789542670764E-48,
-1.));
#37699=DIRECTION('ref_axis',(-4.33680868994202E-19,1.,-1.18789542670764E-48));
#37700=DIRECTION('center_axis',(5.15167520928809E-67,-1.18789542670764E-48,
-1.));
#37701=DIRECTION('ref_axis',(0.,1.,0.));
#37702=DIRECTION('center_axis',(-0.941987190897914,-0.335648806142557,0.000105448247712849));
#37703=DIRECTION('ref_axis',(0.335622530211483,-0.941917287593983,-0.0122204969636003));
#37704=DIRECTION('center_axis',(0.912735272471151,-0.408551482887487,9.06501467033935E-5));
#37705=DIRECTION('ref_axis',(0.408507431040848,0.912640070960968,0.0144837723251257));
#37706=DIRECTION('center_axis',(5.15167520928809E-67,-1.18789542670764E-48,
-1.));
#37707=DIRECTION('ref_axis',(-4.33680868994202E-19,1.,-1.18789542670764E-48));
#37708=DIRECTION('center_axis',(5.15167520928809E-67,-1.18789542670764E-48,
-1.));
#37709=DIRECTION('ref_axis',(0.,1.,0.));
#37710=DIRECTION('center_axis',(-0.912748656948201,-0.408521576076371,0.000105448247247158));
#37711=DIRECTION('ref_axis',(0.408489896594259,-0.912681030716532,-0.012220497151094));
#37712=DIRECTION('center_axis',(0.941976194141716,-0.335679670895989,9.06501466623777E-5));
#37713=DIRECTION('ref_axis',(0.335643224270751,0.941877829837572,0.0144837723539316));
#37714=DIRECTION('center_axis',(5.15167520928809E-67,-1.18789542670764E-48,
-1.));
#37715=DIRECTION('ref_axis',(-4.33680868994202E-19,1.,-1.18789542670764E-48));
#37716=DIRECTION('center_axis',(5.15167520928809E-67,-1.18789542670764E-48,
-1.));
#37717=DIRECTION('ref_axis',(0.,1.,0.));
#37718=DIRECTION('center_axis',(-0.877882724009451,-0.478875674644697,0.000105448247674909));
#37719=DIRECTION('ref_axis',(0.478838786928496,-0.877817791793333,-0.0122204968770904));
#37720=DIRECTION('center_axis',(0.965409519336493,-0.26073828210877,9.06501465579451E-5));
#37721=DIRECTION('ref_axis',(0.260709665410522,0.965308598686875,0.0144837723924504));
#37722=DIRECTION('center_axis',(5.15167520928809E-67,-1.18789542670764E-48,
-1.));
#37723=DIRECTION('ref_axis',(-4.33680868994202E-19,1.,-1.18789542670764E-48));
#37724=DIRECTION('center_axis',(5.15167520928809E-67,-1.18789542670764E-48,
-1.));
#37725=DIRECTION('ref_axis',(0.,1.,0.));
#37726=DIRECTION('center_axis',(-0.837604352151306,-0.546277345437149,0.00010544824776483));
#37727=DIRECTION('ref_axis',(0.546235476910197,-0.837542514275933,-0.0122204969227218));
#37728=DIRECTION('center_axis',(0.982890773813463,-0.184189355107518,9.06501466980053E-5));
#37729=DIRECTION('ref_axis',(0.184168744767822,0.982787919027818,0.0144837724235038));
#37730=DIRECTION('center_axis',(5.15167520928809E-67,-1.18789542670764E-48,
-1.));
#37731=DIRECTION('ref_axis',(-4.33680868994202E-19,1.,-1.18789542670764E-48));
#37732=DIRECTION('center_axis',(5.15167520928809E-67,-1.18789542670764E-48,
-1.));
#37733=DIRECTION('ref_axis',(0.,1.,0.));
#37734=DIRECTION('center_axis',(-0.792161870930109,-0.610311034739809,0.000105448247597277));
#37735=DIRECTION('ref_axis',(0.610264443535208,-0.792103508646315,-0.0122204969972532));
#37736=DIRECTION('center_axis',(0.994312179825469,-0.106504839482882,9.06501468290203E-5));
#37737=DIRECTION('ref_axis',(0.106492362571566,0.994208025039157,0.0144837723561435));
#37738=DIRECTION('center_axis',(5.15167520928809E-67,-1.18789542670764E-48,
-1.));
#37739=DIRECTION('ref_axis',(-4.33680868994202E-19,1.,-1.18789542670764E-48));
#37740=DIRECTION('center_axis',(5.15167520928809E-67,-1.18789542670764E-48,
-1.));
#37741=DIRECTION('ref_axis',(0.,1.,0.));
#37742=DIRECTION('center_axis',(-0.741835448354634,-0.670581953563579,0.000105448247853962));
#37743=DIRECTION('ref_axis',(0.67053092693267,-0.741780921486687,-0.0122204969283275));
#37744=DIRECTION('center_axis',(0.99960332060645,-0.0281636861065795,9.06501468718404E-5));
#37745=DIRECTION('ref_axis',(0.0281594195477731,0.999498507967606,0.014483772342229));
#37746=DIRECTION('center_axis',(5.15167520928809E-67,-1.18789542670764E-48,
-1.));
#37747=DIRECTION('ref_axis',(-4.33680868994202E-19,1.,-1.18789542670764E-48));
#37748=DIRECTION('center_axis',(5.15167520928809E-67,-1.18789542670764E-48,
-1.));
#37749=DIRECTION('ref_axis',(0.,1.,0.));
#37750=DIRECTION('center_axis',(-0.686935363552547,-0.726718511654683,0.000105448246665782));
#37751=DIRECTION('ref_axis',(0.726663364188996,-0.686885008272227,-0.0122204973873402));
#37752=DIRECTION('center_axis',(0.998731574514055,0.0503511057597249,9.06501467982717E-5));
#37753=DIRECTION('ref_axis',(0.050347135661256,-0.998626750226507,-0.0144837723936806));
#37754=DIRECTION('center_axis',(5.15167520928809E-67,-1.18789542670764E-48,
-1.));
#37755=DIRECTION('ref_axis',(-4.33680868994202E-19,1.,-1.18789542670764E-48));
#37756=DIRECTION('center_axis',(5.15167520928809E-67,-1.18789542670764E-48,
-1.));
#37757=DIRECTION('ref_axis',(0.,1.,0.));
#37758=DIRECTION('center_axis',(-0.627800093808639,-0.778374608459533,0.000105448247779514));
#37759=DIRECTION('ref_axis',(0.778315680170178,-0.627754220581,-0.0122204968791585));
#37760=DIRECTION('center_axis',(0.991702316152886,0.12855546631533,9.06501466251883E-5));
#37761=DIRECTION('ref_axis',(0.128543284036466,-0.991598126493403,-0.0144837724330683));
#37762=DIRECTION('center_axis',(5.15167520928809E-67,-1.18789542670764E-48,
-1.));
#37763=DIRECTION('ref_axis',(-4.33680868994202E-19,1.,-1.18789542670764E-48));
#37764=DIRECTION('center_axis',(5.15167520928809E-67,-1.18789542670764E-48,
-1.));
#37765=DIRECTION('ref_axis',(0.,1.,0.));
#37766=DIRECTION('center_axis',(-0.564794227719968,-0.825231766969057,0.000105448247863909));
#37767=DIRECTION('ref_axis',(0.825169421163414,-0.564753119364088,-0.0122204969362205));
#37768=DIRECTION('center_axis',(0.978558883238036,0.205967239672914,9.06501468463484E-5));
#37769=DIRECTION('ref_axis',(0.205946920321936,-0.978455970573291,-0.014483772277592));
#37770=DIRECTION('center_axis',(5.15167520928809E-67,-1.18789542670764E-48,
-1.));
#37771=DIRECTION('ref_axis',(-4.33680868994202E-19,1.,-1.18789542670764E-48));
#37772=DIRECTION('center_axis',(5.15167520928809E-67,-1.18789542670764E-48,
-1.));
#37773=DIRECTION('ref_axis',(0.,1.,0.));
#37774=DIRECTION('center_axis',(-0.498306217403848,-0.86700109721807,0.000105448247661773));
#37775=DIRECTION('ref_axis',(0.866935718279092,-0.498270127366718,-0.0122204969566953));
#37776=DIRECTION('center_axis',(0.959382309404258,0.282109156506314,9.06501467982869E-5));
#37777=DIRECTION('ref_axis',(0.282080825358155,-0.959281308221622,-0.014483772363392));
#37778=DIRECTION('center_axis',(5.15167520928809E-67,-1.18789542670764E-48,
-1.));
#37779=DIRECTION('ref_axis',(-4.33680868994202E-19,1.,-1.18789542670764E-48));
#37780=DIRECTION('center_axis',(5.15167520928809E-67,-1.18789542670764E-48,
-1.));
#37781=DIRECTION('ref_axis',(0.,1.,0.));
#37782=DIRECTION('center_axis',(-0.428745983554159,-0.903425077395378,0.000105448247692435));
#37783=DIRECTION('ref_axis',(0.903357068405516,-0.428715134342697,-0.0122204970158381));
#37784=DIRECTION('center_axis',(0.934290824605943,0.356511776579256,9.06501468588022E-5));
#37785=DIRECTION('ref_axis',(0.35647560830508,-0.934192357612417,-0.0144837723703894));
#37786=DIRECTION('center_axis',(5.15167520928809E-67,-1.18789542670764E-48,
-1.));
#37787=DIRECTION('ref_axis',(-4.33680868994202E-19,1.,-1.18789542670764E-48));
#37788=DIRECTION('center_axis',(5.15167520928809E-67,-1.18789542670764E-48,
-1.));
#37789=DIRECTION('ref_axis',(0.,1.,0.));
#37790=DIRECTION('center_axis',(-0.356542388142294,-0.934279141551633,0.000105448247232403));
#37791=DIRECTION('ref_axis',(0.934208921807365,-0.356516969951681,-0.0122204972072322));
#37792=DIRECTION('center_axis',(0.903439126190767,0.428716382997215,9.06501468179925E-5));
#37793=DIRECTION('ref_axis',(0.428672600586429,-0.903343800468082,-0.0144837723797852));
#37794=DIRECTION('center_axis',(5.15167520928809E-67,-1.18789542670764E-48,
-1.));
#37795=DIRECTION('ref_axis',(-4.33680868994202E-19,1.,-1.18789542670764E-48));
#37796=DIRECTION('center_axis',(5.15167520928809E-67,-1.18789542670764E-48,
-1.));
#37797=DIRECTION('ref_axis',(0.,1.,0.));
#37798=DIRECTION('center_axis',(-0.282140590347279,-0.959373064120083,0.000105448247741099));
#37799=DIRECTION('ref_axis',(0.959301066555032,-0.282120759891086,-0.012220496915153));
#37800=DIRECTION('center_axis',(0.867017425138588,0.498277810351419,9.06501468672452E-5));
#37801=DIRECTION('ref_axis',(0.498226683737162,-0.866925828401598,-0.0144837723840689));
#37802=DIRECTION('center_axis',(5.15167520928809E-67,-1.18789542670764E-48,
-1.));
#37803=DIRECTION('ref_axis',(-4.33680868994202E-19,1.,-1.18789542670764E-48));
#37804=DIRECTION('center_axis',(5.15167520928809E-67,-1.18789542670764E-48,
-1.));
#37805=DIRECTION('ref_axis',(0.,1.,0.));
#37806=DIRECTION('center_axis',(-0.20599930198994,-0.978552132724836,0.000105448247552452));
#37807=DIRECTION('ref_axis',(0.97847880122346,-0.205985181528044,-0.0122204970095074));
#37808=DIRECTION('center_axis',(0.825250273348004,0.564767189310424,9.06501467639861E-5));
#37809=DIRECTION('ref_axis',(0.56470903370563,-0.825162970321598,-0.0144837723432248));
#37810=DIRECTION('center_axis',(5.15167520928809E-67,-1.18789542670764E-48,
-1.));
#37811=DIRECTION('ref_axis',(-4.33680868994202E-19,1.,-1.18789542670764E-48));
#37812=DIRECTION('center_axis',(5.15167520928809E-67,-1.18789542670764E-48,
-1.));
#37813=DIRECTION('ref_axis',(0.,1.,0.));
#37814=DIRECTION('center_axis',(-0.128587959431095,-0.991698102030056,0.000105448246015545));
#37815=DIRECTION('ref_axis',(0.991623888697772,-0.128579636020076,-0.0122204977334817));
#37816=DIRECTION('center_axis',(0.778395179198649,0.627774590743249,9.06501467187627E-5));
#37817=DIRECTION('ref_axis',(0.62770976469618,-0.778312708134389,-0.0144837723532511));
#37818=DIRECTION('center_axis',(5.15167520928809E-67,-1.18789542670764E-48,
-1.));
#37819=DIRECTION('ref_axis',(-4.33680868994202E-19,1.,-1.18789542670764E-48));
#37820=DIRECTION('center_axis',(5.15167520928809E-67,-1.18789542670764E-48,
-1.));
#37821=DIRECTION('ref_axis',(0.,1.,0.));
#37822=DIRECTION('center_axis',(-0.0503838293498799,-0.99872992276226,0.000105448247790322));
#37823=DIRECTION('ref_axis',(0.998655285167012,-0.050381354308516,-0.0122204969634886));
#37824=DIRECTION('center_axis',(0.726741019926698,0.686911553068118,9.06501468063716E-5));
#37825=DIRECTION('ref_axis',(0.686840456253071,-0.726663889286322,-0.0144837723452766));
#37826=DIRECTION('center_axis',(5.15167520928809E-67,-1.18789542670764E-48,
-1.));
#37827=DIRECTION('ref_axis',(-4.33680868994202E-19,1.,-1.18789542670764E-48));
#37828=DIRECTION('center_axis',(5.15167520928809E-67,-1.18789542670764E-48,
-1.));
#37829=DIRECTION('ref_axis',(0.,1.,0.));
#37830=DIRECTION('center_axis',(0.0281309337977714,-0.999604241409735,0.000105448247661813));
#37831=DIRECTION('ref_axis',(0.999529639707556,0.0281275452111717,-0.0122204969816086));
#37832=DIRECTION('center_axis',(0.670606260601294,0.741813477246741,9.06501466782892E-5));
#37833=DIRECTION('ref_axis',(0.741736547997904,-0.67053494591962,-0.0144837724617815));
#37834=DIRECTION('center_axis',(5.15167520928809E-67,-1.18789542670764E-48,
-1.));
#37835=DIRECTION('ref_axis',(-4.33680868994202E-19,1.,-1.18789542670764E-48));
#37836=DIRECTION('center_axis',(5.15167520928809E-67,-1.18789542670764E-48,
-1.));
#37837=DIRECTION('ref_axis',(0.,1.,0.));
#37838=DIRECTION('center_axis',(0.106472260384112,-0.994315667506736,0.000105448247531298));
#37839=DIRECTION('ref_axis',(0.994241561642015,0.106463029061287,-0.01222049699245));
#37840=DIRECTION('center_axis',(0.610336990679746,0.792141874660432,9.06501467541659E-5));
#37841=DIRECTION('ref_axis',(0.792059587274579,-0.610271931637685,-0.0144837723550388));
#37842=DIRECTION('center_axis',(5.15167520928809E-67,-1.18789542670764E-48,
-1.));
#37843=DIRECTION('ref_axis',(-4.33680868994202E-19,1.,-1.18789542670764E-48));
#37844=DIRECTION('center_axis',(5.15167520928809E-67,-1.18789542670764E-48,
-1.));
#37845=DIRECTION('ref_axis',(0.,1.,0.));
#37846=DIRECTION('center_axis',(0.184157150078655,-0.982896806870169,0.000105448247826086));
#37847=DIRECTION('ref_axis',(0.982823653731041,0.184142132933918,-0.01222049693405));
#37848=DIRECTION('center_axis',(0.546304790253063,0.837586454002874,9.06501468026834E-5));
#37849=DIRECTION('ref_axis',(0.837499315807096,-0.546246387959628,-0.0144837724265968));
#37850=DIRECTION('center_axis',(5.15167520928809E-67,-1.18789542670764E-48,
-1.));
#37851=DIRECTION('ref_axis',(-4.33680868994202E-19,1.,-1.18789542670764E-48));
#37852=DIRECTION('center_axis',(5.15167520928809E-67,-1.18789542670764E-48,
-1.));
#37853=DIRECTION('ref_axis',(0.,1.,0.));
#37854=DIRECTION('center_axis',(0.260706649723291,-0.965418060567921,0.000105448239312411));
#37855=DIRECTION('ref_axis',(0.965346311124436,0.260685939330442,-0.0122205005564138));
#37856=DIRECTION('center_axis',(0.478904439129984,0.877867034330454,9.06501466836614E-5));
#37857=DIRECTION('ref_axis',(0.877775582561938,-0.478853053655605,-0.0144837723936657));
#37858=DIRECTION('center_axis',(5.15167520928809E-67,-1.18789542670764E-48,
-1.));
#37859=DIRECTION('ref_axis',(-4.33680868994202E-19,1.,-1.18789542670764E-48));
#37860=DIRECTION('center_axis',(5.15167520928809E-67,-1.18789542670764E-48,
-1.));
#37861=DIRECTION('ref_axis',(0.,1.,0.));
#37862=DIRECTION('center_axis',(0.335648806142683,-0.941987190897869,0.000105448247681778));
#37863=DIRECTION('ref_axis',(0.941917287594608,0.335622530211854,-0.012220496905163));
#37864=DIRECTION('center_axis',(0.408551482887321,0.912735272471225,9.06501468104788E-5));
#37865=DIRECTION('ref_axis',(0.912640070960436,-0.408507431040405,-0.014483772371131));
#37866=DIRECTION('center_axis',(5.15167520928809E-67,-1.18789542670764E-48,
-1.));
#37867=DIRECTION('ref_axis',(-4.33680868994202E-19,1.,-1.18789542670764E-48));
#37868=DIRECTION('center_axis',(5.15167520928809E-67,-1.18789542670764E-48,
-1.));
#37869=DIRECTION('ref_axis',(0.,1.,0.));
#37870=DIRECTION('center_axis',(0.408521576076219,-0.912748656948269,0.000105448247344423));
#37871=DIRECTION('ref_axis',(0.912681030717311,0.408489896594431,-0.0122204970871443));
#37872=DIRECTION('center_axis',(0.335679670895796,0.941976194141785,9.06501467685389E-5));
#37873=DIRECTION('ref_axis',(0.941877829836932,-0.335643224270299,-0.0144837724059784));
#37874=DIRECTION('center_axis',(5.15167520928809E-67,-1.18789542670764E-48,
-1.));
#37875=DIRECTION('ref_axis',(-4.33680868994202E-19,1.,-1.18789542670764E-48));
#37876=DIRECTION('center_axis',(5.15167520928809E-67,-1.18789542670764E-48,
-1.));
#37877=DIRECTION('ref_axis',(0.,1.,0.));
#37878=DIRECTION('center_axis',(0.478875674644822,-0.877882724009383,0.000105448247602163));
#37879=DIRECTION('ref_axis',(0.877817791792273,0.47883878692807,-0.0122204969699355));
#37880=DIRECTION('center_axis',(0.260738282108074,0.965409519336681,9.06501468936573E-5));
#37881=DIRECTION('ref_axis',(0.965308598687316,-0.260709665409891,-0.0144837723743816));
#37882=DIRECTION('center_axis',(5.15167520928809E-67,-1.18789542670764E-48,
-1.));
#37883=DIRECTION('ref_axis',(-4.33680868994202E-19,1.,-1.18789542670764E-48));
#37884=DIRECTION('center_axis',(5.15167520928809E-67,-1.18789542670764E-48,
-1.));
#37885=DIRECTION('ref_axis',(0.,1.,0.));
#37886=DIRECTION('center_axis',(0.546277345437349,-0.837604352151176,0.000105448247639465));
#37887=DIRECTION('ref_axis',(0.837542514275712,0.546235476910338,-0.0122204969316073));
#37888=DIRECTION('center_axis',(0.184189355107516,0.982890773813463,9.06501467024073E-5));
#37889=DIRECTION('ref_axis',(0.982787919028468,-0.184168744767946,-0.0144837723778112));
#37890=DIRECTION('center_axis',(5.15167520928809E-67,-1.18789542670764E-48,
-1.));
#37891=DIRECTION('ref_axis',(-4.33680868994202E-19,1.,-1.18789542670764E-48));
#37892=DIRECTION('center_axis',(5.15167520928809E-67,-1.18789542670764E-48,
-1.));
#37893=DIRECTION('ref_axis',(0.,1.,0.));
#37894=DIRECTION('center_axis',(0.610311034750668,-0.792161870921744,0.000105448241406271));
#37895=DIRECTION('ref_axis',(0.79210350861157,0.610264443525473,-0.0122204997355093));
#37896=DIRECTION('center_axis',(0.106504839483129,0.994312179825443,9.06501467375791E-5));
#37897=DIRECTION('ref_axis',(0.994208025038601,-0.106492362571754,-0.0144837723929676));
#37898=DIRECTION('center_axis',(5.15167520928809E-67,-1.18789542670764E-48,
-1.));
#37899=DIRECTION('ref_axis',(-4.33680868994202E-19,1.,-1.18789542670764E-48));
#37900=DIRECTION('center_axis',(5.15167520928809E-67,-1.18789542670764E-48,
-1.));
#37901=DIRECTION('ref_axis',(0.,1.,0.));
#37902=DIRECTION('center_axis',(0.670581953563674,-0.741835448354548,0.000105448247759945));
#37903=DIRECTION('ref_axis',(0.741780921486581,0.670530926932748,-0.0122204969305506));
#37904=DIRECTION('center_axis',(0.0281636861069903,0.999603320606438,9.06501466992701E-5));
#37905=DIRECTION('ref_axis',(0.999498507967367,-0.0281594195481785,-0.0144837723579484));
#37906=DIRECTION('center_axis',(5.15167520928809E-67,-1.18789542670764E-48,
-1.));
#37907=DIRECTION('ref_axis',(-4.33680868994202E-19,1.,-1.18789542670764E-48));
#37908=DIRECTION('center_axis',(5.15167520928809E-67,-1.18789542670764E-48,
-1.));
#37909=DIRECTION('ref_axis',(0.,1.,0.));
#37910=DIRECTION('center_axis',(0.726718511653026,-0.6869353635543,0.000105448247761845));
#37911=DIRECTION('ref_axis',(0.686885008277897,0.726663364191536,-0.0122204969175564));
#37912=DIRECTION('center_axis',(-0.0503511057596336,0.99873157451406,9.06501467774672E-5));
#37913=DIRECTION('ref_axis',(0.998626750226755,0.0503471356611751,-0.0144837723768601));
#37914=DIRECTION('center_axis',(5.15167520928809E-67,-1.18789542670764E-48,
-1.));
#37915=DIRECTION('ref_axis',(-4.33680868994202E-19,1.,-1.18789542670764E-48));
#37916=DIRECTION('center_axis',(5.15167520928809E-67,-1.18789542670764E-48,
-1.));
#37917=DIRECTION('ref_axis',(0.,1.,0.));
#37918=DIRECTION('center_axis',(0.778374608459656,-0.627800093808486,0.000105448247696036));
#37919=DIRECTION('ref_axis',(0.627754220580537,0.778315680169911,-0.0122204969200215));
#37920=DIRECTION('center_axis',(-0.128555466315276,0.991702316152893,9.06501466266556E-5));
#37921=DIRECTION('ref_axis',(0.991598126493641,0.128543284036441,-0.0144837724170315));
#37922=DIRECTION('center_axis',(5.15167520928809E-67,-1.18789542670764E-48,
-1.));
#37923=DIRECTION('ref_axis',(-4.33680868994202E-19,1.,-1.18789542670764E-48));
#37924=DIRECTION('center_axis',(5.15167520928809E-67,-1.18789542670764E-48,
-1.));
#37925=DIRECTION('ref_axis',(0.,1.,0.));
#37926=DIRECTION('center_axis',(0.825231766969182,-0.564794227719785,0.000105448247768853));
#37927=DIRECTION('ref_axis',(0.564753119363901,0.825169421163535,-0.0122204969367096));
#37928=DIRECTION('center_axis',(-0.205967239672835,0.978558883238052,9.06501467925213E-5));
#37929=DIRECTION('ref_axis',(0.978455970572528,0.205946920321698,-0.0144837723325158));
#37930=DIRECTION('center_axis',(5.15167520928809E-67,-1.18789542670764E-48,
-1.));
#37931=DIRECTION('ref_axis',(-4.33680868994202E-19,1.,-1.18789542670764E-48));
#37932=DIRECTION('center_axis',(5.15167520928809E-67,-1.18789542670764E-48,
-1.));
#37933=DIRECTION('ref_axis',(0.,1.,0.));
#37934=DIRECTION('center_axis',(0.867001097218019,-0.498306217403936,0.000105448247742928));
#37935=DIRECTION('ref_axis',(0.498270127367224,0.866935718279781,-0.0122204968872419));
#37936=DIRECTION('center_axis',(-0.282109156506148,0.959382309404307,9.06501467249393E-5));
#37937=DIRECTION('ref_axis',(0.959281308221143,0.282080825357837,-0.0144837724013445));
#37938=DIRECTION('center_axis',(5.15167520928809E-67,-1.18789542670764E-48,
-1.));
#37939=DIRECTION('ref_axis',(-4.33680868994202E-19,1.,-1.18789542670764E-48));
#37940=DIRECTION('center_axis',(5.15167520928809E-67,-1.18789542670764E-48,
-1.));
#37941=DIRECTION('ref_axis',(0.,1.,0.));
#37942=DIRECTION('center_axis',(0.903425077395463,-0.428745983553979,0.000105448247628158));
#37943=DIRECTION('ref_axis',(0.428715134343002,0.903357068406648,-0.0122204969215573));
#37944=DIRECTION('center_axis',(-0.356511776579108,0.934290824606,9.06501467950618E-5));
#37945=DIRECTION('ref_axis',(0.934192357613078,0.356475608305158,-0.0144837723258434));
#37946=DIRECTION('center_axis',(5.15167520928809E-67,-1.18789542670764E-48,
-1.));
#37947=DIRECTION('ref_axis',(-4.33680868994202E-19,1.,-1.18789542670764E-48));
#37948=DIRECTION('center_axis',(5.15167520928809E-67,-1.18789542670764E-48,
-1.));
#37949=DIRECTION('ref_axis',(0.,1.,0.));
#37950=DIRECTION('center_axis',(0.93427914155167,-0.356542388142199,0.000105448247170392));
#37951=DIRECTION('ref_axis',(0.356516969951772,0.934208921807903,-0.012220497163456));
#37952=DIRECTION('center_axis',(-0.428716382997142,0.903439126190801,9.06501468381065E-5));
#37953=DIRECTION('ref_axis',(0.903343800468038,0.42867260058632,-0.0144837723857595));
#37954=DIRECTION('center_axis',(5.15167520928809E-67,-1.18789542670764E-48,
-1.));
#37955=DIRECTION('ref_axis',(-4.33680868994202E-19,1.,-1.18789542670764E-48));
#37956=DIRECTION('center_axis',(5.15167520928809E-67,-1.18789542670764E-48,
-1.));
#37957=DIRECTION('ref_axis',(0.,1.,0.));
#37958=DIRECTION('center_axis',(0.959373064120116,-0.282140590347164,0.000105448247729292));
#37959=DIRECTION('ref_axis',(0.282120759890968,0.959301066555056,-0.0122204969160199));
#37960=DIRECTION('center_axis',(-0.498277810351142,0.867017425138747,9.06501467342992E-5));
#37961=DIRECTION('ref_axis',(0.866925828401964,0.498226683737,-0.0144837723677419));
#37962=DIRECTION('center_axis',(5.15167520928809E-67,-1.18789542670764E-48,
-1.));
#37963=DIRECTION('ref_axis',(-4.33680868994202E-19,1.,-1.18789542670764E-48));
#37964=DIRECTION('center_axis',(5.15167520928809E-67,-1.18789542670764E-48,
-1.));
#37965=DIRECTION('ref_axis',(0.,1.,0.));
#37966=DIRECTION('center_axis',(0.978552132724802,-0.205999301990102,0.000105448247615573));
#37967=DIRECTION('ref_axis',(0.205985181528349,0.978478801224133,-0.0122204969505153));
#37968=DIRECTION('center_axis',(-0.564767189310334,0.825250273348065,9.0650146758551E-5));
#37969=DIRECTION('ref_axis',(0.82516297032109,0.564709033705155,-0.014483772390721));
#37970=DIRECTION('center_axis',(5.15167520928809E-67,-1.18789542670764E-48,
-1.));
#37971=DIRECTION('ref_axis',(-4.33680868994202E-19,1.,-1.18789542670764E-48));
#37972=DIRECTION('center_axis',(5.15167520928809E-67,-1.18789542670764E-48,
-1.));
#37973=DIRECTION('ref_axis',(0.,1.,0.));
#37974=DIRECTION('center_axis',(0.991698102030069,-0.128587959430995,0.000105448245943976));
#37975=DIRECTION('ref_axis',(0.128579636019992,0.99162388869792,-0.0122204977223251));
#37976=DIRECTION('center_axis',(-0.627774590743336,0.778395179198579,9.06501467764949E-5));
#37977=DIRECTION('ref_axis',(0.778312708134504,0.627709764696415,-0.014483772336843));
#37978=DIRECTION('center_axis',(5.15167520928809E-67,-1.18789542670764E-48,
-1.));
#37979=DIRECTION('ref_axis',(-4.33680868994202E-19,1.,-1.18789542670764E-48));
#37980=DIRECTION('center_axis',(5.15167520928809E-67,-1.18789542670764E-48,
-1.));
#37981=DIRECTION('ref_axis',(0.,1.,0.));
#37982=DIRECTION('center_axis',(0.998729922762269,-0.0503838293497056,0.000105448247690158));
#37983=DIRECTION('ref_axis',(0.0503813543083624,0.998655285167543,-0.0122204969206726));
#37984=DIRECTION('center_axis',(-0.686911553068082,0.726741019926732,9.065014676939E-5));
#37985=DIRECTION('ref_axis',(0.726663889285701,0.686840456252424,-0.0144837724071123));
#37986=DIRECTION('center_axis',(5.15167520928809E-67,-1.18789542670764E-48,
-1.));
#37987=DIRECTION('ref_axis',(-4.33680868994202E-19,1.,-1.18789542670764E-48));
#37988=DIRECTION('center_axis',(5.15167520928809E-67,-1.18789542670764E-48,
-1.));
#37989=DIRECTION('ref_axis',(0.,1.,0.));
#37990=DIRECTION('center_axis',(0.999604241409737,0.0281309337977193,0.000105448247673278));
#37991=DIRECTION('ref_axis',(0.0281275452111183,-0.999529639707527,0.0122204969841135));
#37992=DIRECTION('center_axis',(-0.741813477246845,0.670606260601179,9.06501467534462E-5));
#37993=DIRECTION('ref_axis',(0.670534945920493,0.741736547999089,-0.0144837723606804));
#37994=DIRECTION('center_axis',(5.15167520928809E-67,-1.18789542670764E-48,
-1.));
#37995=DIRECTION('ref_axis',(-4.33680868994202E-19,1.,-1.18789542670764E-48));
#37996=DIRECTION('center_axis',(5.15167520928809E-67,-1.18789542670764E-48,
-1.));
#37997=DIRECTION('ref_axis',(0.,1.,0.));
#37998=DIRECTION('center_axis',(0.994315667506773,0.106472260383761,0.000105448247684943));
#37999=DIRECTION('ref_axis',(0.106463029060952,-0.994241561642206,0.0122204969798675));
#38000=DIRECTION('center_axis',(-0.792141874660476,0.610336990679688,9.06501468075157E-5));
#38001=DIRECTION('ref_axis',(0.610271931637649,0.792059587274653,-0.0144837723525293));
#38002=DIRECTION('center_axis',(5.15167520928809E-67,-1.18789542670764E-48,
-1.));
#38003=DIRECTION('ref_axis',(-4.33680868994202E-19,1.,-1.18789542670764E-48));
#38004=DIRECTION('center_axis',(5.15167520928809E-67,-1.18789542670764E-48,
-1.));
#38005=DIRECTION('ref_axis',(0.,1.,0.));
#38006=DIRECTION('center_axis',(0.982896806870138,0.184157150078822,0.000105448247739781));
#38007=DIRECTION('ref_axis',(0.184142132934029,-0.982823653730722,0.0122204969580191));
#38008=DIRECTION('center_axis',(-0.837586454002804,0.546304790253169,9.06501467452083E-5));
#38009=DIRECTION('ref_axis',(0.546246387960594,0.837499315808325,-0.0144837723191043));
#38010=DIRECTION('center_axis',(5.15167520928809E-67,-1.18789542670764E-48,
-1.));
#38011=DIRECTION('ref_axis',(-4.33680868994202E-19,1.,-1.18789542670764E-48));
#38012=DIRECTION('center_axis',(5.15167520928809E-67,-1.18789542670764E-48,
-1.));
#38013=DIRECTION('ref_axis',(0.,1.,0.));
#38014=DIRECTION('center_axis',(-0.778395179198544,-0.62777459074338,9.06501468008605E-5));
#38015=DIRECTION('ref_axis',(0.62770976469586,-0.778312708133716,0.0144837724032618));
#38016=DIRECTION('center_axis',(5.15167520928809E-67,-1.18789542670764E-48,
-1.));
#38017=DIRECTION('ref_axis',(-4.33680868994202E-19,1.,-1.18789542670764E-48));
#38018=DIRECTION('center_axis',(0.128587959434843,0.991698102029569,0.000105448247713068));
#38019=DIRECTION('ref_axis',(0.991623888707174,-0.128579636025041,0.0122204969182792));
#38020=DIRECTION('center_axis',(5.15167520928809E-67,-1.18789542670764E-48,
-1.));
#38021=DIRECTION('ref_axis',(0.,1.,0.));
#38022=DIRECTION('center_axis',(-0.82525027334801,-0.564767189310415,9.06501467887519E-5));
#38023=DIRECTION('ref_axis',(0.56470903370554,-0.825162970321483,0.0144837723533119));
#38024=DIRECTION('center_axis',(5.15167520928809E-67,-1.18789542670764E-48,
-1.));
#38025=DIRECTION('ref_axis',(-4.33680868994202E-19,1.,-1.18789542670764E-48));
#38026=DIRECTION('center_axis',(0.205999301990312,0.978552132724757,0.000105448247717959));
#38027=DIRECTION('ref_axis',(0.978478801224664,-0.205985181528676,0.0122204969024898));
#38028=DIRECTION('center_axis',(5.15167520928809E-67,-1.18789542670764E-48,
-1.));
#38029=DIRECTION('ref_axis',(0.,1.,0.));
#38030=DIRECTION('center_axis',(-0.867017425138643,-0.498277810351323,9.06501468256068E-5));
#38031=DIRECTION('ref_axis',(0.498226683737087,-0.866925828401692,0.014483772381015));
#38032=DIRECTION('center_axis',(5.15167520928809E-67,-1.18789542670764E-48,
-1.));
#38033=DIRECTION('ref_axis',(-4.33680868994202E-19,1.,-1.18789542670764E-48));
#38034=DIRECTION('center_axis',(0.282140590347035,0.959373064120154,0.000105448247634384));
#38035=DIRECTION('ref_axis',(0.959301066555324,-0.282120759890904,0.0122204968965099));
#38036=DIRECTION('center_axis',(5.15167520928809E-67,-1.18789542670764E-48,
-1.));
#38037=DIRECTION('ref_axis',(0.,1.,0.));
#38038=DIRECTION('center_axis',(-0.903439126190879,-0.428716382996979,9.06501467301661E-5));
#38039=DIRECTION('ref_axis',(0.428672600586422,-0.903343800468688,0.0144837723422516));
#38040=DIRECTION('center_axis',(5.15167520928809E-67,-1.18789542670764E-48,
-1.));
#38041=DIRECTION('ref_axis',(-4.33680868994202E-19,1.,-1.18789542670764E-48));
#38042=DIRECTION('center_axis',(0.356542388143256,0.934279141551266,0.000105448247681697));
#38043=DIRECTION('ref_axis',(0.934208921810558,-0.356516969953973,0.0122204968962765));
#38044=DIRECTION('center_axis',(5.15167520928809E-67,-1.18789542670764E-48,
-1.));
#38045=DIRECTION('ref_axis',(0.,1.,0.));
#38046=DIRECTION('center_axis',(-0.934290824606111,-0.356511776578816,9.06501466618288E-5));
#38047=DIRECTION('ref_axis',(0.356475608304419,-0.934192357612002,0.0144837724134131));
#38048=DIRECTION('center_axis',(5.15167520928809E-67,-1.18789542670764E-48,
-1.));
#38049=DIRECTION('ref_axis',(-4.33680868994202E-19,1.,-1.18789542670764E-48));
#38050=DIRECTION('center_axis',(0.428745983554273,0.903425077395324,0.000105448247749283));
#38051=DIRECTION('ref_axis',(0.903357068406257,-0.428715134343181,0.0122204969441668));
#38052=DIRECTION('center_axis',(5.15167520928809E-67,-1.18789542670764E-48,
-1.));
#38053=DIRECTION('ref_axis',(0.,1.,0.));
#38054=DIRECTION('center_axis',(-0.959382309404256,-0.282109156506322,9.06501468215648E-5));
#38055=DIRECTION('ref_axis',(0.282080825358184,-0.959281308221691,0.0144837723582998));
#38056=DIRECTION('center_axis',(5.15167520928809E-67,-1.18789542670764E-48,
-1.));
#38057=DIRECTION('ref_axis',(-4.33680868994202E-19,1.,-1.18789542670764E-48));
#38058=DIRECTION('center_axis',(0.498306217397306,0.86700109722183,0.000105448244261109));
#38059=DIRECTION('ref_axis',(0.866935718266673,-0.498270127351015,0.0122204984779969));
#38060=DIRECTION('center_axis',(5.15167520928809E-67,-1.18789542670764E-48,
-1.));
#38061=DIRECTION('ref_axis',(0.,1.,0.));
#38062=DIRECTION('center_axis',(-0.978558883238081,-0.205967239672699,9.06501467769327E-5));
#38063=DIRECTION('ref_axis',(0.205946920321355,-0.978455970571544,0.0144837724038677));
#38064=DIRECTION('center_axis',(5.15167520928809E-67,-1.18789542670764E-48,
-1.));
#38065=DIRECTION('ref_axis',(-4.33680868994202E-19,1.,-1.18789542670764E-48));
#38066=DIRECTION('center_axis',(0.564794227718686,0.825231766969935,0.000105448247134299));
#38067=DIRECTION('ref_axis',(0.825169421162366,-0.564753119361502,0.0122204971264834));
#38068=DIRECTION('center_axis',(5.15167520928809E-67,-1.18789542670764E-48,
-1.));
#38069=DIRECTION('ref_axis',(0.,1.,0.));
#38070=DIRECTION('center_axis',(-0.991702316152861,-0.128555466315523,9.06501467288715E-5));
#38071=DIRECTION('ref_axis',(0.12854328403675,-0.991598126494102,0.0144837723826971));
#38072=DIRECTION('center_axis',(5.15167520928809E-67,-1.18789542670764E-48,
-1.));
#38073=DIRECTION('ref_axis',(-4.33680868994202E-19,1.,-1.18789542670764E-48));
#38074=DIRECTION('center_axis',(0.627800093808552,0.778374608459603,0.000105448247728723));
#38075=DIRECTION('ref_axis',(0.778315680170199,-0.627754220580874,0.0122204968843025));
#38076=DIRECTION('center_axis',(5.15167520928809E-67,-1.18789542670764E-48,
-1.));
#38077=DIRECTION('ref_axis',(0.,1.,0.));
#38078=DIRECTION('center_axis',(-0.998731574514058,-0.0503511057596628,
9.06501468007229E-5));
#38079=DIRECTION('ref_axis',(0.0503471356611987,-0.998626750226619,0.0144837723861814));
#38080=DIRECTION('center_axis',(5.15167520928809E-67,-1.18789542670764E-48,
-1.));
#38081=DIRECTION('ref_axis',(-4.33680868994202E-19,1.,-1.18789542670764E-48));
#38082=DIRECTION('center_axis',(0.686935363554282,0.726718511653043,0.000105448247718559));
#38083=DIRECTION('ref_axis',(0.726663364191442,-0.686885008277775,0.012220496930023));
#38084=DIRECTION('center_axis',(5.15167520928809E-67,-1.18789542670764E-48,
-1.));
#38085=DIRECTION('ref_axis',(0.,1.,0.));
#38086=DIRECTION('center_axis',(-0.99960332060644,0.0281636861069471,9.06501467308329E-5));
#38087=DIRECTION('ref_axis',(0.0281594195481261,0.999498507967114,-0.0144837723754724));
#38088=DIRECTION('center_axis',(5.15167520928809E-67,-1.18789542670764E-48,
-1.));
#38089=DIRECTION('ref_axis',(-4.33680868994202E-19,1.,-1.18789542670764E-48));
#38090=DIRECTION('center_axis',(0.741835448354451,0.670581953563782,0.00010544824772104));
#38091=DIRECTION('ref_axis',(0.670530926933101,-0.74178092148675,0.0122204969008548));
#38092=DIRECTION('center_axis',(5.15167520928809E-67,-1.18789542670764E-48,
-1.));
#38093=DIRECTION('ref_axis',(0.,1.,0.));
#38094=DIRECTION('center_axis',(-0.994312179825441,0.106504839483146,9.06501467381912E-5));
#38095=DIRECTION('ref_axis',(0.106492362571802,0.99420802503887,-0.0144837723741357));
#38096=DIRECTION('center_axis',(5.15167520928809E-67,-1.18789542670764E-48,
-1.));
#38097=DIRECTION('ref_axis',(-4.33680868994202E-19,1.,-1.18789542670764E-48));
#38098=DIRECTION('center_axis',(0.792161870929241,0.610311034740936,0.000105448246928053));
#38099=DIRECTION('ref_axis',(0.610264443534212,-0.792103508642726,0.0122204972796185));
#38100=DIRECTION('center_axis',(5.15167520928809E-67,-1.18789542670764E-48,
-1.));
#38101=DIRECTION('ref_axis',(0.,1.,0.));
#38102=DIRECTION('center_axis',(-0.982890773813477,0.184189355107443,9.06501467544422E-5));
#38103=DIRECTION('ref_axis',(0.184168744767819,0.982787919028209,-0.0144837723970302));
#38104=DIRECTION('center_axis',(5.15167520928809E-67,-1.18789542670764E-48,
-1.));
#38105=DIRECTION('ref_axis',(-4.33680868994202E-19,1.,-1.18789542670764E-48));
#38106=DIRECTION('center_axis',(0.837604352151223,0.546277345437276,0.000105448247675196));
#38107=DIRECTION('ref_axis',(0.546235476910048,-0.837542514275434,0.0122204969635834));
#38108=DIRECTION('center_axis',(5.15167520928809E-67,-1.18789542670764E-48,
-1.));
#38109=DIRECTION('ref_axis',(0.,1.,0.));
#38110=DIRECTION('center_axis',(-0.96540951933663,0.260738282108263,9.06501468112521E-5));
#38111=DIRECTION('ref_axis',(0.26070966540993,0.965308598686718,-0.0144837724135372));
#38112=DIRECTION('center_axis',(5.15167520928809E-67,-1.18789542670764E-48,
-1.));
#38113=DIRECTION('ref_axis',(-4.33680868994202E-19,1.,-1.18789542670764E-48));
#38114=DIRECTION('center_axis',(0.877882724009476,0.478875674644651,0.000105448247670176));
#38115=DIRECTION('ref_axis',(0.478838786927941,-0.877817791792444,0.0122204969627255));
#38116=DIRECTION('center_axis',(5.15167520928809E-67,-1.18789542670764E-48,
-1.));
#38117=DIRECTION('ref_axis',(0.,1.,0.));
#38118=DIRECTION('center_axis',(-0.941976194141744,0.33567967089591,9.06501467361574E-5));
#38119=DIRECTION('ref_axis',(0.335643224270696,0.941877829837669,-0.0144837723488913));
#38120=DIRECTION('center_axis',(5.15167520928809E-67,-1.18789542670764E-48,
-1.));
#38121=DIRECTION('ref_axis',(-4.33680868994202E-19,1.,-1.18789542670764E-48));
#38122=DIRECTION('center_axis',(0.912748656948457,0.408521576075799,0.000105448247549386));
#38123=DIRECTION('ref_axis',(0.408489896594413,-0.912681030718381,0.0122204970078645));
#38124=DIRECTION('center_axis',(5.15167520928809E-67,-1.18789542670764E-48,
-1.));
#38125=DIRECTION('ref_axis',(0.,1.,0.));
#38126=DIRECTION('center_axis',(0.965418060567994,0.260706649723021,0.000105448239440975));
#38127=DIRECTION('ref_axis',(0.260685939330027,-0.965346311123993,0.0122205006002244));
#38128=DIRECTION('center_axis',(-0.877867034330543,0.478904439129822,9.06501467527618E-5));
#38129=DIRECTION('ref_axis',(0.478853053655558,0.877775582562237,-0.014483772377146));
#38130=DIRECTION('center_axis',(5.15167520928809E-67,-1.18789542670764E-48,
-1.));
#38131=DIRECTION('ref_axis',(-4.33680868994202E-19,1.,-1.18789542670764E-48));
#38132=DIRECTION('center_axis',(5.15167520928809E-67,-1.18789542670764E-48,
-1.));
#38133=DIRECTION('ref_axis',(-4.33680868994202E-19,1.,-1.18789542670764E-48));
#38134=DIRECTION('',(5.15167520928809E-67,-1.18789542670764E-48,-1.));
#38135=DIRECTION('center_axis',(5.15167520928809E-67,-1.18789542670764E-48,
-1.));
#38136=DIRECTION('ref_axis',(-4.33680868994202E-19,1.,-1.18789542670764E-48));
#38137=DIRECTION('',(-5.15167520928809E-67,1.18789542670764E-48,1.));
#38138=DIRECTION('center_axis',(5.15167520928809E-67,-1.18789542670764E-48,
-1.));
#38139=DIRECTION('ref_axis',(-4.33680868994202E-19,1.,-1.18789542670764E-48));
#38140=DIRECTION('',(-5.15167520928809E-67,1.18789542670764E-48,1.));
#38141=DIRECTION('',(5.15167520928809E-67,-1.18789542670764E-48,-1.));
#38142=DIRECTION('center_axis',(5.15167520928809E-67,-1.18789542670764E-48,
-1.));
#38143=DIRECTION('ref_axis',(-4.33680868994202E-19,1.,-1.18789542670764E-48));
#38144=DIRECTION('center_axis',(5.15167520928809E-67,-1.18789542670764E-48,
-1.));
#38145=DIRECTION('ref_axis',(-4.33680868994202E-19,1.,-1.18789542670764E-48));
#38146=DIRECTION('',(-5.15167520928809E-67,1.18789542670764E-48,1.));
#38147=DIRECTION('',(5.15167520928809E-67,-1.18789542670764E-48,-1.));
#38148=DIRECTION('center_axis',(5.15167520928809E-67,-1.18789542670764E-48,
-1.));
#38149=DIRECTION('ref_axis',(-4.33680868994202E-19,1.,-1.18789542670764E-48));
#38150=DIRECTION('center_axis',(5.15167520928809E-67,-1.18789542670764E-48,
-1.));
#38151=DIRECTION('ref_axis',(-4.33680868994202E-19,1.,-1.18789542670764E-48));
#38152=DIRECTION('',(-5.15167520928809E-67,1.18789542670764E-48,1.));
#38153=DIRECTION('',(5.15167520928809E-67,-1.18789542670764E-48,-1.));
#38154=DIRECTION('center_axis',(5.15167520928809E-67,-1.18789542670764E-48,
-1.));
#38155=DIRECTION('ref_axis',(-4.33680868994202E-19,1.,-1.18789542670764E-48));
#38156=DIRECTION('center_axis',(5.15167520928809E-67,-1.18789542670764E-48,
-1.));
#38157=DIRECTION('ref_axis',(-4.33680868994202E-19,1.,-1.18789542670764E-48));
#38158=DIRECTION('',(-5.15167520928809E-67,1.18789542670764E-48,1.));
#38159=DIRECTION('',(5.15167520928809E-67,-1.18789542670764E-48,-1.));
#38160=DIRECTION('center_axis',(5.15167520928809E-67,-1.18789542670764E-48,
-1.));
#38161=DIRECTION('ref_axis',(-4.33680868994202E-19,1.,-1.18789542670764E-48));
#38162=DIRECTION('center_axis',(5.15167520928809E-67,-1.18789542670764E-48,
-1.));
#38163=DIRECTION('ref_axis',(-4.33680868994202E-19,1.,-1.18789542670764E-48));
#38164=DIRECTION('',(-5.15167520928809E-67,1.18789542670764E-48,1.));
#38165=DIRECTION('',(5.15167520928809E-67,-1.18789542670764E-48,-1.));
#38166=DIRECTION('center_axis',(5.15167520928809E-67,-1.18789542670764E-48,
-1.));
#38167=DIRECTION('ref_axis',(-4.33680868994202E-19,1.,-1.18789542670764E-48));
#38168=DIRECTION('center_axis',(5.15167520928809E-67,-1.18789542670764E-48,
-1.));
#38169=DIRECTION('ref_axis',(-4.33680868994202E-19,1.,-1.18789542670764E-48));
#38170=DIRECTION('',(-5.15167520928809E-67,1.18789542670764E-48,1.));
#38171=DIRECTION('',(5.15167520928809E-67,-1.18789542670764E-48,-1.));
#38172=DIRECTION('center_axis',(5.15167520928809E-67,-1.18789542670764E-48,
-1.));
#38173=DIRECTION('ref_axis',(-4.33680868994202E-19,1.,-1.18789542670764E-48));
#38174=DIRECTION('center_axis',(5.15167520928809E-67,-1.18789542670764E-48,
-1.));
#38175=DIRECTION('ref_axis',(-4.33680868994202E-19,1.,-1.18789542670764E-48));
#38176=DIRECTION('',(-5.15167520928809E-67,1.18789542670764E-48,1.));
#38177=DIRECTION('',(5.15167520928809E-67,-1.18789542670764E-48,-1.));
#38178=DIRECTION('center_axis',(5.15167520928809E-67,-1.18789542670764E-48,
-1.));
#38179=DIRECTION('ref_axis',(-4.33680868994202E-19,1.,-1.18789542670764E-48));
#38180=DIRECTION('center_axis',(5.15167520928809E-67,-1.18789542670764E-48,
-1.));
#38181=DIRECTION('ref_axis',(-4.33680868994202E-19,1.,-1.18789542670764E-48));
#38182=DIRECTION('',(-5.15167520928809E-67,1.18789542670764E-48,1.));
#38183=DIRECTION('',(5.15167520928809E-67,-1.18789542670764E-48,-1.));
#38184=DIRECTION('center_axis',(5.15167520928809E-67,-1.18789542670764E-48,
-1.));
#38185=DIRECTION('ref_axis',(-4.33680868994202E-19,1.,-1.18789542670764E-48));
#38186=DIRECTION('center_axis',(5.15167520928809E-67,-1.18789542670764E-48,
-1.));
#38187=DIRECTION('ref_axis',(-4.33680868994202E-19,1.,-1.18789542670764E-48));
#38188=DIRECTION('',(-5.15167520928809E-67,1.18789542670764E-48,1.));
#38189=DIRECTION('',(5.15167520928809E-67,-1.18789542670764E-48,-1.));
#38190=DIRECTION('center_axis',(5.15167520928809E-67,-1.18789542670764E-48,
-1.));
#38191=DIRECTION('ref_axis',(-4.33680868994202E-19,1.,-1.18789542670764E-48));
#38192=DIRECTION('center_axis',(5.15167520928809E-67,-1.18789542670764E-48,
-1.));
#38193=DIRECTION('ref_axis',(-4.33680868994202E-19,1.,-1.18789542670764E-48));
#38194=DIRECTION('',(-5.15167520928809E-67,1.18789542670764E-48,1.));
#38195=DIRECTION('',(5.15167520928809E-67,-1.18789542670764E-48,-1.));
#38196=DIRECTION('center_axis',(5.15167520928809E-67,-1.18789542670764E-48,
-1.));
#38197=DIRECTION('ref_axis',(-4.33680868994202E-19,1.,-1.18789542670764E-48));
#38198=DIRECTION('center_axis',(5.15167520928809E-67,-1.18789542670764E-48,
-1.));
#38199=DIRECTION('ref_axis',(-4.33680868994202E-19,1.,-1.18789542670764E-48));
#38200=DIRECTION('',(-5.15167520928809E-67,1.18789542670764E-48,1.));
#38201=DIRECTION('',(5.15167520928809E-67,-1.18789542670764E-48,-1.));
#38202=DIRECTION('center_axis',(5.15167520928809E-67,-1.18789542670764E-48,
-1.));
#38203=DIRECTION('ref_axis',(-4.33680868994202E-19,1.,-1.18789542670764E-48));
#38204=DIRECTION('center_axis',(5.15167520928809E-67,-1.18789542670764E-48,
-1.));
#38205=DIRECTION('ref_axis',(-4.33680868994202E-19,1.,-1.18789542670764E-48));
#38206=DIRECTION('',(-5.15167520928809E-67,1.18789542670764E-48,1.));
#38207=DIRECTION('',(5.15167520928809E-67,-1.18789542670764E-48,-1.));
#38208=DIRECTION('center_axis',(5.15167520928809E-67,-1.18789542670764E-48,
-1.));
#38209=DIRECTION('ref_axis',(-4.33680868994202E-19,1.,-1.18789542670764E-48));
#38210=DIRECTION('center_axis',(5.15167520928809E-67,-1.18789542670764E-48,
-1.));
#38211=DIRECTION('ref_axis',(-4.33680868994202E-19,1.,-1.18789542670764E-48));
#38212=DIRECTION('',(-5.15167520928809E-67,1.18789542670764E-48,1.));
#38213=DIRECTION('',(5.15167520928809E-67,-1.18789542670764E-48,-1.));
#38214=DIRECTION('center_axis',(5.15167520928809E-67,-1.18789542670764E-48,
-1.));
#38215=DIRECTION('ref_axis',(-4.33680868994202E-19,1.,-1.18789542670764E-48));
#38216=DIRECTION('center_axis',(5.15167520928809E-67,-1.18789542670764E-48,
-1.));
#38217=DIRECTION('ref_axis',(-4.33680868994202E-19,1.,-1.18789542670764E-48));
#38218=DIRECTION('',(-5.15167520928809E-67,1.18789542670764E-48,1.));
#38219=DIRECTION('',(5.15167520928809E-67,-1.18789542670764E-48,-1.));
#38220=DIRECTION('center_axis',(5.15167520928809E-67,-1.18789542670764E-48,
-1.));
#38221=DIRECTION('ref_axis',(-4.33680868994202E-19,1.,-1.18789542670764E-48));
#38222=DIRECTION('center_axis',(5.15167520928809E-67,-1.18789542670764E-48,
-1.));
#38223=DIRECTION('ref_axis',(-4.33680868994202E-19,1.,-1.18789542670764E-48));
#38224=DIRECTION('',(-5.15167520928809E-67,1.18789542670764E-48,1.));
#38225=DIRECTION('',(5.15167520928809E-67,-1.18789542670764E-48,-1.));
#38226=DIRECTION('center_axis',(5.15167520928809E-67,-1.18789542670764E-48,
-1.));
#38227=DIRECTION('ref_axis',(-4.33680868994202E-19,1.,-1.18789542670764E-48));
#38228=DIRECTION('center_axis',(5.15167520928809E-67,-1.18789542670764E-48,
-1.));
#38229=DIRECTION('ref_axis',(-4.33680868994202E-19,1.,-1.18789542670764E-48));
#38230=DIRECTION('',(-5.15167520928809E-67,1.18789542670764E-48,1.));
#38231=DIRECTION('',(5.15167520928809E-67,-1.18789542670764E-48,-1.));
#38232=DIRECTION('center_axis',(5.15167520928809E-67,-1.18789542670764E-48,
-1.));
#38233=DIRECTION('ref_axis',(-4.33680868994202E-19,1.,-1.18789542670764E-48));
#38234=DIRECTION('center_axis',(5.15167520928809E-67,-1.18789542670764E-48,
-1.));
#38235=DIRECTION('ref_axis',(-4.33680868994202E-19,1.,-1.18789542670764E-48));
#38236=DIRECTION('',(-5.15167520928809E-67,1.18789542670764E-48,1.));
#38237=DIRECTION('',(5.15167520928809E-67,-1.18789542670764E-48,-1.));
#38238=DIRECTION('center_axis',(5.15167520928809E-67,-1.18789542670764E-48,
-1.));
#38239=DIRECTION('ref_axis',(-4.33680868994202E-19,1.,-1.18789542670764E-48));
#38240=DIRECTION('center_axis',(5.15167520928809E-67,-1.18789542670764E-48,
-1.));
#38241=DIRECTION('ref_axis',(-4.33680868994202E-19,1.,-1.18789542670764E-48));
#38242=DIRECTION('',(-5.15167520928809E-67,1.18789542670764E-48,1.));
#38243=DIRECTION('',(5.15167520928809E-67,-1.18789542670764E-48,-1.));
#38244=DIRECTION('center_axis',(5.15167520928809E-67,-1.18789542670764E-48,
-1.));
#38245=DIRECTION('ref_axis',(-4.33680868994202E-19,1.,-1.18789542670764E-48));
#38246=DIRECTION('center_axis',(5.15167520928809E-67,-1.18789542670764E-48,
-1.));
#38247=DIRECTION('ref_axis',(-4.33680868994202E-19,1.,-1.18789542670764E-48));
#38248=DIRECTION('',(-5.15167520928809E-67,1.18789542670764E-48,1.));
#38249=DIRECTION('',(5.15167520928809E-67,-1.18789542670764E-48,-1.));
#38250=DIRECTION('center_axis',(5.15167520928809E-67,-1.18789542670764E-48,
-1.));
#38251=DIRECTION('ref_axis',(-4.33680868994202E-19,1.,-1.18789542670764E-48));
#38252=DIRECTION('center_axis',(5.15167520928809E-67,-1.18789542670764E-48,
-1.));
#38253=DIRECTION('ref_axis',(-4.33680868994202E-19,1.,-1.18789542670764E-48));
#38254=DIRECTION('',(-5.15167520928809E-67,1.18789542670764E-48,1.));
#38255=DIRECTION('',(5.15167520928809E-67,-1.18789542670764E-48,-1.));
#38256=DIRECTION('center_axis',(5.15167520928809E-67,-1.18789542670764E-48,
-1.));
#38257=DIRECTION('ref_axis',(-4.33680868994202E-19,1.,-1.18789542670764E-48));
#38258=DIRECTION('center_axis',(5.15167520928809E-67,-1.18789542670764E-48,
-1.));
#38259=DIRECTION('ref_axis',(-4.33680868994202E-19,1.,-1.18789542670764E-48));
#38260=DIRECTION('',(-5.15167520928809E-67,1.18789542670764E-48,1.));
#38261=DIRECTION('',(5.15167520928809E-67,-1.18789542670764E-48,-1.));
#38262=DIRECTION('center_axis',(5.15167520928809E-67,-1.18789542670764E-48,
-1.));
#38263=DIRECTION('ref_axis',(-4.33680868994202E-19,1.,-1.18789542670764E-48));
#38264=DIRECTION('center_axis',(5.15167520928809E-67,-1.18789542670764E-48,
-1.));
#38265=DIRECTION('ref_axis',(-4.33680868994202E-19,1.,-1.18789542670764E-48));
#38266=DIRECTION('',(-5.15167520928809E-67,1.18789542670764E-48,1.));
#38267=DIRECTION('',(5.15167520928809E-67,-1.18789542670764E-48,-1.));
#38268=DIRECTION('center_axis',(5.15167520928809E-67,-1.18789542670764E-48,
-1.));
#38269=DIRECTION('ref_axis',(-4.33680868994202E-19,1.,-1.18789542670764E-48));
#38270=DIRECTION('center_axis',(5.15167520928809E-67,-1.18789542670764E-48,
-1.));
#38271=DIRECTION('ref_axis',(-4.33680868994202E-19,1.,-1.18789542670764E-48));
#38272=DIRECTION('',(-5.15167520928809E-67,1.18789542670764E-48,1.));
#38273=DIRECTION('',(5.15167520928809E-67,-1.18789542670764E-48,-1.));
#38274=DIRECTION('center_axis',(5.15167520928809E-67,-1.18789542670764E-48,
-1.));
#38275=DIRECTION('ref_axis',(-4.33680868994202E-19,1.,-1.18789542670764E-48));
#38276=DIRECTION('center_axis',(5.15167520928809E-67,-1.18789542670764E-48,
-1.));
#38277=DIRECTION('ref_axis',(-4.33680868994202E-19,1.,-1.18789542670764E-48));
#38278=DIRECTION('',(-5.15167520928809E-67,1.18789542670764E-48,1.));
#38279=DIRECTION('',(5.15167520928809E-67,-1.18789542670764E-48,-1.));
#38280=DIRECTION('center_axis',(5.15167520928809E-67,-1.18789542670764E-48,
-1.));
#38281=DIRECTION('ref_axis',(-4.33680868994202E-19,1.,-1.18789542670764E-48));
#38282=DIRECTION('center_axis',(5.15167520928809E-67,-1.18789542670764E-48,
-1.));
#38283=DIRECTION('ref_axis',(-4.33680868994202E-19,1.,-1.18789542670764E-48));
#38284=DIRECTION('',(-5.15167520928809E-67,1.18789542670764E-48,1.));
#38285=DIRECTION('',(5.15167520928809E-67,-1.18789542670764E-48,-1.));
#38286=DIRECTION('center_axis',(5.15167520928809E-67,-1.18789542670764E-48,
-1.));
#38287=DIRECTION('ref_axis',(-4.33680868994202E-19,1.,-1.18789542670764E-48));
#38288=DIRECTION('center_axis',(5.15167520928809E-67,-1.18789542670764E-48,
-1.));
#38289=DIRECTION('ref_axis',(-4.33680868994202E-19,1.,-1.18789542670764E-48));
#38290=DIRECTION('',(-5.15167520928809E-67,1.18789542670764E-48,1.));
#38291=DIRECTION('',(5.15167520928809E-67,-1.18789542670764E-48,-1.));
#38292=DIRECTION('center_axis',(5.15167520928809E-67,-1.18789542670764E-48,
-1.));
#38293=DIRECTION('ref_axis',(-4.33680868994202E-19,1.,-1.18789542670764E-48));
#38294=DIRECTION('center_axis',(5.15167520928809E-67,-1.18789542670764E-48,
-1.));
#38295=DIRECTION('ref_axis',(-4.33680868994202E-19,1.,-1.18789542670764E-48));
#38296=DIRECTION('',(-5.15167520928809E-67,1.18789542670764E-48,1.));
#38297=DIRECTION('',(5.15167520928809E-67,-1.18789542670764E-48,-1.));
#38298=DIRECTION('center_axis',(5.15167520928809E-67,-1.18789542670764E-48,
-1.));
#38299=DIRECTION('ref_axis',(-4.33680868994202E-19,1.,-1.18789542670764E-48));
#38300=DIRECTION('center_axis',(5.15167520928809E-67,-1.18789542670764E-48,
-1.));
#38301=DIRECTION('ref_axis',(-4.33680868994202E-19,1.,-1.18789542670764E-48));
#38302=DIRECTION('',(-5.15167520928809E-67,1.18789542670764E-48,1.));
#38303=DIRECTION('',(5.15167520928809E-67,-1.18789542670764E-48,-1.));
#38304=DIRECTION('center_axis',(5.15167520928809E-67,-1.18789542670764E-48,
-1.));
#38305=DIRECTION('ref_axis',(-4.33680868994202E-19,1.,-1.18789542670764E-48));
#38306=DIRECTION('center_axis',(5.15167520928809E-67,-1.18789542670764E-48,
-1.));
#38307=DIRECTION('ref_axis',(-4.33680868994202E-19,1.,-1.18789542670764E-48));
#38308=DIRECTION('',(-5.15167520928809E-67,1.18789542670764E-48,1.));
#38309=DIRECTION('',(5.15167520928809E-67,-1.18789542670764E-48,-1.));
#38310=DIRECTION('center_axis',(5.15167520928809E-67,-1.18789542670764E-48,
-1.));
#38311=DIRECTION('ref_axis',(-4.33680868994202E-19,1.,-1.18789542670764E-48));
#38312=DIRECTION('center_axis',(5.15167520928809E-67,-1.18789542670764E-48,
-1.));
#38313=DIRECTION('ref_axis',(-4.33680868994202E-19,1.,-1.18789542670764E-48));
#38314=DIRECTION('',(-5.15167520928809E-67,1.18789542670764E-48,1.));
#38315=DIRECTION('',(5.15167520928809E-67,-1.18789542670764E-48,-1.));
#38316=DIRECTION('center_axis',(5.15167520928809E-67,-1.18789542670764E-48,
-1.));
#38317=DIRECTION('ref_axis',(-4.33680868994202E-19,1.,-1.18789542670764E-48));
#38318=DIRECTION('center_axis',(5.15167520928809E-67,-1.18789542670764E-48,
-1.));
#38319=DIRECTION('ref_axis',(-4.33680868994202E-19,1.,-1.18789542670764E-48));
#38320=DIRECTION('',(-5.15167520928809E-67,1.18789542670764E-48,1.));
#38321=DIRECTION('',(5.15167520928809E-67,-1.18789542670764E-48,-1.));
#38322=DIRECTION('center_axis',(5.15167520928809E-67,-1.18789542670764E-48,
-1.));
#38323=DIRECTION('ref_axis',(-4.33680868994202E-19,1.,-1.18789542670764E-48));
#38324=DIRECTION('center_axis',(5.15167520928809E-67,-1.18789542670764E-48,
-1.));
#38325=DIRECTION('ref_axis',(-4.33680868994202E-19,1.,-1.18789542670764E-48));
#38326=DIRECTION('',(-5.15167520928809E-67,1.18789542670764E-48,1.));
#38327=DIRECTION('',(5.15167520928809E-67,-1.18789542670764E-48,-1.));
#38328=DIRECTION('center_axis',(5.15167520928809E-67,-1.18789542670764E-48,
-1.));
#38329=DIRECTION('ref_axis',(-4.33680868994202E-19,1.,-1.18789542670764E-48));
#38330=DIRECTION('center_axis',(5.15167520928809E-67,-1.18789542670764E-48,
-1.));
#38331=DIRECTION('ref_axis',(-4.33680868994202E-19,1.,-1.18789542670764E-48));
#38332=DIRECTION('',(-5.15167520928809E-67,1.18789542670764E-48,1.));
#38333=DIRECTION('',(5.15167520928809E-67,-1.18789542670764E-48,-1.));
#38334=DIRECTION('center_axis',(5.15167520928809E-67,-1.18789542670764E-48,
-1.));
#38335=DIRECTION('ref_axis',(-4.33680868994202E-19,1.,-1.18789542670764E-48));
#38336=DIRECTION('center_axis',(5.15167520928809E-67,-1.18789542670764E-48,
-1.));
#38337=DIRECTION('ref_axis',(-4.33680868994202E-19,1.,-1.18789542670764E-48));
#38338=DIRECTION('',(-5.15167520928809E-67,1.18789542670764E-48,1.));
#38339=DIRECTION('',(5.15167520928809E-67,-1.18789542670764E-48,-1.));
#38340=DIRECTION('center_axis',(5.15167520928809E-67,-1.18789542670764E-48,
-1.));
#38341=DIRECTION('ref_axis',(-4.33680868994202E-19,1.,-1.18789542670764E-48));
#38342=DIRECTION('center_axis',(5.15167520928809E-67,-1.18789542670764E-48,
-1.));
#38343=DIRECTION('ref_axis',(-4.33680868994202E-19,1.,-1.18789542670764E-48));
#38344=DIRECTION('',(-5.15167520928809E-67,1.18789542670764E-48,1.));
#38345=DIRECTION('',(5.15167520928809E-67,-1.18789542670764E-48,-1.));
#38346=DIRECTION('center_axis',(5.15167520928809E-67,-1.18789542670764E-48,
-1.));
#38347=DIRECTION('ref_axis',(-4.33680868994202E-19,1.,-1.18789542670764E-48));
#38348=DIRECTION('center_axis',(5.15167520928809E-67,-1.18789542670764E-48,
-1.));
#38349=DIRECTION('ref_axis',(-4.33680868994202E-19,1.,-1.18789542670764E-48));
#38350=DIRECTION('',(-5.15167520928809E-67,1.18789542670764E-48,1.));
#38351=DIRECTION('',(5.15167520928809E-67,-1.18789542670764E-48,-1.));
#38352=DIRECTION('center_axis',(5.15167520928809E-67,-1.18789542670764E-48,
-1.));
#38353=DIRECTION('ref_axis',(-4.33680868994202E-19,1.,-1.18789542670764E-48));
#38354=DIRECTION('center_axis',(5.15167520928809E-67,-1.18789542670764E-48,
-1.));
#38355=DIRECTION('ref_axis',(-4.33680868994202E-19,1.,-1.18789542670764E-48));
#38356=DIRECTION('',(-5.15167520928809E-67,1.18789542670764E-48,1.));
#38357=DIRECTION('',(5.15167520928809E-67,-1.18789542670764E-48,-1.));
#38358=DIRECTION('center_axis',(5.15167520928809E-67,-1.18789542670764E-48,
-1.));
#38359=DIRECTION('ref_axis',(-4.33680868994202E-19,1.,-1.18789542670764E-48));
#38360=DIRECTION('center_axis',(5.15167520928809E-67,-1.18789542670764E-48,
-1.));
#38361=DIRECTION('ref_axis',(-4.33680868994202E-19,1.,-1.18789542670764E-48));
#38362=DIRECTION('',(-5.15167520928809E-67,1.18789542670764E-48,1.));
#38363=DIRECTION('',(5.15167520928809E-67,-1.18789542670764E-48,-1.));
#38364=DIRECTION('center_axis',(5.15167520928809E-67,-1.18789542670764E-48,
-1.));
#38365=DIRECTION('ref_axis',(-4.33680868994202E-19,1.,-1.18789542670764E-48));
#38366=DIRECTION('center_axis',(5.15167520928809E-67,-1.18789542670764E-48,
-1.));
#38367=DIRECTION('ref_axis',(-4.33680868994202E-19,1.,-1.18789542670764E-48));
#38368=DIRECTION('',(-5.15167520928809E-67,1.18789542670764E-48,1.));
#38369=DIRECTION('',(5.15167520928809E-67,-1.18789542670764E-48,-1.));
#38370=DIRECTION('center_axis',(5.15167520928809E-67,-1.18789542670764E-48,
-1.));
#38371=DIRECTION('ref_axis',(-4.33680868994202E-19,1.,-1.18789542670764E-48));
#38372=DIRECTION('center_axis',(5.15167520928809E-67,-1.18789542670764E-48,
-1.));
#38373=DIRECTION('ref_axis',(-4.33680868994202E-19,1.,-1.18789542670764E-48));
#38374=DIRECTION('',(-5.15167520928809E-67,1.18789542670764E-48,1.));
#38375=DIRECTION('',(5.15167520928809E-67,-1.18789542670764E-48,-1.));
#38376=DIRECTION('center_axis',(5.15167520928809E-67,-1.18789542670764E-48,
-1.));
#38377=DIRECTION('ref_axis',(-4.33680868994202E-19,1.,-1.18789542670764E-48));
#38378=DIRECTION('center_axis',(5.15167520928809E-67,-1.18789542670764E-48,
-1.));
#38379=DIRECTION('ref_axis',(-4.33680868994202E-19,1.,-1.18789542670764E-48));
#38380=DIRECTION('',(-5.15167520928809E-67,1.18789542670764E-48,1.));
#38381=DIRECTION('',(5.15167520928809E-67,-1.18789542670764E-48,-1.));
#38382=DIRECTION('center_axis',(5.15167520928809E-67,-1.18789542670764E-48,
-1.));
#38383=DIRECTION('ref_axis',(-4.33680868994202E-19,1.,-1.18789542670764E-48));
#38384=DIRECTION('center_axis',(5.15167520928809E-67,-1.18789542670764E-48,
-1.));
#38385=DIRECTION('ref_axis',(-4.33680868994202E-19,1.,-1.18789542670764E-48));
#38386=DIRECTION('',(-5.15167520928809E-67,1.18789542670764E-48,1.));
#38387=DIRECTION('',(5.15167520928809E-67,-1.18789542670764E-48,-1.));
#38388=DIRECTION('center_axis',(5.15167520928809E-67,-1.18789542670764E-48,
-1.));
#38389=DIRECTION('ref_axis',(-4.33680868994202E-19,1.,-1.18789542670764E-48));
#38390=DIRECTION('center_axis',(5.15167520928809E-67,-1.18789542670764E-48,
-1.));
#38391=DIRECTION('ref_axis',(-4.33680868994202E-19,1.,-1.18789542670764E-48));
#38392=DIRECTION('',(-5.15167520928809E-67,1.18789542670764E-48,1.));
#38393=DIRECTION('',(5.15167520928809E-67,-1.18789542670764E-48,-1.));
#38394=DIRECTION('center_axis',(5.15167520928809E-67,-1.18789542670764E-48,
-1.));
#38395=DIRECTION('ref_axis',(-4.33680868994202E-19,1.,-1.18789542670764E-48));
#38396=DIRECTION('center_axis',(5.15167520928809E-67,-1.18789542670764E-48,
-1.));
#38397=DIRECTION('ref_axis',(-4.33680868994202E-19,1.,-1.18789542670764E-48));
#38398=DIRECTION('',(-5.15167520928809E-67,1.18789542670764E-48,1.));
#38399=DIRECTION('',(5.15167520928809E-67,-1.18789542670764E-48,-1.));
#38400=DIRECTION('center_axis',(5.15167520928809E-67,-1.18789542670764E-48,
-1.));
#38401=DIRECTION('ref_axis',(-4.33680868994202E-19,1.,-1.18789542670764E-48));
#38402=DIRECTION('center_axis',(5.15167520928809E-67,-1.18789542670764E-48,
-1.));
#38403=DIRECTION('ref_axis',(-4.33680868994202E-19,1.,-1.18789542670764E-48));
#38404=DIRECTION('',(-5.15167520928809E-67,1.18789542670764E-48,1.));
#38405=DIRECTION('',(5.15167520928809E-67,-1.18789542670764E-48,-1.));
#38406=DIRECTION('center_axis',(5.15167520928809E-67,-1.18789542670764E-48,
-1.));
#38407=DIRECTION('ref_axis',(-4.33680868994202E-19,1.,-1.18789542670764E-48));
#38408=DIRECTION('center_axis',(5.15167520928809E-67,-1.18789542670764E-48,
-1.));
#38409=DIRECTION('ref_axis',(-4.33680868994202E-19,1.,-1.18789542670764E-48));
#38410=DIRECTION('',(-5.15167520928809E-67,1.18789542670764E-48,1.));
#38411=DIRECTION('',(5.15167520928809E-67,-1.18789542670764E-48,-1.));
#38412=DIRECTION('center_axis',(5.15167520928809E-67,-1.18789542670764E-48,
-1.));
#38413=DIRECTION('ref_axis',(-4.33680868994202E-19,1.,-1.18789542670764E-48));
#38414=DIRECTION('center_axis',(5.15167520928809E-67,-1.18789542670764E-48,
-1.));
#38415=DIRECTION('ref_axis',(-4.33680868994202E-19,1.,-1.18789542670764E-48));
#38416=DIRECTION('',(-5.15167520928809E-67,1.18789542670764E-48,1.));
#38417=DIRECTION('',(5.15167520928809E-67,-1.18789542670764E-48,-1.));
#38418=DIRECTION('center_axis',(5.15167520928809E-67,-1.18789542670764E-48,
-1.));
#38419=DIRECTION('ref_axis',(-4.33680868994202E-19,1.,-1.18789542670764E-48));
#38420=DIRECTION('center_axis',(5.15167520928809E-67,-1.18789542670764E-48,
-1.));
#38421=DIRECTION('ref_axis',(-4.33680868994202E-19,1.,-1.18789542670764E-48));
#38422=DIRECTION('',(-5.15167520928809E-67,1.18789542670764E-48,1.));
#38423=DIRECTION('',(5.15167520928809E-67,-1.18789542670764E-48,-1.));
#38424=DIRECTION('center_axis',(5.15167520928809E-67,-1.18789542670764E-48,
-1.));
#38425=DIRECTION('ref_axis',(-4.33680868994202E-19,1.,-1.18789542670764E-48));
#38426=DIRECTION('center_axis',(5.15167520928809E-67,-1.18789542670764E-48,
-1.));
#38427=DIRECTION('ref_axis',(-4.33680868994202E-19,1.,-1.18789542670764E-48));
#38428=DIRECTION('',(-5.15167520928809E-67,1.18789542670764E-48,1.));
#38429=DIRECTION('',(5.15167520928809E-67,-1.18789542670764E-48,-1.));
#38430=DIRECTION('center_axis',(5.15167520928809E-67,-1.18789542670764E-48,
-1.));
#38431=DIRECTION('ref_axis',(-4.33680868994202E-19,1.,-1.18789542670764E-48));
#38432=DIRECTION('center_axis',(5.15167520928809E-67,-1.18789542670764E-48,
-1.));
#38433=DIRECTION('ref_axis',(-4.33680868994202E-19,1.,-1.18789542670764E-48));
#38434=DIRECTION('',(-5.15167520928809E-67,1.18789542670764E-48,1.));
#38435=DIRECTION('',(5.15167520928809E-67,-1.18789542670764E-48,-1.));
#38436=DIRECTION('center_axis',(5.15167520928809E-67,-1.18789542670764E-48,
-1.));
#38437=DIRECTION('ref_axis',(-4.33680868994202E-19,1.,-1.18789542670764E-48));
#38438=DIRECTION('center_axis',(5.15167520928809E-67,-1.18789542670764E-48,
-1.));
#38439=DIRECTION('ref_axis',(-4.33680868994202E-19,1.,-1.18789542670764E-48));
#38440=DIRECTION('',(-5.15167520928809E-67,1.18789542670764E-48,1.));
#38441=DIRECTION('',(5.15167520928809E-67,-1.18789542670764E-48,-1.));
#38442=DIRECTION('center_axis',(5.15167520928809E-67,-1.18789542670764E-48,
-1.));
#38443=DIRECTION('ref_axis',(-4.33680868994202E-19,1.,-1.18789542670764E-48));
#38444=DIRECTION('center_axis',(5.15167520928809E-67,-1.18789542670764E-48,
-1.));
#38445=DIRECTION('ref_axis',(-4.33680868994202E-19,1.,-1.18789542670764E-48));
#38446=DIRECTION('',(-5.15167520928809E-67,1.18789542670764E-48,1.));
#38447=DIRECTION('',(5.15167520928809E-67,-1.18789542670764E-48,-1.));
#38448=DIRECTION('center_axis',(5.15167520928809E-67,-1.18789542670764E-48,
-1.));
#38449=DIRECTION('ref_axis',(-4.33680868994202E-19,1.,-1.18789542670764E-48));
#38450=DIRECTION('center_axis',(5.15167520928809E-67,-1.18789542670764E-48,
-1.));
#38451=DIRECTION('ref_axis',(-4.33680868994202E-19,1.,-1.18789542670764E-48));
#38452=DIRECTION('',(-5.15167520928809E-67,1.18789542670764E-48,1.));
#38453=DIRECTION('',(5.15167520928809E-67,-1.18789542670764E-48,-1.));
#38454=DIRECTION('center_axis',(5.15167520928809E-67,-1.18789542670764E-48,
-1.));
#38455=DIRECTION('ref_axis',(-4.33680868994202E-19,1.,-1.18789542670764E-48));
#38456=DIRECTION('center_axis',(5.15167520928809E-67,-1.18789542670764E-48,
-1.));
#38457=DIRECTION('ref_axis',(-4.33680868994202E-19,1.,-1.18789542670764E-48));
#38458=DIRECTION('',(-5.15167520928809E-67,1.18789542670764E-48,1.));
#38459=DIRECTION('',(5.15167520928809E-67,-1.18789542670764E-48,-1.));
#38460=DIRECTION('center_axis',(5.15167520928809E-67,-1.18789542670764E-48,
-1.));
#38461=DIRECTION('ref_axis',(-4.33680868994202E-19,1.,-1.18789542670764E-48));
#38462=DIRECTION('center_axis',(5.15167520928809E-67,-1.18789542670764E-48,
-1.));
#38463=DIRECTION('ref_axis',(-4.33680868994202E-19,1.,-1.18789542670764E-48));
#38464=DIRECTION('',(-5.15167520928809E-67,1.18789542670764E-48,1.));
#38465=DIRECTION('',(5.15167520928809E-67,-1.18789542670764E-48,-1.));
#38466=DIRECTION('center_axis',(5.15167520928809E-67,-1.18789542670764E-48,
-1.));
#38467=DIRECTION('ref_axis',(-4.33680868994202E-19,1.,-1.18789542670764E-48));
#38468=DIRECTION('center_axis',(5.15167520928809E-67,-1.18789542670764E-48,
-1.));
#38469=DIRECTION('ref_axis',(-4.33680868994202E-19,1.,-1.18789542670764E-48));
#38470=DIRECTION('',(-5.15167520928809E-67,1.18789542670764E-48,1.));
#38471=DIRECTION('',(5.15167520928809E-67,-1.18789542670764E-48,-1.));
#38472=DIRECTION('center_axis',(5.15167520928809E-67,-1.18789542670764E-48,
-1.));
#38473=DIRECTION('ref_axis',(-4.33680868994202E-19,1.,-1.18789542670764E-48));
#38474=DIRECTION('center_axis',(5.15167520928809E-67,-1.18789542670764E-48,
-1.));
#38475=DIRECTION('ref_axis',(-4.33680868994202E-19,1.,-1.18789542670764E-48));
#38476=DIRECTION('',(-5.15167520928809E-67,1.18789542670764E-48,1.));
#38477=DIRECTION('',(5.15167520928809E-67,-1.18789542670764E-48,-1.));
#38478=DIRECTION('center_axis',(5.15167520928809E-67,-1.18789542670764E-48,
-1.));
#38479=DIRECTION('ref_axis',(-4.33680868994202E-19,1.,-1.18789542670764E-48));
#38480=DIRECTION('center_axis',(5.15167520928809E-67,-1.18789542670764E-48,
-1.));
#38481=DIRECTION('ref_axis',(-4.33680868994202E-19,1.,-1.18789542670764E-48));
#38482=DIRECTION('',(-5.15167520928809E-67,1.18789542670764E-48,1.));
#38483=DIRECTION('',(5.15167520928809E-67,-1.18789542670764E-48,-1.));
#38484=DIRECTION('center_axis',(5.15167520928809E-67,-1.18789542670764E-48,
-1.));
#38485=DIRECTION('ref_axis',(-4.33680868994202E-19,1.,-1.18789542670764E-48));
#38486=DIRECTION('center_axis',(5.15167520928809E-67,-1.18789542670764E-48,
-1.));
#38487=DIRECTION('ref_axis',(-4.33680868994202E-19,1.,-1.18789542670764E-48));
#38488=DIRECTION('',(-5.15167520928809E-67,1.18789542670764E-48,1.));
#38489=DIRECTION('',(5.15167520928809E-67,-1.18789542670764E-48,-1.));
#38490=DIRECTION('center_axis',(5.15167520928809E-67,-1.18789542670764E-48,
-1.));
#38491=DIRECTION('ref_axis',(-4.33680868994202E-19,1.,-1.18789542670764E-48));
#38492=DIRECTION('center_axis',(5.15167520928809E-67,-1.18789542670764E-48,
-1.));
#38493=DIRECTION('ref_axis',(-4.33680868994202E-19,1.,-1.18789542670764E-48));
#38494=DIRECTION('',(-5.15167520928809E-67,1.18789542670764E-48,1.));
#38495=DIRECTION('',(5.15167520928809E-67,-1.18789542670764E-48,-1.));
#38496=DIRECTION('center_axis',(5.15167520928809E-67,-1.18789542670764E-48,
-1.));
#38497=DIRECTION('ref_axis',(-4.33680868994202E-19,1.,-1.18789542670764E-48));
#38498=DIRECTION('center_axis',(5.15167520928809E-67,-1.18789542670764E-48,
-1.));
#38499=DIRECTION('ref_axis',(-4.33680868994202E-19,1.,-1.18789542670764E-48));
#38500=DIRECTION('',(-5.15167520928809E-67,1.18789542670764E-48,1.));
#38501=DIRECTION('',(5.15167520928809E-67,-1.18789542670764E-48,-1.));
#38502=DIRECTION('center_axis',(5.15167520928809E-67,-1.18789542670764E-48,
-1.));
#38503=DIRECTION('ref_axis',(-4.33680868994202E-19,1.,-1.18789542670764E-48));
#38504=DIRECTION('center_axis',(5.15167520928809E-67,-1.18789542670764E-48,
-1.));
#38505=DIRECTION('ref_axis',(-4.33680868994202E-19,1.,-1.18789542670764E-48));
#38506=DIRECTION('',(-5.15167520928809E-67,1.18789542670764E-48,1.));
#38507=DIRECTION('',(5.15167520928809E-67,-1.18789542670764E-48,-1.));
#38508=DIRECTION('center_axis',(5.15167520928809E-67,-1.18789542670764E-48,
-1.));
#38509=DIRECTION('ref_axis',(-4.33680868994202E-19,1.,-1.18789542670764E-48));
#38510=DIRECTION('center_axis',(5.15167520928809E-67,-1.18789542670764E-48,
-1.));
#38511=DIRECTION('ref_axis',(-4.33680868994202E-19,1.,-1.18789542670764E-48));
#38512=DIRECTION('',(-5.15167520928809E-67,1.18789542670764E-48,1.));
#38513=DIRECTION('',(5.15167520928809E-67,-1.18789542670764E-48,-1.));
#38514=DIRECTION('center_axis',(5.15167520928809E-67,-1.18789542670764E-48,
-1.));
#38515=DIRECTION('ref_axis',(-4.33680868994202E-19,1.,-1.18789542670764E-48));
#38516=DIRECTION('center_axis',(5.15167520928809E-67,-1.18789542670764E-48,
-1.));
#38517=DIRECTION('ref_axis',(-4.33680868994202E-19,1.,-1.18789542670764E-48));
#38518=DIRECTION('',(5.15167520928809E-67,-1.18789542670764E-48,-1.));
#38519=DIRECTION('center_axis',(5.15167520928809E-67,-1.18789542670764E-48,
-1.));
#38520=DIRECTION('ref_axis',(-4.33680868994202E-19,1.,-1.18789542670764E-48));
#38521=DIRECTION('',(-5.15167520928809E-67,1.18789542670764E-48,1.));
#38522=DIRECTION('center_axis',(5.15167520928809E-67,-1.18789542670764E-48,
-1.));
#38523=DIRECTION('ref_axis',(-4.33680868994202E-19,1.,-1.18789542670764E-48));
#38524=DIRECTION('',(5.15167520928809E-67,-1.18789542670764E-48,-1.));
#38525=DIRECTION('center_axis',(5.15167520928809E-67,-1.18789542670764E-48,
-1.));
#38526=DIRECTION('ref_axis',(-4.33680868994202E-19,1.,-1.18789542670764E-48));
#38527=DIRECTION('',(-5.15167520928809E-67,1.18789542670764E-48,1.));
#38528=DIRECTION('center_axis',(5.15167520928809E-67,-1.18789542670764E-48,
-1.));
#38529=DIRECTION('ref_axis',(-4.33680868994202E-19,1.,-1.18789542670764E-48));
#38530=DIRECTION('',(5.15167520928809E-67,-1.18789542670764E-48,-1.));
#38531=DIRECTION('center_axis',(5.15167520928809E-67,-1.18789542670764E-48,
-1.));
#38532=DIRECTION('ref_axis',(-4.33680868994202E-19,1.,-1.18789542670764E-48));
#38533=DIRECTION('',(-5.15167520928809E-67,1.18789542670764E-48,1.));
#38534=DIRECTION('center_axis',(5.15167520928809E-67,-1.18789542670764E-48,
-1.));
#38535=DIRECTION('ref_axis',(-4.33680868994202E-19,1.,-1.18789542670764E-48));
#38536=DIRECTION('',(5.15167520928809E-67,-1.18789542670764E-48,-1.));
#38537=DIRECTION('center_axis',(5.15167520928809E-67,-1.18789542670764E-48,
-1.));
#38538=DIRECTION('ref_axis',(-4.33680868994202E-19,1.,-1.18789542670764E-48));
#38539=DIRECTION('',(-5.15167520928809E-67,1.18789542670764E-48,1.));
#38540=DIRECTION('center_axis',(5.15167520928809E-67,-1.18789542670764E-48,
-1.));
#38541=DIRECTION('ref_axis',(-4.33680868994202E-19,1.,-1.18789542670764E-48));
#38542=DIRECTION('',(5.15167520928809E-67,-1.18789542670764E-48,-1.));
#38543=DIRECTION('center_axis',(5.15167520928809E-67,-1.18789542670764E-48,
-1.));
#38544=DIRECTION('ref_axis',(-4.33680868994202E-19,1.,-1.18789542670764E-48));
#38545=DIRECTION('',(-5.15167520928809E-67,1.18789542670764E-48,1.));
#38546=DIRECTION('center_axis',(5.15167520928809E-67,-1.18789542670764E-48,
-1.));
#38547=DIRECTION('ref_axis',(-4.33680868994202E-19,1.,-1.18789542670764E-48));
#38548=DIRECTION('',(5.15167520928809E-67,-1.18789542670764E-48,-1.));
#38549=DIRECTION('center_axis',(5.15167520928809E-67,-1.18789542670764E-48,
-1.));
#38550=DIRECTION('ref_axis',(-4.33680868994202E-19,1.,-1.18789542670764E-48));
#38551=DIRECTION('',(-5.15167520928809E-67,1.18789542670764E-48,1.));
#38552=DIRECTION('center_axis',(5.15167520928809E-67,-1.18789542670764E-48,
-1.));
#38553=DIRECTION('ref_axis',(-4.33680868994202E-19,1.,-1.18789542670764E-48));
#38554=DIRECTION('',(5.15167520928809E-67,-1.18789542670764E-48,-1.));
#38555=DIRECTION('center_axis',(5.15167520928809E-67,-1.18789542670764E-48,
-1.));
#38556=DIRECTION('ref_axis',(-4.33680868994202E-19,1.,-1.18789542670764E-48));
#38557=DIRECTION('',(-5.15167520928809E-67,1.18789542670764E-48,1.));
#38558=DIRECTION('center_axis',(5.15167520928809E-67,-1.18789542670764E-48,
-1.));
#38559=DIRECTION('ref_axis',(-4.33680868994202E-19,1.,-1.18789542670764E-48));
#38560=DIRECTION('',(5.15167520928809E-67,-1.18789542670764E-48,-1.));
#38561=DIRECTION('center_axis',(5.15167520928809E-67,-1.18789542670764E-48,
-1.));
#38562=DIRECTION('ref_axis',(-4.33680868994202E-19,1.,-1.18789542670764E-48));
#38563=DIRECTION('',(-5.15167520928809E-67,1.18789542670764E-48,1.));
#38564=DIRECTION('center_axis',(5.15167520928809E-67,-1.18789542670764E-48,
-1.));
#38565=DIRECTION('ref_axis',(-4.33680868994202E-19,1.,-1.18789542670764E-48));
#38566=DIRECTION('',(5.15167520928809E-67,-1.18789542670764E-48,-1.));
#38567=DIRECTION('center_axis',(5.15167520928809E-67,-1.18789542670764E-48,
-1.));
#38568=DIRECTION('ref_axis',(-4.33680868994202E-19,1.,-1.18789542670764E-48));
#38569=DIRECTION('',(-5.15167520928809E-67,1.18789542670764E-48,1.));
#38570=DIRECTION('center_axis',(5.15167520928809E-67,-1.18789542670764E-48,
-1.));
#38571=DIRECTION('ref_axis',(-4.33680868994202E-19,1.,-1.18789542670764E-48));
#38572=DIRECTION('',(5.15167520928809E-67,-1.18789542670764E-48,-1.));
#38573=DIRECTION('center_axis',(5.15167520928809E-67,-1.18789542670764E-48,
-1.));
#38574=DIRECTION('ref_axis',(-4.33680868994202E-19,1.,-1.18789542670764E-48));
#38575=DIRECTION('',(-5.15167520928809E-67,1.18789542670764E-48,1.));
#38576=DIRECTION('center_axis',(5.15167520928809E-67,-1.18789542670764E-48,
-1.));
#38577=DIRECTION('ref_axis',(-4.33680868994202E-19,1.,-1.18789542670764E-48));
#38578=DIRECTION('',(5.15167520928809E-67,-1.18789542670764E-48,-1.));
#38579=DIRECTION('center_axis',(5.15167520928809E-67,-1.18789542670764E-48,
-1.));
#38580=DIRECTION('ref_axis',(-4.33680868994202E-19,1.,-1.18789542670764E-48));
#38581=DIRECTION('',(-5.15167520928809E-67,1.18789542670764E-48,1.));
#38582=DIRECTION('center_axis',(5.15167520928809E-67,-1.18789542670764E-48,
-1.));
#38583=DIRECTION('ref_axis',(-4.33680868994202E-19,1.,-1.18789542670764E-48));
#38584=DIRECTION('',(5.15167520928809E-67,-1.18789542670764E-48,-1.));
#38585=DIRECTION('center_axis',(5.15167520928809E-67,-1.18789542670764E-48,
-1.));
#38586=DIRECTION('ref_axis',(-4.33680868994202E-19,1.,-1.18789542670764E-48));
#38587=DIRECTION('',(-5.15167520928809E-67,1.18789542670764E-48,1.));
#38588=DIRECTION('center_axis',(5.15167520928809E-67,-1.18789542670764E-48,
-1.));
#38589=DIRECTION('ref_axis',(-4.33680868994202E-19,1.,-1.18789542670764E-48));
#38590=DIRECTION('',(5.15167520928809E-67,-1.18789542670764E-48,-1.));
#38591=DIRECTION('center_axis',(5.15167520928809E-67,-1.18789542670764E-48,
-1.));
#38592=DIRECTION('ref_axis',(-4.33680868994202E-19,1.,-1.18789542670764E-48));
#38593=DIRECTION('',(-5.15167520928809E-67,1.18789542670764E-48,1.));
#38594=DIRECTION('center_axis',(5.15167520928809E-67,-1.18789542670764E-48,
-1.));
#38595=DIRECTION('ref_axis',(-4.33680868994202E-19,1.,-1.18789542670764E-48));
#38596=DIRECTION('',(5.15167520928809E-67,-1.18789542670764E-48,-1.));
#38597=DIRECTION('center_axis',(5.15167520928809E-67,-1.18789542670764E-48,
-1.));
#38598=DIRECTION('ref_axis',(-4.33680868994202E-19,1.,-1.18789542670764E-48));
#38599=DIRECTION('',(-5.15167520928809E-67,1.18789542670764E-48,1.));
#38600=DIRECTION('center_axis',(5.15167520928809E-67,-1.18789542670764E-48,
-1.));
#38601=DIRECTION('ref_axis',(-4.33680868994202E-19,1.,-1.18789542670764E-48));
#38602=DIRECTION('',(-5.15167520928809E-67,1.18789542670764E-48,1.));
#38603=DIRECTION('',(5.15167520928809E-67,-1.18789542670764E-48,-1.));
#38604=DIRECTION('center_axis',(5.15167520928809E-67,-1.18789542670764E-48,
-1.));
#38605=DIRECTION('ref_axis',(-4.33680868994202E-19,1.,-1.18789542670764E-48));
#38606=DIRECTION('center_axis',(5.15167520928809E-67,-1.18789542670764E-48,
-1.));
#38607=DIRECTION('ref_axis',(0.,1.,0.));
#38608=DIRECTION('center_axis',(-0.726718511656259,-0.686935363550879,-0.000105448246390915));
#38609=DIRECTION('ref_axis',(0.686885008270217,-0.726663364190208,-0.0122204974282148));
#38610=DIRECTION('center_axis',(0.0503511057571476,0.998731574514185,-9.06501463958382E-5));
#38611=DIRECTION('ref_axis',(0.998626750226923,-0.0503471356586858,-0.0144837723739379));
#38612=DIRECTION('center_axis',(5.15167520928809E-67,-1.18789542670764E-48,
-1.));
#38613=DIRECTION('ref_axis',(0.,1.,0.));
#38614=DIRECTION('center_axis',(-0.0281636861094737,0.999603320606368,-9.06501463234301E-5));
#38615=DIRECTION('ref_axis',(0.999498507968587,0.0281594195507115,-0.0144837722688343));
#38616=DIRECTION('center_axis',(-0.670581953565459,-0.741835448352935,-0.000105448247414229));
#38617=DIRECTION('ref_axis',(0.741780921484837,-0.670530926934418,-0.0122204969447688));
#38618=DIRECTION('center_axis',(5.15167520928809E-67,-1.18789542670764E-48,
-1.));
#38619=DIRECTION('ref_axis',(0.,1.,0.));
#38620=DIRECTION('center_axis',(-0.106504839485416,0.994312179825198,-9.06501464431132E-5));
#38621=DIRECTION('ref_axis',(0.994208025038947,0.106492362574112,-0.014483772351861));
#38622=DIRECTION('center_axis',(-0.610311034741592,-0.792161870928735,-0.000105448247339917));
#38623=DIRECTION('ref_axis',(0.792103508645573,-0.610264443537491,-0.0122204969313235));
#38624=DIRECTION('center_axis',(5.15167520928809E-67,-1.18789542670764E-48,
-1.));
#38625=DIRECTION('ref_axis',(0.,1.,0.));
#38626=DIRECTION('center_axis',(-0.184189355109993,0.982890773812999,-9.06501463311491E-5));
#38627=DIRECTION('ref_axis',(0.982787919029266,0.184168744770673,-0.0144837722890199));
#38628=DIRECTION('center_axis',(-0.546277345439217,-0.837604352149957,-0.000105448247410497));
#38629=DIRECTION('ref_axis',(0.837542514274823,-0.546235476912428,-0.0122204968991007));
#38630=DIRECTION('center_axis',(5.15167520928809E-67,-1.18789542670764E-48,
-1.));
#38631=DIRECTION('ref_axis',(0.,1.,0.));
#38632=DIRECTION('center_axis',(-0.260738282110594,0.965409519336,-9.0650146457266E-5));
#38633=DIRECTION('ref_axis',(0.965308598686112,0.260709665412272,-0.0144837724117514));
#38634=DIRECTION('center_axis',(-0.478875674647023,-0.877882724008182,-0.000105448247224529));
#38635=DIRECTION('ref_axis',(0.877817791791478,-0.478838786930502,-0.0122204969317693));
#38636=DIRECTION('center_axis',(5.15167520928809E-67,-1.18789542670764E-48,
-1.));
#38637=DIRECTION('ref_axis',(0.,1.,0.));
#38638=DIRECTION('center_axis',(-0.335679670898074,0.941976194140973,-9.06501464082373E-5));
#38639=DIRECTION('ref_axis',(0.941877829837014,0.335643224272907,-0.014483772340284));
#38640=DIRECTION('center_axis',(-0.40852157607848,-0.912748656947257,-0.000105448246964389));
#38641=DIRECTION('ref_axis',(0.912681030716442,-0.408489896596762,-0.0122204970741974));
#38642=DIRECTION('center_axis',(5.15167520928809E-67,-1.18789542670764E-48,
-1.));
#38643=DIRECTION('ref_axis',(0.,1.,0.));
#38644=DIRECTION('center_axis',(-0.408551482889657,0.91273527247018,-9.06501463992171E-5));
#38645=DIRECTION('ref_axis',(0.91264007096006,0.408507431043052,-0.014483772320157));
#38646=DIRECTION('center_axis',(-0.335648806144879,-0.941987190897087,-0.000105448247367288));
#38647=DIRECTION('ref_axis',(0.941917287594001,-0.335622530214118,-0.0122204968897907));
#38648=DIRECTION('center_axis',(5.15167520928809E-67,-1.18789542670764E-48,
-1.));
#38649=DIRECTION('ref_axis',(0.,1.,0.));
#38650=DIRECTION('center_axis',(-0.478904439132113,0.877867034329292,-9.06501463430316E-5));
#38651=DIRECTION('ref_axis',(0.877775582560928,0.478853053657823,-0.0144837723815965));
#38652=DIRECTION('center_axis',(-0.260706649707894,-0.965418060572078,-0.000105448247265905));
#38653=DIRECTION('ref_axis',(0.965346311170054,-0.260685939326527,-0.0122204970363453));
#38654=DIRECTION('center_axis',(5.15167520928809E-67,-1.18789542670764E-48,
-1.));
#38655=DIRECTION('ref_axis',(0.,1.,0.));
#38656=DIRECTION('center_axis',(-0.546304790255147,0.837586454001514,-9.06501464163507E-5));
#38657=DIRECTION('ref_axis',(0.837499315806636,0.546246387962313,-0.0144837723519214));
#38658=DIRECTION('center_axis',(-0.184157150081311,-0.982896806869672,-0.00010544824733539));
#38659=DIRECTION('ref_axis',(0.982823653730718,-0.184142132936614,-0.012220496919376));
#38660=DIRECTION('center_axis',(5.15167520928809E-67,-1.18789542670764E-48,
-1.));
#38661=DIRECTION('ref_axis',(0.,1.,0.));
#38662=DIRECTION('center_axis',(-0.610336990681852,0.792141874658809,-9.06501463120476E-5));
#38663=DIRECTION('ref_axis',(0.792059587273495,0.610271931640219,-0.0144837723075503));
#38664=DIRECTION('center_axis',(-0.106472260385922,-0.994315667506542,-0.000105448247451369));
#38665=DIRECTION('ref_axis',(0.994241561642557,-0.106463029063183,-0.0122204969318448));
#38666=DIRECTION('center_axis',(5.15167520928809E-67,-1.18789542670764E-48,
-1.));
#38667=DIRECTION('ref_axis',(0.,1.,0.));
#38668=DIRECTION('center_axis',(-0.670606260603123,0.741813477245087,-9.06501463072396E-5));
#38669=DIRECTION('ref_axis',(0.741736547997548,0.670534945922644,-0.0144837723400245));
#38670=DIRECTION('center_axis',(-0.0281309338001256,-0.999604241409669,
-0.000105448247349234));
#38671=DIRECTION('ref_axis',(0.999529639708615,-0.0281275452135709,-0.012220496889411));
#38672=DIRECTION('center_axis',(5.15167520928809E-67,-1.18789542670764E-48,
-1.));
#38673=DIRECTION('ref_axis',(0.,1.,0.));
#38674=DIRECTION('center_axis',(-0.726741019928497,0.686911553066215,-9.0650146372247E-5));
#38675=DIRECTION('ref_axis',(0.686840456250864,0.726663889287803,-0.014483772375632));
#38676=DIRECTION('center_axis',(0.0503838293471008,-0.9987299227624,-0.000105448247268434));
#38677=DIRECTION('ref_axis',(0.998655285167451,0.0503813543057433,-0.0122204969390446));
#38678=DIRECTION('center_axis',(5.15167520928809E-67,-1.18789542670764E-48,
-1.));
#38679=DIRECTION('ref_axis',(0.,1.,0.));
#38680=DIRECTION('center_axis',(-0.77839517919999,0.627774590741587,-9.06501465192481E-5));
#38681=DIRECTION('ref_axis',(0.62770976469511,0.778312708136478,-0.0144837722873138));
#38682=DIRECTION('center_axis',(0.128587959432554,-0.991698102029866,-0.000105448247403937));
#38683=DIRECTION('ref_axis',(0.991623888707038,0.128579636022696,-0.0122204969540051));
#38684=DIRECTION('center_axis',(5.15167520928809E-67,-1.18789542670764E-48,
-1.));
#38685=DIRECTION('ref_axis',(0.,1.,0.));
#38686=DIRECTION('center_axis',(-0.825250273349494,0.564767189308247,-9.06501463546308E-5));
#38687=DIRECTION('ref_axis',(0.564709033703414,0.82516297032304,-0.0144837723475052));
#38688=DIRECTION('center_axis',(0.205999301987418,-0.978552132725367,-0.000105448247113811));
#38689=DIRECTION('ref_axis',(0.978478801224233,0.205985181525565,-0.0122204969893998));
#38690=DIRECTION('center_axis',(5.15167520928809E-67,-1.18789542670764E-48,
-1.));
#38691=DIRECTION('ref_axis',(0.,1.,0.));
#38692=DIRECTION('center_axis',(-0.867017425140065,0.498277810348848,-9.06501462870057E-5));
#38693=DIRECTION('ref_axis',(0.498226683734515,0.866925828402957,-0.0144837723937473));
#38694=DIRECTION('center_axis',(0.282140590344591,-0.959373064120873,-0.000105448247263863));
#38695=DIRECTION('ref_axis',(0.959301066555575,0.282120759888322,-0.0122204969363817));
#38696=DIRECTION('center_axis',(5.15167520928809E-67,-1.18789542670764E-48,
-1.));
#38697=DIRECTION('ref_axis',(0.,1.,0.));
#38698=DIRECTION('center_axis',(-0.903439126191882,0.428716382994866,-9.06501464245823E-5));
#38699=DIRECTION('ref_axis',(0.42867260058449,0.903343800470088,-0.0144837723120868));
#38700=DIRECTION('center_axis',(0.356542388140961,-0.934279141552142,-0.000105448247299974));
#38701=DIRECTION('ref_axis',(0.934208921811354,0.356516969951643,-0.0122204969034503));
#38702=DIRECTION('center_axis',(5.15167520928809E-67,-1.18789542670764E-48,
-1.));
#38703=DIRECTION('ref_axis',(0.,1.,0.));
#38704=DIRECTION('center_axis',(-0.934290824606917,0.356511776576704,-9.06501463905499E-5));
#38705=DIRECTION('ref_axis',(0.356475608302988,0.934192357614636,-0.0144837722787681));
#38706=DIRECTION('center_axis',(0.428745983551553,-0.903425077396614,-0.000105448247174382));
#38707=DIRECTION('ref_axis',(0.903357068407879,0.428715134340607,-0.0122204969145006));
#38708=DIRECTION('center_axis',(5.15167520928809E-67,-1.18789542670764E-48,
-1.));
#38709=DIRECTION('ref_axis',(0.,1.,0.));
#38710=DIRECTION('center_axis',(-0.959382309405018,0.282109156503729,-9.06501463332588E-5));
#38711=DIRECTION('ref_axis',(0.282080825355611,0.959281308222547,-0.0144837723517365));
#38712=DIRECTION('center_axis',(0.498306217395032,-0.867001097223137,-0.000105448243846677));
#38713=DIRECTION('ref_axis',(0.866935718268405,0.498270127348975,-0.0122204984383232));
#38714=DIRECTION('center_axis',(5.15167520928809E-67,-1.18789542670764E-48,
-1.));
#38715=DIRECTION('ref_axis',(0.,1.,0.));
#38716=DIRECTION('center_axis',(-0.978558883238511,0.205967239670656,-9.06501465473592E-5));
#38717=DIRECTION('ref_axis',(0.205946920319669,0.978455970573743,-0.0144837722792749));
#38718=DIRECTION('center_axis',(0.564794227716619,-0.825231766971349,-0.000105448246777006));
#38719=DIRECTION('ref_axis',(0.825169421163283,0.564753119359096,-0.01222049717581));
#38720=DIRECTION('center_axis',(5.15167520928809E-67,-1.18789542670764E-48,
-1.));
#38721=DIRECTION('ref_axis',(0.,1.,0.));
#38722=DIRECTION('center_axis',(-0.991702316153162,0.128555466313202,-9.0650146420716E-5));
#38723=DIRECTION('ref_axis',(0.128543284034494,0.991598126494967,-0.0144837723435229));
#38724=DIRECTION('center_axis',(0.627800093806525,-0.778374608461238,-0.000105448247294656));
#38725=DIRECTION('ref_axis',(0.778315680171741,0.627754220578766,-0.012220496894383));
#38726=DIRECTION('center_axis',(5.15167520928809E-67,-1.18789542670764E-48,
-1.));
#38727=DIRECTION('ref_axis',(0.,1.,0.));
#38728=DIRECTION('center_axis',(-0.998731574514195,0.0503511057569474,-9.06501463044587E-5));
#38729=DIRECTION('ref_axis',(0.0503471356585215,0.998626750227776,-0.0144837723156803));
#38730=DIRECTION('center_axis',(0.686935363552588,-0.726718511654644,-0.000105448247440854));
#38731=DIRECTION('ref_axis',(0.726663364192637,0.6868850082757,-0.0122204969756106));
#38732=DIRECTION('center_axis',(5.15167520928809E-67,-1.18789542670764E-48,
-1.));
#38733=DIRECTION('ref_axis',(0.,1.,0.));
#38734=DIRECTION('center_axis',(-0.99960332060638,-0.0281636861090561,-9.06501465204533E-5));
#38735=DIRECTION('ref_axis',(0.0281594195503036,-0.999498507968962,0.0144837722437162));
#38736=DIRECTION('center_axis',(0.741835448352776,-0.670581953565635,-0.000105448247295083));
#38737=DIRECTION('ref_axis',(0.67053092693442,0.741780921484487,-0.0122204969658991));
#38738=DIRECTION('center_axis',(5.15167520928809E-67,-1.18789542670764E-48,
-1.));
#38739=DIRECTION('ref_axis',(0.,1.,0.));
#38740=DIRECTION('center_axis',(-0.994312179825187,-0.106504839485521,-9.0650146389517E-5));
#38741=DIRECTION('ref_axis',(0.106492362574174,-0.994208025038546,0.0144837723789195));
#38742=DIRECTION('center_axis',(0.792161870927703,-0.610311034742932,-0.000105448246562834));
#38743=DIRECTION('ref_axis',(0.610264443536631,0.792103508641721,-0.0122204972240042));
#38744=DIRECTION('center_axis',(5.15167520928809E-67,-1.18789542670764E-48,
-1.));
#38745=DIRECTION('ref_axis',(0.,1.,0.));
#38746=DIRECTION('center_axis',(-0.982890773812962,-0.18418935511019,-9.06501462458389E-5));
#38747=DIRECTION('ref_axis',(0.184168744770736,-0.982787919028534,0.0144837723378535));
#38748=DIRECTION('center_axis',(0.837604352149828,-0.546277345439416,-0.000105448247288724));
#38749=DIRECTION('ref_axis',(0.546235476912052,0.837542514273825,-0.0122204969843265));
#38750=DIRECTION('center_axis',(5.15167520928809E-67,-1.18789542670764E-48,
-1.));
#38751=DIRECTION('ref_axis',(0.,1.,0.));
#38752=DIRECTION('center_axis',(-0.965409519335916,-0.260738282110905,-9.06501463158079E-5));
#38753=DIRECTION('ref_axis',(0.260709665413015,-0.965308598687581,0.0144837723005081));
#38754=DIRECTION('center_axis',(0.877882724007609,-0.478875674648073,-0.000105448246644854));
#38755=DIRECTION('ref_axis',(0.47883878693024,0.877817791788535,-0.012220497153411));
#38756=DIRECTION('center_axis',(5.15167520928809E-67,-1.18789542670764E-48,
-1.));
#38757=DIRECTION('ref_axis',(0.,1.,0.));
#38758=DIRECTION('center_axis',(-0.941976194141077,-0.335679670897783,-9.06501465752214E-5));
#38759=DIRECTION('ref_axis',(0.335643224272825,-0.941877829837701,0.0144837722974511));
#38760=DIRECTION('center_axis',(0.912748656947635,-0.408521576077636,-0.000105448247395522));
#38761=DIRECTION('ref_axis',(0.408489896596716,0.912681030718573,-0.0122204969165703));
#38762=DIRECTION('center_axis',(5.15167520928809E-67,-1.18789542670764E-48,
-1.));
#38763=DIRECTION('ref_axis',(0.,1.,0.));
#38764=DIRECTION('center_axis',(-0.912735272470059,-0.408551482889927,-9.0650146236208E-5));
#38765=DIRECTION('ref_axis',(0.408507431042893,-0.912640070958992,0.0144837723919199));
#38766=DIRECTION('center_axis',(0.941987190897161,-0.335648806144671,-0.000105448247475279));
#38767=DIRECTION('ref_axis',(0.335622530214028,0.941917287594399,-0.0122204968616106));
#38768=DIRECTION('center_axis',(5.15167520928809E-67,-1.18789542670764E-48,
-1.));
#38769=DIRECTION('ref_axis',(0.,1.,0.));
#38770=DIRECTION('center_axis',(-0.877867034329361,-0.478904439131988,-9.06501463610722E-5));
#38771=DIRECTION('ref_axis',(0.478853053657853,-0.877775582561276,0.0144837723595397));
#38772=DIRECTION('center_axis',(0.965418060572122,-0.260706649707733,-0.000105448247352975));
#38773=DIRECTION('ref_axis',(0.260685939326823,0.965346311171741,-0.012220496896787));
#38774=DIRECTION('center_axis',(5.15167520928809E-67,-1.18789542670764E-48,
-1.));
#38775=DIRECTION('ref_axis',(0.,1.,0.));
#38776=DIRECTION('center_axis',(-0.837586454001461,-0.546304790255229,-9.06501463408637E-5));
#38777=DIRECTION('ref_axis',(0.54624638796239,-0.837499315806573,0.0144837723526967));
#38778=DIRECTION('center_axis',(0.982896806869685,-0.184157150081241,-0.000105448247384682));
#38779=DIRECTION('ref_axis',(0.184142132936524,0.982823653730634,-0.0122204969274716));
#38780=DIRECTION('center_axis',(5.15167520928809E-67,-1.18789542670764E-48,
-1.));
#38781=DIRECTION('ref_axis',(0.,1.,0.));
#38782=DIRECTION('center_axis',(-0.792141874658961,-0.610336990681655,-9.06501464140886E-5));
#38783=DIRECTION('ref_axis',(0.610271931639049,-0.792059587272402,0.0144837724166105));
#38784=DIRECTION('center_axis',(0.994315667506523,-0.1064722603861,-0.000105448247372999));
#38785=DIRECTION('ref_axis',(0.106463029063429,0.994241561643113,-0.0122204968844733));
#38786=DIRECTION('center_axis',(5.15167520928809E-67,-1.18789542670764E-48,
-1.));
#38787=DIRECTION('ref_axis',(0.,1.,0.));
#38788=DIRECTION('center_axis',(-0.741813477245026,-0.670606260603191,-9.06501462657205E-5));
#38789=DIRECTION('ref_axis',(0.670534945922615,-0.741736547997381,0.0144837723499451));
#38790=DIRECTION('center_axis',(0.999604241409683,-0.0281309337996267,-0.000105448247542078));
#38791=DIRECTION('ref_axis',(0.0281275452130772,0.999529639708833,-0.0122204968727785));
#38792=DIRECTION('center_axis',(5.15167520928809E-67,-1.18789542670764E-48,
-1.));
#38793=DIRECTION('ref_axis',(0.,1.,0.));
#38794=DIRECTION('center_axis',(-0.686911553066313,-0.726741019928404,-9.0650146445407E-5));
#38795=DIRECTION('ref_axis',(0.726663889287897,-0.686840456251137,0.0144837723579623));
#38796=DIRECTION('center_axis',(0.998729922762429,0.0503838293465177,-0.00010544824700806));
#38797=DIRECTION('ref_axis',(0.0503813543051317,-0.998655285166875,0.0122204969886123));
#38798=DIRECTION('center_axis',(5.15167520928809E-67,-1.18789542670764E-48,
-1.));
#38799=DIRECTION('ref_axis',(0.,1.,0.));
#38800=DIRECTION('center_axis',(-0.627774590741284,-0.778395179200234,-9.06501463091932E-5));
#38801=DIRECTION('ref_axis',(0.778312708136324,-0.627709764694486,0.014483772322638));
#38802=DIRECTION('center_axis',(0.991698102029894,0.128587959432343,-0.000105448247307732));
#38803=DIRECTION('ref_axis',(0.128579636022594,-0.991623888707978,0.0122204968787672));
#38804=DIRECTION('center_axis',(5.15167520928809E-67,-1.18789542670764E-48,
-1.));
#38805=DIRECTION('ref_axis',(0.,1.,0.));
#38806=DIRECTION('center_axis',(-0.564767189308512,-0.825250273349312,-9.06501464604225E-5));
#38807=DIRECTION('ref_axis',(0.825162970323365,-0.564709033704023,0.014483772305219));
#38808=DIRECTION('center_axis',(0.978552132725239,0.205999301988023,-0.000105448247439453));
#38809=DIRECTION('ref_axis',(0.205985181526365,-0.978478801225051,0.0122204969104439));
#38810=DIRECTION('center_axis',(5.15167520928809E-67,-1.18789542670764E-48,
-1.));
#38811=DIRECTION('ref_axis',(0.,1.,0.));
#38812=DIRECTION('center_axis',(-0.498277810349565,-0.867017425139653,-9.06501466563663E-5));
#38813=DIRECTION('ref_axis',(0.86692582840462,-0.498226683736414,0.0144837722289047));
#38814=DIRECTION('center_axis',(0.959373064120893,0.282140590344525,-0.00010544824722367));
#38815=DIRECTION('ref_axis',(0.282120759888269,-0.959301066555644,0.0122204969322086));
#38816=DIRECTION('center_axis',(5.15167520928809E-67,-1.18789542670764E-48,
-1.));
#38817=DIRECTION('ref_axis',(0.,1.,0.));
#38818=DIRECTION('center_axis',(-0.428716382994794,-0.903439126191916,-9.06501464376821E-5));
#38819=DIRECTION('ref_axis',(0.903343800470677,-0.428672600584677,0.0144837722698243));
#38820=DIRECTION('center_axis',(0.934279141552165,0.356542388140901,-0.000105448247303552));
#38821=DIRECTION('ref_axis',(0.356516969951467,-0.934208921811066,0.0122204969306124));
#38822=DIRECTION('center_axis',(5.15167520928809E-67,-1.18789542670764E-48,
-1.));
#38823=DIRECTION('ref_axis',(0.,1.,0.));
#38824=DIRECTION('center_axis',(-0.356511776576584,-0.934290824606963,-9.06501462973138E-5));
#38825=DIRECTION('ref_axis',(0.9341923576135,-0.356475608302424,0.0144837723659048));
#38826=DIRECTION('center_axis',(0.903425077396469,0.42874598355186,-0.000105448247323971));
#38827=DIRECTION('ref_axis',(0.428715134340782,-0.903357068407445,0.0122204969404582));
#38828=DIRECTION('center_axis',(5.15167520928809E-67,-1.18789542670764E-48,
-1.));
#38829=DIRECTION('ref_axis',(0.,1.,0.));
#38830=DIRECTION('center_axis',(-0.282109156503611,-0.959382309405053,-9.06501462853803E-5));
#38831=DIRECTION('ref_axis',(0.959281308222382,-0.282080825355435,0.0144837723660616));
#38832=DIRECTION('center_axis',(0.867001097223284,0.498306217394775,-0.000105448243705777));
#38833=DIRECTION('ref_axis',(0.498270127348596,-0.86693571826834,0.0122204984583659));
#38834=DIRECTION('center_axis',(5.15167520928809E-67,-1.18789542670764E-48,
-1.));
#38835=DIRECTION('ref_axis',(0.,1.,0.));
#38836=DIRECTION('center_axis',(-0.205967239670074,-0.978558883238633,-9.06501462899978E-5));
#38837=DIRECTION('ref_axis',(0.978455970573443,-0.205946920318997,0.0144837723091262));
#38838=DIRECTION('center_axis',(0.825231766971361,0.564794227716602,-0.000105448246768021));
#38839=DIRECTION('ref_axis',(0.56475311935916,-0.825169421163415,0.0122204971638891));
#38840=DIRECTION('center_axis',(5.15167520928809E-67,-1.18789542670764E-48,
-1.));
#38841=DIRECTION('ref_axis',(0.,1.,0.));
#38842=DIRECTION('center_axis',(-0.128555466313085,-0.991702316153177,-9.06501463759606E-5));
#38843=DIRECTION('ref_axis',(0.991598126495219,-0.128543284034406,0.014483772327091));
#38844=DIRECTION('center_axis',(0.778374608461285,0.627800093806467,-0.000105448247278628));
#38845=DIRECTION('ref_axis',(0.627754220578617,-0.778315680171672,0.0122204969064386));
#38846=DIRECTION('center_axis',(5.15167520928809E-67,-1.18789542670764E-48,
-1.));
#38847=DIRECTION('ref_axis',(0.,1.,0.));
#38848=DIRECTION('center_axis',(-0.0503511057568215,-0.998731574514202,
-9.06501462140748E-5));
#38849=DIRECTION('ref_axis',(0.998626750226433,-0.0503471356583347,0.0144837724089729));
#38850=DIRECTION('center_axis',(0.72671851165485,0.686935363552371,-0.000105448247305609));
#38851=DIRECTION('ref_axis',(0.68688500827568,-0.726663364193057,0.0122204969517677));
#38852=DIRECTION('center_axis',(5.15167520928809E-67,-1.18789542670764E-48,
-1.));
#38853=DIRECTION('ref_axis',(0.,1.,0.));
#38854=DIRECTION('center_axis',(0.028163686109212,-0.999603320606376,-9.06501464412085E-5));
#38855=DIRECTION('ref_axis',(0.999498507967367,0.0281594195504058,0.0144837723535955));
#38856=DIRECTION('center_axis',(0.670581953565646,0.741835448352765,-0.000105448247317749));
#38857=DIRECTION('ref_axis',(0.741780921484837,-0.670530926934763,0.0122204969257884));
#38858=DIRECTION('center_axis',(5.15167520928809E-67,-1.18789542670764E-48,
-1.));
#38859=DIRECTION('ref_axis',(0.,1.,0.));
#38860=DIRECTION('center_axis',(0.106504839485654,-0.994312179825173,-9.06501463242885E-5));
#38861=DIRECTION('ref_axis',(0.994208025039066,0.106492362574368,0.0144837723417732));
#38862=DIRECTION('center_axis',(0.610311034742769,0.792161870927829,-0.000105448246632335));
#38863=DIRECTION('ref_axis',(0.792103508641049,-0.610264443535841,0.012220497306985));
#38864=DIRECTION('center_axis',(5.15167520928809E-67,-1.18789542670764E-48,
-1.));
#38865=DIRECTION('ref_axis',(0.,1.,0.));
#38866=DIRECTION('center_axis',(0.184189355110076,-0.982890773812984,-9.06501463014399E-5));
#38867=DIRECTION('ref_axis',(0.982787919027527,0.184168744770422,0.0144837724102069));
#38868=DIRECTION('center_axis',(0.546277345439608,0.837604352149702,-0.000105448247164003));
#38869=DIRECTION('ref_axis',(0.837542514274121,-0.546235476912526,0.0122204969428009));
#38870=DIRECTION('center_axis',(5.15167520928809E-67,-1.18789542670764E-48,
-1.));
#38871=DIRECTION('ref_axis',(0.,1.,0.));
#38872=DIRECTION('center_axis',(0.260738282110494,-0.965409519336027,-9.06501465102787E-5));
#38873=DIRECTION('ref_axis',(0.965308598687087,0.260709665412434,0.0144837723438797));
#38874=DIRECTION('center_axis',(0.47887567464682,0.877882724008293,-0.000105448247318393));
#38875=DIRECTION('ref_axis',(0.877817791791359,-0.47883878693017,0.0122204969532827));
#38876=DIRECTION('center_axis',(5.15167520928809E-67,-1.18789542670764E-48,
-1.));
#38877=DIRECTION('ref_axis',(0.,1.,0.));
#38878=DIRECTION('center_axis',(0.335679670898317,-0.941976194140886,-9.06501463025926E-5));
#38879=DIRECTION('ref_axis',(0.941877829837149,0.335643224273232,0.0144837723239312));
#38880=DIRECTION('center_axis',(0.408521576078182,0.912748656947391,-0.000105448247109452));
#38881=DIRECTION('ref_axis',(0.912681030717227,-0.408489896596761,0.0122204970155898));
#38882=DIRECTION('center_axis',(5.15167520928809E-67,-1.18789542670764E-48,
-1.));
#38883=DIRECTION('ref_axis',(0.,1.,0.));
#38884=DIRECTION('center_axis',(0.40855148288974,-0.912735272470143,-9.06501463607514E-5));
#38885=DIRECTION('ref_axis',(0.912640070959719,0.408507431042997,0.0144837723432182));
#38886=DIRECTION('center_axis',(0.33564880614496,0.941987190897058,-0.00010544824731253));
#38887=DIRECTION('ref_axis',(0.941917287593217,-0.335622530213924,0.0122204969555834));
#38888=DIRECTION('center_axis',(5.15167520928809E-67,-1.18789542670764E-48,
-1.));
#38889=DIRECTION('ref_axis',(0.,1.,0.));
#38890=DIRECTION('center_axis',(0.47890443913187,-0.877867034329425,-9.06501464476592E-5));
#38891=DIRECTION('ref_axis',(0.877775582561568,0.47885305365786,0.0144837723415746));
#38892=DIRECTION('center_axis',(0.260706649725499,0.965418060567325,-0.000105448239035086));
#38893=DIRECTION('ref_axis',(0.965346311123191,-0.260685939332472,0.0122205006114622));
#38894=DIRECTION('center_axis',(5.15167520928809E-67,-1.18789542670764E-48,
-1.));
#38895=DIRECTION('ref_axis',(0.,1.,0.));
#38896=DIRECTION('center_axis',(0.546304790255255,-0.837586454001444,-9.0650146342598E-5));
#38897=DIRECTION('ref_axis',(0.837499315807156,0.546246387962813,0.0144837723030219));
#38898=DIRECTION('center_axis',(0.184157150081292,0.982896806869675,-0.000105448247335927));
#38899=DIRECTION('ref_axis',(0.982823653730575,-0.184142132936566,0.0122204969315608));
#38900=DIRECTION('center_axis',(5.15167520928809E-67,-1.18789542670764E-48,
-1.));
#38901=DIRECTION('ref_axis',(0.,1.,0.));
#38902=DIRECTION('center_axis',(0.610336990681674,-0.792141874658946,-9.06501464101343E-5));
#38903=DIRECTION('ref_axis',(0.792059587273886,0.610271931640238,0.0144837722853376));
#38904=DIRECTION('center_axis',(0.106472260386401,0.99431566750649,-0.000105448247238185));
#38905=DIRECTION('ref_axis',(0.994241561642249,-0.106463029063635,0.0122204969529716));
#38906=DIRECTION('center_axis',(5.15167520928809E-67,-1.18789542670764E-48,
-1.));
#38907=DIRECTION('ref_axis',(0.,1.,0.));
#38908=DIRECTION('center_axis',(0.670606260602894,-0.741813477245294,-9.06501464627064E-5));
#38909=DIRECTION('ref_axis',(0.741736547997723,0.670534945922382,0.0144837723432088));
#38910=DIRECTION('center_axis',(0.0281309337999561,0.999604241409674,-0.000105448247417899));
#38911=DIRECTION('ref_axis',(0.999529639708026,-0.0281275452133787,0.0122204969380853));
#38912=DIRECTION('center_axis',(5.15167520928809E-67,-1.18789542670764E-48,
-1.));
#38913=DIRECTION('ref_axis',(0.,1.,0.));
#38914=DIRECTION('center_axis',(0.726741019928368,-0.686911553066351,-9.0650146471134E-5));
#38915=DIRECTION('ref_axis',(0.686840456251459,0.726663889288164,0.0144837723292476));
#38916=DIRECTION('center_axis',(-0.050383829347144,0.998729922762398,-0.000105448247269544));
#38917=DIRECTION('ref_axis',(0.998655285167744,0.0503813543057988,0.0122204969148411));
#38918=DIRECTION('center_axis',(5.15167520928809E-67,-1.18789542670764E-48,
-1.));
#38919=DIRECTION('ref_axis',(0.,1.,0.));
#38920=DIRECTION('center_axis',(0.778395179200218,-0.627774590741304,-9.06501463631465E-5));
#38921=DIRECTION('ref_axis',(0.627709764694807,0.778312708136684,0.0144837722894029));
#38922=DIRECTION('center_axis',(-0.12858795942834,0.991698102030413,-0.000105448245500489));
#38923=DIRECTION('ref_axis',(0.991623888698102,0.128579636017312,0.0122204977357358));
#38924=DIRECTION('center_axis',(5.15167520928809E-67,-1.18789542670764E-48,
-1.));
#38925=DIRECTION('ref_axis',(0.,1.,0.));
#38926=DIRECTION('center_axis',(0.825250273349428,-0.564767189308343,-9.06501464028957E-5));
#38927=DIRECTION('ref_axis',(0.564709033703531,0.825162970323003,0.0144837723450398));
#38928=DIRECTION('center_axis',(-0.205999301987628,0.978552132725322,-0.000105448247257059));
#38929=DIRECTION('ref_axis',(0.978478801225208,0.205985181525983,0.0122204969042825));
#38930=DIRECTION('center_axis',(5.15167520928809E-67,-1.18789542670764E-48,
-1.));
#38931=DIRECTION('ref_axis',(0.,1.,0.));
#38932=DIRECTION('center_axis',(0.867017425139937,-0.498277810349071,-9.06501464136658E-5));
#38933=DIRECTION('ref_axis',(0.498226683735389,0.866925828403975,0.0144837723027363));
#38934=DIRECTION('center_axis',(-0.282140590344626,0.959373064120863,-0.000105448247277017));
#38935=DIRECTION('ref_axis',(0.959301066555094,0.282120759888223,0.0122204969764503));
#38936=DIRECTION('center_axis',(5.15167520928809E-67,-1.18789542670764E-48,
-1.));
#38937=DIRECTION('ref_axis',(0.,1.,0.));
#38938=DIRECTION('center_axis',(0.90343912619187,-0.42871638299489,-9.06501464260602E-5));
#38939=DIRECTION('ref_axis',(0.428672600584421,0.903343800469878,0.0144837723272369));
#38940=DIRECTION('center_axis',(-0.356542388139781,0.934279141552593,-0.000105448246761887));
#38941=DIRECTION('ref_axis',(0.934208921809314,0.35651696994953,0.012220497120973));
#38942=DIRECTION('center_axis',(5.15167520928809E-67,-1.18789542670764E-48,
-1.));
#38943=DIRECTION('ref_axis',(0.,1.,0.));
#38944=DIRECTION('center_axis',(0.934290824606888,-0.35651177657678,-9.06501464134324E-5));
#38945=DIRECTION('ref_axis',(0.356475608302711,0.934192357613664,0.0144837723482609));
#38946=DIRECTION('center_axis',(-0.428745983551679,0.903425077396555,-0.000105448247222545));
#38947=DIRECTION('ref_axis',(0.903357068407448,0.428715134340562,0.0122204969479439));
#38948=DIRECTION('center_axis',(5.15167520928809E-67,-1.18789542670764E-48,
-1.));
#38949=DIRECTION('ref_axis',(0.,1.,0.));
#38950=DIRECTION('center_axis',(0.959382309405034,-0.282109156503675,-9.06501462956451E-5));
#38951=DIRECTION('ref_axis',(0.282080825355574,0.959281308222623,0.0144837723473633));
#38952=DIRECTION('center_axis',(-0.498306217401744,0.867001097219279,-0.000105448247347347));
#38953=DIRECTION('ref_axis',(0.866935718280794,0.498270127364887,0.0122204969106369));
#38954=DIRECTION('center_axis',(5.15167520928809E-67,-1.18789542670764E-48,
-1.));
#38955=DIRECTION('ref_axis',(0.,1.,0.));
#38956=DIRECTION('center_axis',(0.978558883238587,-0.205967239670296,-9.06501464061553E-5));
#38957=DIRECTION('ref_axis',(0.205946920319019,0.978455970572407,0.0144837723787919));
#38958=DIRECTION('center_axis',(-0.564794227717559,0.825231766970706,-0.000105448247271081));
#38959=DIRECTION('ref_axis',(0.825169421165301,0.564753119361831,0.0122204969131223));
#38960=DIRECTION('center_axis',(5.15167520928809E-67,-1.18789542670764E-48,
-1.));
#38961=DIRECTION('ref_axis',(0.,1.,0.));
#38962=DIRECTION('center_axis',(0.99170231615319,-0.128555466312983,-9.06501463191467E-5));
#38963=DIRECTION('ref_axis',(0.128543284034309,0.991598126495285,0.014483772323378));
#38964=DIRECTION('center_axis',(-0.627800093806562,0.778374608461208,-0.000105448247350595));
#38965=DIRECTION('ref_axis',(0.778315680171392,0.627754220578551,0.0122204969276863));
#38966=DIRECTION('center_axis',(5.15167520928809E-67,-1.18789542670764E-48,
-1.));
#38967=DIRECTION('ref_axis',(0.,1.,0.));
#38968=DIRECTION('center_axis',(0.998731574514188,-0.0503511057570843,-9.06501463742907E-5));
#38969=DIRECTION('ref_axis',(0.0503471356586318,0.998626750227146,0.0144837723587898));
#38970=DIRECTION('center_axis',(-0.686935363552425,0.726718511654798,-0.000105448247333776));
#38971=DIRECTION('ref_axis',(0.726663364192883,0.686885008275621,0.0122204969654078));
#38972=DIRECTION('center_axis',(5.15167520928809E-67,-1.18789542670764E-48,
-1.));
#38973=DIRECTION('ref_axis',(0.,1.,0.));
#38974=DIRECTION('center_axis',(0.999603320606373,0.0281636861093081,-9.0650146390368E-5));
#38975=DIRECTION('ref_axis',(0.0281594195505035,-0.99949850796739,-0.0144837723518616));
#38976=DIRECTION('center_axis',(-0.741835448352795,0.670581953565614,-0.000105448247334273));
#38977=DIRECTION('ref_axis',(0.670530926935027,0.741780921485189,0.0122204968899333));
#38978=DIRECTION('center_axis',(5.15167520928809E-67,-1.18789542670764E-48,
-1.));
#38979=DIRECTION('ref_axis',(0.,1.,0.));
#38980=DIRECTION('center_axis',(0.994312179825183,0.106504839485559,-9.06501463756277E-5));
#38981=DIRECTION('ref_axis',(0.106492362574294,-0.994208025039266,-0.0144837723286163));
#38982=DIRECTION('center_axis',(-0.792161870920044,0.610311034752874,-0.00010544824088436));
#38983=DIRECTION('ref_axis',(0.610264443527485,0.792103508609612,0.0122204997619462));
#38984=DIRECTION('center_axis',(5.15167520928809E-67,-1.18789542670764E-48,
-1.));
#38985=DIRECTION('ref_axis',(0.,1.,0.));
#38986=DIRECTION('center_axis',(0.982890773813025,0.184189355109853,-9.06501463812825E-5));
#38987=DIRECTION('ref_axis',(0.184168744770323,-0.982787919028214,-0.0144837723648623));
#38988=DIRECTION('center_axis',(-0.837604352149864,0.54627734543936,-0.00010544824728987));
#38989=DIRECTION('ref_axis',(0.546235476912709,0.837542514274935,0.0122204968788532));
#38990=DIRECTION('center_axis',(5.15167520928809E-67,-1.18789542670764E-48,
-1.));
#38991=DIRECTION('ref_axis',(0.,1.,0.));
#38992=DIRECTION('center_axis',(-0.778374608461274,-0.62780009380648,-0.000105448247267533));
#38993=DIRECTION('ref_axis',(0.627754220578446,-0.77831568017143,-0.0122204969306265));
#38994=DIRECTION('center_axis',(0.128555466313028,0.991702316153185,-9.06501463500336E-5));
#38995=DIRECTION('ref_axis',(0.991598126495177,-0.128543284034342,-0.0144837723304925));
#38996=DIRECTION('center_axis',(5.15167520928809E-67,-1.18789542670764E-48,
-1.));
#38997=DIRECTION('ref_axis',(0.,1.,0.));
#38998=DIRECTION('center_axis',(-0.825231766970672,-0.564794227717608,-0.000105448247309068));
#38999=DIRECTION('ref_axis',(0.564753119361638,-0.825169421164907,-0.012220496948613));
#39000=DIRECTION('center_axis',(0.205967239670274,0.978558883238591,-9.0650146374353E-5));
#39001=DIRECTION('ref_axis',(0.978455970572943,-0.205946920319105,-0.0144837723413512));
#39002=DIRECTION('center_axis',(5.15167520928809E-67,-1.18789542670764E-48,
-1.));
#39003=DIRECTION('ref_axis',(0.,1.,0.));
#39004=DIRECTION('center_axis',(-0.86700109721932,-0.498306217401672,-0.00010544824729092));
#39005=DIRECTION('ref_axis',(0.498270127364739,-0.8669357182807,-0.0122204969233888));
#39006=DIRECTION('center_axis',(0.282109156504052,0.959382309404923,-9.06501464701313E-5));
#39007=DIRECTION('ref_axis',(0.959281308222407,-0.282080825355923,-0.0144837723548786));
#39008=DIRECTION('center_axis',(5.15167520928809E-67,-1.18789542670764E-48,
-1.));
#39009=DIRECTION('ref_axis',(0.,1.,0.));
#39010=DIRECTION('center_axis',(-0.903425077396529,-0.428745983551733,-0.000105448247249315));
#39011=DIRECTION('ref_axis',(0.428715134340504,-0.903357068407182,-0.0122204969696425));
#39012=DIRECTION('center_axis',(0.356511776576785,0.934290824606886,-9.06501464239672E-5));
#39013=DIRECTION('ref_axis',(0.934192357613866,-0.356475608302793,-0.0144837723332318));
#39014=DIRECTION('center_axis',(5.15167520928809E-67,-1.18789542670764E-48,
-1.));
#39015=DIRECTION('ref_axis',(0.,1.,0.));
#39016=DIRECTION('center_axis',(-0.934279141552621,-0.356542388139705,-0.000105448246733279));
#39017=DIRECTION('ref_axis',(0.356516969949183,-0.934208921808614,-0.0122204971846563));
#39018=DIRECTION('center_axis',(0.428716382994808,0.903439126191909,-9.06501463770139E-5));
#39019=DIRECTION('ref_axis',(0.903343800469329,-0.428672600584064,-0.0144837723720362));
#39020=DIRECTION('center_axis',(5.15167520928809E-67,-1.18789542670764E-48,
-1.));
#39021=DIRECTION('ref_axis',(0.,1.,0.));
#39022=DIRECTION('center_axis',(-0.959373064120865,-0.282140590344618,-0.000105448247270857));
#39023=DIRECTION('ref_axis',(0.282120759888191,-0.959301066555013,-0.0122204969835453));
#39024=DIRECTION('center_axis',(0.498277810349034,0.867017425139958,-9.06501463569771E-5));
#39025=DIRECTION('ref_axis',(0.866925828403698,-0.498226683735182,-0.0144837723264648));
#39026=DIRECTION('center_axis',(5.15167520928809E-67,-1.18789542670764E-48,
-1.));
#39027=DIRECTION('ref_axis',(0.,1.,0.));
#39028=DIRECTION('center_axis',(-0.978552132725285,-0.205999301987804,-0.000105448247338301));
#39029=DIRECTION('ref_axis',(0.205985181526041,-0.978478801224581,-0.0122204969535068));
#39030=DIRECTION('center_axis',(0.564767189308271,0.825250273349477,-9.06501463565956E-5));
#39031=DIRECTION('ref_axis',(0.825162970322881,-0.564709033703342,-0.0144837723594094));
#39032=DIRECTION('center_axis',(5.15167520928809E-67,-1.18789542670764E-48,
-1.));
#39033=DIRECTION('ref_axis',(0.,1.,0.));
#39034=DIRECTION('center_axis',(-0.991698102030424,-0.128587959428258,-0.000105448245434831));
#39035=DIRECTION('ref_axis',(0.128579636017166,-0.991623888697594,-0.0122204977785004));
#39036=DIRECTION('center_axis',(0.627774590741263,0.778395179200251,-9.06501463298504E-5));
#39037=DIRECTION('ref_axis',(0.778312708136619,-0.627709764694687,-0.0144837722981268));
#39038=DIRECTION('center_axis',(5.15167520928809E-67,-1.18789542670764E-48,
-1.));
#39039=DIRECTION('ref_axis',(0.,1.,0.));
#39040=DIRECTION('center_axis',(-0.998729922762387,-0.0503838293473624,
-0.000105448247373321));
#39041=DIRECTION('ref_axis',(0.0503813543060242,-0.998655285167869,-0.0122204969036645));
#39042=DIRECTION('center_axis',(0.686911553066443,0.726741019928282,-9.06501464895761E-5));
#39043=DIRECTION('ref_axis',(0.726663889287984,-0.686840456251464,-0.0144837723380814));
#39044=DIRECTION('center_axis',(5.15167520928809E-67,-1.18789542670764E-48,
-1.));
#39045=DIRECTION('ref_axis',(0.,1.,0.));
#39046=DIRECTION('center_axis',(-0.999604241409666,0.0281309338002504,-0.00010544824728445));
#39047=DIRECTION('ref_axis',(0.0281275452136831,0.999529639708247,0.0122204969192793));
#39048=DIRECTION('center_axis',(0.741813477245179,0.670606260603021,-9.06501463486941E-5));
#39049=DIRECTION('ref_axis',(0.670534945922386,-0.741736547997471,-0.0144837723559454));
#39050=DIRECTION('center_axis',(5.15167520928809E-67,-1.18789542670764E-48,
-1.));
#39051=DIRECTION('ref_axis',(0.,1.,0.));
#39052=DIRECTION('center_axis',(-0.994315667506492,0.106472260386385,-0.000105448247246095));
#39053=DIRECTION('ref_axis',(0.106463029063669,0.99424156164268,0.0122204969176238));
#39054=DIRECTION('center_axis',(0.792141874658893,0.610336990681743,-9.06501463537118E-5));
#39055=DIRECTION('ref_axis',(0.610271931639807,-0.792059587273192,-0.0144837723414781));
#39056=DIRECTION('center_axis',(5.15167520928809E-67,-1.18789542670764E-48,
-1.));
#39057=DIRECTION('ref_axis',(0.,1.,0.));
#39058=DIRECTION('center_axis',(-0.98289680686965,0.184157150081429,-0.000105448247288298));
#39059=DIRECTION('ref_axis',(0.184142132936832,0.982823653731204,0.0122204968770007));
#39060=DIRECTION('center_axis',(0.837586454001503,0.546304790255165,-9.06501464022278E-5));
#39061=DIRECTION('ref_axis',(0.546246387962582,-0.837499315807004,-0.0144837723204838));
#39062=DIRECTION('center_axis',(5.15167520928809E-67,-1.18789542670764E-48,
-1.));
#39063=DIRECTION('ref_axis',(0.,1.,0.));
#39064=DIRECTION('center_axis',(-0.965418060567323,0.260706649725506,-0.000105448239021929));
#39065=DIRECTION('ref_axis',(0.260685939332638,0.965346311123758,0.0122205005631217));
#39066=DIRECTION('center_axis',(0.877867034329392,0.478904439131931,-9.06501464072983E-5));
#39067=DIRECTION('ref_axis',(0.478853053658107,-0.87777558256187,-0.0144837723150808));
#39068=DIRECTION('center_axis',(5.15167520928809E-67,-1.18789542670764E-48,
-1.));
#39069=DIRECTION('ref_axis',(0.,1.,0.));
#39070=DIRECTION('center_axis',(-0.94198719089703,0.335648806145038,-0.000105448247300868));
#39071=DIRECTION('ref_axis',(0.335622530213848,0.941917287592769,0.0122204969921728));
#39072=DIRECTION('center_axis',(0.912735272470196,0.40855148288962,-9.06501464040206E-5));
#39073=DIRECTION('ref_axis',(0.408507431043198,-0.912640070960478,-0.01448377228974));
#39074=DIRECTION('center_axis',(5.15167520928809E-67,-1.18789542670764E-48,
-1.));
#39075=DIRECTION('ref_axis',(0.,1.,0.));
#39076=DIRECTION('center_axis',(0.965409519335958,0.260738282110751,-9.06501464007405E-5));
#39077=DIRECTION('ref_axis',(0.260709665412327,-0.965308598685698,-0.0144837724383535));
#39078=DIRECTION('center_axis',(-0.87788272400828,0.478875674646843,-0.000105448247307507));
#39079=DIRECTION('ref_axis',(0.478838786930294,0.877817791791527,0.0122204969363654));
#39080=DIRECTION('center_axis',(5.15167520928809E-67,-1.18789542670764E-48,
-1.));
#39081=DIRECTION('ref_axis',(-4.33680868994202E-19,1.,-1.18789542670764E-48));
#39082=DIRECTION('center_axis',(5.15167520928809E-67,-1.18789542670764E-48,
-1.));
#39083=DIRECTION('ref_axis',(-4.33680868994202E-19,1.,-1.18789542670764E-48));
#39084=DIRECTION('center_axis',(5.15167520928809E-67,-1.18789542670764E-48,
-1.));
#39085=DIRECTION('ref_axis',(0.,1.,0.));
#39086=DIRECTION('center_axis',(0.941987190897879,0.335648806142656,0.000105448247691596));
#39087=DIRECTION('ref_axis',(0.335622530211987,-0.941917287595053,0.0122204968672344));
#39088=DIRECTION('center_axis',(-0.912735272471169,0.408551482887447,9.06501467246596E-5));
#39089=DIRECTION('ref_axis',(0.408507431040732,0.912640070960819,-0.0144837723377799));
#39090=DIRECTION('center_axis',(5.15167520928809E-67,-1.18789542670764E-48,
-1.));
#39091=DIRECTION('ref_axis',(-4.33680868994202E-19,1.,-1.18789542670764E-48));
#39092=DIRECTION('center_axis',(5.15167520928809E-67,-1.18789542670764E-48,
-1.));
#39093=DIRECTION('ref_axis',(-4.33680868994202E-19,1.,-1.18789542670764E-48));
#39094=DIRECTION('',(-5.15167520928809E-67,1.18789542670764E-48,1.));
#39095=DIRECTION('',(5.15167520928809E-67,-1.18789542670764E-48,-1.));
#39096=DIRECTION('center_axis',(5.15167520928809E-67,-1.18789542670764E-48,
-1.));
#39097=DIRECTION('ref_axis',(-4.33680868994202E-19,1.,-1.18789542670764E-48));
#39098=DIRECTION('center_axis',(5.15167520928809E-67,-1.18789542670764E-48,
-1.));
#39099=DIRECTION('ref_axis',(0.,1.,0.));
#39100=DIRECTION('center_axis',(0.941976194140935,0.33567967089818,-9.06501463865783E-5));
#39101=DIRECTION('ref_axis',(0.335643224273153,-0.94187782983736,-0.014483772312066));
#39102=DIRECTION('center_axis',(-0.912748656947277,0.408521576078436,-0.000105448246989675));
#39103=DIRECTION('ref_axis',(0.408489896596946,0.91268103071696,0.012220497029356));
#39104=DIRECTION('center_axis',(-5.15167520928809E-67,1.18789542670764E-48,
1.));
#39105=DIRECTION('ref_axis',(4.33680868994202E-19,-1.,1.18789542670764E-48));
#39106=DIRECTION('center_axis',(0.,0.,1.));
#39107=DIRECTION('ref_axis',(1.,4.33680868994202E-19,0.));
#39108=DIRECTION('',(0.866025403784438,0.5,0.));
#39109=DIRECTION('',(-4.33680868994202E-19,1.,0.));
#39110=DIRECTION('',(-0.866025403784439,0.499999999999999,0.));
#39111=DIRECTION('',(-0.866025403784439,-0.5,0.));
#39112=DIRECTION('',(6.01359520363859E-16,-1.,0.));
#39113=DIRECTION('',(0.866025403784439,-0.5,0.));
#39114=DIRECTION('center_axis',(1.,4.33680868994202E-19,0.));
#39115=DIRECTION('ref_axis',(0.,0.,-1.));
#39116=DIRECTION('',(0.,0.,1.));
#39117=DIRECTION('',(0.,0.,1.));
#39118=DIRECTION('center_axis',(0.499999999999999,0.866025403784439,0.));
#39119=DIRECTION('ref_axis',(-0.866025403784439,0.499999999999999,0.));
#39120=DIRECTION('',(0.,0.,1.));
#39121=DIRECTION('center_axis',(-0.5,0.866025403784439,0.));
#39122=DIRECTION('ref_axis',(-0.866025403784439,-0.5,0.));
#39123=DIRECTION('',(0.,0.,1.));
#39124=DIRECTION('center_axis',(-1.,-6.01359520363859E-16,0.));
#39125=DIRECTION('ref_axis',(6.01359520363859E-16,-1.,0.));
#39126=DIRECTION('',(0.,0.,1.));
#39127=DIRECTION('center_axis',(-0.5,-0.866025403784439,0.));
#39128=DIRECTION('ref_axis',(0.866025403784439,-0.5,0.));
#39129=DIRECTION('',(0.,0.,1.));
#39130=DIRECTION('center_axis',(0.5,-0.866025403784439,0.));
#39131=DIRECTION('ref_axis',(0.866025403784439,0.5,0.));
#39132=DIRECTION('',(1.0568194522281E-16,0.866025403784468,-0.499999999999949));
#39133=DIRECTION('center_axis',(4.70261923768679E-35,-1.08435016942139E-16,
1.));
#39134=DIRECTION('ref_axis',(0.378466979033695,0.925614793410903,1.00369055805406E-16));
#39135=DIRECTION('center_axis',(0.912653256146669,-0.408734674385332,0.));
#39136=DIRECTION('ref_axis',(0.408734674385332,0.912653256146669,0.));
#39137=DIRECTION('',(0.,0.,1.));
#39138=DIRECTION('center_axis',(0.,0.,1.));
#39139=DIRECTION('ref_axis',(1.,4.33680868994202E-19,0.));
#39140=DIRECTION('',(0.,0.,1.));
#39141=DIRECTION('center_axis',(-0.912653256146668,-0.408734674385334,0.));
#39142=DIRECTION('ref_axis',(0.408734674385334,-0.912653256146668,0.));
#39143=DIRECTION('center_axis',(0.877770897795706,-0.479080630982844,8.35636401295593E-50));
#39144=DIRECTION('ref_axis',(0.479080630982844,0.877770897795706,2.97282767021015E-66));
#39145=DIRECTION('',(-9.32012009987243E-50,3.66188516048321E-51,1.));
#39146=DIRECTION('center_axis',(-9.32012009987243E-50,3.66188516048321E-51,
1.));
#39147=DIRECTION('ref_axis',(1.,4.33680868994202E-19,9.32012009987243E-50));
#39148=DIRECTION('',(-9.32012009987243E-50,3.66188516048321E-51,1.));
#39149=DIRECTION('center_axis',(-0.941908803685482,-0.335868732602165,-8.65571190069724E-50));
#39150=DIRECTION('ref_axis',(0.335868732602165,-0.941908803685482,-2.86613947502886E-66));
#39151=DIRECTION('center_axis',(0.941908803685478,-0.335868732602176,-8.65571190069562E-50));
#39152=DIRECTION('ref_axis',(0.335868732602176,0.941908803685478,5.69318196416785E-66));
#39153=DIRECTION('',(9.32012009987071E-50,3.66188516048189E-51,1.));
#39154=DIRECTION('center_axis',(9.32012009987071E-50,3.66188516048189E-51,
1.));
#39155=DIRECTION('ref_axis',(1.,4.33680868994202E-19,-9.32012009987071E-50));
#39156=DIRECTION('',(9.32012009987071E-50,3.66188516048189E-51,1.));
#39157=DIRECTION('center_axis',(-0.877770897795712,-0.479080630982834,8.35636401295441E-50));
#39158=DIRECTION('ref_axis',(0.479080630982834,-0.877770897795712,-1.78392693329902E-66));
#39159=DIRECTION('center_axis',(0.965357170233111,-0.260932048394827,-1.75574063469501E-49));
#39160=DIRECTION('ref_axis',(0.260932048394827,0.965357170233111,-8.03239509524584E-66));
#39161=DIRECTION('',(1.85827785600731E-49,1.46249639022155E-50,1.));
#39162=DIRECTION('center_axis',(1.8582778560073E-49,1.46249639022155E-50,
1.));
#39163=DIRECTION('ref_axis',(1.,4.33680868994202E-19,-1.8582778560073E-49));
#39164=DIRECTION('',(1.85827785600731E-49,1.46249639022155E-50,1.));
#39165=DIRECTION('center_axis',(-0.837476789971396,-0.546472896179862,1.63618603752562E-49));
#39166=DIRECTION('ref_axis',(0.546472896179862,-0.837476789971396,1.23627039651628E-65));
#39167=DIRECTION('center_axis',(0.982853788812423,-0.184386631340412,-2.66502014323869E-49));
#39168=DIRECTION('ref_axis',(0.184386631340412,0.982853788812423,-4.59929189808117E-66));
#39169=DIRECTION('',(2.77308680110516E-49,3.28216451991643E-50,1.));
#39170=DIRECTION('center_axis',(2.77308680110516E-49,3.28216451991643E-50,
1.));
#39171=DIRECTION('ref_axis',(1.,4.33680868994202E-19,-2.77308680110516E-49));
#39172=DIRECTION('',(2.77308680110516E-49,3.28216451991643E-50,1.));
#39173=DIRECTION('center_axis',(-0.792019359247614,-0.610495974251263,2.39671325397326E-49));
#39174=DIRECTION('ref_axis',(0.610495974251263,-0.792019359247614,-2.26955332198497E-65));
#39175=DIRECTION('center_axis',(0.994290786951656,-0.106704409389008,-3.5878037051643E-49));
#39176=DIRECTION('ref_axis',(0.106704409389008,0.994290786951656,1.37166247450949E-66));
#39177=DIRECTION('',(3.67079874392927E-49,5.81397404601223E-50,1.));
#39178=DIRECTION('center_axis',(3.67079874392927E-49,5.81397404601223E-50,
1.));
#39179=DIRECTION('ref_axis',(1.,4.33680868994202E-19,-3.67079874392927E-49));
#39180=DIRECTION('',(3.67079874392927E-49,5.81397404601223E-50,1.));
#39181=DIRECTION('center_axis',(-0.741678865800908,-0.670755141630892,3.11252914744798E-49));
#39182=DIRECTION('ref_axis',(0.670755141630892,-0.741678865800908,-3.59898235302298E-65));
#39183=DIRECTION('center_axis',(0.999597651754094,-0.028364319270904,-4.5184020529559E-49));
#39184=DIRECTION('ref_axis',(0.028364319270904,0.999597651754094,-3.26521667006146E-66));
#39185=DIRECTION('',(4.54587899183259E-49,9.04231552086841E-50,1.));
#39186=DIRECTION('center_axis',(4.54587899183259E-49,9.04231552086841E-50,
1.));
#39187=DIRECTION('ref_axis',(1.,4.33680868994202E-19,-4.54587899183259E-49));
#39188=DIRECTION('',(4.54587899183259E-49,9.04231552086841E-50,1.));
#39189=DIRECTION('center_axis',(-0.68676567551329,-0.726878880513649,3.77922047493358E-49));
#39190=DIRECTION('ref_axis',(0.726878880513649,-0.68676567551329,8.44347396578498E-67));
#39191=DIRECTION('center_axis',(0.998741664633518,0.0501506463075991,-5.45107773834402E-49));
#39192=DIRECTION('ref_axis',(-0.0501506463075991,0.998741664633518,-5.68155672720376E-65));
#39193=DIRECTION('center_axis',(-0.62761834646337,-0.778521169386283,4.39267686269876E-49));
#39194=DIRECTION('ref_axis',(0.778521169386283,-0.62761834646337,2.86838711888421E-65));
#39195=DIRECTION('center_axis',(0.991728103035171,0.128356416474834,-6.38008050558209E-49));
#39196=DIRECTION('ref_axis',(-0.128356416474834,0.991728103035171,2.64164793875071E-66));
#39197=DIRECTION('center_axis',(-0.564601541603225,-0.825363616365092,4.94911614811798E-49));
#39198=DIRECTION('ref_axis',(0.825363616365092,-0.564601541603225,-1.21982614064914E-65));
#39199=DIRECTION('center_axis',(0.978600207898554,0.20577082665166,-7.29968274368531E-49));
#39200=DIRECTION('ref_axis',(-0.20577082665166,0.978600207898554,7.99368498149713E-66));
#39201=DIRECTION('center_axis',(-0.498103780490032,-0.867117422187756,5.44510769796179E-49));
#39202=DIRECTION('ref_axis',(0.867117422187756,-0.498103780490032,-1.67935322369464E-65));
#39203=DIRECTION('center_axis',(0.95943891706265,0.281916591256437,-8.20421479905702E-49));
#39204=DIRECTION('ref_axis',(-0.281916591256437,0.95943891706265,1.24589067679861E-65));
#39205=DIRECTION('center_axis',(-0.428535043933802,-0.903525160756829,5.87759355939149E-49));
#39206=DIRECTION('ref_axis',(0.903525160756829,-0.428535043933802,-8.86364012879408E-65));
#39207=DIRECTION('center_axis',(0.93436236625724,0.356324246329338,-9.08809993078841E-49));
#39208=DIRECTION('ref_axis',(-0.356324246329338,0.93436236625724,-2.69950222050985E-65));
#39209=DIRECTION('center_axis',(-0.356324246329358,-0.934362366257233,6.24390731325522E-49));
#39210=DIRECTION('ref_axis',(0.934362366257233,-0.356324246329358,4.50754916861586E-65));
#39211=DIRECTION('center_axis',(0.903525160756839,0.428535043933782,-9.94588869312071E-49));
#39212=DIRECTION('ref_axis',(-0.428535043933782,0.903525160756839,-3.06876799885187E-65));
#39213=DIRECTION('center_axis',(-0.281916591256458,-0.959438917062644,6.54179051344872E-49));
#39214=DIRECTION('ref_axis',(0.959438917062644,-0.281916591256458,5.46345068117847E-65));
#39215=DIRECTION('center_axis',(0.867117422187767,0.498103780490012,-1.07722925330905E-48));
#39216=DIRECTION('ref_axis',(-0.498103780490012,0.867117422187767,2.63677046246647E-65));
#39217=DIRECTION('center_axis',(-0.205770826651682,-0.978600207898549,6.76940661098659E-49));
#39218=DIRECTION('ref_axis',(0.978600207898549,-0.205770826651682,1.20007194121145E-65));
#39219=DIRECTION('center_axis',(0.825363616365104,0.564601541603207,-1.15622163962171E-48));
#39220=DIRECTION('ref_axis',(-0.564601541603207,0.825363616365104,5.34857418276646E-65));
#39221=DIRECTION('center_axis',(-0.128356416474855,-0.991728103035168,6.92535227693746E-49));
#39222=DIRECTION('ref_axis',(0.991728103035168,-0.128356416474855,1.05782428992148E-64));
#39223=DIRECTION('center_axis',(0.778521169386297,0.627618346463353,-1.2310790139208E-48));
#39224=DIRECTION('ref_axis',(-0.627618346463353,0.778521169386297,-3.24299836420865E-65));
#39225=DIRECTION('center_axis',(-0.0501506463076206,-0.998741664633517,
7.00866605441356E-49));
#39226=DIRECTION('ref_axis',(0.998741664633517,-0.0501506463076206,5.61717615944791E-66));
#39227=DIRECTION('center_axis',(0.83747678997139,-0.546472896179871,1.63618603752577E-49));
#39228=DIRECTION('ref_axis',(0.546472896179871,0.83747678997139,8.18221406165844E-66));
#39229=DIRECTION('',(-1.85827785600747E-49,1.46249639022181E-50,1.));
#39230=DIRECTION('center_axis',(-1.85827785600747E-49,1.46249639022181E-50,
1.));
#39231=DIRECTION('ref_axis',(1.,4.33680868994202E-19,1.85827785600747E-49));
#39232=DIRECTION('',(-1.85827785600747E-49,1.46249639022181E-50,1.));
#39233=DIRECTION('center_axis',(-0.965357170233114,-0.260932048394816,-1.75574063469517E-49));
#39234=DIRECTION('ref_axis',(0.260932048394816,-0.965357170233114,4.85072620126884E-66));
#39235=DIRECTION('center_axis',(0.792019359247608,-0.610495974251272,2.39671325397339E-49));
#39236=DIRECTION('ref_axis',(0.610495974251272,0.792019359247608,6.86514884131891E-66));
#39237=DIRECTION('',(-2.77308680110532E-49,3.28216451991683E-50,1.));
#39238=DIRECTION('center_axis',(-2.77308680110532E-49,3.28216451991683E-50,
1.));
#39239=DIRECTION('ref_axis',(1.,4.33680868994202E-19,2.77308680110532E-49));
#39240=DIRECTION('',(-2.77308680110532E-49,3.28216451991683E-50,1.));
#39241=DIRECTION('center_axis',(-0.982853788812425,-0.184386631340402,-2.66502014323885E-49));
#39242=DIRECTION('ref_axis',(0.184386631340402,-0.982853788812425,5.0100483719309E-66));
#39243=DIRECTION('center_axis',(0.741678865800901,-0.6707551416309,3.11252914744811E-49));
#39244=DIRECTION('ref_axis',(0.6707551416309,0.741678865800901,2.48321099822104E-65));
#39245=DIRECTION('',(-3.67079874392942E-49,5.81397404601274E-50,1.));
#39246=DIRECTION('center_axis',(-3.67079874392942E-49,5.81397404601274E-50,
1.));
#39247=DIRECTION('ref_axis',(1.,4.33680868994202E-19,3.67079874392942E-49));
#39248=DIRECTION('',(-3.67079874392942E-49,5.81397404601274E-50,1.));
#39249=DIRECTION('center_axis',(-0.994290786951657,-0.106704409388997,-3.58780370516446E-49));
#39250=DIRECTION('ref_axis',(0.106704409388997,-0.994290786951657,8.97464790050996E-66));
#39251=DIRECTION('center_axis',(0.686765675513281,-0.726878880513656,3.77922047493371E-49));
#39252=DIRECTION('ref_axis',(0.726878880513657,0.686765675513281,3.1589153081368E-66));
#39253=DIRECTION('',(-4.54587899183275E-49,9.04231552086907E-50,1.));
#39254=DIRECTION('center_axis',(-4.54587899183275E-49,9.04231552086907E-50,
1.));
#39255=DIRECTION('ref_axis',(1.,4.33680868994202E-19,4.54587899183275E-49));
#39256=DIRECTION('',(-4.54587899183275E-49,9.04231552086907E-50,1.));
#39257=DIRECTION('center_axis',(-0.999597651754094,-0.0283643192708926,
-4.51840205295607E-49));
#39258=DIRECTION('ref_axis',(0.0283643192708926,-0.999597651754094,-3.99287521021606E-67));
#39259=DIRECTION('center_axis',(0.627618346463361,-0.77852116938629,4.39267686269887E-49));
#39260=DIRECTION('ref_axis',(0.77852116938629,0.627618346463361,3.8324092947301E-66));
#39261=DIRECTION('',(-5.39293238409326E-49,1.29472851457609E-49,1.));
#39262=DIRECTION('center_axis',(-5.39293238409326E-49,1.29472851457609E-49,
1.));
#39263=DIRECTION('ref_axis',(-0.453990499739606,-0.891006524188338,-1.29472851457643E-49));
#39264=DIRECTION('',(-5.39293238409326E-49,1.29472851457609E-49,1.));
#39265=DIRECTION('center_axis',(-0.998741664633517,0.0501506463076103,-5.45107773834419E-49));
#39266=DIRECTION('ref_axis',(-0.0501506463076103,-0.998741664633517,1.75141110323522E-67));
#39267=DIRECTION('center_axis',(0.564601541603216,-0.825363616365098,4.94911614811808E-49));
#39268=DIRECTION('ref_axis',(0.825363616365098,0.564601541603216,-2.63676715352381E-65));
#39269=DIRECTION('',(-6.20673655487384E-49,1.75048074844164E-49,1.));
#39270=DIRECTION('center_axis',(-6.20673655487384E-49,1.75048074844164E-49,
1.));
#39271=DIRECTION('ref_axis',(-0.52249856471585,-0.852640164354153,-1.75048074844092E-49));
#39272=DIRECTION('',(-6.20673655487384E-49,1.75048074844164E-49,1.));
#39273=DIRECTION('center_axis',(-0.99172810303517,0.128356416474844,-6.38008050558225E-49));
#39274=DIRECTION('ref_axis',(-0.128356416474844,-0.99172810303517,-6.45104663994926E-66));
#39275=DIRECTION('center_axis',(0.498103780490022,-0.867117422187761,5.44510769796189E-49));
#39276=DIRECTION('ref_axis',(0.867117422187761,0.498103780490022,4.62928424055004E-65));
#39277=DIRECTION('',(-6.98227413084428E-49,2.26867838960881E-49,1.));
#39278=DIRECTION('center_axis',(-6.98227413084428E-49,2.26867838960881E-49,
1.));
#39279=DIRECTION('ref_axis',(-0.587785252292493,-0.809016994374933,-2.26867838960897E-49));
#39280=DIRECTION('',(-6.98227413084428E-49,2.26867838960881E-49,1.));
#39281=DIRECTION('center_axis',(-0.978600207898551,0.205770826651671,-7.29968274368548E-49));
#39282=DIRECTION('ref_axis',(-0.205770826651671,-0.978600207898551,-8.37640359713844E-66));
#39283=DIRECTION('center_axis',(0.428535043933792,-0.903525160756834,5.87759355939158E-49));
#39284=DIRECTION('ref_axis',(0.903525160756834,0.428535043933792,-6.0990810847752E-65));
#39285=DIRECTION('',(-7.71476366495631E-49,2.84612657730158E-49,1.));
#39286=DIRECTION('center_axis',(-7.71476366495631E-49,2.84612657730158E-49,
1.));
#39287=DIRECTION('ref_axis',(-0.649448048330161,-0.76040596560005,-2.84612657730134E-49));
#39288=DIRECTION('',(-7.71476366495631E-49,2.84612657730158E-49,1.));
#39289=DIRECTION('center_axis',(-0.959438917062647,0.281916591256448,-8.20421479905718E-49));
#39290=DIRECTION('ref_axis',(-0.281916591256448,-0.959438917062647,-3.25299225253391E-65));
#39291=DIRECTION('center_axis',(0.356324246329348,-0.934362366257237,6.2439073132553E-49));
#39292=DIRECTION('ref_axis',(0.934362366257237,0.356324246329348,-6.3916346242107E-66));
#39293=DIRECTION('',(-8.39968911565463E-49,3.47926515142182E-49,1.));
#39294=DIRECTION('center_axis',(-8.39968911565463E-49,3.47926515142182E-49,
1.));
#39295=DIRECTION('ref_axis',(-0.707106781186566,-0.707106781186529,-3.47926515142204E-49));
#39296=DIRECTION('',(-8.39968911565463E-49,3.47926515142182E-49,1.));
#39297=DIRECTION('center_axis',(-0.934362366257236,0.356324246329348,-9.08809993078856E-49));
#39298=DIRECTION('ref_axis',(-0.356324246329348,-0.934362366257236,-6.41640199023417E-65));
#39299=DIRECTION('center_axis',(0.281916591256447,-0.959438917062647,6.54179051344879E-49));
#39300=DIRECTION('ref_axis',(0.959438917062647,0.281916591256447,-1.09781434718078E-65));
#39301=DIRECTION('',(-9.03282768977487E-49,4.16419060212015E-49,1.));
#39302=DIRECTION('center_axis',(-9.03282768977487E-49,4.16419060212015E-49,
1.));
#39303=DIRECTION('ref_axis',(-0.760405965599942,-0.649448048330288,-4.16419060211889E-49));
#39304=DIRECTION('',(-9.03282768977487E-49,4.16419060212015E-49,1.));
#39305=DIRECTION('center_axis',(-0.903525160756834,0.428535043933793,-9.94588869312087E-49));
#39306=DIRECTION('ref_axis',(-0.428535043933793,-0.903525160756834,3.14193955482054E-65));
#39307=DIRECTION('center_axis',(0.205770826651671,-0.978600207898551,6.76940661098664E-49));
#39308=DIRECTION('ref_axis',(0.978600207898551,0.205770826651671,1.21103353553181E-65));
#39309=DIRECTION('',(-9.61027587746764E-49,4.89668013623218E-49,1.));
#39310=DIRECTION('center_axis',(-9.61027587746764E-49,4.89668013623218E-49,
1.));
#39311=DIRECTION('ref_axis',(-0.809016994374948,-0.587785252292472,-4.89668013623217E-49));
#39312=DIRECTION('',(-9.61027587746764E-49,4.89668013623218E-49,1.));
#39313=DIRECTION('center_axis',(-0.867117422187761,0.498103780490022,-1.07722925330906E-48));
#39314=DIRECTION('ref_axis',(-0.498103780490022,-0.867117422187761,1.20400755006059E-65));
#39315=DIRECTION('center_axis',(0.128356416474844,-0.99172810303517,6.92535227693751E-49));
#39316=DIRECTION('ref_axis',(0.99172810303517,0.128356416474844,1.37955244398014E-65));
#39317=DIRECTION('',(-1.01284735186348E-48,5.67221771220262E-49,1.));
#39318=DIRECTION('center_axis',(-1.01284735186348E-48,5.67221771220262E-49,
1.));
#39319=DIRECTION('ref_axis',(-0.852640164354111,-0.522498564715917,-5.67221771220297E-49));
#39320=DIRECTION('',(-1.01284735186348E-48,5.67221771220262E-49,1.));
#39321=DIRECTION('center_axis',(-0.825363616365097,0.564601541603216,-1.15622163962172E-48));
#39322=DIRECTION('ref_axis',(-0.564601541603216,-0.825363616365097,3.75089637720347E-65));
#39323=DIRECTION('center_axis',(0.0501506463076098,-0.998741664633517,7.0086660544136E-49));
#39324=DIRECTION('ref_axis',(0.998741664633517,0.0501506463076098,-1.39822384050416E-65));
#39325=DIRECTION('',(-1.05842257525004E-48,6.4860218829832E-49,1.));
#39326=DIRECTION('center_axis',(-1.05842257525004E-48,6.4860218829832E-49,
1.));
#39327=DIRECTION('ref_axis',(-0.891006524188326,-0.453990499739629,-6.48602188298224E-49));
#39328=DIRECTION('',(-1.05842257525004E-48,6.4860218829832E-49,1.));
#39329=DIRECTION('center_axis',(-0.77852116938629,0.627618346463361,-1.23107901392082E-48));
#39330=DIRECTION('ref_axis',(-0.627618346463361,-0.77852116938629,-1.0235164758246E-65));
#39331=DIRECTION('center_axis',(-0.0283643192708931,-0.999597651754094,
7.01883428627214E-49));
#39332=DIRECTION('ref_axis',(0.999597651754094,-0.0283643192708931,-4.40612052675408E-66));
#39333=DIRECTION('',(-1.09747227149895E-48,7.33307527524372E-49,1.));
#39334=DIRECTION('center_axis',(-1.09747227149895E-48,7.33307527524372E-49,
1.));
#39335=DIRECTION('ref_axis',(-0.923879532511259,-0.382683432365157,-7.33307527524286E-49));
#39336=DIRECTION('',(-1.09747227149895E-48,7.33307527524372E-49,1.));
#39337=DIRECTION('center_axis',(-0.726878880513656,0.686765675513282,-1.30133985560119E-48));
#39338=DIRECTION('ref_axis',(-0.686765675513282,-0.726878880513656,-1.0460740182702E-64));
#39339=DIRECTION('center_axis',(-0.106704409388998,-0.994290786951657,6.95579428198243E-49));
#39340=DIRECTION('ref_axis',(0.994290786951657,-0.106704409388998,-7.09717408543387E-66));
#39341=DIRECTION('',(-1.12975568624752E-48,8.20815552314704E-49,1.));
#39342=DIRECTION('center_axis',(-1.12975568624752E-48,8.20815552314704E-49,
1.));
#39343=DIRECTION('ref_axis',(-0.951056516295187,-0.309016994374844,-8.20815552314827E-49));
#39344=DIRECTION('',(-1.12975568624752E-48,8.20815552314704E-49,1.));
#39345=DIRECTION('center_axis',(-0.6707551416309,0.741678865800901,-1.36657098320978E-48));
#39346=DIRECTION('ref_axis',(-0.741678865800901,-0.6707551416309,3.57211103088032E-65));
#39347=DIRECTION('center_axis',(-0.184386631340402,-0.982853788812425,6.81993470413386E-49));
#39348=DIRECTION('ref_axis',(0.982853788812425,-0.184386631340402,2.71684956354986E-65));
#39349=DIRECTION('',(-1.15507378150848E-48,9.10586746597114E-49,1.));
#39350=DIRECTION('center_axis',(-1.15507378150848E-48,9.10586746597114E-49,
1.));
#39351=DIRECTION('ref_axis',(-0.972369920397692,-0.233445363855843,-9.1058674659719E-49));
#39352=DIRECTION('',(-1.15507378150848E-48,9.10586746597114E-49,1.));
#39353=DIRECTION('center_axis',(-0.610495974251271,0.792019359247608,-1.42637022515333E-48));
#39354=DIRECTION('ref_axis',(-0.792019359247608,-0.610495974251271,3.09249712984754E-64));
#39355=DIRECTION('center_axis',(-0.260932048394816,-0.965357170233114,6.61209317220174E-49));
#39356=DIRECTION('ref_axis',(0.965357170233114,-0.260932048394816,1.42679734120621E-65));
#39357=DIRECTION('',(-1.17327046280543E-48,1.0020676411069E-48,1.));
#39358=DIRECTION('center_axis',(-1.17327046280543E-48,1.0020676411069E-48,
1.));
#39359=DIRECTION('ref_axis',(-0.987688340595155,-0.156434465040119,-1.00206764110703E-48));
#39360=DIRECTION('',(-1.17327046280543E-48,1.0020676411069E-48,1.));
#39361=DIRECTION('center_axis',(-0.546472896179871,0.83747678997139,-1.48036889921999E-48));
#39362=DIRECTION('ref_axis',(-0.83747678997139,-0.546472896179871,5.98336102584152E-65));
#39363=DIRECTION('center_axis',(-0.335868732602165,-0.941908803685482,6.33355109834478E-49));
#39364=DIRECTION('ref_axis',(0.941908803685482,-0.335868732602165,5.83703495410428E-65));
#39365=DIRECTION('',(-1.18423354154716E-48,1.09469422570892E-48,1.));
#39366=DIRECTION('center_axis',(-1.18423354154716E-48,1.09469422570892E-48,
1.));
#39367=DIRECTION('ref_axis',(-0.996917333733132,-0.0784590957277897,-1.09469422570898E-48));
#39368=DIRECTION('',(-1.18423354154716E-48,1.09469422570892E-48,1.));
#39369=DIRECTION('center_axis',(-0.479080630982844,0.877770897795706,-1.52823408562776E-48));
#39370=DIRECTION('ref_axis',(-0.877770897795706,-0.479080630982844,-1.85065299173653E-65));
#39371=DIRECTION('center_axis',(-0.408734674385335,-0.912653256146667,5.98602578707292E-49));
#39372=DIRECTION('ref_axis',(0.912653256146667,-0.408734674385335,-4.742731066544E-66));
#39373=DIRECTION('',(-1.18789542670764E-48,1.18789542670765E-48,1.));
#39374=DIRECTION('center_axis',(-1.18789542670764E-48,1.18789542670765E-48,
1.));
#39375=DIRECTION('ref_axis',(4.33680868994202E-19,-1.,1.18789542670765E-48));
#39376=DIRECTION('',(-1.18789542670764E-48,1.18789542670765E-48,1.));
#39377=DIRECTION('center_axis',(-0.408734674385331,0.912653256146669,-1.56967067958564E-48));
#39378=DIRECTION('ref_axis',(-0.912653256146669,-0.408734674385331,-1.44539080722799E-64));
#39379=DIRECTION('center_axis',(-0.479080630982847,-0.877770897795704,5.57165984749406E-49));
#39380=DIRECTION('ref_axis',(0.877770897795704,-0.479080630982847,-3.32989513528092E-65));
#39381=DIRECTION('',(-1.18423354154716E-48,1.28109662770637E-48,1.));
#39382=DIRECTION('center_axis',(-1.18423354154716E-48,1.28109662770637E-48,
1.));
#39383=DIRECTION('ref_axis',(4.33680868994202E-19,-1.,1.28109662770637E-48));
#39384=DIRECTION('',(-1.18423354154716E-48,1.28109662770637E-48,1.));
#39385=DIRECTION('center_axis',(-0.335868732602161,0.941908803685483,-1.60442321071283E-48));
#39386=DIRECTION('ref_axis',(-0.941908803685483,-0.335868732602161,-1.10077185323049E-64));
#39387=DIRECTION('center_axis',(-0.546472896179874,-0.837476789971388,5.09300798341636E-49));
#39388=DIRECTION('ref_axis',(0.837476789971388,-0.546472896179874,-4.24396990687181E-65));
#39389=DIRECTION('',(-1.17327046280542E-48,1.37372321230839E-48,1.));
#39390=DIRECTION('center_axis',(-1.17327046280542E-48,1.37372321230839E-48,
1.));
#39391=DIRECTION('ref_axis',(4.33680868994202E-19,-1.,1.37372321230839E-48));
#39392=DIRECTION('',(-1.17327046280542E-48,1.37372321230839E-48,1.));
#39393=DIRECTION('center_axis',(-0.260932048394812,0.965357170233115,-1.63227741809852E-48));
#39394=DIRECTION('ref_axis',(-0.965357170233115,-0.260932048394812,1.79840374663787E-65));
#39395=DIRECTION('center_axis',(-0.610495974251274,-0.792019359247605,4.55302124274975E-49));
#39396=DIRECTION('ref_axis',(0.792019359247605,-0.610495974251274,-1.92107929694605E-65));
#39397=DIRECTION('',(-1.15507378150847E-48,1.46520410681818E-48,1.));
#39398=DIRECTION('center_axis',(-1.15507378150847E-48,1.46520410681818E-48,
1.));
#39399=DIRECTION('ref_axis',(4.33680868994202E-19,-1.,1.46520410681818E-48));
#39400=DIRECTION('',(-1.15507378150847E-48,1.46520410681818E-48,1.));
#39401=DIRECTION('center_axis',(-0.184386631340398,0.982853788812426,-1.65306157129174E-48));
#39402=DIRECTION('ref_axis',(-0.982853788812426,-0.184386631340398,3.00112067034686E-65));
#39403=DIRECTION('center_axis',(-0.670755141630903,-0.741678865800898,3.95502882331426E-49));
#39404=DIRECTION('ref_axis',(0.741678865800898,-0.670755141630903,1.84878394507284E-65));
#39405=DIRECTION('',(-1.12975568624751E-48,1.55497530110059E-48,1.));
#39406=DIRECTION('center_axis',(-1.12975568624751E-48,1.55497530110059E-48,
1.));
#39407=DIRECTION('ref_axis',(4.33680868994202E-19,-1.,1.55497530110059E-48));
#39408=DIRECTION('',(-1.12975568624751E-48,1.55497530110059E-48,1.));
#39409=DIRECTION('center_axis',(-0.106704409388993,0.994290786951657,-1.66664752907659E-48));
#39410=DIRECTION('ref_axis',(-0.994290786951658,-0.106704409388993,-2.84767254643969E-65));
#39411=DIRECTION('center_axis',(-0.726878880513659,-0.686765675513279,3.30271754722836E-49));
#39412=DIRECTION('ref_axis',(0.686765675513279,-0.726878880513659,1.35737227185702E-66));
#39413=DIRECTION('',(-1.09747227149895E-48,1.64248332589092E-48,1.));
#39414=DIRECTION('center_axis',(-1.09747227149895E-48,1.64248332589092E-48,
1.));
#39415=DIRECTION('ref_axis',(4.33680868994202E-19,-1.,1.64248332589092E-48));
#39416=DIRECTION('',(-1.09747227149895E-48,1.64248332589092E-48,1.));
#39417=DIRECTION('center_axis',(-0.0283643192708891,0.999597651754094,-1.67295152950556E-48));
#39418=DIRECTION('ref_axis',(-0.999597651754094,-0.0283643192708891,-1.01926051780483E-65));
#39419=DIRECTION('center_axis',(-0.778521169386292,-0.627618346463358,2.60010913042463E-49));
#39420=DIRECTION('ref_axis',(0.627618346463358,-0.778521169386292,-1.77736454987801E-64));
#39421=DIRECTION('',(-1.05842257525003E-48,1.72718866511697E-48,1.));
#39422=DIRECTION('center_axis',(-1.05842257525003E-48,1.72718866511697E-48,
1.));
#39423=DIRECTION('ref_axis',(-0.891006524188322,0.453990499739636,-1.72718866511707E-48));
#39424=DIRECTION('',(-1.05842257525003E-48,1.72718866511697E-48,1.));
#39425=DIRECTION('center_axis',(0.050150646307614,0.998741664633517,-1.67193470631971E-48));
#39426=DIRECTION('ref_axis',(-0.998741664633517,0.050150646307614,1.52017605534737E-65));
#39427=DIRECTION('center_axis',(-0.8253636163651,-0.564601541603213,1.85153538743368E-49));
#39428=DIRECTION('ref_axis',(0.564601541603213,-0.8253636163651,-7.9609822926636E-66));
#39429=DIRECTION('',(-1.01284735186348E-48,1.80856908219503E-48,1.));
#39430=DIRECTION('center_axis',(-1.01284735186348E-48,1.80856908219503E-48,
1.));
#39431=DIRECTION('ref_axis',(-0.852640164354107,0.522498564715924,-1.808569082195E-48));
#39432=DIRECTION('',(-1.01284735186348E-48,1.80856908219503E-48,1.));
#39433=DIRECTION('center_axis',(0.128356416474848,0.991728103035169,-1.6636033285721E-48));
#39434=DIRECTION('ref_axis',(-0.991728103035169,0.128356416474848,-6.99057875847398E-66));
#39435=DIRECTION('center_axis',(-0.867117422187763,-0.498103780490019,1.06161152430708E-49));
#39436=DIRECTION('ref_axis',(0.498103780490019,-0.867117422187763,1.00088346227585E-65));
#39437=DIRECTION('',(-9.61027587746759E-49,1.88612283979207E-48,1.));
#39438=DIRECTION('center_axis',(-9.61027587746759E-49,1.88612283979207E-48,
1.));
#39439=DIRECTION('ref_axis',(-0.809016994374894,0.587785252292546,-1.88612283979215E-48));
#39440=DIRECTION('',(-9.61027587746759E-49,1.88612283979207E-48,1.));
#39441=DIRECTION('center_axis',(0.205770826651675,0.978600207898551,-1.64800876197701E-48));
#39442=DIRECTION('ref_axis',(-0.978600207898551,0.205770826651675,2.0991990898783E-65));
#39443=DIRECTION('center_axis',(-0.903525160756836,-0.428535043933789,2.35207684337335E-50));
#39444=DIRECTION('ref_axis',(0.428535043933789,-0.903525160756836,-9.18347163738211E-68));
#39445=DIRECTION('',(-9.03282768977482E-49,1.95937179320328E-48,1.));
#39446=DIRECTION('center_axis',(-9.03282768977482E-49,1.95937179320328E-48,
1.));
#39447=DIRECTION('ref_axis',(-0.760405965599999,0.649448048330221,-1.95937179320332E-48));
#39448=DIRECTION('',(-9.03282768977482E-49,1.95937179320328E-48,1.));
#39449=DIRECTION('center_axis',(0.281916591256451,0.959438917062646,-1.62524715222323E-48));
#39450=DIRECTION('ref_axis',(-0.959438917062646,0.281916591256451,8.99283719863503E-66));
#39451=DIRECTION('center_axis',(-0.934362366257238,-0.356324246329344,-6.22581077994971E-50));
#39452=DIRECTION('ref_axis',(0.356324246329344,-0.934362366257238,-2.14283631075808E-67));
#39453=DIRECTION('',(-8.39968911565457E-49,2.02786433827311E-48,1.));
#39454=DIRECTION('center_axis',(-8.39968911565457E-49,2.02786433827311E-48,
1.));
#39455=DIRECTION('ref_axis',(-0.707106781186559,0.707106781186536,-2.02786433827309E-48));
#39456=DIRECTION('',(-8.39968911565457E-49,2.02786433827311E-48,1.));
#39457=DIRECTION('center_axis',(0.356324246329351,0.934362366257235,-1.59545883220388E-48));
#39458=DIRECTION('ref_axis',(-0.934362366257235,0.356324246329351,6.60900149289003E-65));
#39459=DIRECTION('center_axis',(-0.959438917062648,-0.281916591256444,-1.50646620972636E-49));
#39460=DIRECTION('ref_axis',(0.281916591256444,-0.959438917062648,3.84808191287826E-66));
#39461=DIRECTION('',(-7.71476366495624E-49,2.09117819568513E-48,1.));
#39462=DIRECTION('center_axis',(-7.71476366495624E-49,2.09117819568513E-48,
1.));
#39463=DIRECTION('ref_axis',(-0.649448048330135,0.760405965600073,-2.09117819568518E-48));
#39464=DIRECTION('',(-7.71476366495624E-49,2.09117819568513E-48,1.));
#39465=DIRECTION('center_axis',(0.428535043933796,0.903525160756832,-1.5588274568175E-48));
#39466=DIRECTION('ref_axis',(-0.903525160756832,0.428535043933796,-3.10862492143316E-66));
#39467=DIRECTION('center_axis',(-0.978600207898552,-0.205770826651667,-2.41099826509806E-49));
#39468=DIRECTION('ref_axis',(0.205770826651667,-0.978600207898552,1.22158844253494E-66));
#39469=DIRECTION('',(-6.98227413084421E-49,2.14892301445441E-48,1.));
#39470=DIRECTION('center_axis',(-6.98227413084421E-49,2.14892301445441E-48,
1.));
#39471=DIRECTION('ref_axis',(-0.587785252292501,0.809016994374927,-2.14892301445438E-48));
#39472=DIRECTION('',(-6.98227413084421E-49,2.14892301445441E-48,1.));
#39473=DIRECTION('center_axis',(0.498103780490025,0.867117422187759,-1.51557887067454E-48));
#39474=DIRECTION('ref_axis',(-0.867117422187759,0.498103780490025,2.99504754920617E-65));
#39475=DIRECTION('center_axis',(-0.99172810303517,-0.128356416474841,-3.33060050320128E-49));
#39476=DIRECTION('ref_axis',(0.128356416474841,-0.99172810303517,-3.10963647347836E-66));
#39477=DIRECTION('',(-6.20673655487377E-49,2.20074277857113E-48,1.));
#39478=DIRECTION('center_axis',(-6.20673655487377E-49,2.20074277857113E-48,
1.));
#39479=DIRECTION('ref_axis',(-0.522498564715884,0.852640164354132,-2.20074277857117E-48));
#39480=DIRECTION('',(-6.20673655487377E-49,2.20074277857113E-48,1.));
#39481=DIRECTION('center_axis',(0.564601541603219,0.825363616365096,-1.46597971569015E-48));
#39482=DIRECTION('ref_axis',(-0.825363616365096,0.564601541603219,-1.28895308917342E-64));
#39483=DIRECTION('center_axis',(-0.998741664633517,-0.0501506463076061,
-4.25960327043935E-49));
#39484=DIRECTION('ref_axis',(0.0501506463076061,-0.998741664633517,-2.80568036684895E-66));
#39485=DIRECTION('',(-5.39293238409318E-49,2.24631800195768E-48,1.));
#39486=DIRECTION('center_axis',(-5.39293238409318E-49,2.24631800195768E-48,
1.));
#39487=DIRECTION('ref_axis',(-0.453990499739489,0.891006524188397,-2.24631800195771E-48));
#39488=DIRECTION('',(-5.39293238409318E-49,2.24631800195768E-48,1.));
#39489=DIRECTION('center_axis',(0.627618346463364,0.778521169386287,-1.41033578714823E-48));
#39490=DIRECTION('ref_axis',(-0.778521169386288,0.627618346463364,5.07659402759256E-65));
#39491=DIRECTION('center_axis',(-0.999597651754094,0.0283643192708965,-5.19227895582746E-49));
#39492=DIRECTION('ref_axis',(-0.0283643192708965,-0.999597651754094,2.50391620144835E-67));
#39493=DIRECTION('',(-4.54587899183267E-49,2.2853676982066E-48,1.));
#39494=DIRECTION('center_axis',(-4.54587899183267E-49,2.2853676982066E-48,
1.));
#39495=DIRECTION('ref_axis',(-0.382683432365006,0.923879532511321,-2.28536769820664E-48));
#39496=DIRECTION('',(-4.54587899183267E-49,2.2853676982066E-48,1.));
#39497=DIRECTION('center_axis',(0.686765675513284,0.726878880513654,-1.34899014837172E-48));
#39498=DIRECTION('ref_axis',(-0.726878880513654,0.686765675513284,4.51664321804638E-65));
#39499=DIRECTION('center_axis',(-0.994290786951657,0.106704409389001,-6.12287730361908E-49));
#39500=DIRECTION('ref_axis',(-0.106704409389001,-0.994290786951657,-3.36897451344462E-66));
#39501=DIRECTION('',(-3.67079874392934E-49,2.31765111295516E-48,1.));
#39502=DIRECTION('center_axis',(-3.67079874392934E-49,2.31765111295516E-48,
1.));
#39503=DIRECTION('ref_axis',(-0.309016994374936,0.951056516295157,-2.31765111295516E-48));
#39504=DIRECTION('',(-3.67079874392934E-49,2.31765111295516E-48,1.));
#39505=DIRECTION('center_axis',(0.741678865800904,0.670755141630897,-1.28232101562316E-48));
#39506=DIRECTION('ref_axis',(-0.670755141630897,0.741678865800904,-7.13448931820408E-65));
#39507=DIRECTION('center_axis',(-0.982853788812424,0.184386631340406,-7.04566086554469E-49));
#39508=DIRECTION('ref_axis',(-0.184386631340406,-0.982853788812424,1.03257498418151E-65));
#39509=DIRECTION('',(-2.77308680110524E-49,2.34296920821612E-48,1.));
#39510=DIRECTION('center_axis',(-2.77308680110524E-49,2.34296920821612E-48,
1.));
#39511=DIRECTION('ref_axis',(-0.233445363855831,0.972369920397695,-2.34296920821614E-48));
#39512=DIRECTION('',(-2.77308680110524E-49,2.34296920821612E-48,1.));
#39513=DIRECTION('center_axis',(0.79201935924761,0.610495974251268,-1.21073942627568E-48));
#39514=DIRECTION('ref_axis',(-0.610495974251268,0.79201935924761,-4.36775682720849E-65));
#39515=DIRECTION('center_axis',(-0.965357170233113,0.260932048394819,-7.95494037408836E-49));
#39516=DIRECTION('ref_axis',(-0.260932048394819,-0.965357170233113,-3.47978634051958E-65));
#39517=DIRECTION('',(-1.85827785600739E-49,2.36116588951307E-48,1.));
#39518=DIRECTION('center_axis',(-1.85827785600739E-49,2.36116588951307E-48,
1.));
#39519=DIRECTION('ref_axis',(-0.156434465040246,0.987688340595135,-2.36116588951307E-48));
#39520=DIRECTION('',(-1.85827785600739E-49,2.36116588951307E-48,1.));
#39521=DIRECTION('center_axis',(0.837476789971392,0.546472896179868,-1.13468670463092E-48));
#39522=DIRECTION('ref_axis',(-0.546472896179868,0.837476789971392,7.35185048458512E-65));
#39523=DIRECTION('center_axis',(-0.94190880368548,0.335868732602169,-8.84510981871381E-49));
#39524=DIRECTION('ref_axis',(-0.335868732602169,-0.94190880368548,-2.80378683690505E-64));
#39525=DIRECTION('',(-9.32012009987159E-50,2.3721289682548E-48,1.));
#39526=DIRECTION('center_axis',(-9.32012009987159E-50,2.3721289682548E-48,
1.));
#39527=DIRECTION('ref_axis',(-0.0784590957277844,0.996917333733133,-2.3721289682548E-48));
#39528=DIRECTION('',(-9.32012009987159E-50,2.3721289682548E-48,1.));
#39529=DIRECTION('center_axis',(0.877770897795708,0.47908063098284,-1.0546317410079E-48));
#39530=DIRECTION('ref_axis',(-0.47908063098284,0.877770897795708,-1.46432166581228E-64));
#39531=DIRECTION('center_axis',(-0.912653256146669,0.408734674385332,-9.71068100878346E-49));
#39532=DIRECTION('ref_axis',(-0.408734674385332,-0.912653256146669,4.78015562106795E-65));
#39533=DIRECTION('',(-1.03033504185762E-66,2.37579085341529E-48,1.));
#39534=DIRECTION('center_axis',(-1.03033504185762E-66,2.37579085341529E-48,
1.));
#39535=DIRECTION('ref_axis',(-5.51899603821915E-14,1.,-2.37579085341529E-48));
#39536=DIRECTION('',(-1.03033504185762E-66,2.37579085341529E-48,1.));
#39537=DIRECTION('center_axis',(0.912653256146668,0.408734674385334,-9.71068100878352E-49));
#39538=DIRECTION('ref_axis',(-0.408734674385334,0.912653256146668,-3.97320112854764E-64));
#39539=DIRECTION('center_axis',(-0.877770897795703,0.47908063098285,-1.05463174100791E-48));
#39540=DIRECTION('ref_axis',(-0.47908063098285,-0.877770897795703,8.5181126283276E-66));
#39541=DIRECTION('',(9.32012009987329E-50,2.3721289682548E-48,1.));
#39542=DIRECTION('center_axis',(9.32012009987329E-50,2.3721289682548E-48,
1.));
#39543=DIRECTION('ref_axis',(0.078459095727909,0.996917333733123,-2.37212896825479E-48));
#39544=DIRECTION('',(9.32012009987329E-50,2.3721289682548E-48,1.));
#39545=DIRECTION('center_axis',(0.941908803685484,0.335868732602158,-8.84510981871371E-49));
#39546=DIRECTION('ref_axis',(-0.335868732602158,0.941908803685484,-1.44601818635795E-65));
#39547=DIRECTION('center_axis',(-0.837476789971386,0.546472896179877,-1.13468670463093E-48));
#39548=DIRECTION('ref_axis',(-0.546472896179877,-0.837476789971386,1.1507371701338E-64));
#39549=DIRECTION('',(1.85827785600756E-49,2.36116588951307E-48,1.));
#39550=DIRECTION('center_axis',(1.85827785600756E-49,2.36116588951307E-48,
1.));
#39551=DIRECTION('ref_axis',(0.156434465040226,0.987688340595138,-2.36116588951307E-48));
#39552=DIRECTION('',(1.85827785600756E-49,2.36116588951307E-48,1.));
#39553=DIRECTION('center_axis',(0.965357170233116,0.260932048394809,-7.95494037408827E-49));
#39554=DIRECTION('ref_axis',(-0.260932048394809,0.965357170233116,-4.20694512990981E-65));
#39555=DIRECTION('center_axis',(-0.792019359247603,0.610495974251277,-1.21073942627569E-48));
#39556=DIRECTION('ref_axis',(-0.610495974251277,-0.792019359247603,-2.13945998802071E-65));
#39557=DIRECTION('',(2.7730868011054E-49,2.34296920821612E-48,1.));
#39558=DIRECTION('center_axis',(2.7730868011054E-49,2.34296920821612E-48,
1.));
#39559=DIRECTION('ref_axis',(0.233445363855898,0.972369920397678,-2.34296920821612E-48));
#39560=DIRECTION('',(2.7730868011054E-49,2.34296920821612E-48,1.));
#39561=DIRECTION('center_axis',(0.982853788812426,0.184386631340395,-7.04566086554459E-49));
#39562=DIRECTION('ref_axis',(-0.184386631340395,0.982853788812426,-1.76256118611904E-65));
#39563=DIRECTION('center_axis',(-0.741678865800896,0.670755141630906,-1.28232101562316E-48));
#39564=DIRECTION('ref_axis',(-0.670755141630906,-0.741678865800896,1.75561258236883E-65));
#39565=DIRECTION('',(3.6707987439295E-49,2.31765111295516E-48,1.));
#39566=DIRECTION('center_axis',(3.6707987439295E-49,2.31765111295516E-48,
1.));
#39567=DIRECTION('ref_axis',(0.309016994374949,0.951056516295153,-2.31765111295516E-48));
#39568=DIRECTION('',(3.6707987439295E-49,2.31765111295516E-48,1.));
#39569=DIRECTION('center_axis',(0.994290786951658,0.10670440938899,-6.12287730361897E-49));
#39570=DIRECTION('ref_axis',(-0.10670440938899,0.994290786951658,-7.83421067979577E-66));
#39571=DIRECTION('center_axis',(-0.686765675513276,0.726878880513661,-1.34899014837172E-48));
#39572=DIRECTION('ref_axis',(-0.726878880513661,-0.686765675513276,5.3563970103269E-65));
#39573=DIRECTION('',(4.54587899183282E-49,2.28536769820659E-48,1.));
#39574=DIRECTION('center_axis',(4.54587899183282E-49,2.28536769820659E-48,
1.));
#39575=DIRECTION('ref_axis',(0.382683432365024,0.923879532511314,-2.28536769820663E-48));
#39576=DIRECTION('',(4.54587899183282E-49,2.28536769820659E-48,1.));
#39577=DIRECTION('center_axis',(0.999597651754094,0.0283643192708856,-5.19227895582736E-49));
#39578=DIRECTION('ref_axis',(-0.0283643192708856,0.999597651754094,1.94568536261846E-66));
#39579=DIRECTION('center_axis',(-0.627618346463355,0.778521169386295,-1.41033578714824E-48));
#39580=DIRECTION('ref_axis',(-0.778521169386295,-0.627618346463355,-4.32781502974933E-65));
#39581=DIRECTION('',(5.39293238409334E-49,2.24631800195767E-48,1.));
#39582=DIRECTION('center_axis',(5.39293238409334E-49,2.24631800195767E-48,
1.));
#39583=DIRECTION('ref_axis',(0.45399049973962,0.89100652418833,-2.24631800195763E-48));
#39584=DIRECTION('',(5.39293238409334E-49,2.24631800195767E-48,1.));
#39585=DIRECTION('center_axis',(0.998741664633517,-0.0501506463076175,-4.25960327043925E-49));
#39586=DIRECTION('ref_axis',(0.0501506463076175,0.998741664633517,-4.14088422014228E-66));
#39587=DIRECTION('center_axis',(-0.56460154160321,0.825363616365102,-1.46597971569016E-48));
#39588=DIRECTION('ref_axis',(-0.825363616365102,-0.56460154160321,7.97777118454868E-65));
#39589=DIRECTION('',(6.20673655487391E-49,2.20074277857112E-48,1.));
#39590=DIRECTION('center_axis',(6.20673655487391E-49,2.20074277857112E-48,
1.));
#39591=DIRECTION('ref_axis',(0.522498564715976,0.852640164354076,-2.20074277857111E-48));
#39592=DIRECTION('',(6.20673655487391E-49,2.20074277857112E-48,1.));
#39593=DIRECTION('center_axis',(0.991728103035169,-0.128356416474851,-3.33060050320119E-49));
#39594=DIRECTION('ref_axis',(0.128356416474851,0.991728103035169,2.08257490756294E-67));
#39595=DIRECTION('center_axis',(-0.498103780490015,0.867117422187765,-1.51557887067454E-48));
#39596=DIRECTION('ref_axis',(-0.867117422187765,-0.498103780490015,2.18779707200991E-65));
#39597=DIRECTION('',(6.98227413084436E-49,2.1489230144544E-48,1.));
#39598=DIRECTION('center_axis',(6.98227413084435E-49,2.1489230144544E-48,
1.));
#39599=DIRECTION('ref_axis',(0.587785252292489,0.809016994374936,-2.14892301445439E-48));
#39600=DIRECTION('',(6.98227413084436E-49,2.1489230144544E-48,1.));
#39601=DIRECTION('center_axis',(0.97860020789855,-0.205770826651679,-2.41099826509796E-49));
#39602=DIRECTION('ref_axis',(0.205770826651679,0.97860020789855,-2.74077973100627E-66));
#39603=DIRECTION('center_axis',(-0.428535043933785,0.903525160756837,-1.55882745681751E-48));
#39604=DIRECTION('ref_axis',(-0.903525160756837,-0.428535043933785,-8.73188639847288E-65));
#39605=DIRECTION('',(7.71476366495637E-49,2.09117819568512E-48,1.));
#39606=DIRECTION('center_axis',(7.71476366495637E-49,2.09117819568512E-48,
1.));
#39607=DIRECTION('ref_axis',(0.649448048330186,0.760405965600029,-2.09117819568512E-48));
#39608=DIRECTION('',(7.71476366495637E-49,2.09117819568512E-48,1.));
#39609=DIRECTION('center_axis',(0.959438917062645,-0.281916591256455,-1.50646620972626E-49));
#39610=DIRECTION('ref_axis',(0.281916591256455,0.959438917062645,-2.91844467010393E-67));
#39611=DIRECTION('center_axis',(-0.356324246329341,0.934362366257239,-1.59545883220388E-48));
#39612=DIRECTION('ref_axis',(-0.934362366257239,-0.356324246329341,1.49301625507406E-64));
#39613=DIRECTION('',(8.39968911565469E-49,2.0278643382731E-48,1.));
#39614=DIRECTION('center_axis',(8.39968911565469E-49,2.0278643382731E-48,
1.));
#39615=DIRECTION('ref_axis',(0.707106781186573,0.707106781186522,-2.02786433827308E-48));
#39616=DIRECTION('',(8.39968911565469E-49,2.0278643382731E-48,1.));
#39617=DIRECTION('center_axis',(0.934362366257234,-0.356324246329355,-6.22581077994883E-50));
#39618=DIRECTION('ref_axis',(0.356324246329355,0.934362366257234,-4.97582464336991E-66));
#39619=DIRECTION('center_axis',(-0.28191659125644,0.959438917062649,-1.62524715222323E-48));
#39620=DIRECTION('ref_axis',(-0.959438917062649,-0.28191659125644,-5.29515836320384E-66));
#39621=DIRECTION('',(9.03282768977493E-49,1.95937179320326E-48,1.));
#39622=DIRECTION('center_axis',(9.03282768977493E-49,1.95937179320326E-48,
1.));
#39623=DIRECTION('ref_axis',(0.760405965600079,0.649448048330127,-1.9593717932032E-48));
#39624=DIRECTION('',(9.03282768977493E-49,1.95937179320326E-48,1.));
#39625=DIRECTION('center_axis',(0.903525160756831,-0.428535043933799,2.35207684337425E-50));
#39626=DIRECTION('ref_axis',(0.428535043933799,0.903525160756831,3.46790681006673E-67));
#39627=DIRECTION('center_axis',(-0.205770826651664,0.978600207898553,-1.64800876197701E-48));
#39628=DIRECTION('ref_axis',(-0.978600207898553,-0.205770826651664,-5.70930081633759E-65));
#39629=DIRECTION('',(9.61027587746769E-49,1.88612283979206E-48,1.));
#39630=DIRECTION('center_axis',(9.61027587746769E-49,1.88612283979206E-48,
1.));
#39631=DIRECTION('ref_axis',(0.809016994374978,0.587785252292432,-1.88612283979202E-48));
#39632=DIRECTION('',(9.61027587746769E-49,1.88612283979206E-48,1.));
#39633=DIRECTION('center_axis',(0.867117422187757,-0.498103780490029,1.06161152430717E-49));
#39634=DIRECTION('ref_axis',(0.498103780490029,0.867117422187757,8.6756046158998E-66));
#39635=DIRECTION('center_axis',(-0.128356416474837,0.991728103035171,-1.6636033285721E-48));
#39636=DIRECTION('ref_axis',(-0.991728103035171,-0.128356416474837,3.98742758462882E-65));
#39637=DIRECTION('',(1.01284735186348E-48,1.80856908219502E-48,1.));
#39638=DIRECTION('center_axis',(1.01284735186348E-48,1.80856908219502E-48,
1.));
#39639=DIRECTION('ref_axis',(0.852640164354111,0.522498564715918,-1.80856908219499E-48));
#39640=DIRECTION('',(1.01284735186348E-48,1.80856908219502E-48,1.));
#39641=DIRECTION('center_axis',(0.825363616365094,-0.564601541603222,1.85153538743376E-49));
#39642=DIRECTION('ref_axis',(0.564601541603222,0.825363616365094,-1.20460226317478E-65));
#39643=DIRECTION('center_axis',(-0.0501506463076026,0.998741664633518,-1.67193470631971E-48));
#39644=DIRECTION('ref_axis',(-0.998741664633518,-0.0501506463076026,9.17993822873344E-66));
#39645=DIRECTION('',(1.05842257525004E-48,1.72718866511696E-48,1.));
#39646=DIRECTION('center_axis',(1.05842257525004E-48,1.72718866511696E-48,
1.));
#39647=DIRECTION('ref_axis',(0.891006524188331,0.453990499739619,-1.72718866511705E-48));
#39648=DIRECTION('',(1.05842257525004E-48,1.72718866511696E-48,1.));
#39649=DIRECTION('center_axis',(0.778521169386285,-0.627618346463367,2.6001091304247E-49));
#39650=DIRECTION('ref_axis',(0.627618346463367,0.778521169386285,-2.38387219843189E-65));
#39651=DIRECTION('center_axis',(0.0283643192709005,0.999597651754094,-1.67295152950556E-48));
#39652=DIRECTION('ref_axis',(-0.999597651754094,0.0283643192709005,5.71503284305285E-66));
#39653=DIRECTION('',(1.09747227149896E-48,1.6424833258909E-48,1.));
#39654=DIRECTION('center_axis',(1.09747227149896E-48,1.6424833258909E-48,
1.));
#39655=DIRECTION('ref_axis',(4.33680868994202E-19,-1.,1.6424833258909E-48));
#39656=DIRECTION('',(1.09747227149896E-48,1.6424833258909E-48,1.));
#39657=DIRECTION('center_axis',(0.726878880513651,-0.686765675513287,3.30271754722842E-49));
#39658=DIRECTION('ref_axis',(0.686765675513287,0.726878880513651,-2.02185804836064E-65));
#39659=DIRECTION('center_axis',(0.106704409389004,0.994290786951656,-1.66664752907659E-48));
#39660=DIRECTION('ref_axis',(-0.994290786951656,0.106704409389004,-7.60908949083185E-66));
#39661=DIRECTION('',(1.12975568624752E-48,1.55497530110057E-48,1.));
#39662=DIRECTION('center_axis',(1.12975568624752E-48,1.55497530110057E-48,
1.));
#39663=DIRECTION('ref_axis',(4.33680868994202E-19,-1.,1.55497530110057E-48));
#39664=DIRECTION('',(1.12975568624752E-48,1.55497530110057E-48,1.));
#39665=DIRECTION('center_axis',(0.670755141630895,-0.741678865800906,3.95502882331431E-49));
#39666=DIRECTION('ref_axis',(0.741678865800906,0.670755141630895,-5.99583083400171E-67));
#39667=DIRECTION('center_axis',(0.184386631340409,0.982853788812424,-1.65306157129173E-48));
#39668=DIRECTION('ref_axis',(-0.982853788812424,0.184386631340409,2.90870213757036E-65));
#39669=DIRECTION('',(1.15507378150848E-48,1.46520410681816E-48,1.));
#39670=DIRECTION('center_axis',(1.15507378150848E-48,1.46520410681816E-48,
1.));
#39671=DIRECTION('ref_axis',(4.33680868994202E-19,-1.,1.46520410681816E-48));
#39672=DIRECTION('',(1.15507378150848E-48,1.46520410681816E-48,1.));
#39673=DIRECTION('center_axis',(0.610495974251266,-0.792019359247612,4.5530212427498E-49));
#39674=DIRECTION('ref_axis',(0.792019359247612,0.610495974251266,2.91962028883906E-65));
#39675=DIRECTION('center_axis',(0.260932048394823,0.965357170233112,-1.63227741809852E-48));
#39676=DIRECTION('ref_axis',(-0.965357170233112,0.260932048394823,3.06323067308603E-65));
#39677=DIRECTION('',(1.17327046280543E-48,1.37372321230838E-48,1.));
#39678=DIRECTION('center_axis',(1.17327046280543E-48,1.37372321230838E-48,
1.));
#39679=DIRECTION('ref_axis',(4.33680868994202E-19,-1.,1.37372321230838E-48));
#39680=DIRECTION('',(1.17327046280543E-48,1.37372321230838E-48,1.));
#39681=DIRECTION('center_axis',(0.546472896179865,-0.837476789971394,5.0930079834164E-49));
#39682=DIRECTION('ref_axis',(0.837476789971394,0.546472896179865,-4.56422939014991E-65));
#39683=DIRECTION('center_axis',(0.335868732602171,0.94190880368548,-1.60442321071282E-48));
#39684=DIRECTION('ref_axis',(-0.94190880368548,0.335868732602171,4.87630450545203E-65));
#39685=DIRECTION('',(1.18423354154716E-48,1.28109662770635E-48,1.));
#39686=DIRECTION('center_axis',(1.18423354154716E-48,1.28109662770635E-48,
1.));
#39687=DIRECTION('ref_axis',(4.33680868994202E-19,-1.,1.28109662770635E-48));
#39688=DIRECTION('',(1.18423354154716E-48,1.28109662770635E-48,1.));
#39689=DIRECTION('center_axis',(0.479080630982838,-0.87777089779571,5.57165984749409E-49));
#39690=DIRECTION('ref_axis',(0.87777089779571,0.479080630982838,-3.73128804317402E-67));
#39691=DIRECTION('center_axis',(0.408734674385341,0.912653256146664,-1.56967067958563E-48));
#39692=DIRECTION('ref_axis',(-0.912653256146664,0.408734674385341,1.45818743306131E-64));
#39693=DIRECTION('center_axis',(0.408734674385325,-0.912653256146672,5.98602578707294E-49));
#39694=DIRECTION('ref_axis',(0.912653256146672,0.408734674385325,1.90174553100142E-65));
#39695=DIRECTION('center_axis',(0.479080630982853,0.877770897795701,-1.52823408562775E-48));
#39696=DIRECTION('ref_axis',(-0.877770897795701,0.479080630982853,5.61428358120402E-65));
#39697=DIRECTION('center_axis',(0.335868732602155,-0.941908803685485,6.33355109834479E-49));
#39698=DIRECTION('ref_axis',(0.941908803685485,0.335868732602155,-2.18452554190007E-64));
#39699=DIRECTION('center_axis',(0.54647289617988,0.837476789971384,-1.48036889921998E-48));
#39700=DIRECTION('ref_axis',(-0.837476789971384,0.54647289617988,1.0038841655118E-64));
#39701=DIRECTION('center_axis',(0.260932048394805,-0.965357170233117,6.61209317220175E-49));
#39702=DIRECTION('ref_axis',(0.965357170233117,0.260932048394805,-1.34731391844263E-65));
#39703=DIRECTION('center_axis',(0.61049597425128,0.792019359247601,-1.42637022515332E-48));
#39704=DIRECTION('ref_axis',(-0.792019359247601,0.61049597425128,4.68595517840464E-65));
#39705=DIRECTION('center_axis',(0.184386631340391,-0.982853788812427,6.81993470413385E-49));
#39706=DIRECTION('ref_axis',(0.982853788812427,0.184386631340391,-4.82159387328582E-66));
#39707=DIRECTION('center_axis',(0.670755141630908,0.741678865800894,-1.36657098320977E-48));
#39708=DIRECTION('ref_axis',(-0.741678865800894,0.670755141630908,-1.20021806126158E-65));
#39709=DIRECTION('center_axis',(0.106704409388986,-0.994290786951658,6.95579428198241E-49));
#39710=DIRECTION('ref_axis',(0.994290786951658,0.106704409388986,-5.2899598259714E-66));
#39711=DIRECTION('center_axis',(0.726878880513664,0.686765675513273,-1.30133985560118E-48));
#39712=DIRECTION('ref_axis',(-0.686765675513273,0.726878880513664,8.56568901676031E-65));
#39713=DIRECTION('center_axis',(0.0283643192708817,-0.999597651754094,7.01883428627211E-49));
#39714=DIRECTION('ref_axis',(0.999597651754094,0.0283643192708817,4.29698701010715E-68));
#39715=DIRECTION('axis',(0.,0.,1.));
#39716=DIRECTION('refdir',(1.,0.,0.));
#39717=DIRECTION('center_axis',(5.15167520928809E-67,-1.18789542670764E-48,
-1.));
#39718=DIRECTION('ref_axis',(-4.33680868994202E-19,1.,-1.18789542670764E-48));
#39719=DIRECTION('',(-5.15167520928809E-67,1.18789542670764E-48,1.));
#39720=DIRECTION('',(-5.15167520928809E-67,1.18789542670764E-48,1.));
#39721=DIRECTION('center_axis',(5.15167520928809E-67,-1.18789542670764E-48,
-1.));
#39722=DIRECTION('ref_axis',(-4.33680868994202E-19,1.,-1.18789542670764E-48));
#39723=DIRECTION('center_axis',(-4.70261923768679E-35,1.08435016942139E-16,
-1.));
#39724=DIRECTION('ref_axis',(-4.33680868994202E-19,1.,1.08435016942139E-16));
#39725=DIRECTION('center_axis',(5.15167520928809E-67,-1.18789542670764E-48,
-1.));
#39726=DIRECTION('ref_axis',(-4.33680868994202E-19,1.,-1.18789542670764E-48));
#39727=DIRECTION('',(-5.15167520928809E-67,1.18789542670764E-48,1.));
#39728=DIRECTION('center_axis',(5.15167520928809E-67,-1.18789542670764E-48,
-1.));
#39729=DIRECTION('ref_axis',(-4.33680868994202E-19,1.,-1.18789542670764E-48));
#39730=DIRECTION('',(-5.15167520928809E-67,1.18789542670764E-48,1.));
#39731=DIRECTION('center_axis',(5.15167520928809E-67,-1.18789542670764E-48,
-1.));
#39732=DIRECTION('ref_axis',(-4.33680868994202E-19,1.,-1.18789542670764E-48));
#39733=DIRECTION('',(-5.15167520928809E-67,1.18789542670764E-48,1.));
#39734=DIRECTION('center_axis',(5.15167520928809E-67,-1.18789542670764E-48,
-1.));
#39735=DIRECTION('ref_axis',(-4.33680868994202E-19,1.,-1.18789542670764E-48));
#39736=DIRECTION('',(-5.15167520928809E-67,1.18789542670764E-48,1.));
#39737=DIRECTION('center_axis',(5.15167520928809E-67,-1.18789542670764E-48,
-1.));
#39738=DIRECTION('ref_axis',(-4.33680868994202E-19,1.,-1.18789542670764E-48));
#39739=DIRECTION('',(-5.15167520928809E-67,1.18789542670764E-48,1.));
#39740=DIRECTION('center_axis',(5.15167520928809E-67,-1.18789542670764E-48,
-1.));
#39741=DIRECTION('ref_axis',(-4.33680868994202E-19,1.,-1.18789542670764E-48));
#39742=DIRECTION('',(-5.15167520928809E-67,1.18789542670764E-48,1.));
#39743=DIRECTION('center_axis',(5.15167520928809E-67,-1.18789542670764E-48,
-1.));
#39744=DIRECTION('ref_axis',(-4.33680868994202E-19,1.,-1.18789542670764E-48));
#39745=DIRECTION('',(-5.15167520928809E-67,1.18789542670764E-48,1.));
#39746=DIRECTION('center_axis',(5.15167520928809E-67,-1.18789542670764E-48,
-1.));
#39747=DIRECTION('ref_axis',(-4.33680868994202E-19,1.,-1.18789542670764E-48));
#39748=DIRECTION('',(-5.15167520928809E-67,1.18789542670764E-48,1.));
#39749=DIRECTION('center_axis',(5.15167520928809E-67,-1.18789542670764E-48,
-1.));
#39750=DIRECTION('ref_axis',(-4.33680868994202E-19,1.,-1.18789542670764E-48));
#39751=DIRECTION('',(-5.15167520928809E-67,1.18789542670764E-48,1.));
#39752=DIRECTION('center_axis',(5.15167520928809E-67,-1.18789542670764E-48,
-1.));
#39753=DIRECTION('ref_axis',(-4.33680868994202E-19,1.,-1.18789542670764E-48));
#39754=DIRECTION('',(-5.15167520928809E-67,1.18789542670764E-48,1.));
#39755=DIRECTION('center_axis',(5.15167520928809E-67,-1.18789542670764E-48,
-1.));
#39756=DIRECTION('ref_axis',(-4.33680868994202E-19,1.,-1.18789542670764E-48));
#39757=DIRECTION('',(-5.15167520928809E-67,1.18789542670764E-48,1.));
#39758=DIRECTION('center_axis',(5.15167520928809E-67,-1.18789542670764E-48,
-1.));
#39759=DIRECTION('ref_axis',(-4.33680868994202E-19,1.,-1.18789542670764E-48));
#39760=DIRECTION('',(-5.15167520928809E-67,1.18789542670764E-48,1.));
#39761=DIRECTION('center_axis',(5.15167520928809E-67,-1.18789542670764E-48,
-1.));
#39762=DIRECTION('ref_axis',(-4.33680868994202E-19,1.,-1.18789542670764E-48));
#39763=DIRECTION('',(-5.15167520928809E-67,1.18789542670764E-48,1.));
#39764=DIRECTION('center_axis',(5.15167520928809E-67,-1.18789542670764E-48,
-1.));
#39765=DIRECTION('ref_axis',(-4.33680868994202E-19,1.,-1.18789542670764E-48));
#39766=DIRECTION('',(-5.15167520928809E-67,1.18789542670764E-48,1.));
#39767=DIRECTION('center_axis',(5.15167520928809E-67,-1.18789542670764E-48,
-1.));
#39768=DIRECTION('ref_axis',(-4.33680868994202E-19,1.,-1.18789542670764E-48));
#39769=DIRECTION('',(-5.15167520928809E-67,1.18789542670764E-48,1.));
#39770=DIRECTION('center_axis',(5.15167520928809E-67,-1.18789542670764E-48,
-1.));
#39771=DIRECTION('ref_axis',(-4.33680868994202E-19,1.,-1.18789542670764E-48));
#39772=DIRECTION('',(-5.15167520928809E-67,1.18789542670764E-48,1.));
#39773=DIRECTION('center_axis',(5.15167520928809E-67,-1.18789542670764E-48,
-1.));
#39774=DIRECTION('ref_axis',(-4.33680868994202E-19,1.,-1.18789542670764E-48));
#39775=DIRECTION('',(-5.15167520928809E-67,1.18789542670764E-48,1.));
#39776=DIRECTION('center_axis',(5.15167520928809E-67,-1.18789542670764E-48,
-1.));
#39777=DIRECTION('ref_axis',(-4.33680868994202E-19,1.,-1.18789542670764E-48));
#39778=DIRECTION('',(-5.15167520928809E-67,1.18789542670764E-48,1.));
#39779=DIRECTION('center_axis',(5.15167520928809E-67,-1.18789542670764E-48,
-1.));
#39780=DIRECTION('ref_axis',(-4.33680868994202E-19,1.,-1.18789542670764E-48));
#39781=DIRECTION('',(-5.15167520928809E-67,1.18789542670764E-48,1.));
#39782=DIRECTION('center_axis',(5.15167520928809E-67,-1.18789542670764E-48,
-1.));
#39783=DIRECTION('ref_axis',(-4.33680868994202E-19,1.,-1.18789542670764E-48));
#39784=DIRECTION('',(-5.15167520928809E-67,1.18789542670764E-48,1.));
#39785=DIRECTION('center_axis',(5.15167520928809E-67,-1.18789542670764E-48,
-1.));
#39786=DIRECTION('ref_axis',(-4.33680868994202E-19,1.,-1.18789542670764E-48));
#39787=DIRECTION('',(-5.15167520928809E-67,1.18789542670764E-48,1.));
#39788=DIRECTION('center_axis',(5.15167520928809E-67,-1.18789542670764E-48,
-1.));
#39789=DIRECTION('ref_axis',(-4.33680868994202E-19,1.,-1.18789542670764E-48));
#39790=DIRECTION('',(-5.15167520928809E-67,1.18789542670764E-48,1.));
#39791=DIRECTION('center_axis',(5.15167520928809E-67,-1.18789542670764E-48,
-1.));
#39792=DIRECTION('ref_axis',(-4.33680868994202E-19,1.,-1.18789542670764E-48));
#39793=DIRECTION('',(-5.15167520928809E-67,1.18789542670764E-48,1.));
#39794=DIRECTION('center_axis',(5.15167520928809E-67,-1.18789542670764E-48,
-1.));
#39795=DIRECTION('ref_axis',(-4.33680868994202E-19,1.,-1.18789542670764E-48));
#39796=DIRECTION('',(-5.15167520928809E-67,1.18789542670764E-48,1.));
#39797=DIRECTION('center_axis',(5.15167520928809E-67,-1.18789542670764E-48,
-1.));
#39798=DIRECTION('ref_axis',(-4.33680868994202E-19,1.,-1.18789542670764E-48));
#39799=DIRECTION('',(-5.15167520928809E-67,1.18789542670764E-48,1.));
#39800=DIRECTION('center_axis',(5.15167520928809E-67,-1.18789542670764E-48,
-1.));
#39801=DIRECTION('ref_axis',(-4.33680868994202E-19,1.,-1.18789542670764E-48));
#39802=DIRECTION('',(-5.15167520928809E-67,1.18789542670764E-48,1.));
#39803=DIRECTION('center_axis',(5.15167520928809E-67,-1.18789542670764E-48,
-1.));
#39804=DIRECTION('ref_axis',(-4.33680868994202E-19,1.,-1.18789542670764E-48));
#39805=DIRECTION('',(-5.15167520928809E-67,1.18789542670764E-48,1.));
#39806=DIRECTION('center_axis',(-5.15167520928809E-67,1.18789542670764E-48,
1.));
#39807=DIRECTION('ref_axis',(4.33680868994202E-19,-1.,1.18789542670764E-48));
#39808=DIRECTION('',(8.69022643068855E-17,-0.707106781186544,-0.707106781186551));
#39809=DIRECTION('center_axis',(5.15167520928809E-67,-1.18789542670764E-48,
-1.));
#39810=DIRECTION('ref_axis',(-4.33680868994202E-19,1.,-1.18789542670764E-48));
#39811=DIRECTION('center_axis',(0.,0.,1.));
#39812=DIRECTION('ref_axis',(5.30947313395831E-16,1.,0.));
#39813=DIRECTION('',(0.,0.,-1.));
#39814=DIRECTION('center_axis',(5.15167520928809E-67,-1.18789542670764E-48,
-1.));
#39815=DIRECTION('ref_axis',(-4.33680868994202E-19,1.,-1.18789542670764E-48));
#39816=DIRECTION('center_axis',(0.,0.,1.));
#39817=DIRECTION('ref_axis',(5.30947313395831E-16,1.,0.));
#39818=DIRECTION('',(0.,0.,-1.));
#39819=DIRECTION('center_axis',(0.,0.,1.));
#39820=DIRECTION('ref_axis',(5.30947313395831E-16,1.,0.));
#39821=DIRECTION('',(0.,0.,-1.));
#39822=DIRECTION('center_axis',(0.,0.,1.));
#39823=DIRECTION('ref_axis',(5.30947313395831E-16,1.,0.));
#39824=DIRECTION('',(0.,0.,-1.));
#39825=DIRECTION('center_axis',(0.,0.,1.));
#39826=DIRECTION('ref_axis',(5.30947313395831E-16,1.,0.));
#39827=DIRECTION('',(0.,0.,-1.));
#39828=DIRECTION('center_axis',(0.,0.,1.));
#39829=DIRECTION('ref_axis',(5.30947313395831E-16,1.,0.));
#39830=DIRECTION('',(0.,0.,-1.));
#39831=DIRECTION('center_axis',(0.,0.,1.));
#39832=DIRECTION('ref_axis',(5.30947313395831E-16,1.,0.));
#39833=DIRECTION('',(0.,0.,-1.));
#39834=DIRECTION('center_axis',(0.,0.,1.));
#39835=DIRECTION('ref_axis',(5.30947313395831E-16,1.,0.));
#39836=DIRECTION('',(0.,0.,-1.));
#39837=DIRECTION('center_axis',(0.,0.,1.));
#39838=DIRECTION('ref_axis',(5.30947313395831E-16,1.,0.));
#39839=DIRECTION('',(0.,0.,-1.));
#39840=DIRECTION('center_axis',(0.,0.,1.));
#39841=DIRECTION('ref_axis',(5.30947313395831E-16,1.,0.));
#39842=DIRECTION('',(0.,0.,-1.));
#39843=DIRECTION('center_axis',(0.,0.,1.));
#39844=DIRECTION('ref_axis',(5.30947313395831E-16,1.,0.));
#39845=DIRECTION('',(0.,0.,-1.));
#39846=DIRECTION('center_axis',(0.,0.,1.));
#39847=DIRECTION('ref_axis',(5.30947313395831E-16,1.,0.));
#39848=DIRECTION('',(0.,0.,-1.));
#39849=DIRECTION('center_axis',(0.,0.,1.));
#39850=DIRECTION('ref_axis',(5.30947313395831E-16,1.,0.));
#39851=DIRECTION('',(0.,0.,-1.));
#39852=DIRECTION('center_axis',(0.,0.,1.));
#39853=DIRECTION('ref_axis',(5.30947313395831E-16,1.,0.));
#39854=DIRECTION('',(0.,0.,-1.));
#39855=DIRECTION('center_axis',(0.,0.,1.));
#39856=DIRECTION('ref_axis',(5.30947313395831E-16,1.,0.));
#39857=DIRECTION('',(0.,0.,-1.));
#39858=DIRECTION('center_axis',(0.,0.,1.));
#39859=DIRECTION('ref_axis',(5.30947313395831E-16,1.,0.));
#39860=DIRECTION('',(0.,0.,-1.));
#39861=DIRECTION('center_axis',(0.,0.,1.));
#39862=DIRECTION('ref_axis',(5.30947313395831E-16,1.,0.));
#39863=DIRECTION('',(0.,0.,-1.));
#39864=DIRECTION('center_axis',(0.,0.,1.));
#39865=DIRECTION('ref_axis',(5.30947313395831E-16,1.,0.));
#39866=DIRECTION('',(0.,0.,-1.));
#39867=DIRECTION('center_axis',(0.,0.,1.));
#39868=DIRECTION('ref_axis',(5.30947313395831E-16,1.,0.));
#39869=DIRECTION('',(0.,0.,-1.));
#39870=DIRECTION('center_axis',(0.,0.,1.));
#39871=DIRECTION('ref_axis',(5.30947313395831E-16,1.,0.));
#39872=DIRECTION('',(0.,0.,-1.));
#39873=DIRECTION('center_axis',(0.,0.,1.));
#39874=DIRECTION('ref_axis',(5.30947313395831E-16,1.,0.));
#39875=DIRECTION('',(0.,0.,-1.));
#39876=DIRECTION('center_axis',(0.,0.,1.));
#39877=DIRECTION('ref_axis',(5.30947313395831E-16,1.,0.));
#39878=DIRECTION('',(0.,0.,-1.));
#39879=DIRECTION('center_axis',(0.,0.,1.));
#39880=DIRECTION('ref_axis',(5.30947313395831E-16,1.,0.));
#39881=DIRECTION('',(0.,0.,-1.));
#39882=DIRECTION('center_axis',(0.,0.,1.));
#39883=DIRECTION('ref_axis',(5.30947313395831E-16,1.,0.));
#39884=DIRECTION('',(0.,0.,-1.));
#39885=DIRECTION('center_axis',(0.,0.,1.));
#39886=DIRECTION('ref_axis',(5.30947313395831E-16,1.,0.));
#39887=DIRECTION('',(0.,0.,-1.));
#39888=DIRECTION('center_axis',(0.,0.,1.));
#39889=DIRECTION('ref_axis',(5.30947313395831E-16,1.,0.));
#39890=DIRECTION('',(0.,0.,-1.));
#39891=DIRECTION('center_axis',(0.,0.,1.));
#39892=DIRECTION('ref_axis',(5.30947313395831E-16,1.,0.));
#39893=DIRECTION('',(0.,0.,-1.));
#39894=DIRECTION('center_axis',(0.,0.,1.));
#39895=DIRECTION('ref_axis',(5.30947313395831E-16,1.,0.));
#39896=DIRECTION('',(0.,0.,-1.));
#39897=DIRECTION('center_axis',(0.,0.,1.));
#39898=DIRECTION('ref_axis',(5.30947313395831E-16,1.,0.));
#39899=DIRECTION('',(0.,0.,-1.));
#39900=DIRECTION('center_axis',(0.,0.,1.));
#39901=DIRECTION('ref_axis',(5.30947313395831E-16,1.,0.));
#39902=DIRECTION('',(0.,0.,-1.));
#39903=DIRECTION('center_axis',(0.,0.,1.));
#39904=DIRECTION('ref_axis',(5.30947313395831E-16,1.,0.));
#39905=DIRECTION('center_axis',(0.,0.,1.));
#39906=DIRECTION('ref_axis',(0.700629269222058,-0.7135254915624,0.));
#39907=DIRECTION('center_axis',(-5.15167520928809E-67,1.18789542670764E-48,
1.));
#39908=DIRECTION('ref_axis',(4.33680868994202E-19,-1.,1.18789542670764E-48));
#39909=DIRECTION('center_axis',(5.15167520928809E-67,-1.18789542670764E-48,
-1.));
#39910=DIRECTION('ref_axis',(-4.33680868994202E-19,1.,-1.18789542670764E-48));
#39911=DIRECTION('center_axis',(5.15167520928809E-67,-1.18789542670764E-48,
-1.));
#39912=DIRECTION('ref_axis',(-4.33680868994202E-19,1.,-1.18789542670764E-48));
#39913=DIRECTION('center_axis',(5.15167520928809E-67,-1.18789542670764E-48,
-1.));
#39914=DIRECTION('ref_axis',(-4.33680868994202E-19,1.,-1.18789542670764E-48));
#39915=DIRECTION('center_axis',(1.09747227149895E-48,7.33307527524356E-49,
1.));
#39916=DIRECTION('ref_axis',(1.,4.33680868994202E-19,-1.09747227149895E-48));
#39917=DIRECTION('center_axis',(-0.654448706060852,0.271081529927754,-0.705841126081008));
#39918=DIRECTION('ref_axis',(0.652112169591586,-0.270113704831613,-0.708370174931649));
#39919=DIRECTION('',(1.09747227149895E-48,7.33307527524356E-49,1.));
#39920=DIRECTION('center_axis',(-0.654448706060939,0.271081529927973,0.705841126080843));
#39921=DIRECTION('ref_axis',(0.652112169592024,-0.270113704830126,0.708370174931813));
#39922=DIRECTION('',(1.09747227149895E-48,7.33307527524356E-49,1.));
#39923=DIRECTION('center_axis',(1.12975568624751E-48,8.20815552314688E-49,
1.));
#39924=DIRECTION('ref_axis',(1.,4.33680868994202E-19,-1.12975568624751E-48));
#39925=DIRECTION('center_axis',(-0.673700070814156,0.218898422362917,-0.705841126084352));
#39926=DIRECTION('ref_axis',(0.671294802430975,-0.218116903290839,-0.708370174928316));
#39927=DIRECTION('',(1.12975568624751E-48,8.20815552314688E-49,1.));
#39928=DIRECTION('center_axis',(-0.673700070814201,0.218898422363249,0.705841126084207));
#39929=DIRECTION('ref_axis',(0.671294802430673,-0.218116903291296,0.708370174928462));
#39930=DIRECTION('',(1.12975568624751E-48,8.20815552314688E-49,1.));
#39931=DIRECTION('center_axis',(1.15507378150847E-48,9.10586746597098E-49,
1.));
#39932=DIRECTION('ref_axis',(1.,4.33680868994202E-19,-1.15507378150847E-48));
#39933=DIRECTION('center_axis',(-0.688797850611722,0.165365733230951,-0.705841126079843));
#39934=DIRECTION('ref_axis',(0.686338679579581,-0.164775338502517,-0.708370174932809));
#39935=DIRECTION('',(1.15507378150847E-48,9.10586746597098E-49,1.));
#39936=DIRECTION('center_axis',(-0.688797850609436,0.165365733233163,0.705841126081556));
#39937=DIRECTION('ref_axis',(0.68633867958204,-0.164775338499612,0.708370174931102));
#39938=DIRECTION('',(1.15507378150847E-48,9.10586746597098E-49,1.));
#39939=DIRECTION('center_axis',(1.17327046280542E-48,1.00206764110688E-48,
1.));
#39940=DIRECTION('ref_axis',(1.,4.33680868994202E-19,-1.17327046280542E-48));
#39941=DIRECTION('center_axis',(-0.699648962604041,0.110813509366852,-0.705841126082132));
#39942=DIRECTION('ref_axis',(0.697151050543932,-0.11041787896162,-0.708370174930529));
#39943=DIRECTION('',(1.17327046280542E-48,1.00206764110688E-48,1.));
#39944=DIRECTION('center_axis',(-0.699648962604175,0.110813509367011,0.705841126081974));
#39945=DIRECTION('ref_axis',(0.697151050543496,-0.110417878963368,0.708370174930686));
#39946=DIRECTION('',(1.17327046280542E-48,1.00206764110688E-48,1.));
#39947=DIRECTION('center_axis',(1.18423354154716E-48,1.09469422570891E-48,
1.));
#39948=DIRECTION('ref_axis',(1.,4.33680868994202E-19,-1.18423354154716E-48));
#39949=DIRECTION('center_axis',(-0.706186506088737,0.0555780833649064,-0.705841126081264));
#39950=DIRECTION('ref_axis',(0.703665253451942,-0.0553796564821394,-0.708370174931394));
#39951=DIRECTION('',(1.18423354154716E-48,1.09469422570891E-48,1.));
#39952=DIRECTION('center_axis',(-0.706186506088284,0.0555780833648712,0.705841126081719));
#39953=DIRECTION('ref_axis',(0.703665253452317,-0.0553796564831855,0.70837017493094));
#39954=DIRECTION('',(1.18423354154716E-48,1.09469422570891E-48,1.));
#39955=DIRECTION('center_axis',(1.18789542670764E-48,1.18789542670763E-48,
1.));
#39956=DIRECTION('ref_axis',(1.,4.33680868994202E-19,-1.18789542670764E-48));
#39957=DIRECTION('center_axis',(-0.70837017493089,-1.25340662871076E-13,
-0.70584112608177));
#39958=DIRECTION('ref_axis',(0.70584112608177,-2.88506822019813E-13,-0.708370174930889));
#39959=DIRECTION('',(1.18789542670764E-48,1.18789542670763E-48,1.));
#39960=DIRECTION('center_axis',(-0.70837017493089,1.25340662871076E-13,
0.70584112608177));
#39961=DIRECTION('ref_axis',(0.70584112608177,2.61497947465894E-13,0.708370174930889));
#39962=DIRECTION('',(1.18789542670764E-48,1.18789542670763E-48,1.));
#39963=DIRECTION('center_axis',(1.05842257525003E-48,6.48602188298306E-49,
1.));
#39964=DIRECTION('ref_axis',(1.,4.33680868994202E-19,-1.05842257525003E-48));
#39965=DIRECTION('center_axis',(-0.631162447404585,0.321593329715507,-0.70584112608203));
#39966=DIRECTION('ref_axis',(0.628909048379288,-0.320445165567225,-0.708370174930631));
#39967=DIRECTION('',(1.05842257525003E-48,6.48602188298306E-49,1.));
#39968=DIRECTION('center_axis',(-0.631162447404969,0.32159332971786,0.705841126080614));
#39969=DIRECTION('ref_axis',(0.628909048378923,-0.320445165564824,0.708370174932041));
#39970=DIRECTION('',(1.05842257525003E-48,6.48602188298306E-49,1.));
#39971=DIRECTION('center_axis',(1.01284735186347E-48,5.67221771220248E-49,
1.));
#39972=DIRECTION('ref_axis',(1.,4.33680868994202E-19,-1.01284735186347E-48));
#39973=DIRECTION('center_axis',(-0.603984862377595,0.370122399687911,-0.705841126081486));
#39974=DIRECTION('ref_axis',(0.601828493750374,-0.368800975294447,-0.708370174931173));
#39975=DIRECTION('',(1.01284735186347E-48,5.67221771220248E-49,1.));
#39976=DIRECTION('center_axis',(-0.603984862377492,0.370122399687834,0.705841126081615));
#39977=DIRECTION('ref_axis',(0.60182849375054,-0.368800975294424,0.708370174931044));
#39978=DIRECTION('',(1.01284735186347E-48,5.67221771220248E-49,1.));
#39979=DIRECTION('center_axis',(9.61027587746754E-49,4.89668013623204E-49,
1.));
#39980=DIRECTION('ref_axis',(1.,4.33680868994202E-19,-9.61027587746754E-49));
#39981=DIRECTION('center_axis',(-0.57308350982942,0.416369541987989,-0.705841126080299));
#39982=DIRECTION('ref_axis',(-0.571037466327478,0.414883004371834,0.708370174932355));
#39983=DIRECTION('',(9.61027587746754E-49,4.89668013623204E-49,1.));
#39984=DIRECTION('center_axis',(-0.573083509826005,0.416369541988967,0.705841126082495));
#39985=DIRECTION('ref_axis',(0.571037466331126,-0.41488300437055,0.708370174930167));
#39986=DIRECTION('',(9.61027587746754E-49,4.89668013623204E-49,1.));
#39987=DIRECTION('center_axis',(9.03282768977476E-49,4.16419060212002E-49,
1.));
#39988=DIRECTION('ref_axis',(1.,4.33680868994202E-19,-9.03282768977476E-49));
#39989=DIRECTION('center_axis',(-0.538648906869708,0.460049627603881,-0.705841126082633));
#39990=DIRECTION('ref_axis',(-0.536725803041031,0.458407141763258,0.70837017493003));
#39991=DIRECTION('',(9.03282768977476E-49,4.16419060212002E-49,1.));
#39992=DIRECTION('center_axis',(-0.53864890686968,0.460049627604191,0.705841126082452));
#39993=DIRECTION('ref_axis',(0.536725803040381,-0.45840714176374,0.70837017493021));
#39994=DIRECTION('',(9.03282768977476E-49,4.16419060212002E-49,1.));
#39995=DIRECTION('center_axis',(8.39968911565451E-49,3.47926515142171E-49,
1.));
#39996=DIRECTION('ref_axis',(1.,4.33680868994202E-19,-8.39968911565451E-49));
#39997=DIRECTION('center_axis',(-0.500893354284786,0.500893354283015,-0.705841126081816));
#39998=DIRECTION('ref_axis',(-0.499105046691526,0.499105046694076,0.708370174930843));
#39999=DIRECTION('',(8.39968911565451E-49,3.47926515142171E-49,1.));
#40000=DIRECTION('center_axis',(-0.500893354285066,0.500893354283687,0.70584112608114));
#40001=DIRECTION('ref_axis',(0.49910504669045,-0.499105046694196,0.708370174931517));
#40002=DIRECTION('',(8.39968911565451E-49,3.47926515142171E-49,1.));
#40003=DIRECTION('center_axis',(7.71476366495618E-49,2.84612657730147E-49,
1.));
#40004=DIRECTION('ref_axis',(1.,4.33680868994202E-19,-7.71476366495618E-49));
#40005=DIRECTION('center_axis',(-0.460049627606723,0.538648906869542,-0.705841126080907));
#40006=DIRECTION('ref_axis',(-0.458407141764148,0.536725803038001,0.708370174931749));
#40007=DIRECTION('',(7.71476366495618E-49,2.84612657730147E-49,1.));
#40008=DIRECTION('center_axis',(-0.460049627603276,0.538648906871872,0.705841126081376));
#40009=DIRECTION('ref_axis',(0.458407141768044,-0.53672580303529,0.708370174931282));
#40010=DIRECTION('',(7.71476366495618E-49,2.84612657730147E-49,1.));
#40011=DIRECTION('center_axis',(6.98227413084414E-49,2.26867838960871E-49,
1.));
#40012=DIRECTION('ref_axis',(1.,4.33680868994202E-19,-6.98227413084414E-49));
#40013=DIRECTION('center_axis',(-0.416369541989573,0.573083509826983,-0.705841126081344));
#40014=DIRECTION('ref_axis',(-0.414883004369422,0.571037466330522,0.708370174931314));
#40015=DIRECTION('',(6.98227413084414E-49,2.26867838960871E-49,1.));
#40016=DIRECTION('center_axis',(-0.416369541986537,0.573083509827722,0.705841126082535));
#40017=DIRECTION('ref_axis',(0.414883004374377,-0.571037466328393,0.708370174930127));
#40018=DIRECTION('',(6.98227413084414E-49,2.26867838960871E-49,1.));
#40019=DIRECTION('center_axis',(6.2067365548737E-49,1.75048074844156E-49,
1.));
#40020=DIRECTION('ref_axis',(1.,4.33680868994202E-19,-6.2067365548737E-49));
#40021=DIRECTION('center_axis',(-0.370122399687787,0.603984862376041,-0.70584112608288));
#40022=DIRECTION('ref_axis',(-0.368800975294937,0.60182849375171,0.708370174929783));
#40023=DIRECTION('',(6.2067365548737E-49,1.75048074844156E-49,1.));
#40024=DIRECTION('center_axis',(-0.370122399687792,0.603984862376936,0.705841126082112));
#40025=DIRECTION('ref_axis',(0.368800975294942,-0.601828493750806,0.708370174930549));
#40026=DIRECTION('',(6.2067365548737E-49,1.75048074844156E-49,1.));
#40027=DIRECTION('center_axis',(5.39293238409311E-49,1.29472851457601E-49,
1.));
#40028=DIRECTION('ref_axis',(1.,4.33680868994202E-19,-5.39293238409311E-49));
#40029=DIRECTION('center_axis',(-0.321593329717153,0.63116244740346,-0.705841126082286));
#40030=DIRECTION('ref_axis',(-0.320445165567263,0.628909048379556,0.708370174930376));
#40031=DIRECTION('',(5.39293238409311E-49,1.29472851457601E-49,1.));
#40032=DIRECTION('center_axis',(-0.321593329716558,0.631162447403966,0.705841126082104));
#40033=DIRECTION('ref_axis',(0.320445165566995,-0.628909048379489,0.708370174930556));
#40034=DIRECTION('',(5.39293238409311E-49,1.29472851457601E-49,1.));
#40035=DIRECTION('center_axis',(0.,0.,1.));
#40036=DIRECTION('ref_axis',(1.,4.33680868994202E-19,0.));
#40037=DIRECTION('',(-0.707106781186549,-8.69022643068862E-17,0.707106781186546));
#40038=DIRECTION('center_axis',(0.,0.,1.));
#40039=DIRECTION('ref_axis',(1.,4.33680868994202E-19,0.));
#40040=DIRECTION('center_axis',(5.15167520928809E-67,-1.18789542670764E-48,
-1.));
#40041=DIRECTION('ref_axis',(0.,1.,0.));
#40042=DIRECTION('center_axis',(5.15167520928809E-67,-1.18789542670764E-48,
-1.));
#40043=DIRECTION('ref_axis',(-4.33680868994202E-19,1.,-1.18789542670764E-48));
#40044=DIRECTION('center_axis',(-1.,0.,-5.15167520928809E-67));
#40045=DIRECTION('ref_axis',(0.,-1.,0.));
#40046=DIRECTION('center_axis',(5.15167520928809E-67,-1.18789542670764E-48,
-1.));
#40047=DIRECTION('ref_axis',(-4.33680868994202E-19,1.,-1.18789542670764E-48));
#40048=DIRECTION('center_axis',(5.15167520928809E-67,-1.18789542670764E-48,
-1.));
#40049=DIRECTION('ref_axis',(-4.33680868994202E-19,1.,-1.18789542670764E-48));
#40050=DIRECTION('center_axis',(5.15167520928809E-67,-1.18789542670764E-48,
-1.));
#40051=DIRECTION('ref_axis',(-4.33680868994202E-19,1.,-1.18789542670764E-48));
#40052=DIRECTION('center_axis',(0.0555758110363288,-0.706157633406642,0.705870190622316));
#40053=DIRECTION('ref_axis',(0.0553775799352608,-0.703694571287346,-0.708341212962532));
#40054=DIRECTION('center_axis',(5.15167520928809E-67,-1.18789542670764E-48,
-1.));
#40055=DIRECTION('ref_axis',(-4.33680868994202E-19,1.,-1.18789542670764E-48));
#40056=DIRECTION('center_axis',(0.11080862020158,-0.699618093636883,0.705872490429338));
#40057=DIRECTION('ref_axis',(0.110419233095995,-0.697182591373234,-0.708338921173046));
#40058=DIRECTION('center_axis',(5.15167520928809E-67,-1.18789542670764E-48,
-1.));
#40059=DIRECTION('ref_axis',(-4.33680868994202E-19,1.,-1.18789542670764E-48));
#40060=DIRECTION('center_axis',(0.165358045050138,-0.688765827029971,0.705874176077378));
#40061=DIRECTION('ref_axis',(0.164780094681068,-0.686371526838389,-0.708337241391723));
#40062=DIRECTION('center_axis',(5.15167520928809E-67,-1.18789542670764E-48,
-1.));
#40063=DIRECTION('ref_axis',(-4.33680868994202E-19,1.,-1.18789542670764E-48));
#40064=DIRECTION('center_axis',(0.218887852522913,-0.673667540197498,0.705875451692549));
#40065=DIRECTION('ref_axis',(0.218125006053852,-0.671328261761447,-0.708335970210719));
#40066=DIRECTION('center_axis',(5.15167520928809E-67,-1.18789542670764E-48,
-1.));
#40067=DIRECTION('ref_axis',(-4.33680868994202E-19,1.,-1.18789542670764E-48));
#40068=DIRECTION('center_axis',(0.271068063822855,-0.654416196007407,0.705876439030603));
#40069=DIRECTION('ref_axis',(0.270125073931967,-0.65214568281518,-0.708334986301518));
#40070=DIRECTION('center_axis',(5.15167520928809E-67,-1.18789542670764E-48,
-1.));
#40071=DIRECTION('ref_axis',(-4.33680868994202E-19,1.,-1.18789542670764E-48));
#40072=DIRECTION('center_axis',(0.321577003370555,-0.631130405143931,0.705877214964523));
#40073=DIRECTION('ref_axis',(0.320459697262731,-0.628942147608601,-0.708334213060304));
#40074=DIRECTION('center_axis',(5.15167520928809E-67,-1.18789542670764E-48,
-1.));
#40075=DIRECTION('ref_axis',(-4.33680868994202E-19,1.,-1.18789542670764E-48));
#40076=DIRECTION('center_axis',(0.370103289326652,-0.603953677099404,0.705877830185721));
#40077=DIRECTION('ref_axis',(0.368818543504099,-0.601860775526205,-0.708333599972859));
#40078=DIRECTION('center_axis',(5.15167520928809E-67,-1.18789542670764E-48,
-1.));
#40079=DIRECTION('ref_axis',(-4.33680868994202E-19,1.,-1.18789542670764E-48));
#40080=DIRECTION('center_axis',(0.416347757295498,-0.573053525770462,0.705878319256975));
#40081=DIRECTION('ref_axis',(0.414903461782555,-0.571068576441932,-0.708333112597058));
#40082=DIRECTION('center_axis',(5.15167520928809E-67,-1.18789542670764E-48,
-1.));
#40083=DIRECTION('ref_axis',(-4.33680868994202E-19,1.,-1.18789542670764E-48));
#40084=DIRECTION('center_axis',(0.460025307051016,-0.538620431161506,0.705878706300177));
#40085=DIRECTION('ref_axis',(0.458430320957564,-0.536755427393206,-0.708332726895123));
#40086=DIRECTION('center_axis',(5.15167520928809E-67,-1.18789542670764E-48,
-1.));
#40087=DIRECTION('ref_axis',(-4.33680868994202E-19,1.,-1.18789542670764E-48));
#40088=DIRECTION('center_axis',(0.500866661619323,-0.500866661619323,0.705879008440277));
#40089=DIRECTION('ref_axis',(0.499130761357991,-0.499132905771573,-0.708332425801768));
#40090=DIRECTION('center_axis',(5.15167520928809E-67,-1.18789542670764E-48,
-1.));
#40091=DIRECTION('ref_axis',(-4.33680868994202E-19,1.,-1.18789542670764E-48));
#40092=DIRECTION('center_axis',(0.53862002836901,-0.46002496303376,0.705879237848482));
#40093=DIRECTION('ref_axis',(0.536753849182443,-0.458432987266868,-0.708332197188161));
#40094=DIRECTION('center_axis',(5.15167520928809E-67,-1.18789542670764E-48,
-1.));
#40095=DIRECTION('ref_axis',(-4.33680868994202E-19,1.,-1.18789542670764E-48));
#40096=DIRECTION('center_axis',(0.573052651970297,-0.416347122442612,0.705879403087785));
#40097=DIRECTION('ref_axis',(0.571067623542823,-0.414906617259439,-0.708332032521106));
#40098=DIRECTION('center_axis',(5.15167520928809E-67,-1.18789542670764E-48,
-1.));
#40099=DIRECTION('ref_axis',(-4.33680868994202E-19,1.,-1.18789542670764E-48));
#40100=DIRECTION('center_axis',(0.603952249837211,-0.370102414699222,0.705879509938047));
#40101=DIRECTION('ref_axis',(0.601860526500507,-0.368822164724135,-0.708331926040847));
#40102=DIRECTION('center_axis',(5.15167520928809E-67,-1.18789542670764E-48,
-1.));
#40103=DIRECTION('ref_axis',(-4.33680868994202E-19,1.,-1.18789542670764E-48));
#40104=DIRECTION('center_axis',(0.631128321247012,-0.321575941572045,0.705879561909807));
#40105=DIRECTION('ref_axis',(0.628942707293582,-0.320463768412346,-0.708331874249054));
#40106=DIRECTION('center_axis',(5.15167520928809E-67,-1.18789542670764E-48,
-1.));
#40107=DIRECTION('ref_axis',(-4.33680868994202E-19,1.,-1.18789542670764E-48));
#40108=DIRECTION('center_axis',(0.654413322126613,-0.271066873422487,0.70587956051735));
#40109=DIRECTION('ref_axis',(0.652147192704133,-0.270129585579022,-0.708331875636714));
#40110=DIRECTION('center_axis',(5.15167520928809E-67,-1.18789542670764E-48,
-1.));
#40111=DIRECTION('ref_axis',(-4.33680868994202E-19,1.,-1.18789542670764E-48));
#40112=DIRECTION('center_axis',(0.673663698306673,-0.218886604216949,0.705879505353533));
#40113=DIRECTION('ref_axis',(0.671330916306432,-0.218129954133086,-0.708331930609559));
#40114=DIRECTION('center_axis',(5.15167520928809E-67,-1.18789542670764E-48,
-1.));
#40115=DIRECTION('ref_axis',(-4.33680868994202E-19,1.,-1.18789542670764E-48));
#40116=DIRECTION('center_axis',(0.688760770927107,-0.165356831187235,0.705879393955946));
#40117=DIRECTION('ref_axis',(0.686375600198304,-0.164785479532649,-0.708332041621451));
#40118=DIRECTION('center_axis',(5.15167520928809E-67,-1.18789542670764E-48,
-1.));
#40119=DIRECTION('ref_axis',(-4.33680868994202E-19,1.,-1.18789542670764E-48));
#40120=DIRECTION('center_axis',(0.699611468639781,-0.110807570905153,0.705879221381242));
#40121=DIRECTION('ref_axis',(0.697188483633051,-0.110425058152577,-0.708332213598567));
#40122=DIRECTION('center_axis',(5.15167520928809E-67,-1.18789542670764E-48,
-1.));
#40123=DIRECTION('ref_axis',(-4.33680868994202E-19,1.,-1.18789542670764E-48));
#40124=DIRECTION('center_axis',(0.706148902304913,-0.0555751238837372,0.705878979272562));
#40125=DIRECTION('ref_axis',(0.703702893729778,-0.0553838490533553,-0.708332454868737));
#40126=DIRECTION('center_axis',(5.15167520928809E-67,-1.18789542670764E-48,
-1.));
#40127=DIRECTION('ref_axis',(-4.33680868994202E-19,1.,-1.18789542670764E-48));
#40128=DIRECTION('center_axis',(0.708332577472403,3.07190287735134E-19,
0.705878856243267));
#40129=DIRECTION('ref_axis',(0.705878856242412,-1.55615277571261E-6,-0.708332577471545));
#40130=DIRECTION('center_axis',(5.15167520928809E-67,-1.18789542670764E-48,
-1.));
#40131=DIRECTION('ref_axis',(-4.33680868994202E-19,1.,-1.18789542670764E-48));
#40132=DIRECTION('center_axis',(0.706157633406551,0.0555758110364317,0.705870190622399));
#40133=DIRECTION('ref_axis',(0.703694571287442,0.0553775799351074,-0.70834121296245));
#40134=DIRECTION('center_axis',(5.15167520928809E-67,-1.18789542670764E-48,
-1.));
#40135=DIRECTION('ref_axis',(-4.33680868994202E-19,1.,-1.18789542670764E-48));
#40136=DIRECTION('center_axis',(0.699618093637069,0.110808620201609,0.705872490429149));
#40137=DIRECTION('ref_axis',(0.697182591372912,0.11041923309682,-0.708338921173234));
#40138=DIRECTION('center_axis',(5.15167520928809E-67,-1.18789542670764E-48,
-1.));
#40139=DIRECTION('ref_axis',(-4.33680868994202E-19,1.,-1.18789542670764E-48));
#40140=DIRECTION('center_axis',(0.688765827030135,0.165358045050174,0.705874176077209));
#40141=DIRECTION('ref_axis',(0.686371526838244,0.16478009468095,-0.708337241391891));
#40142=DIRECTION('center_axis',(5.15167520928809E-67,-1.18789542670764E-48,
-1.));
#40143=DIRECTION('ref_axis',(-4.33680868994202E-19,1.,-1.18789542670764E-48));
#40144=DIRECTION('center_axis',(0.673667540197388,0.21888785252289,0.705875451692661));
#40145=DIRECTION('ref_axis',(0.671328261761852,0.21812500605297,-0.708335970210607));
#40146=DIRECTION('center_axis',(5.15167520928809E-67,-1.18789542670764E-48,
-1.));
#40147=DIRECTION('ref_axis',(-4.33680868994202E-19,1.,-1.18789542670764E-48));
#40148=DIRECTION('center_axis',(0.654416196007382,0.271068063822859,0.705876439030624));
#40149=DIRECTION('ref_axis',(0.652145682814771,0.270125073933009,-0.708334986301497));
#40150=DIRECTION('center_axis',(5.15167520928809E-67,-1.18789542670764E-48,
-1.));
#40151=DIRECTION('ref_axis',(-4.33680868994202E-19,1.,-1.18789542670764E-48));
#40152=DIRECTION('center_axis',(0.631130405143941,0.321577003370555,0.705877214964514));
#40153=DIRECTION('ref_axis',(0.628942147608526,0.320459697262857,-0.708334213060313));
#40154=DIRECTION('center_axis',(5.15167520928809E-67,-1.18789542670764E-48,
-1.));
#40155=DIRECTION('ref_axis',(-4.33680868994202E-19,1.,-1.18789542670764E-48));
#40156=DIRECTION('center_axis',(0.603953677099555,0.370103289326611,0.705877830185613));
#40157=DIRECTION('ref_axis',(0.601860775525942,0.368818543504321,-0.708333599972967));
#40158=DIRECTION('center_axis',(5.15167520928809E-67,-1.18789542670764E-48,
-1.));
#40159=DIRECTION('ref_axis',(-4.33680868994202E-19,1.,-1.18789542670764E-48));
#40160=DIRECTION('center_axis',(0.573053525770564,0.41634775729573,0.705878319256755));
#40161=DIRECTION('ref_axis',(-0.571068576442187,-0.414903461781831,0.708333112597277));
#40162=DIRECTION('center_axis',(5.15167520928809E-67,-1.18789542670764E-48,
-1.));
#40163=DIRECTION('ref_axis',(-4.33680868994202E-19,1.,-1.18789542670764E-48));
#40164=DIRECTION('center_axis',(0.538620431161647,0.46002530705115,0.705878706299982));
#40165=DIRECTION('ref_axis',(-0.536755427393011,-0.458430320957492,0.708332726895318));
#40166=DIRECTION('center_axis',(5.15167520928809E-67,-1.18789542670764E-48,
-1.));
#40167=DIRECTION('ref_axis',(-4.33680868994202E-19,1.,-1.18789542670764E-48));
#40168=DIRECTION('center_axis',(0.500866661619527,0.500866661619527,0.705879008439988));
#40169=DIRECTION('ref_axis',(-0.49913290577155,-0.499130761357605,0.708332425802057));
#40170=DIRECTION('center_axis',(5.15167520928809E-67,-1.18789542670764E-48,
-1.));
#40171=DIRECTION('ref_axis',(-4.33680868994202E-19,1.,-1.18789542670764E-48));
#40172=DIRECTION('center_axis',(0.460024963033642,0.538620028368862,0.705879237848672));
#40173=DIRECTION('ref_axis',(-0.45843298726639,-0.536753849183101,0.708332197187972));
#40174=DIRECTION('center_axis',(5.15167520928809E-67,-1.18789542670764E-48,
-1.));
#40175=DIRECTION('ref_axis',(-4.33680868994202E-19,1.,-1.18789542670764E-48));
#40176=DIRECTION('center_axis',(0.416347122442686,0.573052651970292,0.705879403087744));
#40177=DIRECTION('ref_axis',(-0.414906617258984,-0.571067623543104,0.708332032521146));
#40178=DIRECTION('center_axis',(5.15167520928809E-67,-1.18789542670764E-48,
-1.));
#40179=DIRECTION('ref_axis',(-4.33680868994202E-19,1.,-1.18789542670764E-48));
#40180=DIRECTION('center_axis',(0.370102414699172,0.603952249837277,0.705879509938016));
#40181=DIRECTION('ref_axis',(-0.368822164724246,-0.601860526500403,0.708331926040877));
#40182=DIRECTION('center_axis',(5.15167520928809E-67,-1.18789542670764E-48,
-1.));
#40183=DIRECTION('ref_axis',(-4.33680868994202E-19,1.,-1.18789542670764E-48));
#40184=DIRECTION('center_axis',(0.321575941571924,0.631128321246917,0.705879561909948));
#40185=DIRECTION('ref_axis',(-0.320463768412656,-0.628942707293582,0.708331874248914));
#40186=DIRECTION('center_axis',(5.15167520928809E-67,-1.18789542670764E-48,
-1.));
#40187=DIRECTION('ref_axis',(-4.33680868994202E-19,1.,-1.18789542670764E-48));
#40188=DIRECTION('center_axis',(0.271066873422485,0.654413322126598,0.705879560517365));
#40189=DIRECTION('ref_axis',(-0.270129585579224,-0.652147192704065,0.708331875636699));
#40190=DIRECTION('center_axis',(5.15167520928809E-67,-1.18789542670764E-48,
-1.));
#40191=DIRECTION('ref_axis',(-4.33680868994202E-19,1.,-1.18789542670764E-48));
#40192=DIRECTION('center_axis',(0.218886604216952,0.67366369830668,0.705879505353526));
#40193=DIRECTION('ref_axis',(-0.218129954132996,-0.671330916306453,0.708331930609566));
#40194=DIRECTION('center_axis',(5.15167520928809E-67,-1.18789542670764E-48,
-1.));
#40195=DIRECTION('ref_axis',(-4.33680868994202E-19,1.,-1.18789542670764E-48));
#40196=DIRECTION('center_axis',(0.16535683118711,0.68876077092705,0.705879393956031));
#40197=DIRECTION('ref_axis',(-0.164785479532882,-0.686375600198336,0.708332041621366));
#40198=DIRECTION('center_axis',(5.15167520928809E-67,-1.18789542670764E-48,
-1.));
#40199=DIRECTION('ref_axis',(-4.33680868994202E-19,1.,-1.18789542670764E-48));
#40200=DIRECTION('center_axis',(0.110807570905159,0.699611468639805,0.705879221381218));
#40201=DIRECTION('ref_axis',(-0.11042505815257,-0.697188483633028,0.708332213598592));
#40202=DIRECTION('center_axis',(5.15167520928809E-67,-1.18789542670764E-48,
-1.));
#40203=DIRECTION('ref_axis',(-4.33680868994202E-19,1.,-1.18789542670764E-48));
#40204=DIRECTION('center_axis',(0.055575123883674,0.706148902304893,0.705878979272587));
#40205=DIRECTION('ref_axis',(-0.0553838490533958,-0.7037028937298,0.708332454868712));
#40206=DIRECTION('center_axis',(5.15167520928809E-67,-1.18789542670764E-48,
-1.));
#40207=DIRECTION('ref_axis',(-4.33680868994202E-19,1.,-1.18789542670764E-48));
#40208=DIRECTION('center_axis',(4.84352581305682E-13,0.70837017493119,0.705841126081468));
#40209=DIRECTION('ref_axis',(-1.41156745807278E-12,-0.705841126081468,0.70837017493119));
#40210=DIRECTION('center_axis',(5.15167520928809E-67,-1.18789542670764E-48,
-1.));
#40211=DIRECTION('ref_axis',(-4.33680868994202E-19,1.,-1.18789542670764E-48));
#40212=DIRECTION('center_axis',(-0.0555758110363152,0.706157633406656,0.705870190622303));
#40213=DIRECTION('ref_axis',(0.0553775799350914,-0.703694571287347,0.708341212962545));
#40214=DIRECTION('center_axis',(5.15167520928809E-67,-1.18789542670764E-48,
-1.));
#40215=DIRECTION('ref_axis',(-4.33680868994202E-19,1.,-1.18789542670764E-48));
#40216=DIRECTION('center_axis',(-0.110808620201596,0.699618093636976,0.705872490429243));
#40217=DIRECTION('ref_axis',(0.11041923309583,-0.697182591373165,0.70833892117314));
#40218=DIRECTION('center_axis',(5.15167520928809E-67,-1.18789542670764E-48,
-1.));
#40219=DIRECTION('ref_axis',(-4.33680868994202E-19,1.,-1.18789542670764E-48));
#40220=DIRECTION('center_axis',(-0.165358045050154,0.688765827030126,0.705874176077223));
#40221=DIRECTION('ref_axis',(0.164780094680844,-0.686371526838284,0.708337241391878));
#40222=DIRECTION('center_axis',(5.15167520928809E-67,-1.18789542670764E-48,
-1.));
#40223=DIRECTION('ref_axis',(-4.33680868994202E-19,1.,-1.18789542670764E-48));
#40224=DIRECTION('center_axis',(-0.218887852522867,0.673667540197309,0.705875451692744));
#40225=DIRECTION('ref_axis',(0.218125006054104,-0.67132826176157,0.708335970210525));
#40226=DIRECTION('center_axis',(5.15167520928809E-67,-1.18789542670764E-48,
-1.));
#40227=DIRECTION('ref_axis',(-4.33680868994202E-19,1.,-1.18789542670764E-48));
#40228=DIRECTION('center_axis',(-0.271068063822887,0.654416196007496,0.705876439030507));
#40229=DIRECTION('ref_axis',(0.270125073932604,-0.652145682814813,0.708334986301614));
#40230=DIRECTION('center_axis',(5.15167520928809E-67,-1.18789542670764E-48,
-1.));
#40231=DIRECTION('ref_axis',(-4.33680868994202E-19,1.,-1.18789542670764E-48));
#40232=DIRECTION('center_axis',(5.15167520928809E-67,-1.18789542670764E-48,
-1.));
#40233=DIRECTION('ref_axis',(-4.33680868994202E-19,1.,-1.18789542670764E-48));
#40234=DIRECTION('center_axis',(5.15167520928809E-67,-1.18789542670764E-48,
-1.));
#40235=DIRECTION('ref_axis',(-4.33680868994202E-19,1.,-1.18789542670764E-48));
#40236=DIRECTION('center_axis',(5.15167520928809E-67,-1.18789542670764E-48,
-1.));
#40237=DIRECTION('ref_axis',(-4.33680868994202E-19,1.,-1.18789542670764E-48));
#40238=DIRECTION('center_axis',(5.15167520928809E-67,-1.18789542670764E-48,
-1.));
#40239=DIRECTION('ref_axis',(-4.33680868994202E-19,1.,-1.18789542670764E-48));
#40240=DIRECTION('center_axis',(5.15167520928809E-67,-1.18789542670764E-48,
-1.));
#40241=DIRECTION('ref_axis',(-4.33680868994202E-19,1.,-1.18789542670764E-48));
#40242=DIRECTION('center_axis',(5.15167520928809E-67,-1.18789542670764E-48,
-1.));
#40243=DIRECTION('ref_axis',(-4.33680868994202E-19,1.,-1.18789542670764E-48));
#40244=DIRECTION('center_axis',(5.15167520928809E-67,-1.18789542670764E-48,
-1.));
#40245=DIRECTION('ref_axis',(-4.33680868994202E-19,1.,-1.18789542670764E-48));
#40246=DIRECTION('center_axis',(5.15167520928809E-67,-1.18789542670764E-48,
-1.));
#40247=DIRECTION('ref_axis',(-4.33680868994202E-19,1.,-1.18789542670764E-48));
#40248=DIRECTION('center_axis',(5.15167520928809E-67,-1.18789542670764E-48,
-1.));
#40249=DIRECTION('ref_axis',(-4.33680868994202E-19,1.,-1.18789542670764E-48));
#40250=DIRECTION('center_axis',(5.15167520928809E-67,-1.18789542670764E-48,
-1.));
#40251=DIRECTION('ref_axis',(-4.33680868994202E-19,1.,-1.18789542670764E-48));
#40252=DIRECTION('center_axis',(5.15167520928809E-67,-1.18789542670764E-48,
-1.));
#40253=DIRECTION('ref_axis',(-4.33680868994202E-19,1.,-1.18789542670764E-48));
#40254=DIRECTION('center_axis',(5.15167520928809E-67,-1.18789542670764E-48,
-1.));
#40255=DIRECTION('ref_axis',(-4.33680868994202E-19,1.,-1.18789542670764E-48));
#40256=DIRECTION('center_axis',(5.15167520928809E-67,-1.18789542670764E-48,
-1.));
#40257=DIRECTION('ref_axis',(-4.33680868994202E-19,1.,-1.18789542670764E-48));
#40258=DIRECTION('center_axis',(5.15167520928809E-67,-1.18789542670764E-48,
-1.));
#40259=DIRECTION('ref_axis',(-4.33680868994202E-19,1.,-1.18789542670764E-48));
#40260=DIRECTION('center_axis',(5.15167520928809E-67,-1.18789542670764E-48,
-1.));
#40261=DIRECTION('ref_axis',(-4.33680868994202E-19,1.,-1.18789542670764E-48));
#40262=DIRECTION('center_axis',(-0.7061576334064,-0.0555758110363729,0.705870190622555));
#40263=DIRECTION('ref_axis',(0.703694571287618,0.0553775799348557,0.708341212962294));
#40264=DIRECTION('center_axis',(5.15167520928809E-67,-1.18789542670764E-48,
-1.));
#40265=DIRECTION('ref_axis',(-4.33680868994202E-19,1.,-1.18789542670764E-48));
#40266=DIRECTION('center_axis',(-0.699618093637056,-0.110808620201623,0.70587249042916));
#40267=DIRECTION('ref_axis',(0.697182591373085,0.110419233095803,0.708338921173223));
#40268=DIRECTION('center_axis',(5.15167520928809E-67,-1.18789542670764E-48,
-1.));
#40269=DIRECTION('ref_axis',(-4.33680868994202E-19,1.,-1.18789542670764E-48));
#40270=DIRECTION('center_axis',(-0.68876582703002,-0.165358045050145,0.705874176077329));
#40271=DIRECTION('ref_axis',(0.686371526838198,0.164780094681657,0.708337241391772));
#40272=DIRECTION('center_axis',(5.15167520928809E-67,-1.18789542670764E-48,
-1.));
#40273=DIRECTION('ref_axis',(-4.33680868994202E-19,1.,-1.18789542670764E-48));
#40274=DIRECTION('center_axis',(-0.673667540197642,-0.218887852522971,0.705875451692394));
#40275=DIRECTION('ref_axis',(0.671328261761337,0.218125006053688,0.708335970210874));
#40276=DIRECTION('center_axis',(5.15167520928809E-67,-1.18789542670764E-48,
-1.));
#40277=DIRECTION('ref_axis',(-4.33680868994202E-19,1.,-1.18789542670764E-48));
#40278=DIRECTION('center_axis',(-0.654416196007479,-0.271068063822885,0.705876439030525));
#40279=DIRECTION('ref_axis',(0.652145682815046,0.270125073932086,0.708334986301596));
#40280=DIRECTION('center_axis',(5.15167520928809E-67,-1.18789542670764E-48,
-1.));
#40281=DIRECTION('ref_axis',(-4.33680868994202E-19,1.,-1.18789542670764E-48));
#40282=DIRECTION('center_axis',(-0.631130405143739,-0.321577003370466,0.705877214964735));
#40283=DIRECTION('ref_axis',(0.628942147608447,0.3204596972635,0.708334213060093));
#40284=DIRECTION('center_axis',(5.15167520928809E-67,-1.18789542670764E-48,
-1.));
#40285=DIRECTION('ref_axis',(-4.33680868994202E-19,1.,-1.18789542670764E-48));
#40286=DIRECTION('center_axis',(-0.603953677099563,-0.37010328932661,0.705877830185607));
#40287=DIRECTION('ref_axis',(0.601860775526009,0.3688185435042,0.708333599972973));
#40288=DIRECTION('center_axis',(5.15167520928809E-67,-1.18789542670764E-48,
-1.));
#40289=DIRECTION('ref_axis',(-4.33680868994202E-19,1.,-1.18789542670764E-48));
#40290=DIRECTION('center_axis',(-0.573053525770468,-0.416347757295655,0.705878319256877));
#40291=DIRECTION('ref_axis',(-0.571068576442267,-0.414903461781928,-0.708333112597156));
#40292=DIRECTION('center_axis',(5.15167520928809E-67,-1.18789542670764E-48,
-1.));
#40293=DIRECTION('ref_axis',(-4.33680868994202E-19,1.,-1.18789542670764E-48));
#40294=DIRECTION('center_axis',(-0.5386204311615,-0.460025307051025,0.705878706300176));
#40295=DIRECTION('ref_axis',(-0.53675542739315,-0.458430320957627,-0.708332726895124));
#40296=DIRECTION('center_axis',(5.15167520928809E-67,-1.18789542670764E-48,
-1.));
#40297=DIRECTION('ref_axis',(-4.33680868994202E-19,1.,-1.18789542670764E-48));
#40298=DIRECTION('center_axis',(-0.500866661619536,-0.500866661619512,0.705879008439992));
#40299=DIRECTION('ref_axis',(-0.499132905770748,-0.499130761358414,-0.708332425802052));
#40300=DIRECTION('center_axis',(5.15167520928809E-67,-1.18789542670764E-48,
-1.));
#40301=DIRECTION('ref_axis',(-4.33680868994202E-19,1.,-1.18789542670764E-48));
#40302=DIRECTION('center_axis',(-0.460024963033767,-0.538620028369008,0.70587923784848));
#40303=DIRECTION('ref_axis',(-0.45843298726701,-0.536753849182318,-0.708332197188163));
#40304=DIRECTION('center_axis',(5.15167520928809E-67,-1.18789542670764E-48,
-1.));
#40305=DIRECTION('ref_axis',(-4.33680868994202E-19,1.,-1.18789542670764E-48));
#40306=DIRECTION('center_axis',(-0.416347122442742,-0.573052651970378,0.705879403087642));
#40307=DIRECTION('ref_axis',(-0.414906617259033,-0.571067623542942,-0.708332032521248));
#40308=DIRECTION('center_axis',(5.15167520928809E-67,-1.18789542670764E-48,
-1.));
#40309=DIRECTION('ref_axis',(-4.33680868994202E-19,1.,-1.18789542670764E-48));
#40310=DIRECTION('center_axis',(-0.370102414699178,-0.603952249837274,0.705879509938015));
#40311=DIRECTION('ref_axis',(-0.368822164723695,-0.601860526500739,-0.708331926040878));
#40312=DIRECTION('center_axis',(5.15167520928809E-67,-1.18789542670764E-48,
-1.));
#40313=DIRECTION('ref_axis',(-4.33680868994202E-19,1.,-1.18789542670764E-48));
#40314=DIRECTION('center_axis',(-0.321575941572111,-0.631128321247095,0.705879561909702));
#40315=DIRECTION('ref_axis',(-0.320463768412258,-0.628942707293509,-0.708331874249159));
#40316=DIRECTION('center_axis',(5.15167520928809E-67,-1.18789542670764E-48,
-1.));
#40317=DIRECTION('ref_axis',(-4.33680868994202E-19,1.,-1.18789542670764E-48));
#40318=DIRECTION('center_axis',(-0.271066873422704,-0.654413322126826,0.70587956051707));
#40319=DIRECTION('ref_axis',(-0.270129585579653,-0.652147192703568,-0.708331875636993));
#40320=DIRECTION('center_axis',(5.15167520928809E-67,-1.18789542670764E-48,
-1.));
#40321=DIRECTION('ref_axis',(-4.33680868994202E-19,1.,-1.18789542670764E-48));
#40322=DIRECTION('center_axis',(-0.218886604216915,-0.673663698306575,0.705879505353637));
#40323=DIRECTION('ref_axis',(-0.218129954131654,-0.671330916307006,-0.708331930609455));
#40324=DIRECTION('center_axis',(5.15167520928809E-67,-1.18789542670764E-48,
-1.));
#40325=DIRECTION('ref_axis',(-4.33680868994202E-19,1.,-1.18789542670764E-48));
#40326=DIRECTION('center_axis',(-0.165356831187205,-0.688760770926913,0.705879393956142));
#40327=DIRECTION('ref_axis',(-0.164785479532657,-0.686375600198504,-0.708332041621255));
#40328=DIRECTION('center_axis',(5.15167520928809E-67,-1.18789542670764E-48,
-1.));
#40329=DIRECTION('ref_axis',(-4.33680868994202E-19,1.,-1.18789542670764E-48));
#40330=DIRECTION('center_axis',(-0.110807570905278,-0.699611468639872,0.705879221381132));
#40331=DIRECTION('ref_axis',(-0.110425058152835,-0.697188483632899,-0.708332213598677));
#40332=DIRECTION('center_axis',(5.15167520928809E-67,-1.18789542670764E-48,
-1.));
#40333=DIRECTION('ref_axis',(-4.33680868994202E-19,1.,-1.18789542670764E-48));
#40334=DIRECTION('center_axis',(-0.0555751238837442,-0.706148902305009,
0.705878979272465));
#40335=DIRECTION('ref_axis',(-0.0553838490528384,-0.703702893729722,-0.708332454868834));
#40336=DIRECTION('center_axis',(5.15167520928809E-67,-1.18789542670764E-48,
-1.));
#40337=DIRECTION('ref_axis',(-4.33680868994202E-19,1.,-1.18789542670764E-48));
#40338=DIRECTION('',(8.62889469402126E-17,0.707106781186547,0.707106781186548));
#40339=DIRECTION('center_axis',(-5.15167520928809E-67,1.18789542670764E-48,
1.));
#40340=DIRECTION('ref_axis',(4.33680868994202E-19,-1.,1.18789542670764E-48));
#40341=DIRECTION('center_axis',(5.15167520928809E-67,-1.18789542670764E-48,
-1.));
#40342=DIRECTION('ref_axis',(-4.33680868994202E-19,1.,-1.18789542670764E-48));
#40343=DIRECTION('center_axis',(0.0555758110363494,0.706157633406676,-0.705870190622281));
#40344=DIRECTION('ref_axis',(0.0553775799347821,0.703694571287349,0.708341212962568));
#40345=DIRECTION('center_axis',(5.15167520928809E-67,-1.18789542670764E-48,
-1.));
#40346=DIRECTION('ref_axis',(-4.33680868994202E-19,1.,-1.18789542670764E-48));
#40347=DIRECTION('center_axis',(0.110808620201597,0.699618093636782,-0.705872490429435));
#40348=DIRECTION('ref_axis',(0.110419233096536,0.697182591373247,0.708338921172949));
#40349=DIRECTION('center_axis',(5.15167520928809E-67,-1.18789542670764E-48,
-1.));
#40350=DIRECTION('ref_axis',(-4.33680868994202E-19,1.,-1.18789542670764E-48));
#40351=DIRECTION('center_axis',(0.165358045050176,0.688765827030065,-0.705874176077277));
#40352=DIRECTION('ref_axis',(0.164780094681565,0.686371526838166,0.708337241391824));
#40353=DIRECTION('center_axis',(5.15167520928809E-67,-1.18789542670764E-48,
-1.));
#40354=DIRECTION('ref_axis',(-4.33680868994202E-19,1.,-1.18789542670764E-48));
#40355=DIRECTION('center_axis',(0.218887852522828,0.673667540197125,-0.705875451692931));
#40356=DIRECTION('ref_axis',(0.218125006053502,0.671328261761963,0.708335970210338));
#40357=DIRECTION('center_axis',(5.15167520928809E-67,-1.18789542670764E-48,
-1.));
#40358=DIRECTION('ref_axis',(-4.33680868994202E-19,1.,-1.18789542670764E-48));
#40359=DIRECTION('center_axis',(0.271068063822916,0.654416196007463,-0.705876439030527));
#40360=DIRECTION('ref_axis',(0.270125073931817,0.65214568281516,0.708334986301594));
#40361=DIRECTION('center_axis',(5.15167520928809E-67,-1.18789542670764E-48,
-1.));
#40362=DIRECTION('ref_axis',(-4.33680868994202E-19,1.,-1.18789542670764E-48));
#40363=DIRECTION('center_axis',(0.321577003370433,0.631130405143686,-0.705877214964798));
#40364=DIRECTION('ref_axis',(0.320459697263181,0.62894214760868,0.70833421306003));
#40365=DIRECTION('center_axis',(5.15167520928809E-67,-1.18789542670764E-48,
-1.));
#40366=DIRECTION('ref_axis',(-4.33680868994202E-19,1.,-1.18789542670764E-48));
#40367=DIRECTION('center_axis',(0.37010328932647,0.603953677099309,-0.705877830185898));
#40368=DIRECTION('ref_axis',(0.368818543504439,0.601860775526204,0.708333599972683));
#40369=DIRECTION('center_axis',(5.15167520928809E-67,-1.18789542670764E-48,
-1.));
#40370=DIRECTION('ref_axis',(-4.33680868994202E-19,1.,-1.18789542670764E-48));
#40371=DIRECTION('center_axis',(0.416347757295563,0.573053525770315,-0.705878319257056));
#40372=DIRECTION('ref_axis',(0.414903461782186,0.5710685764423,0.708333112596977));
#40373=DIRECTION('center_axis',(5.15167520928809E-67,-1.18789542670764E-48,
-1.));
#40374=DIRECTION('ref_axis',(-4.33680868994202E-19,1.,-1.18789542670764E-48));
#40375=DIRECTION('center_axis',(0.46002530705103,0.538620431161473,-0.705878706300193));
#40376=DIRECTION('ref_axis',(0.458430320957387,0.536755427393379,0.708332726895108));
#40377=DIRECTION('center_axis',(5.15167520928809E-67,-1.18789542670764E-48,
-1.));
#40378=DIRECTION('ref_axis',(-4.33680868994202E-19,1.,-1.18789542670764E-48));
#40379=DIRECTION('center_axis',(0.500866661619595,0.500866661619595,-0.705879008439891));
#40380=DIRECTION('ref_axis',(0.499130761358023,0.499132905770996,0.708332425802153));
#40381=DIRECTION('center_axis',(5.15167520928809E-67,-1.18789542670764E-48,
-1.));
#40382=DIRECTION('ref_axis',(-4.33680868994202E-19,1.,-1.18789542670764E-48));
#40383=DIRECTION('center_axis',(0.538620028368889,0.460024963033635,-0.705879237848656));
#40384=DIRECTION('ref_axis',(0.536753849182959,0.458432987266531,0.708332197187987));
#40385=DIRECTION('center_axis',(5.15167520928809E-67,-1.18789542670764E-48,
-1.));
#40386=DIRECTION('ref_axis',(-4.33680868994202E-19,1.,-1.18789542670764E-48));
#40387=DIRECTION('center_axis',(0.573052651970233,0.416347122442629,-0.705879403087826));
#40388=DIRECTION('ref_axis',(0.57106762354309,0.414906617259142,0.708332032521065));
#40389=DIRECTION('center_axis',(5.15167520928809E-67,-1.18789542670764E-48,
-1.));
#40390=DIRECTION('ref_axis',(-4.33680868994202E-19,1.,-1.18789542670764E-48));
#40391=DIRECTION('center_axis',(0.603952249837032,0.370102414699012,-0.70587950993831));
#40392=DIRECTION('ref_axis',(0.601860526500475,0.36882216472469,0.708331926040585));
#40393=DIRECTION('center_axis',(5.15167520928809E-67,-1.18789542670764E-48,
-1.));
#40394=DIRECTION('ref_axis',(-4.33680868994202E-19,1.,-1.18789542670764E-48));
#40395=DIRECTION('center_axis',(0.631128321246922,0.32157594157199,-0.705879561909913));
#40396=DIRECTION('ref_axis',(0.628942707293632,0.32046376841248,0.708331874248949));
#40397=DIRECTION('center_axis',(5.15167520928809E-67,-1.18789542670764E-48,
-1.));
#40398=DIRECTION('ref_axis',(-4.33680868994202E-19,1.,-1.18789542670764E-48));
#40399=DIRECTION('center_axis',(0.654413322126609,0.271066873422466,-0.705879560517362));
#40400=DIRECTION('ref_axis',(0.652147192704168,0.270129585578968,0.708331875636702));
#40401=DIRECTION('center_axis',(5.15167520928809E-67,-1.18789542670764E-48,
-1.));
#40402=DIRECTION('ref_axis',(-4.33680868994202E-19,1.,-1.18789542670764E-48));
#40403=DIRECTION('center_axis',(0.673663698306398,0.218886604216837,-0.70587950535383));
#40404=DIRECTION('ref_axis',(0.671330916306662,0.218129954133339,0.708331930609263));
#40405=DIRECTION('center_axis',(5.15167520928809E-67,-1.18789542670764E-48,
-1.));
#40406=DIRECTION('ref_axis',(-4.33680868994202E-19,1.,-1.18789542670764E-48));
#40407=DIRECTION('center_axis',(0.688760770927087,0.165356831187229,-0.705879393955967));
#40408=DIRECTION('ref_axis',(0.686375600198292,0.164785479532791,0.70833204162143));
#40409=DIRECTION('center_axis',(5.15167520928809E-67,-1.18789542670764E-48,
-1.));
#40410=DIRECTION('ref_axis',(-4.33680868994202E-19,1.,-1.18789542670764E-48));
#40411=DIRECTION('center_axis',(0.699611468639904,0.110807570905141,-0.705879221381122));
#40412=DIRECTION('ref_axis',(0.697188483632864,0.11042505815299,0.708332213598687));
#40413=DIRECTION('center_axis',(5.15167520928809E-67,-1.18789542670764E-48,
-1.));
#40414=DIRECTION('ref_axis',(-4.33680868994202E-19,1.,-1.18789542670764E-48));
#40415=DIRECTION('center_axis',(0.706148902304704,0.0555751238836885,-0.705878979272775));
#40416=DIRECTION('ref_axis',(0.703702893729991,0.0553838490533688,0.708332454868525));
#40417=DIRECTION('center_axis',(5.15167520928809E-67,-1.18789542670764E-48,
-1.));
#40418=DIRECTION('ref_axis',(-4.33680868994202E-19,1.,-1.18789542670764E-48));
#40419=DIRECTION('center_axis',(0.708332577472139,3.0719028773502E-19,-0.705878856243532));
#40420=DIRECTION('ref_axis',(0.705878856242677,1.5561538090606E-6,0.708332577471281));
#40421=DIRECTION('center_axis',(5.15167520928809E-67,-1.18789542670764E-48,
-1.));
#40422=DIRECTION('ref_axis',(-4.33680868994202E-19,1.,-1.18789542670764E-48));
#40423=DIRECTION('center_axis',(0.706157633406651,-0.0555758110363464,-0.705870190622306));
#40424=DIRECTION('ref_axis',(0.703694571287399,-0.0553775799344575,0.708341212962543));
#40425=DIRECTION('center_axis',(5.15167520928809E-67,-1.18789542670764E-48,
-1.));
#40426=DIRECTION('ref_axis',(-4.33680868994202E-19,1.,-1.18789542670764E-48));
#40427=DIRECTION('center_axis',(0.699618093636944,-0.110808620201621,-0.705872490429271));
#40428=DIRECTION('ref_axis',(0.697182591373154,-0.110419233096072,0.708338921173112));
#40429=DIRECTION('center_axis',(5.15167520928809E-67,-1.18789542670764E-48,
-1.));
#40430=DIRECTION('ref_axis',(-4.33680868994202E-19,1.,-1.18789542670764E-48));
#40431=DIRECTION('center_axis',(0.688765827030149,-0.165358045050179,-0.705874176077195));
#40432=DIRECTION('ref_axis',(0.686371526838092,-0.164780094681522,0.708337241391906));
#40433=DIRECTION('center_axis',(5.15167520928809E-67,-1.18789542670764E-48,
-1.));
#40434=DIRECTION('ref_axis',(-4.33680868994202E-19,1.,-1.18789542670764E-48));
#40435=DIRECTION('center_axis',(0.673667540197491,-0.218887852522947,-0.705875451692545));
#40436=DIRECTION('ref_axis',(0.671328261761432,-0.218125006053886,0.708335970210723));
#40437=DIRECTION('center_axis',(5.15167520928809E-67,-1.18789542670764E-48,
-1.));
#40438=DIRECTION('ref_axis',(-4.33680868994202E-19,1.,-1.18789542670764E-48));
#40439=DIRECTION('center_axis',(0.654416196007489,-0.271068063822922,-0.705876439030501));
#40440=DIRECTION('ref_axis',(0.652145682814786,-0.270125073932652,0.70833498630162));
#40441=DIRECTION('center_axis',(5.15167520928809E-67,-1.18789542670764E-48,
-1.));
#40442=DIRECTION('ref_axis',(-4.33680868994202E-19,1.,-1.18789542670764E-48));
#40443=DIRECTION('center_axis',(0.631130405143858,-0.321577003370522,-0.705877214964604));
#40444=DIRECTION('ref_axis',(0.628942147608515,-0.320459697263077,0.708334213060224));
#40445=DIRECTION('center_axis',(5.15167520928809E-67,-1.18789542670764E-48,
-1.));
#40446=DIRECTION('ref_axis',(-4.33680868994202E-19,1.,-1.18789542670764E-48));
#40447=DIRECTION('center_axis',(0.603953677099314,-0.37010328932649,-0.705877830185883));
#40448=DIRECTION('ref_axis',(0.60186077552563,-0.368818543505346,0.708333599972698));
#40449=DIRECTION('center_axis',(5.15167520928809E-67,-1.18789542670764E-48,
-1.));
#40450=DIRECTION('ref_axis',(-4.33680868994202E-19,1.,-1.18789542670764E-48));
#40451=DIRECTION('center_axis',(0.573053525770311,-0.416347757295561,-0.70587831925706));
#40452=DIRECTION('ref_axis',(-0.571068576442179,0.41490346178236,-0.708333112596973));
#40453=DIRECTION('center_axis',(5.15167520928809E-67,-1.18789542670764E-48,
-1.));
#40454=DIRECTION('ref_axis',(-4.33680868994202E-19,1.,-1.18789542670764E-48));
#40455=DIRECTION('center_axis',(0.53862043116148,-0.460025307051029,-0.705878706300189));
#40456=DIRECTION('ref_axis',(-0.536755427393413,0.45843032095734,-0.708332726895112));
#40457=DIRECTION('center_axis',(5.15167520928809E-67,-1.18789542670764E-48,
-1.));
#40458=DIRECTION('ref_axis',(-4.33680868994202E-19,1.,-1.18789542670764E-48));
#40459=DIRECTION('center_axis',(0.500866661619453,-0.500866661619453,-0.705879008440093));
#40460=DIRECTION('ref_axis',(-0.499132905770974,0.49913076135833,-0.708332425801952));
#40461=DIRECTION('center_axis',(5.15167520928809E-67,-1.18789542670764E-48,
-1.));
#40462=DIRECTION('ref_axis',(-4.33680868994202E-19,1.,-1.18789542670764E-48));
#40463=DIRECTION('center_axis',(0.460024963033751,-0.538620028369041,-0.705879237848464));
#40464=DIRECTION('ref_axis',(-0.458432987266724,0.536753849182542,-0.708332197188179));
#40465=DIRECTION('center_axis',(5.15167520928809E-67,-1.18789542670764E-48,
-1.));
#40466=DIRECTION('ref_axis',(-4.33680868994202E-19,1.,-1.18789542670764E-48));
#40467=DIRECTION('center_axis',(0.416347122442499,-0.573052651970059,-0.705879403088044));
#40468=DIRECTION('ref_axis',(-0.414906617258677,0.571067623543698,-0.708332032520848));
#40469=DIRECTION('center_axis',(5.15167520928809E-67,-1.18789542670764E-48,
-1.));
#40470=DIRECTION('ref_axis',(-4.33680868994202E-19,1.,-1.18789542670764E-48));
#40471=DIRECTION('center_axis',(0.370102414698996,-0.603952249837027,-0.705879509938322));
#40472=DIRECTION('ref_axis',(-0.36882216472453,0.601860526500588,-0.708331926040572));
#40473=DIRECTION('center_axis',(5.15167520928809E-67,-1.18789542670764E-48,
-1.));
#40474=DIRECTION('ref_axis',(-4.33680868994202E-19,1.,-1.18789542670764E-48));
#40475=DIRECTION('center_axis',(0.321575941571994,-0.631128321246919,-0.705879561909914));
#40476=DIRECTION('ref_axis',(-0.320463768412686,0.628942707293528,-0.708331874248948));
#40477=DIRECTION('center_axis',(5.15167520928809E-67,-1.18789542670764E-48,
-1.));
#40478=DIRECTION('ref_axis',(-4.33680868994202E-19,1.,-1.18789542670764E-48));
#40479=DIRECTION('center_axis',(0.27106687342253,-0.654413322126797,-0.705879560517163));
#40480=DIRECTION('ref_axis',(-0.270129585579053,0.652147192703917,-0.7083318756369));
#40481=DIRECTION('center_axis',(5.15167520928809E-67,-1.18789542670764E-48,
-1.));
#40482=DIRECTION('ref_axis',(-4.33680868994202E-19,1.,-1.18789542670764E-48));
#40483=DIRECTION('center_axis',(0.218886604216888,-0.673663698306596,-0.705879505353626));
#40484=DIRECTION('ref_axis',(-0.218129954133397,0.671330916306428,-0.708331930609466));
#40485=DIRECTION('center_axis',(5.15167520928809E-67,-1.18789542670764E-48,
-1.));
#40486=DIRECTION('ref_axis',(-4.33680868994202E-19,1.,-1.18789542670764E-48));
#40487=DIRECTION('center_axis',(0.165356831187193,-0.688760770926925,-0.705879393956133));
#40488=DIRECTION('ref_axis',(-0.164785479532379,0.686375600198561,-0.708332041621264));
#40489=DIRECTION('center_axis',(5.15167520928809E-67,-1.18789542670764E-48,
-1.));
#40490=DIRECTION('ref_axis',(-4.33680868994202E-19,1.,-1.18789542670764E-48));
#40491=DIRECTION('center_axis',(0.110807570905112,-0.699611468639716,-0.705879221381312));
#40492=DIRECTION('ref_axis',(-0.110425058152835,0.697188483633082,-0.708332213598497));
#40493=DIRECTION('center_axis',(5.15167520928809E-67,-1.18789542670764E-48,
-1.));
#40494=DIRECTION('ref_axis',(-4.33680868994202E-19,1.,-1.18789542670764E-48));
#40495=DIRECTION('center_axis',(0.0555751238837179,-0.706148902304883,-0.705878979272593));
#40496=DIRECTION('ref_axis',(-0.0553838490533129,0.703702893729813,-0.708332454868706));
#40497=DIRECTION('center_axis',(5.15167520928809E-67,-1.18789542670764E-48,
-1.));
#40498=DIRECTION('ref_axis',(-4.33680868994202E-19,1.,-1.18789542670764E-48));
#40499=DIRECTION('center_axis',(4.22129745643424E-13,-0.708370174930854,
-0.705841126081805));
#40500=DIRECTION('ref_axis',(-3.47233154276107E-12,0.705841126081805,-0.708370174930854));
#40501=DIRECTION('center_axis',(5.15167520928809E-67,-1.18789542670764E-48,
-1.));
#40502=DIRECTION('ref_axis',(-4.33680868994202E-19,1.,-1.18789542670764E-48));
#40503=DIRECTION('center_axis',(-0.0555758110363383,-0.706157633406556,
-0.705870190622402));
#40504=DIRECTION('ref_axis',(0.0553775799352142,0.703694571287436,-0.708341212962447));
#40505=DIRECTION('center_axis',(5.15167520928809E-67,-1.18789542670764E-48,
-1.));
#40506=DIRECTION('ref_axis',(-4.33680868994202E-19,1.,-1.18789542670764E-48));
#40507=DIRECTION('center_axis',(-0.110808620201578,-0.699618093636773,-0.705872490429447));
#40508=DIRECTION('ref_axis',(0.110419233096311,0.697182591373295,-0.708338921172937));
#40509=DIRECTION('center_axis',(5.15167520928809E-67,-1.18789542670764E-48,
-1.));
#40510=DIRECTION('ref_axis',(-4.33680868994202E-19,1.,-1.18789542670764E-48));
#40511=DIRECTION('center_axis',(-0.165358045050148,-0.688765827029952,-0.705874176077394));
#40512=DIRECTION('ref_axis',(0.164780094682061,0.686371526838168,-0.708337241391707));
#40513=DIRECTION('center_axis',(5.15167520928809E-67,-1.18789542670764E-48,
-1.));
#40514=DIRECTION('ref_axis',(-4.33680868994202E-19,1.,-1.18789542670764E-48));
#40515=DIRECTION('center_axis',(-0.218887852522884,-0.673667540197305,-0.705875451692742));
#40516=DIRECTION('ref_axis',(0.218125006053241,0.671328261761849,-0.708335970210527));
#40517=DIRECTION('center_axis',(5.15167520928809E-67,-1.18789542670764E-48,
-1.));
#40518=DIRECTION('ref_axis',(-4.33680868994202E-19,1.,-1.18789542670764E-48));
#40519=DIRECTION('center_axis',(-0.271068063822912,-0.654416196007481,-0.705876439030512));
#40520=DIRECTION('ref_axis',(0.270125073931987,0.652145682815073,-0.708334986301609));
#40521=DIRECTION('center_axis',(5.15167520928809E-67,-1.18789542670764E-48,
-1.));
#40522=DIRECTION('ref_axis',(-4.33680868994202E-19,1.,-1.18789542670764E-48));
#40523=DIRECTION('center_axis',(-0.321577003370454,-0.631130405143677,-0.705877214964797));
#40524=DIRECTION('ref_axis',(0.32045969726294,0.628942147608801,-0.708334213060031));
#40525=DIRECTION('center_axis',(5.15167520928809E-67,-1.18789542670764E-48,
-1.));
#40526=DIRECTION('ref_axis',(-4.33680868994202E-19,1.,-1.18789542670764E-48));
#40527=DIRECTION('center_axis',(-0.370103289326527,-0.60395367709939,-0.705877830185799));
#40528=DIRECTION('ref_axis',(0.368818543504467,0.601860775526071,-0.708333599972782));
#40529=DIRECTION('center_axis',(5.15167520928809E-67,-1.18789542670764E-48,
-1.));
#40530=DIRECTION('ref_axis',(-4.33680868994202E-19,1.,-1.18789542670764E-48));
#40531=DIRECTION('center_axis',(-0.41634775729562,-0.5730535257704,-0.705878319256953));
#40532=DIRECTION('ref_axis',(0.414903461781904,0.571068576442378,-0.70833311259708));
#40533=DIRECTION('center_axis',(5.15167520928809E-67,-1.18789542670764E-48,
-1.));
#40534=DIRECTION('ref_axis',(-4.33680868994202E-19,1.,-1.18789542670764E-48));
#40535=DIRECTION('center_axis',(-0.460025307050912,-0.538620431161332,-0.705878706300378));
#40536=DIRECTION('ref_axis',(0.458430320957773,0.536755427393291,-0.708332726894923));
#40537=DIRECTION('center_axis',(5.15167520928809E-67,-1.18789542670764E-48,
-1.));
#40538=DIRECTION('ref_axis',(-4.33680868994202E-19,1.,-1.18789542670764E-48));
#40539=DIRECTION('center_axis',(-0.500866661619468,-0.500866661619444,-0.705879008440089));
#40540=DIRECTION('ref_axis',(0.499130761358181,0.499132905771117,-0.708332425801956));
#40541=DIRECTION('center_axis',(5.15167520928809E-67,-1.18789542670764E-48,
-1.));
#40542=DIRECTION('ref_axis',(-4.33680868994202E-19,1.,-1.18789542670764E-48));
#40543=DIRECTION('center_axis',(-0.538620028368883,-0.46002496303363,-0.705879237848664));
#40544=DIRECTION('ref_axis',(0.536753849182796,0.458432987266734,-0.70833219718798));
#40545=DIRECTION('center_axis',(5.15167520928809E-67,-1.18789542670764E-48,
-1.));
#40546=DIRECTION('ref_axis',(-4.33680868994202E-19,1.,-1.18789542670764E-48));
#40547=DIRECTION('center_axis',(-0.573052651970218,-0.416347122442612,-0.705879403087848));
#40548=DIRECTION('ref_axis',(0.571067623543181,0.414906617259055,-0.708332032521043));
#40549=DIRECTION('center_axis',(5.15167520928809E-67,-1.18789542670764E-48,
-1.));
#40550=DIRECTION('ref_axis',(-4.33680868994202E-19,1.,-1.18789542670764E-48));
#40551=DIRECTION('center_axis',(-0.603952249837038,-0.37010241469901,-0.705879509938305));
#40552=DIRECTION('ref_axis',(0.601860526500551,0.368822164724558,-0.708331926040589));
#40553=DIRECTION('center_axis',(5.15167520928809E-67,-1.18789542670764E-48,
-1.));
#40554=DIRECTION('ref_axis',(-4.33680868994202E-19,1.,-1.18789542670764E-48));
#40555=DIRECTION('center_axis',(-0.631128321246897,-0.32157594157199,-0.705879561909935));
#40556=DIRECTION('ref_axis',(0.628942707294004,0.320463768411799,-0.708331874248927));
#40557=DIRECTION('center_axis',(5.15167520928809E-67,-1.18789542670764E-48,
-1.));
#40558=DIRECTION('ref_axis',(-4.33680868994202E-19,1.,-1.18789542670764E-48));
#40559=DIRECTION('center_axis',(-0.654413322126778,-0.271066873422522,-0.705879560517184));
#40560=DIRECTION('ref_axis',(0.65214719270402,0.270129585578859,-0.708331875636879));
#40561=DIRECTION('center_axis',(5.15167520928809E-67,-1.18789542670764E-48,
-1.));
#40562=DIRECTION('ref_axis',(-4.33680868994202E-19,1.,-1.18789542670764E-48));
#40563=DIRECTION('center_axis',(-0.673663698306464,-0.218886604216857,-0.705879505353761));
#40564=DIRECTION('ref_axis',(0.671330916306719,0.218129954132939,-0.708331930609331));
#40565=DIRECTION('center_axis',(5.15167520928809E-67,-1.18789542670764E-48,
-1.));
#40566=DIRECTION('ref_axis',(-4.33680868994202E-19,1.,-1.18789542670764E-48));
#40567=DIRECTION('center_axis',(-0.688760770927255,-0.165356831187267,-0.705879393955794));
#40568=DIRECTION('ref_axis',(0.686375600198197,0.164785479532444,-0.708332041621602));
#40569=DIRECTION('center_axis',(5.15167520928809E-67,-1.18789542670764E-48,
-1.));
#40570=DIRECTION('ref_axis',(-4.33680868994202E-19,1.,-1.18789542670764E-48));
#40571=DIRECTION('center_axis',(-0.699611468639891,-0.110807570905155,-0.705879221381132));
#40572=DIRECTION('ref_axis',(0.697188483632974,0.110425058152362,-0.708332213598677));
#40573=DIRECTION('center_axis',(5.15167520928809E-67,-1.18789542670764E-48,
-1.));
#40574=DIRECTION('ref_axis',(-4.33680868994202E-19,1.,-1.18789542670764E-48));
#40575=DIRECTION('center_axis',(-0.706148902304619,-0.0555751238836977,
-0.705878979272859));
#40576=DIRECTION('ref_axis',(0.703702893730101,0.0553838490530483,-0.708332454868441));
#40577=DIRECTION('center_axis',(5.15167520928809E-67,-1.18789542670764E-48,
-1.));
#40578=DIRECTION('ref_axis',(-4.33680868994202E-19,1.,-1.18789542670764E-48));
#40579=DIRECTION('center_axis',(5.15167520928809E-67,-1.18789542670764E-48,
-1.));
#40580=DIRECTION('ref_axis',(-4.33680868994202E-19,1.,-1.18789542670764E-48));
#40581=DIRECTION('center_axis',(5.15167520928809E-67,-1.18789542670764E-48,
-1.));
#40582=DIRECTION('ref_axis',(-4.33680868994202E-19,1.,-1.18789542670764E-48));
#40583=DIRECTION('center_axis',(5.15167520928809E-67,-1.18789542670764E-48,
-1.));
#40584=DIRECTION('ref_axis',(-4.33680868994202E-19,1.,-1.18789542670764E-48));
#40585=DIRECTION('center_axis',(5.15167520928809E-67,-1.18789542670764E-48,
-1.));
#40586=DIRECTION('ref_axis',(-4.33680868994202E-19,1.,-1.18789542670764E-48));
#40587=DIRECTION('center_axis',(5.15167520928809E-67,-1.18789542670764E-48,
-1.));
#40588=DIRECTION('ref_axis',(-4.33680868994202E-19,1.,-1.18789542670764E-48));
#40589=DIRECTION('center_axis',(5.15167520928809E-67,-1.18789542670764E-48,
-1.));
#40590=DIRECTION('ref_axis',(-4.33680868994202E-19,1.,-1.18789542670764E-48));
#40591=DIRECTION('center_axis',(5.15167520928809E-67,-1.18789542670764E-48,
-1.));
#40592=DIRECTION('ref_axis',(-4.33680868994202E-19,1.,-1.18789542670764E-48));
#40593=DIRECTION('center_axis',(5.15167520928809E-67,-1.18789542670764E-48,
-1.));
#40594=DIRECTION('ref_axis',(-4.33680868994202E-19,1.,-1.18789542670764E-48));
#40595=DIRECTION('center_axis',(5.15167520928809E-67,-1.18789542670764E-48,
-1.));
#40596=DIRECTION('ref_axis',(-4.33680868994202E-19,1.,-1.18789542670764E-48));
#40597=DIRECTION('center_axis',(5.15167520928809E-67,-1.18789542670764E-48,
-1.));
#40598=DIRECTION('ref_axis',(-4.33680868994202E-19,1.,-1.18789542670764E-48));
#40599=DIRECTION('center_axis',(5.15167520928809E-67,-1.18789542670764E-48,
-1.));
#40600=DIRECTION('ref_axis',(-4.33680868994202E-19,1.,-1.18789542670764E-48));
#40601=DIRECTION('center_axis',(5.15167520928809E-67,-1.18789542670764E-48,
-1.));
#40602=DIRECTION('ref_axis',(-4.33680868994202E-19,1.,-1.18789542670764E-48));
#40603=DIRECTION('center_axis',(5.15167520928809E-67,-1.18789542670764E-48,
-1.));
#40604=DIRECTION('ref_axis',(-4.33680868994202E-19,1.,-1.18789542670764E-48));
#40605=DIRECTION('center_axis',(5.15167520928809E-67,-1.18789542670764E-48,
-1.));
#40606=DIRECTION('ref_axis',(-4.33680868994202E-19,1.,-1.18789542670764E-48));
#40607=DIRECTION('center_axis',(5.15167520928809E-67,-1.18789542670764E-48,
-1.));
#40608=DIRECTION('ref_axis',(-4.33680868994202E-19,1.,-1.18789542670764E-48));
#40609=DIRECTION('center_axis',(-0.271066873422527,0.654413322126802,-0.70587956051716));
#40610=DIRECTION('ref_axis',(-0.270129585578839,0.652147192704003,0.708331875636903));
#40611=DIRECTION('center_axis',(5.15167520928809E-67,-1.18789542670764E-48,
-1.));
#40612=DIRECTION('ref_axis',(-4.33680868994202E-19,1.,-1.18789542670764E-48));
#40613=DIRECTION('center_axis',(-0.218886604216929,0.673663698306674,-0.705879505353539));
#40614=DIRECTION('ref_axis',(-0.218129954131946,0.671330916306808,0.708331930609553));
#40615=DIRECTION('center_axis',(5.15167520928809E-67,-1.18789542670764E-48,
-1.));
#40616=DIRECTION('ref_axis',(-4.33680868994202E-19,1.,-1.18789542670764E-48));
#40617=DIRECTION('center_axis',(-0.16535683118721,0.688760770927084,-0.705879393955974));
#40618=DIRECTION('ref_axis',(-0.164785479532737,0.686375600198312,0.708332041621423));
#40619=DIRECTION('center_axis',(5.15167520928809E-67,-1.18789542670764E-48,
-1.));
#40620=DIRECTION('ref_axis',(-4.33680868994202E-19,1.,-1.18789542670764E-48));
#40621=DIRECTION('center_axis',(-0.110807570905113,0.699611468639715,-0.705879221381313));
#40622=DIRECTION('ref_axis',(-0.110425058151779,0.69718848363325,0.708332213598496));
#40623=DIRECTION('center_axis',(5.15167520928809E-67,-1.18789542670764E-48,
-1.));
#40624=DIRECTION('ref_axis',(-4.33680868994202E-19,1.,-1.18789542670764E-48));
#40625=DIRECTION('center_axis',(-0.0555751238836985,0.706148902304822,-0.705878979272656));
#40626=DIRECTION('ref_axis',(-0.0553838490532064,0.703702893729884,0.708332454868643));
#40627=DIRECTION('center_axis',(5.15167520928809E-67,-1.18789542670764E-48,
-1.));
#40628=DIRECTION('ref_axis',(-4.33680868994202E-19,1.,-1.18789542670764E-48));
#40629=DIRECTION('',(8.69022643068848E-17,-0.707106781186538,-0.707106781186557));
#40630=DIRECTION('center_axis',(5.15167520928809E-67,-1.18789542670764E-48,
-1.));
#40631=DIRECTION('ref_axis',(-4.33680868994202E-19,1.,-1.18789542670764E-48));
#40632=DIRECTION('center_axis',(5.15167520928809E-67,-1.18789542670764E-48,
-1.));
#40633=DIRECTION('ref_axis',(-4.33680868994202E-19,1.,-1.18789542670764E-48));
#40634=DIRECTION('center_axis',(5.15167520928809E-67,-1.18789542670764E-48,
-1.));
#40635=DIRECTION('ref_axis',(0.,1.,0.));
#40636=DIRECTION('center_axis',(5.15167520928809E-67,-1.18789542670764E-48,
-1.));
#40637=DIRECTION('ref_axis',(-4.33680868994202E-19,1.,-1.18789542670764E-48));
#40638=DIRECTION('center_axis',(1.,0.,5.15167520928809E-67));
#40639=DIRECTION('ref_axis',(0.,-1.,0.));
#40640=DIRECTION('center_axis',(5.15167520928809E-67,-1.18789542670764E-48,
-1.));
#40641=DIRECTION('ref_axis',(-4.33680868994202E-19,1.,-1.18789542670764E-48));
#40642=DIRECTION('center_axis',(5.15167520928809E-67,-1.18789542670764E-48,
-1.));
#40643=DIRECTION('ref_axis',(-4.33680868994202E-19,1.,-1.18789542670764E-48));
#40644=DIRECTION('',(-5.15167520928809E-67,1.18789542670764E-48,1.));
#40645=DIRECTION('center_axis',(5.15167520928809E-67,-1.18789542670764E-48,
-1.));
#40646=DIRECTION('ref_axis',(0.,1.,0.));
#40647=DIRECTION('center_axis',(5.15167520928809E-67,-1.18789542670764E-48,
-1.));
#40648=DIRECTION('ref_axis',(-4.33680868994202E-19,1.,-1.18789542670764E-48));
#40649=DIRECTION('center_axis',(-1.,0.,-5.15167520928809E-67));
#40650=DIRECTION('ref_axis',(0.,-1.,0.));
#40651=DIRECTION('center_axis',(5.15167520928809E-67,-1.18789542670764E-48,
-1.));
#40652=DIRECTION('ref_axis',(0.,1.,0.));
#40653=DIRECTION('center_axis',(1.,0.,5.15167520928809E-67));
#40654=DIRECTION('ref_axis',(0.,-1.,0.));
#40655=DIRECTION('center_axis',(5.15167520928809E-67,-1.18789542670764E-48,
-1.));
#40656=DIRECTION('ref_axis',(-4.33680868994202E-19,1.,-1.18789542670764E-48));
#40657=DIRECTION('center_axis',(5.15167520928809E-67,-1.18789542670764E-48,
-1.));
#40658=DIRECTION('ref_axis',(0.,1.,0.));
#40659=DIRECTION('center_axis',(-0.726741019926939,-0.686911553067863,9.06501466507717E-5));
#40660=DIRECTION('ref_axis',(0.686840456252471,-0.726663889286196,0.0144837723800636));
#40661=DIRECTION('center_axis',(5.15167520928809E-67,-1.18789542670764E-48,
-1.));
#40662=DIRECTION('ref_axis',(-4.33680868994202E-19,1.,-1.18789542670764E-48));
#40663=DIRECTION('center_axis',(0.0503838293498797,0.99872992276226,0.000105448247773495));
#40664=DIRECTION('ref_axis',(0.998655285166785,-0.0503813543085061,0.012220496982052));
#40665=DIRECTION('center_axis',(5.15167520928809E-67,-1.18789542670764E-48,
-1.));
#40666=DIRECTION('ref_axis',(0.,1.,0.));
#40667=DIRECTION('center_axis',(-0.0281309337977199,0.999604241409737,0.000105448247664664));
#40668=DIRECTION('ref_axis',(0.999529639708461,0.0281275452111534,0.0122204969076063));
#40669=DIRECTION('center_axis',(-0.670606260601171,-0.741813477246852,9.06501467500846E-5));
#40670=DIRECTION('ref_axis',(0.741736547998884,-0.670534945920291,0.0144837723805249));
#40671=DIRECTION('center_axis',(5.15167520928809E-67,-1.18789542670764E-48,
-1.));
#40672=DIRECTION('ref_axis',(-4.33680868994202E-19,1.,-1.18789542670764E-48));
#40673=DIRECTION('center_axis',(5.15167520928809E-67,-1.18789542670764E-48,
-1.));
#40674=DIRECTION('ref_axis',(0.,1.,0.));
#40675=DIRECTION('center_axis',(-0.106472260383779,0.994315667506771,0.000105448247699395));
#40676=DIRECTION('ref_axis',(0.99424156164256,0.106463029061011,0.0122204969504906));
#40677=DIRECTION('center_axis',(-0.610336990679751,-0.792141874660428,9.06501467512865E-5));
#40678=DIRECTION('ref_axis',(0.792059587274889,-0.610271931637935,0.0144837723275367));
#40679=DIRECTION('center_axis',(5.15167520928809E-67,-1.18789542670764E-48,
-1.));
#40680=DIRECTION('ref_axis',(-4.33680868994202E-19,1.,-1.18789542670764E-48));
#40681=DIRECTION('center_axis',(5.15167520928809E-67,-1.18789542670764E-48,
-1.));
#40682=DIRECTION('ref_axis',(0.,1.,0.));
#40683=DIRECTION('center_axis',(-0.18415715007879,0.982896806870144,0.000105448247763879));
#40684=DIRECTION('ref_axis',(0.982823653730846,0.18414213293402,0.0122204969481005));
#40685=DIRECTION('center_axis',(-0.546304790252955,-0.837586454002944,9.06501468511952E-5));
#40686=DIRECTION('ref_axis',(0.837499315807933,-0.546246387960026,0.0144837723631749));
#40687=DIRECTION('center_axis',(5.15167520928809E-67,-1.18789542670764E-48,
-1.));
#40688=DIRECTION('ref_axis',(-4.33680868994202E-19,1.,-1.18789542670764E-48));
#40689=DIRECTION('center_axis',(5.15167520928809E-67,-1.18789542670764E-48,
-1.));
#40690=DIRECTION('ref_axis',(0.,1.,0.));
#40691=DIRECTION('center_axis',(-0.260706649705391,0.965418060572754,0.000105448247684059));
#40692=DIRECTION('ref_axis',(0.965346311171948,0.260685939324359,0.0122204969329739));
#40693=DIRECTION('center_axis',(-0.478904439129961,-0.877867034330466,9.06501466909999E-5));
#40694=DIRECTION('ref_axis',(0.877775582562065,-0.478853053655646,0.0144837723846339));
#40695=DIRECTION('center_axis',(5.15167520928809E-67,-1.18789542670764E-48,
-1.));
#40696=DIRECTION('ref_axis',(-4.33680868994202E-19,1.,-1.18789542670764E-48));
#40697=DIRECTION('center_axis',(5.15167520928809E-67,-1.18789542670764E-48,
-1.));
#40698=DIRECTION('ref_axis',(0.,1.,0.));
#40699=DIRECTION('center_axis',(-0.33564880614276,0.941987190897842,0.000105448247631265));
#40700=DIRECTION('ref_axis',(0.941917287593993,0.335622530211717,0.0122204969563928));
#40701=DIRECTION('center_axis',(-0.408551482887427,-0.912735272471178,9.06501467675252E-5));
#40702=DIRECTION('ref_axis',(0.91264007095957,-0.408507431040139,0.0144837724331839));
#40703=DIRECTION('center_axis',(5.15167520928809E-67,-1.18789542670764E-48,
-1.));
#40704=DIRECTION('ref_axis',(-4.33680868994202E-19,1.,-1.18789542670764E-48));
#40705=DIRECTION('center_axis',(5.15167520928809E-67,-1.18789542670764E-48,
-1.));
#40706=DIRECTION('ref_axis',(0.,1.,0.));
#40707=DIRECTION('center_axis',(-0.408521576075341,0.912748656948662,0.000105448247753309));
#40708=DIRECTION('ref_axis',(0.912681030719062,0.40848989659417,0.0122204969651243));
#40709=DIRECTION('center_axis',(-0.335679670896088,-0.941976194141681,9.06501466394305E-5));
#40710=DIRECTION('ref_axis',(0.941877829837658,-0.335643224270894,0.0144837723450194));
#40711=DIRECTION('center_axis',(5.15167520928809E-67,-1.18789542670764E-48,
-1.));
#40712=DIRECTION('ref_axis',(-4.33680868994202E-19,1.,-1.18789542670764E-48));
#40713=DIRECTION('center_axis',(5.15167520928809E-67,-1.18789542670764E-48,
-1.));
#40714=DIRECTION('ref_axis',(0.,1.,0.));
#40715=DIRECTION('center_axis',(-0.478875674645407,0.877882724009063,0.000105448247283112));
#40716=DIRECTION('ref_axis',(0.877817791790398,0.478838786927794,0.012220497115417));
#40717=DIRECTION('center_axis',(-0.260738282108194,-0.965409519336649,9.06501468435925E-5));
#40718=DIRECTION('ref_axis',(0.965308598687812,-0.260709665410158,0.0144837723364994));
#40719=DIRECTION('center_axis',(5.15167520928809E-67,-1.18789542670764E-48,
-1.));
#40720=DIRECTION('ref_axis',(-4.33680868994202E-19,1.,-1.18789542670764E-48));
#40721=DIRECTION('center_axis',(5.15167520928809E-67,-1.18789542670764E-48,
-1.));
#40722=DIRECTION('ref_axis',(0.,1.,0.));
#40723=DIRECTION('center_axis',(-0.546277345437336,0.837604352151184,0.000105448247639474));
#40724=DIRECTION('ref_axis',(0.837542514276272,0.546235476910692,0.0122204968773897));
#40725=DIRECTION('center_axis',(-0.184189355107295,-0.982890773813505,9.06501468099581E-5));
#40726=DIRECTION('ref_axis',(0.982787919029019,-0.184168744767822,0.0144837723419927));
#40727=DIRECTION('center_axis',(5.15167520928809E-67,-1.18789542670764E-48,
-1.));
#40728=DIRECTION('ref_axis',(-4.33680868994202E-19,1.,-1.18789542670764E-48));
#40729=DIRECTION('center_axis',(5.15167520928809E-67,-1.18789542670764E-48,
-1.));
#40730=DIRECTION('ref_axis',(0.,1.,0.));
#40731=DIRECTION('center_axis',(-0.610311034740724,0.792161870929404,0.000105448247072483));
#40732=DIRECTION('ref_axis',(0.792103508642798,0.610264443533926,0.0122204972891987));
#40733=DIRECTION('center_axis',(-0.106504839483277,-0.994312179825427,9.06501466463657E-5));
#40734=DIRECTION('ref_axis',(0.994208025037708,-0.106492362571804,0.014483772453865));
#40735=DIRECTION('center_axis',(5.15167520928809E-67,-1.18789542670764E-48,
-1.));
#40736=DIRECTION('ref_axis',(-4.33680868994202E-19,1.,-1.18789542670764E-48));
#40737=DIRECTION('center_axis',(5.15167520928809E-67,-1.18789542670764E-48,
-1.));
#40738=DIRECTION('ref_axis',(0.,1.,0.));
#40739=DIRECTION('center_axis',(-0.670581953563772,0.74183544835446,0.000105448247723866));
#40740=DIRECTION('ref_axis',(0.741780921486778,0.670530926933108,0.012220496898794));
#40741=DIRECTION('center_axis',(-0.0281636861068304,-0.999603320606443,
9.06501467794172E-5));
#40742=DIRECTION('ref_axis',(0.999498507966719,-0.0281594195479949,0.0144837724030356));
#40743=DIRECTION('center_axis',(5.15167520928809E-67,-1.18789542670764E-48,
-1.));
#40744=DIRECTION('ref_axis',(-4.33680868994202E-19,1.,-1.18789542670764E-48));
#40745=DIRECTION('center_axis',(5.15167520928809E-67,-1.18789542670764E-48,
-1.));
#40746=DIRECTION('ref_axis',(0.,1.,0.));
#40747=DIRECTION('center_axis',(-0.726718511653027,0.686935363554299,0.000105448247728815));
#40748=DIRECTION('ref_axis',(0.686885008277766,0.726663364191397,0.0122204969332444));
#40749=DIRECTION('center_axis',(0.050351105759542,-0.998731574514065,9.06501467573609E-5));
#40750=DIRECTION('ref_axis',(0.998626750226961,0.0503471356610921,0.014483772362966));
#40751=DIRECTION('center_axis',(5.15167520928809E-67,-1.18789542670764E-48,
-1.));
#40752=DIRECTION('ref_axis',(-4.33680868994202E-19,1.,-1.18789542670764E-48));
#40753=DIRECTION('center_axis',(5.15167520928809E-67,-1.18789542670764E-48,
-1.));
#40754=DIRECTION('ref_axis',(0.,1.,0.));
#40755=DIRECTION('center_axis',(-0.778374608459537,0.627800093808634,0.000105448247783041));
#40756=DIRECTION('ref_axis',(0.627754220580437,0.778315680169477,0.01222049695274));
#40757=DIRECTION('center_axis',(0.128555466315269,-0.991702316152894,9.06501465984867E-5));
#40758=DIRECTION('ref_axis',(0.99159812649388,0.128543284036463,0.0144837724004731));
#40759=DIRECTION('center_axis',(5.15167520928809E-67,-1.18789542670764E-48,
-1.));
#40760=DIRECTION('ref_axis',(-4.33680868994202E-19,1.,-1.18789542670764E-48));
#40761=DIRECTION('center_axis',(5.15167520928809E-67,-1.18789542670764E-48,
-1.));
#40762=DIRECTION('ref_axis',(0.,1.,0.));
#40763=DIRECTION('center_axis',(-0.825231766969855,0.564794227718802,0.000105448247237627));
#40764=DIRECTION('ref_axis',(0.564753119361559,0.825169421162197,0.0122204971352771));
#40765=DIRECTION('center_axis',(0.205967239672467,-0.97855888323813,9.06501466256469E-5));
#40766=DIRECTION('ref_axis',(0.978455970572454,0.205946920321296,0.0144837723432324));
#40767=DIRECTION('center_axis',(5.15167520928809E-67,-1.18789542670764E-48,
-1.));
#40768=DIRECTION('ref_axis',(-4.33680868994202E-19,1.,-1.18789542670764E-48));
#40769=DIRECTION('center_axis',(5.15167520928809E-67,-1.18789542670764E-48,
-1.));
#40770=DIRECTION('ref_axis',(0.,1.,0.));
#40771=DIRECTION('center_axis',(-0.867001097222074,0.498306217396881,0.00010544824406792));
#40772=DIRECTION('ref_axis',(0.498270127350421,0.866935718266621,0.0122204985059196));
#40773=DIRECTION('center_axis',(0.282109156506117,-0.959382309404316,9.06501467341775E-5));
#40774=DIRECTION('ref_axis',(0.959281308220891,0.282080825357731,0.0144837724201092));
#40775=DIRECTION('center_axis',(5.15167520928809E-67,-1.18789542670764E-48,
-1.));
#40776=DIRECTION('ref_axis',(-4.33680868994202E-19,1.,-1.18789542670764E-48));
#40777=DIRECTION('center_axis',(5.15167520928809E-67,-1.18789542670764E-48,
-1.));
#40778=DIRECTION('ref_axis',(0.,1.,0.));
#40779=DIRECTION('center_axis',(-0.903425077395399,0.428745983554114,0.00010544824771057));
#40780=DIRECTION('ref_axis',(0.42871513434286,0.903357068405985,0.0122204969754959));
#40781=DIRECTION('center_axis',(0.356511776578972,-0.934290824606052,9.06501467185522E-5));
#40782=DIRECTION('ref_axis',(0.934192357612503,0.356475608304786,0.0144837723720686));
#40783=DIRECTION('center_axis',(5.15167520928809E-67,-1.18789542670764E-48,
-1.));
#40784=DIRECTION('ref_axis',(-4.33680868994202E-19,1.,-1.18789542670764E-48));
#40785=DIRECTION('center_axis',(5.15167520928809E-67,-1.18789542670764E-48,
-1.));
#40786=DIRECTION('ref_axis',(0.,1.,0.));
#40787=DIRECTION('center_axis',(-0.934279141551227,0.35654238814336,0.000105448247725771));
#40788=DIRECTION('ref_axis',(0.356516969954114,0.934208921810617,0.0122204968876431));
#40789=DIRECTION('center_axis',(0.428716382996855,-0.903439126190938,9.06501466905075E-5));
#40790=DIRECTION('ref_axis',(0.903343800467886,0.428672600585895,0.0144837724078269));
#40791=DIRECTION('center_axis',(5.15167520928809E-67,-1.18789542670764E-48,
-1.));
#40792=DIRECTION('ref_axis',(-4.33680868994202E-19,1.,-1.18789542670764E-48));
#40793=DIRECTION('center_axis',(5.15167520928809E-67,-1.18789542670764E-48,
-1.));
#40794=DIRECTION('ref_axis',(0.,1.,0.));
#40795=DIRECTION('center_axis',(-0.959373064120116,0.282140590347166,0.000105448247704078));
#40796=DIRECTION('ref_axis',(0.282120759890668,0.959301066553995,0.0122204970062476));
#40797=DIRECTION('center_axis',(0.498277810351468,-0.867017425138559,9.06501469271671E-5));
#40798=DIRECTION('ref_axis',(0.86692582840188,0.498226683737388,0.0144837723593644));
#40799=DIRECTION('center_axis',(5.15167520928809E-67,-1.18789542670764E-48,
-1.));
#40800=DIRECTION('ref_axis',(-4.33680868994202E-19,1.,-1.18789542670764E-48));
#40801=DIRECTION('center_axis',(5.15167520928809E-67,-1.18789542670764E-48,
-1.));
#40802=DIRECTION('ref_axis',(0.,1.,0.));
#40803=DIRECTION('center_axis',(-0.978552132724721,0.205999301990486,0.000105448247790145));
#40804=DIRECTION('ref_axis',(0.205985181528783,0.978478801224291,0.0122204969305395));
#40805=DIRECTION('center_axis',(0.564767189310343,-0.825250273348059,9.06501467424166E-5));
#40806=DIRECTION('ref_axis',(0.825162970321744,0.56470903370561,0.0144837723356968));
#40807=DIRECTION('center_axis',(5.15167520928809E-67,-1.18789542670764E-48,
-1.));
#40808=DIRECTION('ref_axis',(-4.33680868994202E-19,1.,-1.18789542670764E-48));
#40809=DIRECTION('center_axis',(5.15167520928809E-67,-1.18789542670764E-48,
-1.));
#40810=DIRECTION('ref_axis',(0.,1.,0.));
#40811=DIRECTION('center_axis',(-0.991698102029505,0.128587959435343,0.000105448247905715));
#40812=DIRECTION('ref_axis',(0.12857963602553,0.991623888707005,0.0122204969268892));
#40813=DIRECTION('center_axis',(0.627774590743107,-0.778395179198763,9.06501466692162E-5));
#40814=DIRECTION('ref_axis',(0.778312708134479,0.627709764696018,0.0144837723553914));
#40815=DIRECTION('center_axis',(5.15167520928809E-67,-1.18789542670764E-48,
-1.));
#40816=DIRECTION('ref_axis',(-4.33680868994202E-19,1.,-1.18789542670764E-48));
#40817=DIRECTION('center_axis',(5.15167520928809E-67,-1.18789542670764E-48,
-1.));
#40818=DIRECTION('ref_axis',(0.,1.,0.));
#40819=DIRECTION('center_axis',(-0.998729922762266,0.05038382934976,0.000105448247701369));
#40820=DIRECTION('ref_axis',(0.0503813543083786,0.998655285166624,0.0122204969957313));
#40821=DIRECTION('center_axis',(0.686911553067687,-0.726741019927105,9.06501465529425E-5));
#40822=DIRECTION('ref_axis',(0.726663889286156,0.686840456252101,0.0144837723995786));
#40823=DIRECTION('center_axis',(5.15167520928809E-67,-1.18789542670764E-48,
-1.));
#40824=DIRECTION('ref_axis',(-4.33680868994202E-19,1.,-1.18789542670764E-48));
#40825=DIRECTION('center_axis',(5.15167520928809E-67,-1.18789542670764E-48,
-1.));
#40826=DIRECTION('ref_axis',(0.,1.,0.));
#40827=DIRECTION('center_axis',(-0.999604241409733,-0.0281309337978441,
0.000105448247608528));
#40828=DIRECTION('ref_axis',(0.0281275452112647,-0.999529639708088,-0.0122204969378127));
#40829=DIRECTION('center_axis',(0.741813477246663,-0.67060626060138,9.06501466416355E-5));
#40830=DIRECTION('ref_axis',(0.670534945920398,0.741736547998582,0.0144837723910712));
#40831=DIRECTION('center_axis',(5.15167520928809E-67,-1.18789542670764E-48,
-1.));
#40832=DIRECTION('ref_axis',(-4.33680868994202E-19,1.,-1.18789542670764E-48));
#40833=DIRECTION('center_axis',(5.15167520928809E-67,-1.18789542670764E-48,
-1.));
#40834=DIRECTION('ref_axis',(0.,1.,0.));
#40835=DIRECTION('center_axis',(-0.994315667506803,-0.106472260383486,0.000105448247832577));
#40836=DIRECTION('ref_axis',(0.10646302906079,-0.994241561643227,-0.0122204968981425));
#40837=DIRECTION('center_axis',(0.792141874660394,-0.610336990679795,9.06501467163515E-5));
#40838=DIRECTION('ref_axis',(0.610271931637984,0.792059587274861,0.0144837723269713));
#40839=DIRECTION('center_axis',(5.15167520928809E-67,-1.18789542670764E-48,
-1.));
#40840=DIRECTION('ref_axis',(-4.33680868994202E-19,1.,-1.18789542670764E-48));
#40841=DIRECTION('center_axis',(5.15167520928809E-67,-1.18789542670764E-48,
-1.));
#40842=DIRECTION('ref_axis',(0.,1.,0.));
#40843=DIRECTION('center_axis',(-0.982896806870098,-0.184157150079038,0.000105448247610839));
#40844=DIRECTION('ref_axis',(0.184142132934261,-0.982823653730751,-0.0122204969521754));
#40845=DIRECTION('center_axis',(0.837586454002892,-0.546304790253034,9.06501468389122E-5));
#40846=DIRECTION('ref_axis',(0.546246387959946,0.837499315807641,0.014483772383082));
#40847=DIRECTION('center_axis',(5.15167520928809E-67,-1.18789542670764E-48,
-1.));
#40848=DIRECTION('ref_axis',(-4.33680868994202E-19,1.,-1.18789542670764E-48));
#40849=DIRECTION('center_axis',(5.15167520928809E-67,-1.18789542670764E-48,
-1.));
#40850=DIRECTION('ref_axis',(0.,1.,0.));
#40851=DIRECTION('center_axis',(-0.965418060572767,-0.260706649705342,0.000105448247695262));
#40852=DIRECTION('ref_axis',(0.260685939324476,-0.965346311172558,-0.0122204968822783));
#40853=DIRECTION('center_axis',(0.877867034330398,-0.478904439130086,9.06501466177592E-5));
#40854=DIRECTION('ref_axis',(0.478853053655353,0.877775582561241,0.0144837724443041));
#40855=DIRECTION('center_axis',(5.15167520928809E-67,-1.18789542670764E-48,
-1.));
#40856=DIRECTION('ref_axis',(-4.33680868994202E-19,1.,-1.18789542670764E-48));
#40857=DIRECTION('center_axis',(5.15167520928809E-67,-1.18789542670764E-48,
-1.));
#40858=DIRECTION('ref_axis',(0.,1.,0.));
#40859=DIRECTION('center_axis',(-0.941987190897914,-0.335648806142557,0.000105448247712849));
#40860=DIRECTION('ref_axis',(0.335622530211483,-0.941917287593983,-0.0122204969636003));
#40861=DIRECTION('center_axis',(0.912735272471151,-0.408551482887487,9.06501467033935E-5));
#40862=DIRECTION('ref_axis',(0.408507431040848,0.912640070960968,0.0144837723251257));
#40863=DIRECTION('center_axis',(5.15167520928809E-67,-1.18789542670764E-48,
-1.));
#40864=DIRECTION('ref_axis',(-4.33680868994202E-19,1.,-1.18789542670764E-48));
#40865=DIRECTION('center_axis',(5.15167520928809E-67,-1.18789542670764E-48,
-1.));
#40866=DIRECTION('ref_axis',(0.,1.,0.));
#40867=DIRECTION('center_axis',(-0.912748656948201,-0.408521576076371,0.000105448247247158));
#40868=DIRECTION('ref_axis',(0.408489896594259,-0.912681030716532,-0.012220497151094));
#40869=DIRECTION('center_axis',(0.941976194141716,-0.335679670895989,9.06501466623777E-5));
#40870=DIRECTION('ref_axis',(0.335643224270751,0.941877829837572,0.0144837723539316));
#40871=DIRECTION('center_axis',(5.15167520928809E-67,-1.18789542670764E-48,
-1.));
#40872=DIRECTION('ref_axis',(-4.33680868994202E-19,1.,-1.18789542670764E-48));
#40873=DIRECTION('center_axis',(5.15167520928809E-67,-1.18789542670764E-48,
-1.));
#40874=DIRECTION('ref_axis',(0.,1.,0.));
#40875=DIRECTION('center_axis',(-0.877882724009451,-0.478875674644697,0.000105448247674909));
#40876=DIRECTION('ref_axis',(0.478838786928496,-0.877817791793333,-0.0122204968770904));
#40877=DIRECTION('center_axis',(0.965409519336493,-0.26073828210877,9.06501465579451E-5));
#40878=DIRECTION('ref_axis',(0.260709665410522,0.965308598686875,0.0144837723924504));
#40879=DIRECTION('center_axis',(5.15167520928809E-67,-1.18789542670764E-48,
-1.));
#40880=DIRECTION('ref_axis',(-4.33680868994202E-19,1.,-1.18789542670764E-48));
#40881=DIRECTION('center_axis',(5.15167520928809E-67,-1.18789542670764E-48,
-1.));
#40882=DIRECTION('ref_axis',(0.,1.,0.));
#40883=DIRECTION('center_axis',(-0.837604352151306,-0.546277345437149,0.00010544824776483));
#40884=DIRECTION('ref_axis',(0.546235476910197,-0.837542514275933,-0.0122204969227218));
#40885=DIRECTION('center_axis',(0.982890773813463,-0.184189355107518,9.06501466980053E-5));
#40886=DIRECTION('ref_axis',(0.184168744767822,0.982787919027818,0.0144837724235038));
#40887=DIRECTION('center_axis',(5.15167520928809E-67,-1.18789542670764E-48,
-1.));
#40888=DIRECTION('ref_axis',(-4.33680868994202E-19,1.,-1.18789542670764E-48));
#40889=DIRECTION('center_axis',(5.15167520928809E-67,-1.18789542670764E-48,
-1.));
#40890=DIRECTION('ref_axis',(0.,1.,0.));
#40891=DIRECTION('center_axis',(-0.792161870930109,-0.610311034739809,0.000105448247597277));
#40892=DIRECTION('ref_axis',(0.610264443535208,-0.792103508646315,-0.0122204969972532));
#40893=DIRECTION('center_axis',(0.994312179825469,-0.106504839482882,9.06501468290203E-5));
#40894=DIRECTION('ref_axis',(0.106492362571566,0.994208025039157,0.0144837723561435));
#40895=DIRECTION('center_axis',(5.15167520928809E-67,-1.18789542670764E-48,
-1.));
#40896=DIRECTION('ref_axis',(-4.33680868994202E-19,1.,-1.18789542670764E-48));
#40897=DIRECTION('center_axis',(5.15167520928809E-67,-1.18789542670764E-48,
-1.));
#40898=DIRECTION('ref_axis',(0.,1.,0.));
#40899=DIRECTION('center_axis',(-0.741835448354634,-0.670581953563579,0.000105448247853962));
#40900=DIRECTION('ref_axis',(0.67053092693267,-0.741780921486687,-0.0122204969283275));
#40901=DIRECTION('center_axis',(0.99960332060645,-0.0281636861065795,9.06501468718404E-5));
#40902=DIRECTION('ref_axis',(0.0281594195477731,0.999498507967606,0.014483772342229));
#40903=DIRECTION('center_axis',(5.15167520928809E-67,-1.18789542670764E-48,
-1.));
#40904=DIRECTION('ref_axis',(-4.33680868994202E-19,1.,-1.18789542670764E-48));
#40905=DIRECTION('center_axis',(5.15167520928809E-67,-1.18789542670764E-48,
-1.));
#40906=DIRECTION('ref_axis',(0.,1.,0.));
#40907=DIRECTION('center_axis',(-0.686935363552547,-0.726718511654683,0.000105448246665782));
#40908=DIRECTION('ref_axis',(0.726663364188996,-0.686885008272227,-0.0122204973873402));
#40909=DIRECTION('center_axis',(0.998731574514055,0.0503511057597249,9.06501467982717E-5));
#40910=DIRECTION('ref_axis',(0.050347135661256,-0.998626750226507,-0.0144837723936806));
#40911=DIRECTION('center_axis',(5.15167520928809E-67,-1.18789542670764E-48,
-1.));
#40912=DIRECTION('ref_axis',(-4.33680868994202E-19,1.,-1.18789542670764E-48));
#40913=DIRECTION('center_axis',(5.15167520928809E-67,-1.18789542670764E-48,
-1.));
#40914=DIRECTION('ref_axis',(0.,1.,0.));
#40915=DIRECTION('center_axis',(-0.627800093808639,-0.778374608459533,0.000105448247779514));
#40916=DIRECTION('ref_axis',(0.778315680170178,-0.627754220581,-0.0122204968791585));
#40917=DIRECTION('center_axis',(0.991702316152886,0.12855546631533,9.06501466251883E-5));
#40918=DIRECTION('ref_axis',(0.128543284036466,-0.991598126493403,-0.0144837724330683));
#40919=DIRECTION('center_axis',(5.15167520928809E-67,-1.18789542670764E-48,
-1.));
#40920=DIRECTION('ref_axis',(-4.33680868994202E-19,1.,-1.18789542670764E-48));
#40921=DIRECTION('center_axis',(5.15167520928809E-67,-1.18789542670764E-48,
-1.));
#40922=DIRECTION('ref_axis',(0.,1.,0.));
#40923=DIRECTION('center_axis',(-0.564794227719968,-0.825231766969057,0.000105448247863909));
#40924=DIRECTION('ref_axis',(0.825169421163414,-0.564753119364088,-0.0122204969362205));
#40925=DIRECTION('center_axis',(0.978558883238036,0.205967239672914,9.06501468463484E-5));
#40926=DIRECTION('ref_axis',(0.205946920321936,-0.978455970573291,-0.014483772277592));
#40927=DIRECTION('center_axis',(5.15167520928809E-67,-1.18789542670764E-48,
-1.));
#40928=DIRECTION('ref_axis',(-4.33680868994202E-19,1.,-1.18789542670764E-48));
#40929=DIRECTION('center_axis',(5.15167520928809E-67,-1.18789542670764E-48,
-1.));
#40930=DIRECTION('ref_axis',(0.,1.,0.));
#40931=DIRECTION('center_axis',(-0.498306217403848,-0.86700109721807,0.000105448247661773));
#40932=DIRECTION('ref_axis',(0.866935718279092,-0.498270127366718,-0.0122204969566953));
#40933=DIRECTION('center_axis',(0.959382309404258,0.282109156506314,9.06501467982869E-5));
#40934=DIRECTION('ref_axis',(0.282080825358155,-0.959281308221622,-0.014483772363392));
#40935=DIRECTION('center_axis',(5.15167520928809E-67,-1.18789542670764E-48,
-1.));
#40936=DIRECTION('ref_axis',(-4.33680868994202E-19,1.,-1.18789542670764E-48));
#40937=DIRECTION('center_axis',(5.15167520928809E-67,-1.18789542670764E-48,
-1.));
#40938=DIRECTION('ref_axis',(0.,1.,0.));
#40939=DIRECTION('center_axis',(-0.428745983554159,-0.903425077395378,0.000105448247692435));
#40940=DIRECTION('ref_axis',(0.903357068405516,-0.428715134342697,-0.0122204970158381));
#40941=DIRECTION('center_axis',(0.934290824605943,0.356511776579256,9.06501468588022E-5));
#40942=DIRECTION('ref_axis',(0.35647560830508,-0.934192357612417,-0.0144837723703894));
#40943=DIRECTION('center_axis',(5.15167520928809E-67,-1.18789542670764E-48,
-1.));
#40944=DIRECTION('ref_axis',(-4.33680868994202E-19,1.,-1.18789542670764E-48));
#40945=DIRECTION('center_axis',(5.15167520928809E-67,-1.18789542670764E-48,
-1.));
#40946=DIRECTION('ref_axis',(0.,1.,0.));
#40947=DIRECTION('center_axis',(-0.356542388142294,-0.934279141551633,0.000105448247232403));
#40948=DIRECTION('ref_axis',(0.934208921807365,-0.356516969951681,-0.0122204972072322));
#40949=DIRECTION('center_axis',(0.903439126190767,0.428716382997215,9.06501468179925E-5));
#40950=DIRECTION('ref_axis',(0.428672600586429,-0.903343800468082,-0.0144837723797852));
#40951=DIRECTION('center_axis',(5.15167520928809E-67,-1.18789542670764E-48,
-1.));
#40952=DIRECTION('ref_axis',(-4.33680868994202E-19,1.,-1.18789542670764E-48));
#40953=DIRECTION('center_axis',(5.15167520928809E-67,-1.18789542670764E-48,
-1.));
#40954=DIRECTION('ref_axis',(0.,1.,0.));
#40955=DIRECTION('center_axis',(-0.282140590347279,-0.959373064120083,0.000105448247741099));
#40956=DIRECTION('ref_axis',(0.959301066555032,-0.282120759891086,-0.012220496915153));
#40957=DIRECTION('center_axis',(0.867017425138588,0.498277810351419,9.06501468672452E-5));
#40958=DIRECTION('ref_axis',(0.498226683737162,-0.866925828401598,-0.0144837723840689));
#40959=DIRECTION('center_axis',(5.15167520928809E-67,-1.18789542670764E-48,
-1.));
#40960=DIRECTION('ref_axis',(-4.33680868994202E-19,1.,-1.18789542670764E-48));
#40961=DIRECTION('center_axis',(5.15167520928809E-67,-1.18789542670764E-48,
-1.));
#40962=DIRECTION('ref_axis',(0.,1.,0.));
#40963=DIRECTION('center_axis',(-0.20599930198994,-0.978552132724836,0.000105448247552452));
#40964=DIRECTION('ref_axis',(0.97847880122346,-0.205985181528044,-0.0122204970095074));
#40965=DIRECTION('center_axis',(0.825250273348004,0.564767189310424,9.06501467639861E-5));
#40966=DIRECTION('ref_axis',(0.56470903370563,-0.825162970321598,-0.0144837723432248));
#40967=DIRECTION('center_axis',(5.15167520928809E-67,-1.18789542670764E-48,
-1.));
#40968=DIRECTION('ref_axis',(-4.33680868994202E-19,1.,-1.18789542670764E-48));
#40969=DIRECTION('center_axis',(5.15167520928809E-67,-1.18789542670764E-48,
-1.));
#40970=DIRECTION('ref_axis',(0.,1.,0.));
#40971=DIRECTION('center_axis',(-0.128587959431095,-0.991698102030056,0.000105448246015545));
#40972=DIRECTION('ref_axis',(0.991623888697772,-0.128579636020076,-0.0122204977334817));
#40973=DIRECTION('center_axis',(0.778395179198649,0.627774590743249,9.06501467187627E-5));
#40974=DIRECTION('ref_axis',(0.62770976469618,-0.778312708134389,-0.0144837723532511));
#40975=DIRECTION('center_axis',(5.15167520928809E-67,-1.18789542670764E-48,
-1.));
#40976=DIRECTION('ref_axis',(-4.33680868994202E-19,1.,-1.18789542670764E-48));
#40977=DIRECTION('center_axis',(5.15167520928809E-67,-1.18789542670764E-48,
-1.));
#40978=DIRECTION('ref_axis',(0.,1.,0.));
#40979=DIRECTION('center_axis',(-0.0503838293498799,-0.99872992276226,0.000105448247790322));
#40980=DIRECTION('ref_axis',(0.998655285167012,-0.050381354308516,-0.0122204969634886));
#40981=DIRECTION('center_axis',(0.726741019926698,0.686911553068118,9.06501468063716E-5));
#40982=DIRECTION('ref_axis',(0.686840456253071,-0.726663889286322,-0.0144837723452766));
#40983=DIRECTION('center_axis',(5.15167520928809E-67,-1.18789542670764E-48,
-1.));
#40984=DIRECTION('ref_axis',(-4.33680868994202E-19,1.,-1.18789542670764E-48));
#40985=DIRECTION('center_axis',(5.15167520928809E-67,-1.18789542670764E-48,
-1.));
#40986=DIRECTION('ref_axis',(0.,1.,0.));
#40987=DIRECTION('center_axis',(0.0281309337977714,-0.999604241409735,0.000105448247661813));
#40988=DIRECTION('ref_axis',(0.999529639707556,0.0281275452111717,-0.0122204969816086));
#40989=DIRECTION('center_axis',(0.670606260601294,0.741813477246741,9.06501466782892E-5));
#40990=DIRECTION('ref_axis',(0.741736547997904,-0.67053494591962,-0.0144837724617815));
#40991=DIRECTION('center_axis',(5.15167520928809E-67,-1.18789542670764E-48,
-1.));
#40992=DIRECTION('ref_axis',(-4.33680868994202E-19,1.,-1.18789542670764E-48));
#40993=DIRECTION('center_axis',(5.15167520928809E-67,-1.18789542670764E-48,
-1.));
#40994=DIRECTION('ref_axis',(0.,1.,0.));
#40995=DIRECTION('center_axis',(0.106472260384112,-0.994315667506736,0.000105448247531298));
#40996=DIRECTION('ref_axis',(0.994241561642015,0.106463029061287,-0.01222049699245));
#40997=DIRECTION('center_axis',(0.610336990679746,0.792141874660432,9.06501467541659E-5));
#40998=DIRECTION('ref_axis',(0.792059587274579,-0.610271931637685,-0.0144837723550388));
#40999=DIRECTION('center_axis',(5.15167520928809E-67,-1.18789542670764E-48,
-1.));
#41000=DIRECTION('ref_axis',(-4.33680868994202E-19,1.,-1.18789542670764E-48));
#41001=DIRECTION('center_axis',(5.15167520928809E-67,-1.18789542670764E-48,
-1.));
#41002=DIRECTION('ref_axis',(0.,1.,0.));
#41003=DIRECTION('center_axis',(0.184157150078655,-0.982896806870169,0.000105448247826086));
#41004=DIRECTION('ref_axis',(0.982823653731041,0.184142132933918,-0.01222049693405));
#41005=DIRECTION('center_axis',(0.546304790253063,0.837586454002874,9.06501468026834E-5));
#41006=DIRECTION('ref_axis',(0.837499315807096,-0.546246387959628,-0.0144837724265968));
#41007=DIRECTION('center_axis',(5.15167520928809E-67,-1.18789542670764E-48,
-1.));
#41008=DIRECTION('ref_axis',(-4.33680868994202E-19,1.,-1.18789542670764E-48));
#41009=DIRECTION('center_axis',(5.15167520928809E-67,-1.18789542670764E-48,
-1.));
#41010=DIRECTION('ref_axis',(0.,1.,0.));
#41011=DIRECTION('center_axis',(0.260706649723291,-0.965418060567921,0.000105448239312411));
#41012=DIRECTION('ref_axis',(0.965346311124436,0.260685939330442,-0.0122205005564138));
#41013=DIRECTION('center_axis',(0.478904439129984,0.877867034330454,9.06501466836614E-5));
#41014=DIRECTION('ref_axis',(0.877775582561938,-0.478853053655605,-0.0144837723936657));
#41015=DIRECTION('center_axis',(5.15167520928809E-67,-1.18789542670764E-48,
-1.));
#41016=DIRECTION('ref_axis',(-4.33680868994202E-19,1.,-1.18789542670764E-48));
#41017=DIRECTION('center_axis',(5.15167520928809E-67,-1.18789542670764E-48,
-1.));
#41018=DIRECTION('ref_axis',(0.,1.,0.));
#41019=DIRECTION('center_axis',(0.335648806142683,-0.941987190897869,0.000105448247681778));
#41020=DIRECTION('ref_axis',(0.941917287594608,0.335622530211854,-0.012220496905163));
#41021=DIRECTION('center_axis',(0.408551482887321,0.912735272471225,9.06501468104788E-5));
#41022=DIRECTION('ref_axis',(0.912640070960436,-0.408507431040405,-0.014483772371131));
#41023=DIRECTION('center_axis',(5.15167520928809E-67,-1.18789542670764E-48,
-1.));
#41024=DIRECTION('ref_axis',(-4.33680868994202E-19,1.,-1.18789542670764E-48));
#41025=DIRECTION('center_axis',(5.15167520928809E-67,-1.18789542670764E-48,
-1.));
#41026=DIRECTION('ref_axis',(0.,1.,0.));
#41027=DIRECTION('center_axis',(0.408521576076219,-0.912748656948269,0.000105448247344423));
#41028=DIRECTION('ref_axis',(0.912681030717311,0.408489896594431,-0.0122204970871443));
#41029=DIRECTION('center_axis',(0.335679670895796,0.941976194141785,9.06501467685389E-5));
#41030=DIRECTION('ref_axis',(0.941877829836932,-0.335643224270299,-0.0144837724059784));
#41031=DIRECTION('center_axis',(5.15167520928809E-67,-1.18789542670764E-48,
-1.));
#41032=DIRECTION('ref_axis',(-4.33680868994202E-19,1.,-1.18789542670764E-48));
#41033=DIRECTION('center_axis',(5.15167520928809E-67,-1.18789542670764E-48,
-1.));
#41034=DIRECTION('ref_axis',(0.,1.,0.));
#41035=DIRECTION('center_axis',(0.478875674644822,-0.877882724009383,0.000105448247602163));
#41036=DIRECTION('ref_axis',(0.877817791792273,0.47883878692807,-0.0122204969699355));
#41037=DIRECTION('center_axis',(0.260738282108074,0.965409519336681,9.06501468936573E-5));
#41038=DIRECTION('ref_axis',(0.965308598687316,-0.260709665409891,-0.0144837723743816));
#41039=DIRECTION('center_axis',(5.15167520928809E-67,-1.18789542670764E-48,
-1.));
#41040=DIRECTION('ref_axis',(-4.33680868994202E-19,1.,-1.18789542670764E-48));
#41041=DIRECTION('center_axis',(5.15167520928809E-67,-1.18789542670764E-48,
-1.));
#41042=DIRECTION('ref_axis',(0.,1.,0.));
#41043=DIRECTION('center_axis',(0.546277345437349,-0.837604352151176,0.000105448247639465));
#41044=DIRECTION('ref_axis',(0.837542514275712,0.546235476910338,-0.0122204969316073));
#41045=DIRECTION('center_axis',(0.184189355107516,0.982890773813463,9.06501467024073E-5));
#41046=DIRECTION('ref_axis',(0.982787919028468,-0.184168744767946,-0.0144837723778112));
#41047=DIRECTION('center_axis',(5.15167520928809E-67,-1.18789542670764E-48,
-1.));
#41048=DIRECTION('ref_axis',(-4.33680868994202E-19,1.,-1.18789542670764E-48));
#41049=DIRECTION('center_axis',(5.15167520928809E-67,-1.18789542670764E-48,
-1.));
#41050=DIRECTION('ref_axis',(0.,1.,0.));
#41051=DIRECTION('center_axis',(0.610311034750668,-0.792161870921744,0.000105448241406271));
#41052=DIRECTION('ref_axis',(0.79210350861157,0.610264443525473,-0.0122204997355093));
#41053=DIRECTION('center_axis',(0.106504839483129,0.994312179825443,9.06501467375791E-5));
#41054=DIRECTION('ref_axis',(0.994208025038601,-0.106492362571754,-0.0144837723929676));
#41055=DIRECTION('center_axis',(5.15167520928809E-67,-1.18789542670764E-48,
-1.));
#41056=DIRECTION('ref_axis',(-4.33680868994202E-19,1.,-1.18789542670764E-48));
#41057=DIRECTION('center_axis',(5.15167520928809E-67,-1.18789542670764E-48,
-1.));
#41058=DIRECTION('ref_axis',(0.,1.,0.));
#41059=DIRECTION('center_axis',(0.670581953563674,-0.741835448354548,0.000105448247759945));
#41060=DIRECTION('ref_axis',(0.741780921486581,0.670530926932748,-0.0122204969305506));
#41061=DIRECTION('center_axis',(0.0281636861069903,0.999603320606438,9.06501466992701E-5));
#41062=DIRECTION('ref_axis',(0.999498507967367,-0.0281594195481785,-0.0144837723579484));
#41063=DIRECTION('center_axis',(5.15167520928809E-67,-1.18789542670764E-48,
-1.));
#41064=DIRECTION('ref_axis',(-4.33680868994202E-19,1.,-1.18789542670764E-48));
#41065=DIRECTION('center_axis',(5.15167520928809E-67,-1.18789542670764E-48,
-1.));
#41066=DIRECTION('ref_axis',(0.,1.,0.));
#41067=DIRECTION('center_axis',(0.726718511653026,-0.6869353635543,0.000105448247761845));
#41068=DIRECTION('ref_axis',(0.686885008277897,0.726663364191536,-0.0122204969175564));
#41069=DIRECTION('center_axis',(-0.0503511057596336,0.99873157451406,9.06501467774672E-5));
#41070=DIRECTION('ref_axis',(0.998626750226755,0.0503471356611751,-0.0144837723768601));
#41071=DIRECTION('center_axis',(5.15167520928809E-67,-1.18789542670764E-48,
-1.));
#41072=DIRECTION('ref_axis',(-4.33680868994202E-19,1.,-1.18789542670764E-48));
#41073=DIRECTION('center_axis',(5.15167520928809E-67,-1.18789542670764E-48,
-1.));
#41074=DIRECTION('ref_axis',(0.,1.,0.));
#41075=DIRECTION('center_axis',(0.778374608459656,-0.627800093808486,0.000105448247696036));
#41076=DIRECTION('ref_axis',(0.627754220580537,0.778315680169911,-0.0122204969200215));
#41077=DIRECTION('center_axis',(-0.128555466315276,0.991702316152893,9.06501466266556E-5));
#41078=DIRECTION('ref_axis',(0.991598126493641,0.128543284036441,-0.0144837724170315));
#41079=DIRECTION('center_axis',(5.15167520928809E-67,-1.18789542670764E-48,
-1.));
#41080=DIRECTION('ref_axis',(-4.33680868994202E-19,1.,-1.18789542670764E-48));
#41081=DIRECTION('center_axis',(5.15167520928809E-67,-1.18789542670764E-48,
-1.));
#41082=DIRECTION('ref_axis',(0.,1.,0.));
#41083=DIRECTION('center_axis',(0.825231766969182,-0.564794227719785,0.000105448247768853));
#41084=DIRECTION('ref_axis',(0.564753119363901,0.825169421163535,-0.0122204969367096));
#41085=DIRECTION('center_axis',(-0.205967239672835,0.978558883238052,9.06501467925213E-5));
#41086=DIRECTION('ref_axis',(0.978455970572528,0.205946920321698,-0.0144837723325158));
#41087=DIRECTION('center_axis',(5.15167520928809E-67,-1.18789542670764E-48,
-1.));
#41088=DIRECTION('ref_axis',(-4.33680868994202E-19,1.,-1.18789542670764E-48));
#41089=DIRECTION('center_axis',(5.15167520928809E-67,-1.18789542670764E-48,
-1.));
#41090=DIRECTION('ref_axis',(0.,1.,0.));
#41091=DIRECTION('center_axis',(0.867001097218019,-0.498306217403936,0.000105448247742928));
#41092=DIRECTION('ref_axis',(0.498270127367224,0.866935718279781,-0.0122204968872419));
#41093=DIRECTION('center_axis',(-0.282109156506148,0.959382309404307,9.06501467249393E-5));
#41094=DIRECTION('ref_axis',(0.959281308221143,0.282080825357837,-0.0144837724013445));
#41095=DIRECTION('center_axis',(5.15167520928809E-67,-1.18789542670764E-48,
-1.));
#41096=DIRECTION('ref_axis',(-4.33680868994202E-19,1.,-1.18789542670764E-48));
#41097=DIRECTION('center_axis',(5.15167520928809E-67,-1.18789542670764E-48,
-1.));
#41098=DIRECTION('ref_axis',(0.,1.,0.));
#41099=DIRECTION('center_axis',(0.903425077395463,-0.428745983553979,0.000105448247628158));
#41100=DIRECTION('ref_axis',(0.428715134343002,0.903357068406648,-0.0122204969215573));
#41101=DIRECTION('center_axis',(-0.356511776579108,0.934290824606,9.06501467950618E-5));
#41102=DIRECTION('ref_axis',(0.934192357613078,0.356475608305158,-0.0144837723258434));
#41103=DIRECTION('center_axis',(5.15167520928809E-67,-1.18789542670764E-48,
-1.));
#41104=DIRECTION('ref_axis',(-4.33680868994202E-19,1.,-1.18789542670764E-48));
#41105=DIRECTION('center_axis',(5.15167520928809E-67,-1.18789542670764E-48,
-1.));
#41106=DIRECTION('ref_axis',(0.,1.,0.));
#41107=DIRECTION('center_axis',(0.93427914155167,-0.356542388142199,0.000105448247170392));
#41108=DIRECTION('ref_axis',(0.356516969951772,0.934208921807903,-0.012220497163456));
#41109=DIRECTION('center_axis',(-0.428716382997142,0.903439126190801,9.06501468381065E-5));
#41110=DIRECTION('ref_axis',(0.903343800468038,0.42867260058632,-0.0144837723857595));
#41111=DIRECTION('center_axis',(5.15167520928809E-67,-1.18789542670764E-48,
-1.));
#41112=DIRECTION('ref_axis',(-4.33680868994202E-19,1.,-1.18789542670764E-48));
#41113=DIRECTION('center_axis',(5.15167520928809E-67,-1.18789542670764E-48,
-1.));
#41114=DIRECTION('ref_axis',(0.,1.,0.));
#41115=DIRECTION('center_axis',(0.959373064120116,-0.282140590347164,0.000105448247729292));
#41116=DIRECTION('ref_axis',(0.282120759890968,0.959301066555056,-0.0122204969160199));
#41117=DIRECTION('center_axis',(-0.498277810351142,0.867017425138747,9.06501467342992E-5));
#41118=DIRECTION('ref_axis',(0.866925828401964,0.498226683737,-0.0144837723677419));
#41119=DIRECTION('center_axis',(5.15167520928809E-67,-1.18789542670764E-48,
-1.));
#41120=DIRECTION('ref_axis',(-4.33680868994202E-19,1.,-1.18789542670764E-48));
#41121=DIRECTION('center_axis',(5.15167520928809E-67,-1.18789542670764E-48,
-1.));
#41122=DIRECTION('ref_axis',(0.,1.,0.));
#41123=DIRECTION('center_axis',(0.978552132724802,-0.205999301990102,0.000105448247615573));
#41124=DIRECTION('ref_axis',(0.205985181528349,0.978478801224133,-0.0122204969505153));
#41125=DIRECTION('center_axis',(-0.564767189310334,0.825250273348065,9.0650146758551E-5));
#41126=DIRECTION('ref_axis',(0.82516297032109,0.564709033705155,-0.014483772390721));
#41127=DIRECTION('center_axis',(5.15167520928809E-67,-1.18789542670764E-48,
-1.));
#41128=DIRECTION('ref_axis',(-4.33680868994202E-19,1.,-1.18789542670764E-48));
#41129=DIRECTION('center_axis',(5.15167520928809E-67,-1.18789542670764E-48,
-1.));
#41130=DIRECTION('ref_axis',(0.,1.,0.));
#41131=DIRECTION('center_axis',(0.991698102030069,-0.128587959430995,0.000105448245943976));
#41132=DIRECTION('ref_axis',(0.128579636019992,0.99162388869792,-0.0122204977223251));
#41133=DIRECTION('center_axis',(-0.627774590743336,0.778395179198579,9.06501467764949E-5));
#41134=DIRECTION('ref_axis',(0.778312708134504,0.627709764696415,-0.014483772336843));
#41135=DIRECTION('center_axis',(5.15167520928809E-67,-1.18789542670764E-48,
-1.));
#41136=DIRECTION('ref_axis',(-4.33680868994202E-19,1.,-1.18789542670764E-48));
#41137=DIRECTION('center_axis',(5.15167520928809E-67,-1.18789542670764E-48,
-1.));
#41138=DIRECTION('ref_axis',(0.,1.,0.));
#41139=DIRECTION('center_axis',(0.998729922762269,-0.0503838293497056,0.000105448247690158));
#41140=DIRECTION('ref_axis',(0.0503813543083624,0.998655285167543,-0.0122204969206726));
#41141=DIRECTION('center_axis',(-0.686911553068082,0.726741019926732,9.065014676939E-5));
#41142=DIRECTION('ref_axis',(0.726663889285701,0.686840456252424,-0.0144837724071123));
#41143=DIRECTION('center_axis',(5.15167520928809E-67,-1.18789542670764E-48,
-1.));
#41144=DIRECTION('ref_axis',(-4.33680868994202E-19,1.,-1.18789542670764E-48));
#41145=DIRECTION('center_axis',(5.15167520928809E-67,-1.18789542670764E-48,
-1.));
#41146=DIRECTION('ref_axis',(0.,1.,0.));
#41147=DIRECTION('center_axis',(0.999604241409737,0.0281309337977193,0.000105448247673278));
#41148=DIRECTION('ref_axis',(0.0281275452111183,-0.999529639707527,0.0122204969841135));
#41149=DIRECTION('center_axis',(-0.741813477246845,0.670606260601179,9.06501467534462E-5));
#41150=DIRECTION('ref_axis',(0.670534945920493,0.741736547999089,-0.0144837723606804));
#41151=DIRECTION('center_axis',(5.15167520928809E-67,-1.18789542670764E-48,
-1.));
#41152=DIRECTION('ref_axis',(-4.33680868994202E-19,1.,-1.18789542670764E-48));
#41153=DIRECTION('center_axis',(5.15167520928809E-67,-1.18789542670764E-48,
-1.));
#41154=DIRECTION('ref_axis',(0.,1.,0.));
#41155=DIRECTION('center_axis',(0.994315667506773,0.106472260383761,0.000105448247684943));
#41156=DIRECTION('ref_axis',(0.106463029060952,-0.994241561642206,0.0122204969798675));
#41157=DIRECTION('center_axis',(-0.792141874660476,0.610336990679688,9.06501468075157E-5));
#41158=DIRECTION('ref_axis',(0.610271931637649,0.792059587274653,-0.0144837723525293));
#41159=DIRECTION('center_axis',(5.15167520928809E-67,-1.18789542670764E-48,
-1.));
#41160=DIRECTION('ref_axis',(-4.33680868994202E-19,1.,-1.18789542670764E-48));
#41161=DIRECTION('center_axis',(5.15167520928809E-67,-1.18789542670764E-48,
-1.));
#41162=DIRECTION('ref_axis',(0.,1.,0.));
#41163=DIRECTION('center_axis',(0.982896806870138,0.184157150078822,0.000105448247739781));
#41164=DIRECTION('ref_axis',(0.184142132934029,-0.982823653730722,0.0122204969580191));
#41165=DIRECTION('center_axis',(-0.837586454002804,0.546304790253169,9.06501467452083E-5));
#41166=DIRECTION('ref_axis',(0.546246387960594,0.837499315808325,-0.0144837723191043));
#41167=DIRECTION('center_axis',(5.15167520928809E-67,-1.18789542670764E-48,
-1.));
#41168=DIRECTION('ref_axis',(-4.33680868994202E-19,1.,-1.18789542670764E-48));
#41169=DIRECTION('center_axis',(5.15167520928809E-67,-1.18789542670764E-48,
-1.));
#41170=DIRECTION('ref_axis',(0.,1.,0.));
#41171=DIRECTION('center_axis',(-0.778395179198544,-0.62777459074338,9.06501468008605E-5));
#41172=DIRECTION('ref_axis',(0.62770976469586,-0.778312708133716,0.0144837724032618));
#41173=DIRECTION('center_axis',(5.15167520928809E-67,-1.18789542670764E-48,
-1.));
#41174=DIRECTION('ref_axis',(-4.33680868994202E-19,1.,-1.18789542670764E-48));
#41175=DIRECTION('center_axis',(0.128587959434843,0.991698102029569,0.000105448247713068));
#41176=DIRECTION('ref_axis',(0.991623888707174,-0.128579636025041,0.0122204969182792));
#41177=DIRECTION('center_axis',(5.15167520928809E-67,-1.18789542670764E-48,
-1.));
#41178=DIRECTION('ref_axis',(0.,1.,0.));
#41179=DIRECTION('center_axis',(-0.82525027334801,-0.564767189310415,9.06501467887519E-5));
#41180=DIRECTION('ref_axis',(0.56470903370554,-0.825162970321483,0.0144837723533119));
#41181=DIRECTION('center_axis',(5.15167520928809E-67,-1.18789542670764E-48,
-1.));
#41182=DIRECTION('ref_axis',(-4.33680868994202E-19,1.,-1.18789542670764E-48));
#41183=DIRECTION('center_axis',(0.205999301990312,0.978552132724757,0.000105448247717959));
#41184=DIRECTION('ref_axis',(0.978478801224664,-0.205985181528676,0.0122204969024898));
#41185=DIRECTION('center_axis',(5.15167520928809E-67,-1.18789542670764E-48,
-1.));
#41186=DIRECTION('ref_axis',(0.,1.,0.));
#41187=DIRECTION('center_axis',(-0.867017425138643,-0.498277810351323,9.06501468256068E-5));
#41188=DIRECTION('ref_axis',(0.498226683737087,-0.866925828401692,0.014483772381015));
#41189=DIRECTION('center_axis',(5.15167520928809E-67,-1.18789542670764E-48,
-1.));
#41190=DIRECTION('ref_axis',(-4.33680868994202E-19,1.,-1.18789542670764E-48));
#41191=DIRECTION('center_axis',(0.282140590347035,0.959373064120154,0.000105448247634384));
#41192=DIRECTION('ref_axis',(0.959301066555324,-0.282120759890904,0.0122204968965099));
#41193=DIRECTION('center_axis',(5.15167520928809E-67,-1.18789542670764E-48,
-1.));
#41194=DIRECTION('ref_axis',(0.,1.,0.));
#41195=DIRECTION('center_axis',(-0.903439126190879,-0.428716382996979,9.06501467301661E-5));
#41196=DIRECTION('ref_axis',(0.428672600586422,-0.903343800468688,0.0144837723422516));
#41197=DIRECTION('center_axis',(5.15167520928809E-67,-1.18789542670764E-48,
-1.));
#41198=DIRECTION('ref_axis',(-4.33680868994202E-19,1.,-1.18789542670764E-48));
#41199=DIRECTION('center_axis',(0.356542388143256,0.934279141551266,0.000105448247681697));
#41200=DIRECTION('ref_axis',(0.934208921810558,-0.356516969953973,0.0122204968962765));
#41201=DIRECTION('center_axis',(5.15167520928809E-67,-1.18789542670764E-48,
-1.));
#41202=DIRECTION('ref_axis',(0.,1.,0.));
#41203=DIRECTION('center_axis',(-0.934290824606111,-0.356511776578816,9.06501466618288E-5));
#41204=DIRECTION('ref_axis',(0.356475608304419,-0.934192357612002,0.0144837724134131));
#41205=DIRECTION('center_axis',(5.15167520928809E-67,-1.18789542670764E-48,
-1.));
#41206=DIRECTION('ref_axis',(-4.33680868994202E-19,1.,-1.18789542670764E-48));
#41207=DIRECTION('center_axis',(0.428745983554273,0.903425077395324,0.000105448247749283));
#41208=DIRECTION('ref_axis',(0.903357068406257,-0.428715134343181,0.0122204969441668));
#41209=DIRECTION('center_axis',(5.15167520928809E-67,-1.18789542670764E-48,
-1.));
#41210=DIRECTION('ref_axis',(0.,1.,0.));
#41211=DIRECTION('center_axis',(-0.959382309404256,-0.282109156506322,9.06501468215648E-5));
#41212=DIRECTION('ref_axis',(0.282080825358184,-0.959281308221691,0.0144837723582998));
#41213=DIRECTION('center_axis',(5.15167520928809E-67,-1.18789542670764E-48,
-1.));
#41214=DIRECTION('ref_axis',(-4.33680868994202E-19,1.,-1.18789542670764E-48));
#41215=DIRECTION('center_axis',(0.498306217397306,0.86700109722183,0.000105448244261109));
#41216=DIRECTION('ref_axis',(0.866935718266673,-0.498270127351015,0.0122204984779969));
#41217=DIRECTION('center_axis',(5.15167520928809E-67,-1.18789542670764E-48,
-1.));
#41218=DIRECTION('ref_axis',(0.,1.,0.));
#41219=DIRECTION('center_axis',(-0.978558883238081,-0.205967239672699,9.06501467769327E-5));
#41220=DIRECTION('ref_axis',(0.205946920321355,-0.978455970571544,0.0144837724038677));
#41221=DIRECTION('center_axis',(5.15167520928809E-67,-1.18789542670764E-48,
-1.));
#41222=DIRECTION('ref_axis',(-4.33680868994202E-19,1.,-1.18789542670764E-48));
#41223=DIRECTION('center_axis',(0.564794227718686,0.825231766969935,0.000105448247134299));
#41224=DIRECTION('ref_axis',(0.825169421162366,-0.564753119361502,0.0122204971264834));
#41225=DIRECTION('center_axis',(5.15167520928809E-67,-1.18789542670764E-48,
-1.));
#41226=DIRECTION('ref_axis',(0.,1.,0.));
#41227=DIRECTION('center_axis',(-0.991702316152861,-0.128555466315523,9.06501467288715E-5));
#41228=DIRECTION('ref_axis',(0.12854328403675,-0.991598126494102,0.0144837723826971));
#41229=DIRECTION('center_axis',(5.15167520928809E-67,-1.18789542670764E-48,
-1.));
#41230=DIRECTION('ref_axis',(-4.33680868994202E-19,1.,-1.18789542670764E-48));
#41231=DIRECTION('center_axis',(0.627800093808552,0.778374608459603,0.000105448247728723));
#41232=DIRECTION('ref_axis',(0.778315680170199,-0.627754220580874,0.0122204968843025));
#41233=DIRECTION('center_axis',(5.15167520928809E-67,-1.18789542670764E-48,
-1.));
#41234=DIRECTION('ref_axis',(0.,1.,0.));
#41235=DIRECTION('center_axis',(-0.998731574514058,-0.0503511057596628,
9.06501468007229E-5));
#41236=DIRECTION('ref_axis',(0.0503471356611987,-0.998626750226619,0.0144837723861814));
#41237=DIRECTION('center_axis',(5.15167520928809E-67,-1.18789542670764E-48,
-1.));
#41238=DIRECTION('ref_axis',(-4.33680868994202E-19,1.,-1.18789542670764E-48));
#41239=DIRECTION('center_axis',(0.686935363554282,0.726718511653043,0.000105448247718559));
#41240=DIRECTION('ref_axis',(0.726663364191442,-0.686885008277775,0.012220496930023));
#41241=DIRECTION('center_axis',(5.15167520928809E-67,-1.18789542670764E-48,
-1.));
#41242=DIRECTION('ref_axis',(0.,1.,0.));
#41243=DIRECTION('center_axis',(-0.99960332060644,0.0281636861069471,9.06501467308329E-5));
#41244=DIRECTION('ref_axis',(0.0281594195481261,0.999498507967114,-0.0144837723754724));
#41245=DIRECTION('center_axis',(5.15167520928809E-67,-1.18789542670764E-48,
-1.));
#41246=DIRECTION('ref_axis',(-4.33680868994202E-19,1.,-1.18789542670764E-48));
#41247=DIRECTION('center_axis',(0.741835448354451,0.670581953563782,0.00010544824772104));
#41248=DIRECTION('ref_axis',(0.670530926933101,-0.74178092148675,0.0122204969008548));
#41249=DIRECTION('center_axis',(5.15167520928809E-67,-1.18789542670764E-48,
-1.));
#41250=DIRECTION('ref_axis',(0.,1.,0.));
#41251=DIRECTION('center_axis',(-0.994312179825441,0.106504839483146,9.06501467381912E-5));
#41252=DIRECTION('ref_axis',(0.106492362571802,0.99420802503887,-0.0144837723741357));
#41253=DIRECTION('center_axis',(5.15167520928809E-67,-1.18789542670764E-48,
-1.));
#41254=DIRECTION('ref_axis',(-4.33680868994202E-19,1.,-1.18789542670764E-48));
#41255=DIRECTION('center_axis',(0.792161870929241,0.610311034740936,0.000105448246928053));
#41256=DIRECTION('ref_axis',(0.610264443534212,-0.792103508642726,0.0122204972796185));
#41257=DIRECTION('center_axis',(5.15167520928809E-67,-1.18789542670764E-48,
-1.));
#41258=DIRECTION('ref_axis',(0.,1.,0.));
#41259=DIRECTION('center_axis',(-0.982890773813477,0.184189355107443,9.06501467544422E-5));
#41260=DIRECTION('ref_axis',(0.184168744767819,0.982787919028209,-0.0144837723970302));
#41261=DIRECTION('center_axis',(5.15167520928809E-67,-1.18789542670764E-48,
-1.));
#41262=DIRECTION('ref_axis',(-4.33680868994202E-19,1.,-1.18789542670764E-48));
#41263=DIRECTION('center_axis',(0.837604352151223,0.546277345437276,0.000105448247675196));
#41264=DIRECTION('ref_axis',(0.546235476910048,-0.837542514275434,0.0122204969635834));
#41265=DIRECTION('center_axis',(5.15167520928809E-67,-1.18789542670764E-48,
-1.));
#41266=DIRECTION('ref_axis',(0.,1.,0.));
#41267=DIRECTION('center_axis',(-0.96540951933663,0.260738282108263,9.06501468112521E-5));
#41268=DIRECTION('ref_axis',(0.26070966540993,0.965308598686718,-0.0144837724135372));
#41269=DIRECTION('center_axis',(5.15167520928809E-67,-1.18789542670764E-48,
-1.));
#41270=DIRECTION('ref_axis',(-4.33680868994202E-19,1.,-1.18789542670764E-48));
#41271=DIRECTION('center_axis',(0.877882724009476,0.478875674644651,0.000105448247670176));
#41272=DIRECTION('ref_axis',(0.478838786927941,-0.877817791792444,0.0122204969627255));
#41273=DIRECTION('center_axis',(5.15167520928809E-67,-1.18789542670764E-48,
-1.));
#41274=DIRECTION('ref_axis',(0.,1.,0.));
#41275=DIRECTION('center_axis',(-0.941976194141744,0.33567967089591,9.06501467361574E-5));
#41276=DIRECTION('ref_axis',(0.335643224270696,0.941877829837669,-0.0144837723488913));
#41277=DIRECTION('center_axis',(5.15167520928809E-67,-1.18789542670764E-48,
-1.));
#41278=DIRECTION('ref_axis',(-4.33680868994202E-19,1.,-1.18789542670764E-48));
#41279=DIRECTION('center_axis',(0.912748656948457,0.408521576075799,0.000105448247549386));
#41280=DIRECTION('ref_axis',(0.408489896594413,-0.912681030718381,0.0122204970078645));
#41281=DIRECTION('center_axis',(5.15167520928809E-67,-1.18789542670764E-48,
-1.));
#41282=DIRECTION('ref_axis',(0.,1.,0.));
#41283=DIRECTION('center_axis',(0.965418060567994,0.260706649723021,0.000105448239440975));
#41284=DIRECTION('ref_axis',(0.260685939330027,-0.965346311123993,0.0122205006002244));
#41285=DIRECTION('center_axis',(-0.877867034330543,0.478904439129822,9.06501467527618E-5));
#41286=DIRECTION('ref_axis',(0.478853053655558,0.877775582562237,-0.014483772377146));
#41287=DIRECTION('center_axis',(5.15167520928809E-67,-1.18789542670764E-48,
-1.));
#41288=DIRECTION('ref_axis',(-4.33680868994202E-19,1.,-1.18789542670764E-48));
#41289=DIRECTION('center_axis',(5.15167520928809E-67,-1.18789542670764E-48,
-1.));
#41290=DIRECTION('ref_axis',(-4.33680868994202E-19,1.,-1.18789542670764E-48));
#41291=DIRECTION('',(5.15167520928809E-67,-1.18789542670764E-48,-1.));
#41292=DIRECTION('center_axis',(5.15167520928809E-67,-1.18789542670764E-48,
-1.));
#41293=DIRECTION('ref_axis',(-4.33680868994202E-19,1.,-1.18789542670764E-48));
#41294=DIRECTION('',(-5.15167520928809E-67,1.18789542670764E-48,1.));
#41295=DIRECTION('center_axis',(5.15167520928809E-67,-1.18789542670764E-48,
-1.));
#41296=DIRECTION('ref_axis',(-4.33680868994202E-19,1.,-1.18789542670764E-48));
#41297=DIRECTION('',(-5.15167520928809E-67,1.18789542670764E-48,1.));
#41298=DIRECTION('',(5.15167520928809E-67,-1.18789542670764E-48,-1.));
#41299=DIRECTION('center_axis',(5.15167520928809E-67,-1.18789542670764E-48,
-1.));
#41300=DIRECTION('ref_axis',(-4.33680868994202E-19,1.,-1.18789542670764E-48));
#41301=DIRECTION('center_axis',(5.15167520928809E-67,-1.18789542670764E-48,
-1.));
#41302=DIRECTION('ref_axis',(-4.33680868994202E-19,1.,-1.18789542670764E-48));
#41303=DIRECTION('',(-5.15167520928809E-67,1.18789542670764E-48,1.));
#41304=DIRECTION('',(5.15167520928809E-67,-1.18789542670764E-48,-1.));
#41305=DIRECTION('center_axis',(5.15167520928809E-67,-1.18789542670764E-48,
-1.));
#41306=DIRECTION('ref_axis',(-4.33680868994202E-19,1.,-1.18789542670764E-48));
#41307=DIRECTION('center_axis',(5.15167520928809E-67,-1.18789542670764E-48,
-1.));
#41308=DIRECTION('ref_axis',(-4.33680868994202E-19,1.,-1.18789542670764E-48));
#41309=DIRECTION('',(-5.15167520928809E-67,1.18789542670764E-48,1.));
#41310=DIRECTION('',(5.15167520928809E-67,-1.18789542670764E-48,-1.));
#41311=DIRECTION('center_axis',(5.15167520928809E-67,-1.18789542670764E-48,
-1.));
#41312=DIRECTION('ref_axis',(-4.33680868994202E-19,1.,-1.18789542670764E-48));
#41313=DIRECTION('center_axis',(5.15167520928809E-67,-1.18789542670764E-48,
-1.));
#41314=DIRECTION('ref_axis',(-4.33680868994202E-19,1.,-1.18789542670764E-48));
#41315=DIRECTION('',(-5.15167520928809E-67,1.18789542670764E-48,1.));
#41316=DIRECTION('',(5.15167520928809E-67,-1.18789542670764E-48,-1.));
#41317=DIRECTION('center_axis',(5.15167520928809E-67,-1.18789542670764E-48,
-1.));
#41318=DIRECTION('ref_axis',(-4.33680868994202E-19,1.,-1.18789542670764E-48));
#41319=DIRECTION('center_axis',(5.15167520928809E-67,-1.18789542670764E-48,
-1.));
#41320=DIRECTION('ref_axis',(-4.33680868994202E-19,1.,-1.18789542670764E-48));
#41321=DIRECTION('',(-5.15167520928809E-67,1.18789542670764E-48,1.));
#41322=DIRECTION('',(5.15167520928809E-67,-1.18789542670764E-48,-1.));
#41323=DIRECTION('center_axis',(5.15167520928809E-67,-1.18789542670764E-48,
-1.));
#41324=DIRECTION('ref_axis',(-4.33680868994202E-19,1.,-1.18789542670764E-48));
#41325=DIRECTION('center_axis',(5.15167520928809E-67,-1.18789542670764E-48,
-1.));
#41326=DIRECTION('ref_axis',(-4.33680868994202E-19,1.,-1.18789542670764E-48));
#41327=DIRECTION('',(-5.15167520928809E-67,1.18789542670764E-48,1.));
#41328=DIRECTION('',(5.15167520928809E-67,-1.18789542670764E-48,-1.));
#41329=DIRECTION('center_axis',(5.15167520928809E-67,-1.18789542670764E-48,
-1.));
#41330=DIRECTION('ref_axis',(-4.33680868994202E-19,1.,-1.18789542670764E-48));
#41331=DIRECTION('center_axis',(5.15167520928809E-67,-1.18789542670764E-48,
-1.));
#41332=DIRECTION('ref_axis',(-4.33680868994202E-19,1.,-1.18789542670764E-48));
#41333=DIRECTION('',(-5.15167520928809E-67,1.18789542670764E-48,1.));
#41334=DIRECTION('',(5.15167520928809E-67,-1.18789542670764E-48,-1.));
#41335=DIRECTION('center_axis',(5.15167520928809E-67,-1.18789542670764E-48,
-1.));
#41336=DIRECTION('ref_axis',(-4.33680868994202E-19,1.,-1.18789542670764E-48));
#41337=DIRECTION('center_axis',(5.15167520928809E-67,-1.18789542670764E-48,
-1.));
#41338=DIRECTION('ref_axis',(-4.33680868994202E-19,1.,-1.18789542670764E-48));
#41339=DIRECTION('',(-5.15167520928809E-67,1.18789542670764E-48,1.));
#41340=DIRECTION('',(5.15167520928809E-67,-1.18789542670764E-48,-1.));
#41341=DIRECTION('center_axis',(5.15167520928809E-67,-1.18789542670764E-48,
-1.));
#41342=DIRECTION('ref_axis',(-4.33680868994202E-19,1.,-1.18789542670764E-48));
#41343=DIRECTION('center_axis',(5.15167520928809E-67,-1.18789542670764E-48,
-1.));
#41344=DIRECTION('ref_axis',(-4.33680868994202E-19,1.,-1.18789542670764E-48));
#41345=DIRECTION('',(-5.15167520928809E-67,1.18789542670764E-48,1.));
#41346=DIRECTION('',(5.15167520928809E-67,-1.18789542670764E-48,-1.));
#41347=DIRECTION('center_axis',(5.15167520928809E-67,-1.18789542670764E-48,
-1.));
#41348=DIRECTION('ref_axis',(-4.33680868994202E-19,1.,-1.18789542670764E-48));
#41349=DIRECTION('center_axis',(5.15167520928809E-67,-1.18789542670764E-48,
-1.));
#41350=DIRECTION('ref_axis',(-4.33680868994202E-19,1.,-1.18789542670764E-48));
#41351=DIRECTION('',(-5.15167520928809E-67,1.18789542670764E-48,1.));
#41352=DIRECTION('',(5.15167520928809E-67,-1.18789542670764E-48,-1.));
#41353=DIRECTION('center_axis',(5.15167520928809E-67,-1.18789542670764E-48,
-1.));
#41354=DIRECTION('ref_axis',(-4.33680868994202E-19,1.,-1.18789542670764E-48));
#41355=DIRECTION('center_axis',(5.15167520928809E-67,-1.18789542670764E-48,
-1.));
#41356=DIRECTION('ref_axis',(-4.33680868994202E-19,1.,-1.18789542670764E-48));
#41357=DIRECTION('',(-5.15167520928809E-67,1.18789542670764E-48,1.));
#41358=DIRECTION('',(5.15167520928809E-67,-1.18789542670764E-48,-1.));
#41359=DIRECTION('center_axis',(5.15167520928809E-67,-1.18789542670764E-48,
-1.));
#41360=DIRECTION('ref_axis',(-4.33680868994202E-19,1.,-1.18789542670764E-48));
#41361=DIRECTION('center_axis',(5.15167520928809E-67,-1.18789542670764E-48,
-1.));
#41362=DIRECTION('ref_axis',(-4.33680868994202E-19,1.,-1.18789542670764E-48));
#41363=DIRECTION('',(-5.15167520928809E-67,1.18789542670764E-48,1.));
#41364=DIRECTION('',(5.15167520928809E-67,-1.18789542670764E-48,-1.));
#41365=DIRECTION('center_axis',(5.15167520928809E-67,-1.18789542670764E-48,
-1.));
#41366=DIRECTION('ref_axis',(-4.33680868994202E-19,1.,-1.18789542670764E-48));
#41367=DIRECTION('center_axis',(5.15167520928809E-67,-1.18789542670764E-48,
-1.));
#41368=DIRECTION('ref_axis',(-4.33680868994202E-19,1.,-1.18789542670764E-48));
#41369=DIRECTION('',(-5.15167520928809E-67,1.18789542670764E-48,1.));
#41370=DIRECTION('',(5.15167520928809E-67,-1.18789542670764E-48,-1.));
#41371=DIRECTION('center_axis',(5.15167520928809E-67,-1.18789542670764E-48,
-1.));
#41372=DIRECTION('ref_axis',(-4.33680868994202E-19,1.,-1.18789542670764E-48));
#41373=DIRECTION('center_axis',(5.15167520928809E-67,-1.18789542670764E-48,
-1.));
#41374=DIRECTION('ref_axis',(-4.33680868994202E-19,1.,-1.18789542670764E-48));
#41375=DIRECTION('',(-5.15167520928809E-67,1.18789542670764E-48,1.));
#41376=DIRECTION('',(5.15167520928809E-67,-1.18789542670764E-48,-1.));
#41377=DIRECTION('center_axis',(5.15167520928809E-67,-1.18789542670764E-48,
-1.));
#41378=DIRECTION('ref_axis',(-4.33680868994202E-19,1.,-1.18789542670764E-48));
#41379=DIRECTION('center_axis',(5.15167520928809E-67,-1.18789542670764E-48,
-1.));
#41380=DIRECTION('ref_axis',(-4.33680868994202E-19,1.,-1.18789542670764E-48));
#41381=DIRECTION('',(-5.15167520928809E-67,1.18789542670764E-48,1.));
#41382=DIRECTION('',(5.15167520928809E-67,-1.18789542670764E-48,-1.));
#41383=DIRECTION('center_axis',(5.15167520928809E-67,-1.18789542670764E-48,
-1.));
#41384=DIRECTION('ref_axis',(-4.33680868994202E-19,1.,-1.18789542670764E-48));
#41385=DIRECTION('center_axis',(5.15167520928809E-67,-1.18789542670764E-48,
-1.));
#41386=DIRECTION('ref_axis',(-4.33680868994202E-19,1.,-1.18789542670764E-48));
#41387=DIRECTION('',(-5.15167520928809E-67,1.18789542670764E-48,1.));
#41388=DIRECTION('',(5.15167520928809E-67,-1.18789542670764E-48,-1.));
#41389=DIRECTION('center_axis',(5.15167520928809E-67,-1.18789542670764E-48,
-1.));
#41390=DIRECTION('ref_axis',(-4.33680868994202E-19,1.,-1.18789542670764E-48));
#41391=DIRECTION('center_axis',(5.15167520928809E-67,-1.18789542670764E-48,
-1.));
#41392=DIRECTION('ref_axis',(-4.33680868994202E-19,1.,-1.18789542670764E-48));
#41393=DIRECTION('',(-5.15167520928809E-67,1.18789542670764E-48,1.));
#41394=DIRECTION('',(5.15167520928809E-67,-1.18789542670764E-48,-1.));
#41395=DIRECTION('center_axis',(5.15167520928809E-67,-1.18789542670764E-48,
-1.));
#41396=DIRECTION('ref_axis',(-4.33680868994202E-19,1.,-1.18789542670764E-48));
#41397=DIRECTION('center_axis',(5.15167520928809E-67,-1.18789542670764E-48,
-1.));
#41398=DIRECTION('ref_axis',(-4.33680868994202E-19,1.,-1.18789542670764E-48));
#41399=DIRECTION('',(-5.15167520928809E-67,1.18789542670764E-48,1.));
#41400=DIRECTION('',(5.15167520928809E-67,-1.18789542670764E-48,-1.));
#41401=DIRECTION('center_axis',(5.15167520928809E-67,-1.18789542670764E-48,
-1.));
#41402=DIRECTION('ref_axis',(-4.33680868994202E-19,1.,-1.18789542670764E-48));
#41403=DIRECTION('center_axis',(5.15167520928809E-67,-1.18789542670764E-48,
-1.));
#41404=DIRECTION('ref_axis',(-4.33680868994202E-19,1.,-1.18789542670764E-48));
#41405=DIRECTION('',(-5.15167520928809E-67,1.18789542670764E-48,1.));
#41406=DIRECTION('',(5.15167520928809E-67,-1.18789542670764E-48,-1.));
#41407=DIRECTION('center_axis',(5.15167520928809E-67,-1.18789542670764E-48,
-1.));
#41408=DIRECTION('ref_axis',(-4.33680868994202E-19,1.,-1.18789542670764E-48));
#41409=DIRECTION('center_axis',(5.15167520928809E-67,-1.18789542670764E-48,
-1.));
#41410=DIRECTION('ref_axis',(-4.33680868994202E-19,1.,-1.18789542670764E-48));
#41411=DIRECTION('',(-5.15167520928809E-67,1.18789542670764E-48,1.));
#41412=DIRECTION('',(5.15167520928809E-67,-1.18789542670764E-48,-1.));
#41413=DIRECTION('center_axis',(5.15167520928809E-67,-1.18789542670764E-48,
-1.));
#41414=DIRECTION('ref_axis',(-4.33680868994202E-19,1.,-1.18789542670764E-48));
#41415=DIRECTION('center_axis',(5.15167520928809E-67,-1.18789542670764E-48,
-1.));
#41416=DIRECTION('ref_axis',(-4.33680868994202E-19,1.,-1.18789542670764E-48));
#41417=DIRECTION('',(-5.15167520928809E-67,1.18789542670764E-48,1.));
#41418=DIRECTION('',(5.15167520928809E-67,-1.18789542670764E-48,-1.));
#41419=DIRECTION('center_axis',(5.15167520928809E-67,-1.18789542670764E-48,
-1.));
#41420=DIRECTION('ref_axis',(-4.33680868994202E-19,1.,-1.18789542670764E-48));
#41421=DIRECTION('center_axis',(5.15167520928809E-67,-1.18789542670764E-48,
-1.));
#41422=DIRECTION('ref_axis',(-4.33680868994202E-19,1.,-1.18789542670764E-48));
#41423=DIRECTION('',(-5.15167520928809E-67,1.18789542670764E-48,1.));
#41424=DIRECTION('',(5.15167520928809E-67,-1.18789542670764E-48,-1.));
#41425=DIRECTION('center_axis',(5.15167520928809E-67,-1.18789542670764E-48,
-1.));
#41426=DIRECTION('ref_axis',(-4.33680868994202E-19,1.,-1.18789542670764E-48));
#41427=DIRECTION('center_axis',(5.15167520928809E-67,-1.18789542670764E-48,
-1.));
#41428=DIRECTION('ref_axis',(-4.33680868994202E-19,1.,-1.18789542670764E-48));
#41429=DIRECTION('',(-5.15167520928809E-67,1.18789542670764E-48,1.));
#41430=DIRECTION('',(5.15167520928809E-67,-1.18789542670764E-48,-1.));
#41431=DIRECTION('center_axis',(5.15167520928809E-67,-1.18789542670764E-48,
-1.));
#41432=DIRECTION('ref_axis',(-4.33680868994202E-19,1.,-1.18789542670764E-48));
#41433=DIRECTION('center_axis',(5.15167520928809E-67,-1.18789542670764E-48,
-1.));
#41434=DIRECTION('ref_axis',(-4.33680868994202E-19,1.,-1.18789542670764E-48));
#41435=DIRECTION('',(-5.15167520928809E-67,1.18789542670764E-48,1.));
#41436=DIRECTION('',(5.15167520928809E-67,-1.18789542670764E-48,-1.));
#41437=DIRECTION('center_axis',(5.15167520928809E-67,-1.18789542670764E-48,
-1.));
#41438=DIRECTION('ref_axis',(-4.33680868994202E-19,1.,-1.18789542670764E-48));
#41439=DIRECTION('center_axis',(5.15167520928809E-67,-1.18789542670764E-48,
-1.));
#41440=DIRECTION('ref_axis',(-4.33680868994202E-19,1.,-1.18789542670764E-48));
#41441=DIRECTION('',(-5.15167520928809E-67,1.18789542670764E-48,1.));
#41442=DIRECTION('',(5.15167520928809E-67,-1.18789542670764E-48,-1.));
#41443=DIRECTION('center_axis',(5.15167520928809E-67,-1.18789542670764E-48,
-1.));
#41444=DIRECTION('ref_axis',(-4.33680868994202E-19,1.,-1.18789542670764E-48));
#41445=DIRECTION('center_axis',(5.15167520928809E-67,-1.18789542670764E-48,
-1.));
#41446=DIRECTION('ref_axis',(-4.33680868994202E-19,1.,-1.18789542670764E-48));
#41447=DIRECTION('',(-5.15167520928809E-67,1.18789542670764E-48,1.));
#41448=DIRECTION('',(5.15167520928809E-67,-1.18789542670764E-48,-1.));
#41449=DIRECTION('center_axis',(5.15167520928809E-67,-1.18789542670764E-48,
-1.));
#41450=DIRECTION('ref_axis',(-4.33680868994202E-19,1.,-1.18789542670764E-48));
#41451=DIRECTION('center_axis',(5.15167520928809E-67,-1.18789542670764E-48,
-1.));
#41452=DIRECTION('ref_axis',(-4.33680868994202E-19,1.,-1.18789542670764E-48));
#41453=DIRECTION('',(-5.15167520928809E-67,1.18789542670764E-48,1.));
#41454=DIRECTION('',(5.15167520928809E-67,-1.18789542670764E-48,-1.));
#41455=DIRECTION('center_axis',(5.15167520928809E-67,-1.18789542670764E-48,
-1.));
#41456=DIRECTION('ref_axis',(-4.33680868994202E-19,1.,-1.18789542670764E-48));
#41457=DIRECTION('center_axis',(5.15167520928809E-67,-1.18789542670764E-48,
-1.));
#41458=DIRECTION('ref_axis',(-4.33680868994202E-19,1.,-1.18789542670764E-48));
#41459=DIRECTION('',(-5.15167520928809E-67,1.18789542670764E-48,1.));
#41460=DIRECTION('',(5.15167520928809E-67,-1.18789542670764E-48,-1.));
#41461=DIRECTION('center_axis',(5.15167520928809E-67,-1.18789542670764E-48,
-1.));
#41462=DIRECTION('ref_axis',(-4.33680868994202E-19,1.,-1.18789542670764E-48));
#41463=DIRECTION('center_axis',(5.15167520928809E-67,-1.18789542670764E-48,
-1.));
#41464=DIRECTION('ref_axis',(-4.33680868994202E-19,1.,-1.18789542670764E-48));
#41465=DIRECTION('',(-5.15167520928809E-67,1.18789542670764E-48,1.));
#41466=DIRECTION('',(5.15167520928809E-67,-1.18789542670764E-48,-1.));
#41467=DIRECTION('center_axis',(5.15167520928809E-67,-1.18789542670764E-48,
-1.));
#41468=DIRECTION('ref_axis',(-4.33680868994202E-19,1.,-1.18789542670764E-48));
#41469=DIRECTION('center_axis',(5.15167520928809E-67,-1.18789542670764E-48,
-1.));
#41470=DIRECTION('ref_axis',(-4.33680868994202E-19,1.,-1.18789542670764E-48));
#41471=DIRECTION('',(-5.15167520928809E-67,1.18789542670764E-48,1.));
#41472=DIRECTION('',(5.15167520928809E-67,-1.18789542670764E-48,-1.));
#41473=DIRECTION('center_axis',(5.15167520928809E-67,-1.18789542670764E-48,
-1.));
#41474=DIRECTION('ref_axis',(-4.33680868994202E-19,1.,-1.18789542670764E-48));
#41475=DIRECTION('center_axis',(5.15167520928809E-67,-1.18789542670764E-48,
-1.));
#41476=DIRECTION('ref_axis',(-4.33680868994202E-19,1.,-1.18789542670764E-48));
#41477=DIRECTION('',(-5.15167520928809E-67,1.18789542670764E-48,1.));
#41478=DIRECTION('',(5.15167520928809E-67,-1.18789542670764E-48,-1.));
#41479=DIRECTION('center_axis',(5.15167520928809E-67,-1.18789542670764E-48,
-1.));
#41480=DIRECTION('ref_axis',(-4.33680868994202E-19,1.,-1.18789542670764E-48));
#41481=DIRECTION('center_axis',(5.15167520928809E-67,-1.18789542670764E-48,
-1.));
#41482=DIRECTION('ref_axis',(-4.33680868994202E-19,1.,-1.18789542670764E-48));
#41483=DIRECTION('',(-5.15167520928809E-67,1.18789542670764E-48,1.));
#41484=DIRECTION('',(5.15167520928809E-67,-1.18789542670764E-48,-1.));
#41485=DIRECTION('center_axis',(5.15167520928809E-67,-1.18789542670764E-48,
-1.));
#41486=DIRECTION('ref_axis',(-4.33680868994202E-19,1.,-1.18789542670764E-48));
#41487=DIRECTION('center_axis',(5.15167520928809E-67,-1.18789542670764E-48,
-1.));
#41488=DIRECTION('ref_axis',(-4.33680868994202E-19,1.,-1.18789542670764E-48));
#41489=DIRECTION('',(-5.15167520928809E-67,1.18789542670764E-48,1.));
#41490=DIRECTION('',(5.15167520928809E-67,-1.18789542670764E-48,-1.));
#41491=DIRECTION('center_axis',(5.15167520928809E-67,-1.18789542670764E-48,
-1.));
#41492=DIRECTION('ref_axis',(-4.33680868994202E-19,1.,-1.18789542670764E-48));
#41493=DIRECTION('center_axis',(5.15167520928809E-67,-1.18789542670764E-48,
-1.));
#41494=DIRECTION('ref_axis',(-4.33680868994202E-19,1.,-1.18789542670764E-48));
#41495=DIRECTION('',(-5.15167520928809E-67,1.18789542670764E-48,1.));
#41496=DIRECTION('',(5.15167520928809E-67,-1.18789542670764E-48,-1.));
#41497=DIRECTION('center_axis',(5.15167520928809E-67,-1.18789542670764E-48,
-1.));
#41498=DIRECTION('ref_axis',(-4.33680868994202E-19,1.,-1.18789542670764E-48));
#41499=DIRECTION('center_axis',(5.15167520928809E-67,-1.18789542670764E-48,
-1.));
#41500=DIRECTION('ref_axis',(-4.33680868994202E-19,1.,-1.18789542670764E-48));
#41501=DIRECTION('',(-5.15167520928809E-67,1.18789542670764E-48,1.));
#41502=DIRECTION('',(5.15167520928809E-67,-1.18789542670764E-48,-1.));
#41503=DIRECTION('center_axis',(5.15167520928809E-67,-1.18789542670764E-48,
-1.));
#41504=DIRECTION('ref_axis',(-4.33680868994202E-19,1.,-1.18789542670764E-48));
#41505=DIRECTION('center_axis',(5.15167520928809E-67,-1.18789542670764E-48,
-1.));
#41506=DIRECTION('ref_axis',(-4.33680868994202E-19,1.,-1.18789542670764E-48));
#41507=DIRECTION('',(-5.15167520928809E-67,1.18789542670764E-48,1.));
#41508=DIRECTION('',(5.15167520928809E-67,-1.18789542670764E-48,-1.));
#41509=DIRECTION('center_axis',(5.15167520928809E-67,-1.18789542670764E-48,
-1.));
#41510=DIRECTION('ref_axis',(-4.33680868994202E-19,1.,-1.18789542670764E-48));
#41511=DIRECTION('center_axis',(5.15167520928809E-67,-1.18789542670764E-48,
-1.));
#41512=DIRECTION('ref_axis',(-4.33680868994202E-19,1.,-1.18789542670764E-48));
#41513=DIRECTION('',(-5.15167520928809E-67,1.18789542670764E-48,1.));
#41514=DIRECTION('',(5.15167520928809E-67,-1.18789542670764E-48,-1.));
#41515=DIRECTION('center_axis',(5.15167520928809E-67,-1.18789542670764E-48,
-1.));
#41516=DIRECTION('ref_axis',(-4.33680868994202E-19,1.,-1.18789542670764E-48));
#41517=DIRECTION('center_axis',(5.15167520928809E-67,-1.18789542670764E-48,
-1.));
#41518=DIRECTION('ref_axis',(-4.33680868994202E-19,1.,-1.18789542670764E-48));
#41519=DIRECTION('',(-5.15167520928809E-67,1.18789542670764E-48,1.));
#41520=DIRECTION('',(5.15167520928809E-67,-1.18789542670764E-48,-1.));
#41521=DIRECTION('center_axis',(5.15167520928809E-67,-1.18789542670764E-48,
-1.));
#41522=DIRECTION('ref_axis',(-4.33680868994202E-19,1.,-1.18789542670764E-48));
#41523=DIRECTION('center_axis',(5.15167520928809E-67,-1.18789542670764E-48,
-1.));
#41524=DIRECTION('ref_axis',(-4.33680868994202E-19,1.,-1.18789542670764E-48));
#41525=DIRECTION('',(-5.15167520928809E-67,1.18789542670764E-48,1.));
#41526=DIRECTION('',(5.15167520928809E-67,-1.18789542670764E-48,-1.));
#41527=DIRECTION('center_axis',(5.15167520928809E-67,-1.18789542670764E-48,
-1.));
#41528=DIRECTION('ref_axis',(-4.33680868994202E-19,1.,-1.18789542670764E-48));
#41529=DIRECTION('center_axis',(5.15167520928809E-67,-1.18789542670764E-48,
-1.));
#41530=DIRECTION('ref_axis',(-4.33680868994202E-19,1.,-1.18789542670764E-48));
#41531=DIRECTION('',(-5.15167520928809E-67,1.18789542670764E-48,1.));
#41532=DIRECTION('',(5.15167520928809E-67,-1.18789542670764E-48,-1.));
#41533=DIRECTION('center_axis',(5.15167520928809E-67,-1.18789542670764E-48,
-1.));
#41534=DIRECTION('ref_axis',(-4.33680868994202E-19,1.,-1.18789542670764E-48));
#41535=DIRECTION('center_axis',(5.15167520928809E-67,-1.18789542670764E-48,
-1.));
#41536=DIRECTION('ref_axis',(-4.33680868994202E-19,1.,-1.18789542670764E-48));
#41537=DIRECTION('',(-5.15167520928809E-67,1.18789542670764E-48,1.));
#41538=DIRECTION('',(5.15167520928809E-67,-1.18789542670764E-48,-1.));
#41539=DIRECTION('center_axis',(5.15167520928809E-67,-1.18789542670764E-48,
-1.));
#41540=DIRECTION('ref_axis',(-4.33680868994202E-19,1.,-1.18789542670764E-48));
#41541=DIRECTION('center_axis',(5.15167520928809E-67,-1.18789542670764E-48,
-1.));
#41542=DIRECTION('ref_axis',(-4.33680868994202E-19,1.,-1.18789542670764E-48));
#41543=DIRECTION('',(-5.15167520928809E-67,1.18789542670764E-48,1.));
#41544=DIRECTION('',(5.15167520928809E-67,-1.18789542670764E-48,-1.));
#41545=DIRECTION('center_axis',(5.15167520928809E-67,-1.18789542670764E-48,
-1.));
#41546=DIRECTION('ref_axis',(-4.33680868994202E-19,1.,-1.18789542670764E-48));
#41547=DIRECTION('center_axis',(5.15167520928809E-67,-1.18789542670764E-48,
-1.));
#41548=DIRECTION('ref_axis',(-4.33680868994202E-19,1.,-1.18789542670764E-48));
#41549=DIRECTION('',(-5.15167520928809E-67,1.18789542670764E-48,1.));
#41550=DIRECTION('',(5.15167520928809E-67,-1.18789542670764E-48,-1.));
#41551=DIRECTION('center_axis',(5.15167520928809E-67,-1.18789542670764E-48,
-1.));
#41552=DIRECTION('ref_axis',(-4.33680868994202E-19,1.,-1.18789542670764E-48));
#41553=DIRECTION('center_axis',(5.15167520928809E-67,-1.18789542670764E-48,
-1.));
#41554=DIRECTION('ref_axis',(-4.33680868994202E-19,1.,-1.18789542670764E-48));
#41555=DIRECTION('',(-5.15167520928809E-67,1.18789542670764E-48,1.));
#41556=DIRECTION('',(5.15167520928809E-67,-1.18789542670764E-48,-1.));
#41557=DIRECTION('center_axis',(5.15167520928809E-67,-1.18789542670764E-48,
-1.));
#41558=DIRECTION('ref_axis',(-4.33680868994202E-19,1.,-1.18789542670764E-48));
#41559=DIRECTION('center_axis',(5.15167520928809E-67,-1.18789542670764E-48,
-1.));
#41560=DIRECTION('ref_axis',(-4.33680868994202E-19,1.,-1.18789542670764E-48));
#41561=DIRECTION('',(-5.15167520928809E-67,1.18789542670764E-48,1.));
#41562=DIRECTION('',(5.15167520928809E-67,-1.18789542670764E-48,-1.));
#41563=DIRECTION('center_axis',(5.15167520928809E-67,-1.18789542670764E-48,
-1.));
#41564=DIRECTION('ref_axis',(-4.33680868994202E-19,1.,-1.18789542670764E-48));
#41565=DIRECTION('center_axis',(5.15167520928809E-67,-1.18789542670764E-48,
-1.));
#41566=DIRECTION('ref_axis',(-4.33680868994202E-19,1.,-1.18789542670764E-48));
#41567=DIRECTION('',(-5.15167520928809E-67,1.18789542670764E-48,1.));
#41568=DIRECTION('',(5.15167520928809E-67,-1.18789542670764E-48,-1.));
#41569=DIRECTION('center_axis',(5.15167520928809E-67,-1.18789542670764E-48,
-1.));
#41570=DIRECTION('ref_axis',(-4.33680868994202E-19,1.,-1.18789542670764E-48));
#41571=DIRECTION('center_axis',(5.15167520928809E-67,-1.18789542670764E-48,
-1.));
#41572=DIRECTION('ref_axis',(-4.33680868994202E-19,1.,-1.18789542670764E-48));
#41573=DIRECTION('',(-5.15167520928809E-67,1.18789542670764E-48,1.));
#41574=DIRECTION('',(5.15167520928809E-67,-1.18789542670764E-48,-1.));
#41575=DIRECTION('center_axis',(5.15167520928809E-67,-1.18789542670764E-48,
-1.));
#41576=DIRECTION('ref_axis',(-4.33680868994202E-19,1.,-1.18789542670764E-48));
#41577=DIRECTION('center_axis',(5.15167520928809E-67,-1.18789542670764E-48,
-1.));
#41578=DIRECTION('ref_axis',(-4.33680868994202E-19,1.,-1.18789542670764E-48));
#41579=DIRECTION('',(-5.15167520928809E-67,1.18789542670764E-48,1.));
#41580=DIRECTION('',(5.15167520928809E-67,-1.18789542670764E-48,-1.));
#41581=DIRECTION('center_axis',(5.15167520928809E-67,-1.18789542670764E-48,
-1.));
#41582=DIRECTION('ref_axis',(-4.33680868994202E-19,1.,-1.18789542670764E-48));
#41583=DIRECTION('center_axis',(5.15167520928809E-67,-1.18789542670764E-48,
-1.));
#41584=DIRECTION('ref_axis',(-4.33680868994202E-19,1.,-1.18789542670764E-48));
#41585=DIRECTION('',(-5.15167520928809E-67,1.18789542670764E-48,1.));
#41586=DIRECTION('',(5.15167520928809E-67,-1.18789542670764E-48,-1.));
#41587=DIRECTION('center_axis',(5.15167520928809E-67,-1.18789542670764E-48,
-1.));
#41588=DIRECTION('ref_axis',(-4.33680868994202E-19,1.,-1.18789542670764E-48));
#41589=DIRECTION('center_axis',(5.15167520928809E-67,-1.18789542670764E-48,
-1.));
#41590=DIRECTION('ref_axis',(-4.33680868994202E-19,1.,-1.18789542670764E-48));
#41591=DIRECTION('',(-5.15167520928809E-67,1.18789542670764E-48,1.));
#41592=DIRECTION('',(5.15167520928809E-67,-1.18789542670764E-48,-1.));
#41593=DIRECTION('center_axis',(5.15167520928809E-67,-1.18789542670764E-48,
-1.));
#41594=DIRECTION('ref_axis',(-4.33680868994202E-19,1.,-1.18789542670764E-48));
#41595=DIRECTION('center_axis',(5.15167520928809E-67,-1.18789542670764E-48,
-1.));
#41596=DIRECTION('ref_axis',(-4.33680868994202E-19,1.,-1.18789542670764E-48));
#41597=DIRECTION('',(-5.15167520928809E-67,1.18789542670764E-48,1.));
#41598=DIRECTION('',(5.15167520928809E-67,-1.18789542670764E-48,-1.));
#41599=DIRECTION('center_axis',(5.15167520928809E-67,-1.18789542670764E-48,
-1.));
#41600=DIRECTION('ref_axis',(-4.33680868994202E-19,1.,-1.18789542670764E-48));
#41601=DIRECTION('center_axis',(5.15167520928809E-67,-1.18789542670764E-48,
-1.));
#41602=DIRECTION('ref_axis',(-4.33680868994202E-19,1.,-1.18789542670764E-48));
#41603=DIRECTION('',(-5.15167520928809E-67,1.18789542670764E-48,1.));
#41604=DIRECTION('',(5.15167520928809E-67,-1.18789542670764E-48,-1.));
#41605=DIRECTION('center_axis',(5.15167520928809E-67,-1.18789542670764E-48,
-1.));
#41606=DIRECTION('ref_axis',(-4.33680868994202E-19,1.,-1.18789542670764E-48));
#41607=DIRECTION('center_axis',(5.15167520928809E-67,-1.18789542670764E-48,
-1.));
#41608=DIRECTION('ref_axis',(-4.33680868994202E-19,1.,-1.18789542670764E-48));
#41609=DIRECTION('',(-5.15167520928809E-67,1.18789542670764E-48,1.));
#41610=DIRECTION('',(5.15167520928809E-67,-1.18789542670764E-48,-1.));
#41611=DIRECTION('center_axis',(5.15167520928809E-67,-1.18789542670764E-48,
-1.));
#41612=DIRECTION('ref_axis',(-4.33680868994202E-19,1.,-1.18789542670764E-48));
#41613=DIRECTION('center_axis',(5.15167520928809E-67,-1.18789542670764E-48,
-1.));
#41614=DIRECTION('ref_axis',(-4.33680868994202E-19,1.,-1.18789542670764E-48));
#41615=DIRECTION('',(-5.15167520928809E-67,1.18789542670764E-48,1.));
#41616=DIRECTION('',(5.15167520928809E-67,-1.18789542670764E-48,-1.));
#41617=DIRECTION('center_axis',(5.15167520928809E-67,-1.18789542670764E-48,
-1.));
#41618=DIRECTION('ref_axis',(-4.33680868994202E-19,1.,-1.18789542670764E-48));
#41619=DIRECTION('center_axis',(5.15167520928809E-67,-1.18789542670764E-48,
-1.));
#41620=DIRECTION('ref_axis',(-4.33680868994202E-19,1.,-1.18789542670764E-48));
#41621=DIRECTION('',(-5.15167520928809E-67,1.18789542670764E-48,1.));
#41622=DIRECTION('',(5.15167520928809E-67,-1.18789542670764E-48,-1.));
#41623=DIRECTION('center_axis',(5.15167520928809E-67,-1.18789542670764E-48,
-1.));
#41624=DIRECTION('ref_axis',(-4.33680868994202E-19,1.,-1.18789542670764E-48));
#41625=DIRECTION('center_axis',(5.15167520928809E-67,-1.18789542670764E-48,
-1.));
#41626=DIRECTION('ref_axis',(-4.33680868994202E-19,1.,-1.18789542670764E-48));
#41627=DIRECTION('',(-5.15167520928809E-67,1.18789542670764E-48,1.));
#41628=DIRECTION('',(5.15167520928809E-67,-1.18789542670764E-48,-1.));
#41629=DIRECTION('center_axis',(5.15167520928809E-67,-1.18789542670764E-48,
-1.));
#41630=DIRECTION('ref_axis',(-4.33680868994202E-19,1.,-1.18789542670764E-48));
#41631=DIRECTION('center_axis',(5.15167520928809E-67,-1.18789542670764E-48,
-1.));
#41632=DIRECTION('ref_axis',(-4.33680868994202E-19,1.,-1.18789542670764E-48));
#41633=DIRECTION('',(-5.15167520928809E-67,1.18789542670764E-48,1.));
#41634=DIRECTION('',(5.15167520928809E-67,-1.18789542670764E-48,-1.));
#41635=DIRECTION('center_axis',(5.15167520928809E-67,-1.18789542670764E-48,
-1.));
#41636=DIRECTION('ref_axis',(-4.33680868994202E-19,1.,-1.18789542670764E-48));
#41637=DIRECTION('center_axis',(5.15167520928809E-67,-1.18789542670764E-48,
-1.));
#41638=DIRECTION('ref_axis',(-4.33680868994202E-19,1.,-1.18789542670764E-48));
#41639=DIRECTION('',(-5.15167520928809E-67,1.18789542670764E-48,1.));
#41640=DIRECTION('',(5.15167520928809E-67,-1.18789542670764E-48,-1.));
#41641=DIRECTION('center_axis',(5.15167520928809E-67,-1.18789542670764E-48,
-1.));
#41642=DIRECTION('ref_axis',(-4.33680868994202E-19,1.,-1.18789542670764E-48));
#41643=DIRECTION('center_axis',(5.15167520928809E-67,-1.18789542670764E-48,
-1.));
#41644=DIRECTION('ref_axis',(-4.33680868994202E-19,1.,-1.18789542670764E-48));
#41645=DIRECTION('',(-5.15167520928809E-67,1.18789542670764E-48,1.));
#41646=DIRECTION('',(5.15167520928809E-67,-1.18789542670764E-48,-1.));
#41647=DIRECTION('center_axis',(5.15167520928809E-67,-1.18789542670764E-48,
-1.));
#41648=DIRECTION('ref_axis',(-4.33680868994202E-19,1.,-1.18789542670764E-48));
#41649=DIRECTION('center_axis',(5.15167520928809E-67,-1.18789542670764E-48,
-1.));
#41650=DIRECTION('ref_axis',(-4.33680868994202E-19,1.,-1.18789542670764E-48));
#41651=DIRECTION('',(-5.15167520928809E-67,1.18789542670764E-48,1.));
#41652=DIRECTION('',(5.15167520928809E-67,-1.18789542670764E-48,-1.));
#41653=DIRECTION('center_axis',(5.15167520928809E-67,-1.18789542670764E-48,
-1.));
#41654=DIRECTION('ref_axis',(-4.33680868994202E-19,1.,-1.18789542670764E-48));
#41655=DIRECTION('center_axis',(5.15167520928809E-67,-1.18789542670764E-48,
-1.));
#41656=DIRECTION('ref_axis',(-4.33680868994202E-19,1.,-1.18789542670764E-48));
#41657=DIRECTION('',(-5.15167520928809E-67,1.18789542670764E-48,1.));
#41658=DIRECTION('',(5.15167520928809E-67,-1.18789542670764E-48,-1.));
#41659=DIRECTION('center_axis',(5.15167520928809E-67,-1.18789542670764E-48,
-1.));
#41660=DIRECTION('ref_axis',(-4.33680868994202E-19,1.,-1.18789542670764E-48));
#41661=DIRECTION('center_axis',(5.15167520928809E-67,-1.18789542670764E-48,
-1.));
#41662=DIRECTION('ref_axis',(-4.33680868994202E-19,1.,-1.18789542670764E-48));
#41663=DIRECTION('',(-5.15167520928809E-67,1.18789542670764E-48,1.));
#41664=DIRECTION('',(5.15167520928809E-67,-1.18789542670764E-48,-1.));
#41665=DIRECTION('center_axis',(5.15167520928809E-67,-1.18789542670764E-48,
-1.));
#41666=DIRECTION('ref_axis',(-4.33680868994202E-19,1.,-1.18789542670764E-48));
#41667=DIRECTION('center_axis',(5.15167520928809E-67,-1.18789542670764E-48,
-1.));
#41668=DIRECTION('ref_axis',(-4.33680868994202E-19,1.,-1.18789542670764E-48));
#41669=DIRECTION('',(-5.15167520928809E-67,1.18789542670764E-48,1.));
#41670=DIRECTION('',(5.15167520928809E-67,-1.18789542670764E-48,-1.));
#41671=DIRECTION('center_axis',(5.15167520928809E-67,-1.18789542670764E-48,
-1.));
#41672=DIRECTION('ref_axis',(-4.33680868994202E-19,1.,-1.18789542670764E-48));
#41673=DIRECTION('center_axis',(5.15167520928809E-67,-1.18789542670764E-48,
-1.));
#41674=DIRECTION('ref_axis',(-4.33680868994202E-19,1.,-1.18789542670764E-48));
#41675=DIRECTION('',(5.15167520928809E-67,-1.18789542670764E-48,-1.));
#41676=DIRECTION('center_axis',(5.15167520928809E-67,-1.18789542670764E-48,
-1.));
#41677=DIRECTION('ref_axis',(-4.33680868994202E-19,1.,-1.18789542670764E-48));
#41678=DIRECTION('',(-5.15167520928809E-67,1.18789542670764E-48,1.));
#41679=DIRECTION('center_axis',(5.15167520928809E-67,-1.18789542670764E-48,
-1.));
#41680=DIRECTION('ref_axis',(-4.33680868994202E-19,1.,-1.18789542670764E-48));
#41681=DIRECTION('',(5.15167520928809E-67,-1.18789542670764E-48,-1.));
#41682=DIRECTION('center_axis',(5.15167520928809E-67,-1.18789542670764E-48,
-1.));
#41683=DIRECTION('ref_axis',(-4.33680868994202E-19,1.,-1.18789542670764E-48));
#41684=DIRECTION('',(-5.15167520928809E-67,1.18789542670764E-48,1.));
#41685=DIRECTION('center_axis',(5.15167520928809E-67,-1.18789542670764E-48,
-1.));
#41686=DIRECTION('ref_axis',(-4.33680868994202E-19,1.,-1.18789542670764E-48));
#41687=DIRECTION('',(5.15167520928809E-67,-1.18789542670764E-48,-1.));
#41688=DIRECTION('center_axis',(5.15167520928809E-67,-1.18789542670764E-48,
-1.));
#41689=DIRECTION('ref_axis',(-4.33680868994202E-19,1.,-1.18789542670764E-48));
#41690=DIRECTION('',(-5.15167520928809E-67,1.18789542670764E-48,1.));
#41691=DIRECTION('center_axis',(5.15167520928809E-67,-1.18789542670764E-48,
-1.));
#41692=DIRECTION('ref_axis',(-4.33680868994202E-19,1.,-1.18789542670764E-48));
#41693=DIRECTION('',(5.15167520928809E-67,-1.18789542670764E-48,-1.));
#41694=DIRECTION('center_axis',(5.15167520928809E-67,-1.18789542670764E-48,
-1.));
#41695=DIRECTION('ref_axis',(-4.33680868994202E-19,1.,-1.18789542670764E-48));
#41696=DIRECTION('',(-5.15167520928809E-67,1.18789542670764E-48,1.));
#41697=DIRECTION('center_axis',(5.15167520928809E-67,-1.18789542670764E-48,
-1.));
#41698=DIRECTION('ref_axis',(-4.33680868994202E-19,1.,-1.18789542670764E-48));
#41699=DIRECTION('',(5.15167520928809E-67,-1.18789542670764E-48,-1.));
#41700=DIRECTION('center_axis',(5.15167520928809E-67,-1.18789542670764E-48,
-1.));
#41701=DIRECTION('ref_axis',(-4.33680868994202E-19,1.,-1.18789542670764E-48));
#41702=DIRECTION('',(-5.15167520928809E-67,1.18789542670764E-48,1.));
#41703=DIRECTION('center_axis',(5.15167520928809E-67,-1.18789542670764E-48,
-1.));
#41704=DIRECTION('ref_axis',(-4.33680868994202E-19,1.,-1.18789542670764E-48));
#41705=DIRECTION('',(5.15167520928809E-67,-1.18789542670764E-48,-1.));
#41706=DIRECTION('center_axis',(5.15167520928809E-67,-1.18789542670764E-48,
-1.));
#41707=DIRECTION('ref_axis',(-4.33680868994202E-19,1.,-1.18789542670764E-48));
#41708=DIRECTION('',(-5.15167520928809E-67,1.18789542670764E-48,1.));
#41709=DIRECTION('center_axis',(5.15167520928809E-67,-1.18789542670764E-48,
-1.));
#41710=DIRECTION('ref_axis',(-4.33680868994202E-19,1.,-1.18789542670764E-48));
#41711=DIRECTION('',(5.15167520928809E-67,-1.18789542670764E-48,-1.));
#41712=DIRECTION('center_axis',(5.15167520928809E-67,-1.18789542670764E-48,
-1.));
#41713=DIRECTION('ref_axis',(-4.33680868994202E-19,1.,-1.18789542670764E-48));
#41714=DIRECTION('',(-5.15167520928809E-67,1.18789542670764E-48,1.));
#41715=DIRECTION('center_axis',(5.15167520928809E-67,-1.18789542670764E-48,
-1.));
#41716=DIRECTION('ref_axis',(-4.33680868994202E-19,1.,-1.18789542670764E-48));
#41717=DIRECTION('',(5.15167520928809E-67,-1.18789542670764E-48,-1.));
#41718=DIRECTION('center_axis',(5.15167520928809E-67,-1.18789542670764E-48,
-1.));
#41719=DIRECTION('ref_axis',(-4.33680868994202E-19,1.,-1.18789542670764E-48));
#41720=DIRECTION('',(-5.15167520928809E-67,1.18789542670764E-48,1.));
#41721=DIRECTION('center_axis',(5.15167520928809E-67,-1.18789542670764E-48,
-1.));
#41722=DIRECTION('ref_axis',(-4.33680868994202E-19,1.,-1.18789542670764E-48));
#41723=DIRECTION('',(5.15167520928809E-67,-1.18789542670764E-48,-1.));
#41724=DIRECTION('center_axis',(5.15167520928809E-67,-1.18789542670764E-48,
-1.));
#41725=DIRECTION('ref_axis',(-4.33680868994202E-19,1.,-1.18789542670764E-48));
#41726=DIRECTION('',(-5.15167520928809E-67,1.18789542670764E-48,1.));
#41727=DIRECTION('center_axis',(5.15167520928809E-67,-1.18789542670764E-48,
-1.));
#41728=DIRECTION('ref_axis',(-4.33680868994202E-19,1.,-1.18789542670764E-48));
#41729=DIRECTION('',(5.15167520928809E-67,-1.18789542670764E-48,-1.));
#41730=DIRECTION('center_axis',(5.15167520928809E-67,-1.18789542670764E-48,
-1.));
#41731=DIRECTION('ref_axis',(-4.33680868994202E-19,1.,-1.18789542670764E-48));
#41732=DIRECTION('',(-5.15167520928809E-67,1.18789542670764E-48,1.));
#41733=DIRECTION('center_axis',(5.15167520928809E-67,-1.18789542670764E-48,
-1.));
#41734=DIRECTION('ref_axis',(-4.33680868994202E-19,1.,-1.18789542670764E-48));
#41735=DIRECTION('',(5.15167520928809E-67,-1.18789542670764E-48,-1.));
#41736=DIRECTION('center_axis',(5.15167520928809E-67,-1.18789542670764E-48,
-1.));
#41737=DIRECTION('ref_axis',(-4.33680868994202E-19,1.,-1.18789542670764E-48));
#41738=DIRECTION('',(-5.15167520928809E-67,1.18789542670764E-48,1.));
#41739=DIRECTION('center_axis',(5.15167520928809E-67,-1.18789542670764E-48,
-1.));
#41740=DIRECTION('ref_axis',(-4.33680868994202E-19,1.,-1.18789542670764E-48));
#41741=DIRECTION('',(5.15167520928809E-67,-1.18789542670764E-48,-1.));
#41742=DIRECTION('center_axis',(5.15167520928809E-67,-1.18789542670764E-48,
-1.));
#41743=DIRECTION('ref_axis',(-4.33680868994202E-19,1.,-1.18789542670764E-48));
#41744=DIRECTION('',(-5.15167520928809E-67,1.18789542670764E-48,1.));
#41745=DIRECTION('center_axis',(5.15167520928809E-67,-1.18789542670764E-48,
-1.));
#41746=DIRECTION('ref_axis',(-4.33680868994202E-19,1.,-1.18789542670764E-48));
#41747=DIRECTION('',(5.15167520928809E-67,-1.18789542670764E-48,-1.));
#41748=DIRECTION('center_axis',(5.15167520928809E-67,-1.18789542670764E-48,
-1.));
#41749=DIRECTION('ref_axis',(-4.33680868994202E-19,1.,-1.18789542670764E-48));
#41750=DIRECTION('',(-5.15167520928809E-67,1.18789542670764E-48,1.));
#41751=DIRECTION('center_axis',(5.15167520928809E-67,-1.18789542670764E-48,
-1.));
#41752=DIRECTION('ref_axis',(-4.33680868994202E-19,1.,-1.18789542670764E-48));
#41753=DIRECTION('',(5.15167520928809E-67,-1.18789542670764E-48,-1.));
#41754=DIRECTION('center_axis',(5.15167520928809E-67,-1.18789542670764E-48,
-1.));
#41755=DIRECTION('ref_axis',(-4.33680868994202E-19,1.,-1.18789542670764E-48));
#41756=DIRECTION('',(-5.15167520928809E-67,1.18789542670764E-48,1.));
#41757=DIRECTION('center_axis',(5.15167520928809E-67,-1.18789542670764E-48,
-1.));
#41758=DIRECTION('ref_axis',(-4.33680868994202E-19,1.,-1.18789542670764E-48));
#41759=DIRECTION('',(-5.15167520928809E-67,1.18789542670764E-48,1.));
#41760=DIRECTION('',(5.15167520928809E-67,-1.18789542670764E-48,-1.));
#41761=DIRECTION('center_axis',(5.15167520928809E-67,-1.18789542670764E-48,
-1.));
#41762=DIRECTION('ref_axis',(-4.33680868994202E-19,1.,-1.18789542670764E-48));
#41763=DIRECTION('center_axis',(5.15167520928809E-67,-1.18789542670764E-48,
-1.));
#41764=DIRECTION('ref_axis',(0.,1.,0.));
#41765=DIRECTION('center_axis',(-0.726718511656259,-0.686935363550879,-0.000105448246390915));
#41766=DIRECTION('ref_axis',(0.686885008270217,-0.726663364190208,-0.0122204974282148));
#41767=DIRECTION('center_axis',(0.0503511057571476,0.998731574514185,-9.06501463958382E-5));
#41768=DIRECTION('ref_axis',(0.998626750226923,-0.0503471356586858,-0.0144837723739379));
#41769=DIRECTION('center_axis',(5.15167520928809E-67,-1.18789542670764E-48,
-1.));
#41770=DIRECTION('ref_axis',(0.,1.,0.));
#41771=DIRECTION('center_axis',(-0.0281636861094737,0.999603320606368,-9.06501463234301E-5));
#41772=DIRECTION('ref_axis',(0.999498507968587,0.0281594195507115,-0.0144837722688343));
#41773=DIRECTION('center_axis',(-0.670581953565459,-0.741835448352935,-0.000105448247414229));
#41774=DIRECTION('ref_axis',(0.741780921484837,-0.670530926934418,-0.0122204969447688));
#41775=DIRECTION('center_axis',(5.15167520928809E-67,-1.18789542670764E-48,
-1.));
#41776=DIRECTION('ref_axis',(0.,1.,0.));
#41777=DIRECTION('center_axis',(-0.106504839485416,0.994312179825198,-9.06501464431132E-5));
#41778=DIRECTION('ref_axis',(0.994208025038947,0.106492362574112,-0.014483772351861));
#41779=DIRECTION('center_axis',(-0.610311034741592,-0.792161870928735,-0.000105448247339917));
#41780=DIRECTION('ref_axis',(0.792103508645573,-0.610264443537491,-0.0122204969313235));
#41781=DIRECTION('center_axis',(5.15167520928809E-67,-1.18789542670764E-48,
-1.));
#41782=DIRECTION('ref_axis',(0.,1.,0.));
#41783=DIRECTION('center_axis',(-0.184189355109993,0.982890773812999,-9.06501463311491E-5));
#41784=DIRECTION('ref_axis',(0.982787919029266,0.184168744770673,-0.0144837722890199));
#41785=DIRECTION('center_axis',(-0.546277345439217,-0.837604352149957,-0.000105448247410497));
#41786=DIRECTION('ref_axis',(0.837542514274823,-0.546235476912428,-0.0122204968991007));
#41787=DIRECTION('center_axis',(5.15167520928809E-67,-1.18789542670764E-48,
-1.));
#41788=DIRECTION('ref_axis',(0.,1.,0.));
#41789=DIRECTION('center_axis',(-0.260738282110594,0.965409519336,-9.0650146457266E-5));
#41790=DIRECTION('ref_axis',(0.965308598686112,0.260709665412272,-0.0144837724117514));
#41791=DIRECTION('center_axis',(-0.478875674647023,-0.877882724008182,-0.000105448247224529));
#41792=DIRECTION('ref_axis',(0.877817791791478,-0.478838786930502,-0.0122204969317693));
#41793=DIRECTION('center_axis',(5.15167520928809E-67,-1.18789542670764E-48,
-1.));
#41794=DIRECTION('ref_axis',(0.,1.,0.));
#41795=DIRECTION('center_axis',(-0.335679670898074,0.941976194140973,-9.06501464082373E-5));
#41796=DIRECTION('ref_axis',(0.941877829837014,0.335643224272907,-0.014483772340284));
#41797=DIRECTION('center_axis',(-0.40852157607848,-0.912748656947257,-0.000105448246964389));
#41798=DIRECTION('ref_axis',(0.912681030716442,-0.408489896596762,-0.0122204970741974));
#41799=DIRECTION('center_axis',(5.15167520928809E-67,-1.18789542670764E-48,
-1.));
#41800=DIRECTION('ref_axis',(0.,1.,0.));
#41801=DIRECTION('center_axis',(-0.408551482889657,0.91273527247018,-9.06501463992171E-5));
#41802=DIRECTION('ref_axis',(0.91264007096006,0.408507431043052,-0.014483772320157));
#41803=DIRECTION('center_axis',(-0.335648806144879,-0.941987190897087,-0.000105448247367288));
#41804=DIRECTION('ref_axis',(0.941917287594001,-0.335622530214118,-0.0122204968897907));
#41805=DIRECTION('center_axis',(5.15167520928809E-67,-1.18789542670764E-48,
-1.));
#41806=DIRECTION('ref_axis',(0.,1.,0.));
#41807=DIRECTION('center_axis',(-0.478904439132113,0.877867034329292,-9.06501463430316E-5));
#41808=DIRECTION('ref_axis',(0.877775582560928,0.478853053657823,-0.0144837723815965));
#41809=DIRECTION('center_axis',(-0.260706649707894,-0.965418060572078,-0.000105448247265905));
#41810=DIRECTION('ref_axis',(0.965346311170054,-0.260685939326527,-0.0122204970363453));
#41811=DIRECTION('center_axis',(5.15167520928809E-67,-1.18789542670764E-48,
-1.));
#41812=DIRECTION('ref_axis',(0.,1.,0.));
#41813=DIRECTION('center_axis',(-0.546304790255147,0.837586454001514,-9.06501464163507E-5));
#41814=DIRECTION('ref_axis',(0.837499315806636,0.546246387962313,-0.0144837723519214));
#41815=DIRECTION('center_axis',(-0.184157150081311,-0.982896806869672,-0.00010544824733539));
#41816=DIRECTION('ref_axis',(0.982823653730718,-0.184142132936614,-0.012220496919376));
#41817=DIRECTION('center_axis',(5.15167520928809E-67,-1.18789542670764E-48,
-1.));
#41818=DIRECTION('ref_axis',(0.,1.,0.));
#41819=DIRECTION('center_axis',(-0.610336990681852,0.792141874658809,-9.06501463120476E-5));
#41820=DIRECTION('ref_axis',(0.792059587273495,0.610271931640219,-0.0144837723075503));
#41821=DIRECTION('center_axis',(-0.106472260385922,-0.994315667506542,-0.000105448247451369));
#41822=DIRECTION('ref_axis',(0.994241561642557,-0.106463029063183,-0.0122204969318448));
#41823=DIRECTION('center_axis',(5.15167520928809E-67,-1.18789542670764E-48,
-1.));
#41824=DIRECTION('ref_axis',(0.,1.,0.));
#41825=DIRECTION('center_axis',(-0.670606260603123,0.741813477245087,-9.06501463072396E-5));
#41826=DIRECTION('ref_axis',(0.741736547997548,0.670534945922644,-0.0144837723400245));
#41827=DIRECTION('center_axis',(-0.0281309338001256,-0.999604241409669,
-0.000105448247349234));
#41828=DIRECTION('ref_axis',(0.999529639708615,-0.0281275452135709,-0.012220496889411));
#41829=DIRECTION('center_axis',(5.15167520928809E-67,-1.18789542670764E-48,
-1.));
#41830=DIRECTION('ref_axis',(0.,1.,0.));
#41831=DIRECTION('center_axis',(-0.726741019928497,0.686911553066215,-9.0650146372247E-5));
#41832=DIRECTION('ref_axis',(0.686840456250864,0.726663889287803,-0.014483772375632));
#41833=DIRECTION('center_axis',(0.0503838293471008,-0.9987299227624,-0.000105448247268434));
#41834=DIRECTION('ref_axis',(0.998655285167451,0.0503813543057433,-0.0122204969390446));
#41835=DIRECTION('center_axis',(5.15167520928809E-67,-1.18789542670764E-48,
-1.));
#41836=DIRECTION('ref_axis',(0.,1.,0.));
#41837=DIRECTION('center_axis',(-0.77839517919999,0.627774590741587,-9.06501465192481E-5));
#41838=DIRECTION('ref_axis',(0.62770976469511,0.778312708136478,-0.0144837722873138));
#41839=DIRECTION('center_axis',(0.128587959432554,-0.991698102029866,-0.000105448247403937));
#41840=DIRECTION('ref_axis',(0.991623888707038,0.128579636022696,-0.0122204969540051));
#41841=DIRECTION('center_axis',(5.15167520928809E-67,-1.18789542670764E-48,
-1.));
#41842=DIRECTION('ref_axis',(0.,1.,0.));
#41843=DIRECTION('center_axis',(-0.825250273349494,0.564767189308247,-9.06501463546308E-5));
#41844=DIRECTION('ref_axis',(0.564709033703414,0.82516297032304,-0.0144837723475052));
#41845=DIRECTION('center_axis',(0.205999301987418,-0.978552132725367,-0.000105448247113811));
#41846=DIRECTION('ref_axis',(0.978478801224233,0.205985181525565,-0.0122204969893998));
#41847=DIRECTION('center_axis',(5.15167520928809E-67,-1.18789542670764E-48,
-1.));
#41848=DIRECTION('ref_axis',(0.,1.,0.));
#41849=DIRECTION('center_axis',(-0.867017425140065,0.498277810348848,-9.06501462870057E-5));
#41850=DIRECTION('ref_axis',(0.498226683734515,0.866925828402957,-0.0144837723937473));
#41851=DIRECTION('center_axis',(0.282140590344591,-0.959373064120873,-0.000105448247263863));
#41852=DIRECTION('ref_axis',(0.959301066555575,0.282120759888322,-0.0122204969363817));
#41853=DIRECTION('center_axis',(5.15167520928809E-67,-1.18789542670764E-48,
-1.));
#41854=DIRECTION('ref_axis',(0.,1.,0.));
#41855=DIRECTION('center_axis',(-0.903439126191882,0.428716382994866,-9.06501464245823E-5));
#41856=DIRECTION('ref_axis',(0.42867260058449,0.903343800470088,-0.0144837723120868));
#41857=DIRECTION('center_axis',(0.356542388140961,-0.934279141552142,-0.000105448247299974));
#41858=DIRECTION('ref_axis',(0.934208921811354,0.356516969951643,-0.0122204969034503));
#41859=DIRECTION('center_axis',(5.15167520928809E-67,-1.18789542670764E-48,
-1.));
#41860=DIRECTION('ref_axis',(0.,1.,0.));
#41861=DIRECTION('center_axis',(-0.934290824606917,0.356511776576704,-9.06501463905499E-5));
#41862=DIRECTION('ref_axis',(0.356475608302988,0.934192357614636,-0.0144837722787681));
#41863=DIRECTION('center_axis',(0.428745983551553,-0.903425077396614,-0.000105448247174382));
#41864=DIRECTION('ref_axis',(0.903357068407879,0.428715134340607,-0.0122204969145006));
#41865=DIRECTION('center_axis',(5.15167520928809E-67,-1.18789542670764E-48,
-1.));
#41866=DIRECTION('ref_axis',(0.,1.,0.));
#41867=DIRECTION('center_axis',(-0.959382309405018,0.282109156503729,-9.06501463332588E-5));
#41868=DIRECTION('ref_axis',(0.282080825355611,0.959281308222547,-0.0144837723517365));
#41869=DIRECTION('center_axis',(0.498306217395032,-0.867001097223137,-0.000105448243846677));
#41870=DIRECTION('ref_axis',(0.866935718268405,0.498270127348975,-0.0122204984383232));
#41871=DIRECTION('center_axis',(5.15167520928809E-67,-1.18789542670764E-48,
-1.));
#41872=DIRECTION('ref_axis',(0.,1.,0.));
#41873=DIRECTION('center_axis',(-0.978558883238511,0.205967239670656,-9.06501465473592E-5));
#41874=DIRECTION('ref_axis',(0.205946920319669,0.978455970573743,-0.0144837722792749));
#41875=DIRECTION('center_axis',(0.564794227716619,-0.825231766971349,-0.000105448246777006));
#41876=DIRECTION('ref_axis',(0.825169421163283,0.564753119359096,-0.01222049717581));
#41877=DIRECTION('center_axis',(5.15167520928809E-67,-1.18789542670764E-48,
-1.));
#41878=DIRECTION('ref_axis',(0.,1.,0.));
#41879=DIRECTION('center_axis',(-0.991702316153162,0.128555466313202,-9.0650146420716E-5));
#41880=DIRECTION('ref_axis',(0.128543284034494,0.991598126494967,-0.0144837723435229));
#41881=DIRECTION('center_axis',(0.627800093806525,-0.778374608461238,-0.000105448247294656));
#41882=DIRECTION('ref_axis',(0.778315680171741,0.627754220578766,-0.012220496894383));
#41883=DIRECTION('center_axis',(5.15167520928809E-67,-1.18789542670764E-48,
-1.));
#41884=DIRECTION('ref_axis',(0.,1.,0.));
#41885=DIRECTION('center_axis',(-0.998731574514195,0.0503511057569474,-9.06501463044587E-5));
#41886=DIRECTION('ref_axis',(0.0503471356585215,0.998626750227776,-0.0144837723156803));
#41887=DIRECTION('center_axis',(0.686935363552588,-0.726718511654644,-0.000105448247440854));
#41888=DIRECTION('ref_axis',(0.726663364192637,0.6868850082757,-0.0122204969756106));
#41889=DIRECTION('center_axis',(5.15167520928809E-67,-1.18789542670764E-48,
-1.));
#41890=DIRECTION('ref_axis',(0.,1.,0.));
#41891=DIRECTION('center_axis',(-0.99960332060638,-0.0281636861090561,-9.06501465204533E-5));
#41892=DIRECTION('ref_axis',(0.0281594195503036,-0.999498507968962,0.0144837722437162));
#41893=DIRECTION('center_axis',(0.741835448352776,-0.670581953565635,-0.000105448247295083));
#41894=DIRECTION('ref_axis',(0.67053092693442,0.741780921484487,-0.0122204969658991));
#41895=DIRECTION('center_axis',(5.15167520928809E-67,-1.18789542670764E-48,
-1.));
#41896=DIRECTION('ref_axis',(0.,1.,0.));
#41897=DIRECTION('center_axis',(-0.994312179825187,-0.106504839485521,-9.0650146389517E-5));
#41898=DIRECTION('ref_axis',(0.106492362574174,-0.994208025038546,0.0144837723789195));
#41899=DIRECTION('center_axis',(0.792161870927703,-0.610311034742932,-0.000105448246562834));
#41900=DIRECTION('ref_axis',(0.610264443536631,0.792103508641721,-0.0122204972240042));
#41901=DIRECTION('center_axis',(5.15167520928809E-67,-1.18789542670764E-48,
-1.));
#41902=DIRECTION('ref_axis',(0.,1.,0.));
#41903=DIRECTION('center_axis',(-0.982890773812962,-0.18418935511019,-9.06501462458389E-5));
#41904=DIRECTION('ref_axis',(0.184168744770736,-0.982787919028534,0.0144837723378535));
#41905=DIRECTION('center_axis',(0.837604352149828,-0.546277345439416,-0.000105448247288724));
#41906=DIRECTION('ref_axis',(0.546235476912052,0.837542514273825,-0.0122204969843265));
#41907=DIRECTION('center_axis',(5.15167520928809E-67,-1.18789542670764E-48,
-1.));
#41908=DIRECTION('ref_axis',(0.,1.,0.));
#41909=DIRECTION('center_axis',(-0.965409519335916,-0.260738282110905,-9.06501463158079E-5));
#41910=DIRECTION('ref_axis',(0.260709665413015,-0.965308598687581,0.0144837723005081));
#41911=DIRECTION('center_axis',(0.877882724007609,-0.478875674648073,-0.000105448246644854));
#41912=DIRECTION('ref_axis',(0.47883878693024,0.877817791788535,-0.012220497153411));
#41913=DIRECTION('center_axis',(5.15167520928809E-67,-1.18789542670764E-48,
-1.));
#41914=DIRECTION('ref_axis',(0.,1.,0.));
#41915=DIRECTION('center_axis',(-0.941976194141077,-0.335679670897783,-9.06501465752214E-5));
#41916=DIRECTION('ref_axis',(0.335643224272825,-0.941877829837701,0.0144837722974511));
#41917=DIRECTION('center_axis',(0.912748656947635,-0.408521576077636,-0.000105448247395522));
#41918=DIRECTION('ref_axis',(0.408489896596716,0.912681030718573,-0.0122204969165703));
#41919=DIRECTION('center_axis',(5.15167520928809E-67,-1.18789542670764E-48,
-1.));
#41920=DIRECTION('ref_axis',(0.,1.,0.));
#41921=DIRECTION('center_axis',(-0.912735272470059,-0.408551482889927,-9.0650146236208E-5));
#41922=DIRECTION('ref_axis',(0.408507431042893,-0.912640070958992,0.0144837723919199));
#41923=DIRECTION('center_axis',(0.941987190897161,-0.335648806144671,-0.000105448247475279));
#41924=DIRECTION('ref_axis',(0.335622530214028,0.941917287594399,-0.0122204968616106));
#41925=DIRECTION('center_axis',(5.15167520928809E-67,-1.18789542670764E-48,
-1.));
#41926=DIRECTION('ref_axis',(0.,1.,0.));
#41927=DIRECTION('center_axis',(-0.877867034329361,-0.478904439131988,-9.06501463610722E-5));
#41928=DIRECTION('ref_axis',(0.478853053657853,-0.877775582561276,0.0144837723595397));
#41929=DIRECTION('center_axis',(0.965418060572122,-0.260706649707733,-0.000105448247352975));
#41930=DIRECTION('ref_axis',(0.260685939326823,0.965346311171741,-0.012220496896787));
#41931=DIRECTION('center_axis',(5.15167520928809E-67,-1.18789542670764E-48,
-1.));
#41932=DIRECTION('ref_axis',(0.,1.,0.));
#41933=DIRECTION('center_axis',(-0.837586454001461,-0.546304790255229,-9.06501463408637E-5));
#41934=DIRECTION('ref_axis',(0.54624638796239,-0.837499315806573,0.0144837723526967));
#41935=DIRECTION('center_axis',(0.982896806869685,-0.184157150081241,-0.000105448247384682));
#41936=DIRECTION('ref_axis',(0.184142132936524,0.982823653730634,-0.0122204969274716));
#41937=DIRECTION('center_axis',(5.15167520928809E-67,-1.18789542670764E-48,
-1.));
#41938=DIRECTION('ref_axis',(0.,1.,0.));
#41939=DIRECTION('center_axis',(-0.792141874658961,-0.610336990681655,-9.06501464140886E-5));
#41940=DIRECTION('ref_axis',(0.610271931639049,-0.792059587272402,0.0144837724166105));
#41941=DIRECTION('center_axis',(0.994315667506523,-0.1064722603861,-0.000105448247372999));
#41942=DIRECTION('ref_axis',(0.106463029063429,0.994241561643113,-0.0122204968844733));
#41943=DIRECTION('center_axis',(5.15167520928809E-67,-1.18789542670764E-48,
-1.));
#41944=DIRECTION('ref_axis',(0.,1.,0.));
#41945=DIRECTION('center_axis',(-0.741813477245026,-0.670606260603191,-9.06501462657205E-5));
#41946=DIRECTION('ref_axis',(0.670534945922615,-0.741736547997381,0.0144837723499451));
#41947=DIRECTION('center_axis',(0.999604241409683,-0.0281309337996267,-0.000105448247542078));
#41948=DIRECTION('ref_axis',(0.0281275452130772,0.999529639708833,-0.0122204968727785));
#41949=DIRECTION('center_axis',(5.15167520928809E-67,-1.18789542670764E-48,
-1.));
#41950=DIRECTION('ref_axis',(0.,1.,0.));
#41951=DIRECTION('center_axis',(-0.686911553066313,-0.726741019928404,-9.0650146445407E-5));
#41952=DIRECTION('ref_axis',(0.726663889287897,-0.686840456251137,0.0144837723579623));
#41953=DIRECTION('center_axis',(0.998729922762429,0.0503838293465177,-0.00010544824700806));
#41954=DIRECTION('ref_axis',(0.0503813543051317,-0.998655285166875,0.0122204969886123));
#41955=DIRECTION('center_axis',(5.15167520928809E-67,-1.18789542670764E-48,
-1.));
#41956=DIRECTION('ref_axis',(0.,1.,0.));
#41957=DIRECTION('center_axis',(-0.627774590741284,-0.778395179200234,-9.06501463091932E-5));
#41958=DIRECTION('ref_axis',(0.778312708136324,-0.627709764694486,0.014483772322638));
#41959=DIRECTION('center_axis',(0.991698102029894,0.128587959432343,-0.000105448247307732));
#41960=DIRECTION('ref_axis',(0.128579636022594,-0.991623888707978,0.0122204968787672));
#41961=DIRECTION('center_axis',(5.15167520928809E-67,-1.18789542670764E-48,
-1.));
#41962=DIRECTION('ref_axis',(0.,1.,0.));
#41963=DIRECTION('center_axis',(-0.564767189308512,-0.825250273349312,-9.06501464604225E-5));
#41964=DIRECTION('ref_axis',(0.825162970323365,-0.564709033704023,0.014483772305219));
#41965=DIRECTION('center_axis',(0.978552132725239,0.205999301988023,-0.000105448247439453));
#41966=DIRECTION('ref_axis',(0.205985181526365,-0.978478801225051,0.0122204969104439));
#41967=DIRECTION('center_axis',(5.15167520928809E-67,-1.18789542670764E-48,
-1.));
#41968=DIRECTION('ref_axis',(0.,1.,0.));
#41969=DIRECTION('center_axis',(-0.498277810349565,-0.867017425139653,-9.06501466563663E-5));
#41970=DIRECTION('ref_axis',(0.86692582840462,-0.498226683736414,0.0144837722289047));
#41971=DIRECTION('center_axis',(0.959373064120893,0.282140590344525,-0.00010544824722367));
#41972=DIRECTION('ref_axis',(0.282120759888269,-0.959301066555644,0.0122204969322086));
#41973=DIRECTION('center_axis',(5.15167520928809E-67,-1.18789542670764E-48,
-1.));
#41974=DIRECTION('ref_axis',(0.,1.,0.));
#41975=DIRECTION('center_axis',(-0.428716382994794,-0.903439126191916,-9.06501464376821E-5));
#41976=DIRECTION('ref_axis',(0.903343800470677,-0.428672600584677,0.0144837722698243));
#41977=DIRECTION('center_axis',(0.934279141552165,0.356542388140901,-0.000105448247303552));
#41978=DIRECTION('ref_axis',(0.356516969951467,-0.934208921811066,0.0122204969306124));
#41979=DIRECTION('center_axis',(5.15167520928809E-67,-1.18789542670764E-48,
-1.));
#41980=DIRECTION('ref_axis',(0.,1.,0.));
#41981=DIRECTION('center_axis',(-0.356511776576584,-0.934290824606963,-9.06501462973138E-5));
#41982=DIRECTION('ref_axis',(0.9341923576135,-0.356475608302424,0.0144837723659048));
#41983=DIRECTION('center_axis',(0.903425077396469,0.42874598355186,-0.000105448247323971));
#41984=DIRECTION('ref_axis',(0.428715134340782,-0.903357068407445,0.0122204969404582));
#41985=DIRECTION('center_axis',(5.15167520928809E-67,-1.18789542670764E-48,
-1.));
#41986=DIRECTION('ref_axis',(0.,1.,0.));
#41987=DIRECTION('center_axis',(-0.282109156503611,-0.959382309405053,-9.06501462853803E-5));
#41988=DIRECTION('ref_axis',(0.959281308222382,-0.282080825355435,0.0144837723660616));
#41989=DIRECTION('center_axis',(0.867001097223284,0.498306217394775,-0.000105448243705777));
#41990=DIRECTION('ref_axis',(0.498270127348596,-0.86693571826834,0.0122204984583659));
#41991=DIRECTION('center_axis',(5.15167520928809E-67,-1.18789542670764E-48,
-1.));
#41992=DIRECTION('ref_axis',(0.,1.,0.));
#41993=DIRECTION('center_axis',(-0.205967239670074,-0.978558883238633,-9.06501462899978E-5));
#41994=DIRECTION('ref_axis',(0.978455970573443,-0.205946920318997,0.0144837723091262));
#41995=DIRECTION('center_axis',(0.825231766971361,0.564794227716602,-0.000105448246768021));
#41996=DIRECTION('ref_axis',(0.56475311935916,-0.825169421163415,0.0122204971638891));
#41997=DIRECTION('center_axis',(5.15167520928809E-67,-1.18789542670764E-48,
-1.));
#41998=DIRECTION('ref_axis',(0.,1.,0.));
#41999=DIRECTION('center_axis',(-0.128555466313085,-0.991702316153177,-9.06501463759606E-5));
#42000=DIRECTION('ref_axis',(0.991598126495219,-0.128543284034406,0.014483772327091));
#42001=DIRECTION('center_axis',(0.778374608461285,0.627800093806467,-0.000105448247278628));
#42002=DIRECTION('ref_axis',(0.627754220578617,-0.778315680171672,0.0122204969064386));
#42003=DIRECTION('center_axis',(5.15167520928809E-67,-1.18789542670764E-48,
-1.));
#42004=DIRECTION('ref_axis',(0.,1.,0.));
#42005=DIRECTION('center_axis',(-0.0503511057568215,-0.998731574514202,
-9.06501462140748E-5));
#42006=DIRECTION('ref_axis',(0.998626750226433,-0.0503471356583347,0.0144837724089729));
#42007=DIRECTION('center_axis',(0.72671851165485,0.686935363552371,-0.000105448247305609));
#42008=DIRECTION('ref_axis',(0.68688500827568,-0.726663364193057,0.0122204969517677));
#42009=DIRECTION('center_axis',(5.15167520928809E-67,-1.18789542670764E-48,
-1.));
#42010=DIRECTION('ref_axis',(0.,1.,0.));
#42011=DIRECTION('center_axis',(0.028163686109212,-0.999603320606376,-9.06501464412085E-5));
#42012=DIRECTION('ref_axis',(0.999498507967367,0.0281594195504058,0.0144837723535955));
#42013=DIRECTION('center_axis',(0.670581953565646,0.741835448352765,-0.000105448247317749));
#42014=DIRECTION('ref_axis',(0.741780921484837,-0.670530926934763,0.0122204969257884));
#42015=DIRECTION('center_axis',(5.15167520928809E-67,-1.18789542670764E-48,
-1.));
#42016=DIRECTION('ref_axis',(0.,1.,0.));
#42017=DIRECTION('center_axis',(0.106504839485654,-0.994312179825173,-9.06501463242885E-5));
#42018=DIRECTION('ref_axis',(0.994208025039066,0.106492362574368,0.0144837723417732));
#42019=DIRECTION('center_axis',(0.610311034742769,0.792161870927829,-0.000105448246632335));
#42020=DIRECTION('ref_axis',(0.792103508641049,-0.610264443535841,0.012220497306985));
#42021=DIRECTION('center_axis',(5.15167520928809E-67,-1.18789542670764E-48,
-1.));
#42022=DIRECTION('ref_axis',(0.,1.,0.));
#42023=DIRECTION('center_axis',(0.184189355110076,-0.982890773812984,-9.06501463014399E-5));
#42024=DIRECTION('ref_axis',(0.982787919027527,0.184168744770422,0.0144837724102069));
#42025=DIRECTION('center_axis',(0.546277345439608,0.837604352149702,-0.000105448247164003));
#42026=DIRECTION('ref_axis',(0.837542514274121,-0.546235476912526,0.0122204969428009));
#42027=DIRECTION('center_axis',(5.15167520928809E-67,-1.18789542670764E-48,
-1.));
#42028=DIRECTION('ref_axis',(0.,1.,0.));
#42029=DIRECTION('center_axis',(0.260738282110494,-0.965409519336027,-9.06501465102787E-5));
#42030=DIRECTION('ref_axis',(0.965308598687087,0.260709665412434,0.0144837723438797));
#42031=DIRECTION('center_axis',(0.47887567464682,0.877882724008293,-0.000105448247318393));
#42032=DIRECTION('ref_axis',(0.877817791791359,-0.47883878693017,0.0122204969532827));
#42033=DIRECTION('center_axis',(5.15167520928809E-67,-1.18789542670764E-48,
-1.));
#42034=DIRECTION('ref_axis',(0.,1.,0.));
#42035=DIRECTION('center_axis',(0.335679670898317,-0.941976194140886,-9.06501463025926E-5));
#42036=DIRECTION('ref_axis',(0.941877829837149,0.335643224273232,0.0144837723239312));
#42037=DIRECTION('center_axis',(0.408521576078182,0.912748656947391,-0.000105448247109452));
#42038=DIRECTION('ref_axis',(0.912681030717227,-0.408489896596761,0.0122204970155898));
#42039=DIRECTION('center_axis',(5.15167520928809E-67,-1.18789542670764E-48,
-1.));
#42040=DIRECTION('ref_axis',(0.,1.,0.));
#42041=DIRECTION('center_axis',(0.40855148288974,-0.912735272470143,-9.06501463607514E-5));
#42042=DIRECTION('ref_axis',(0.912640070959719,0.408507431042997,0.0144837723432182));
#42043=DIRECTION('center_axis',(0.33564880614496,0.941987190897058,-0.00010544824731253));
#42044=DIRECTION('ref_axis',(0.941917287593217,-0.335622530213924,0.0122204969555834));
#42045=DIRECTION('center_axis',(5.15167520928809E-67,-1.18789542670764E-48,
-1.));
#42046=DIRECTION('ref_axis',(0.,1.,0.));
#42047=DIRECTION('center_axis',(0.47890443913187,-0.877867034329425,-9.06501464476592E-5));
#42048=DIRECTION('ref_axis',(0.877775582561568,0.47885305365786,0.0144837723415746));
#42049=DIRECTION('center_axis',(0.260706649725499,0.965418060567325,-0.000105448239035086));
#42050=DIRECTION('ref_axis',(0.965346311123191,-0.260685939332472,0.0122205006114622));
#42051=DIRECTION('center_axis',(5.15167520928809E-67,-1.18789542670764E-48,
-1.));
#42052=DIRECTION('ref_axis',(0.,1.,0.));
#42053=DIRECTION('center_axis',(0.546304790255255,-0.837586454001444,-9.0650146342598E-5));
#42054=DIRECTION('ref_axis',(0.837499315807156,0.546246387962813,0.0144837723030219));
#42055=DIRECTION('center_axis',(0.184157150081292,0.982896806869675,-0.000105448247335927));
#42056=DIRECTION('ref_axis',(0.982823653730575,-0.184142132936566,0.0122204969315608));
#42057=DIRECTION('center_axis',(5.15167520928809E-67,-1.18789542670764E-48,
-1.));
#42058=DIRECTION('ref_axis',(0.,1.,0.));
#42059=DIRECTION('center_axis',(0.610336990681674,-0.792141874658946,-9.06501464101343E-5));
#42060=DIRECTION('ref_axis',(0.792059587273886,0.610271931640238,0.0144837722853376));
#42061=DIRECTION('center_axis',(0.106472260386401,0.99431566750649,-0.000105448247238185));
#42062=DIRECTION('ref_axis',(0.994241561642249,-0.106463029063635,0.0122204969529716));
#42063=DIRECTION('center_axis',(5.15167520928809E-67,-1.18789542670764E-48,
-1.));
#42064=DIRECTION('ref_axis',(0.,1.,0.));
#42065=DIRECTION('center_axis',(0.670606260602894,-0.741813477245294,-9.06501464627064E-5));
#42066=DIRECTION('ref_axis',(0.741736547997723,0.670534945922382,0.0144837723432088));
#42067=DIRECTION('center_axis',(0.0281309337999561,0.999604241409674,-0.000105448247417899));
#42068=DIRECTION('ref_axis',(0.999529639708026,-0.0281275452133787,0.0122204969380853));
#42069=DIRECTION('center_axis',(5.15167520928809E-67,-1.18789542670764E-48,
-1.));
#42070=DIRECTION('ref_axis',(0.,1.,0.));
#42071=DIRECTION('center_axis',(0.726741019928368,-0.686911553066351,-9.0650146471134E-5));
#42072=DIRECTION('ref_axis',(0.686840456251459,0.726663889288164,0.0144837723292476));
#42073=DIRECTION('center_axis',(-0.050383829347144,0.998729922762398,-0.000105448247269544));
#42074=DIRECTION('ref_axis',(0.998655285167744,0.0503813543057988,0.0122204969148411));
#42075=DIRECTION('center_axis',(5.15167520928809E-67,-1.18789542670764E-48,
-1.));
#42076=DIRECTION('ref_axis',(0.,1.,0.));
#42077=DIRECTION('center_axis',(0.778395179200218,-0.627774590741304,-9.06501463631465E-5));
#42078=DIRECTION('ref_axis',(0.627709764694807,0.778312708136684,0.0144837722894029));
#42079=DIRECTION('center_axis',(-0.12858795942834,0.991698102030413,-0.000105448245500489));
#42080=DIRECTION('ref_axis',(0.991623888698102,0.128579636017312,0.0122204977357358));
#42081=DIRECTION('center_axis',(5.15167520928809E-67,-1.18789542670764E-48,
-1.));
#42082=DIRECTION('ref_axis',(0.,1.,0.));
#42083=DIRECTION('center_axis',(0.825250273349428,-0.564767189308343,-9.06501464028957E-5));
#42084=DIRECTION('ref_axis',(0.564709033703531,0.825162970323003,0.0144837723450398));
#42085=DIRECTION('center_axis',(-0.205999301987628,0.978552132725322,-0.000105448247257059));
#42086=DIRECTION('ref_axis',(0.978478801225208,0.205985181525983,0.0122204969042825));
#42087=DIRECTION('center_axis',(5.15167520928809E-67,-1.18789542670764E-48,
-1.));
#42088=DIRECTION('ref_axis',(0.,1.,0.));
#42089=DIRECTION('center_axis',(0.867017425139937,-0.498277810349071,-9.06501464136658E-5));
#42090=DIRECTION('ref_axis',(0.498226683735389,0.866925828403975,0.0144837723027363));
#42091=DIRECTION('center_axis',(-0.282140590344626,0.959373064120863,-0.000105448247277017));
#42092=DIRECTION('ref_axis',(0.959301066555094,0.282120759888223,0.0122204969764503));
#42093=DIRECTION('center_axis',(5.15167520928809E-67,-1.18789542670764E-48,
-1.));
#42094=DIRECTION('ref_axis',(0.,1.,0.));
#42095=DIRECTION('center_axis',(0.90343912619187,-0.42871638299489,-9.06501464260602E-5));
#42096=DIRECTION('ref_axis',(0.428672600584421,0.903343800469878,0.0144837723272369));
#42097=DIRECTION('center_axis',(-0.356542388139781,0.934279141552593,-0.000105448246761887));
#42098=DIRECTION('ref_axis',(0.934208921809314,0.35651696994953,0.012220497120973));
#42099=DIRECTION('center_axis',(5.15167520928809E-67,-1.18789542670764E-48,
-1.));
#42100=DIRECTION('ref_axis',(0.,1.,0.));
#42101=DIRECTION('center_axis',(0.934290824606888,-0.35651177657678,-9.06501464134324E-5));
#42102=DIRECTION('ref_axis',(0.356475608302711,0.934192357613664,0.0144837723482609));
#42103=DIRECTION('center_axis',(-0.428745983551679,0.903425077396555,-0.000105448247222545));
#42104=DIRECTION('ref_axis',(0.903357068407448,0.428715134340562,0.0122204969479439));
#42105=DIRECTION('center_axis',(5.15167520928809E-67,-1.18789542670764E-48,
-1.));
#42106=DIRECTION('ref_axis',(0.,1.,0.));
#42107=DIRECTION('center_axis',(0.959382309405034,-0.282109156503675,-9.06501462956451E-5));
#42108=DIRECTION('ref_axis',(0.282080825355574,0.959281308222623,0.0144837723473633));
#42109=DIRECTION('center_axis',(-0.498306217401744,0.867001097219279,-0.000105448247347347));
#42110=DIRECTION('ref_axis',(0.866935718280794,0.498270127364887,0.0122204969106369));
#42111=DIRECTION('center_axis',(5.15167520928809E-67,-1.18789542670764E-48,
-1.));
#42112=DIRECTION('ref_axis',(0.,1.,0.));
#42113=DIRECTION('center_axis',(0.978558883238587,-0.205967239670296,-9.06501464061553E-5));
#42114=DIRECTION('ref_axis',(0.205946920319019,0.978455970572407,0.0144837723787919));
#42115=DIRECTION('center_axis',(-0.564794227717559,0.825231766970706,-0.000105448247271081));
#42116=DIRECTION('ref_axis',(0.825169421165301,0.564753119361831,0.0122204969131223));
#42117=DIRECTION('center_axis',(5.15167520928809E-67,-1.18789542670764E-48,
-1.));
#42118=DIRECTION('ref_axis',(0.,1.,0.));
#42119=DIRECTION('center_axis',(0.99170231615319,-0.128555466312983,-9.06501463191467E-5));
#42120=DIRECTION('ref_axis',(0.128543284034309,0.991598126495285,0.014483772323378));
#42121=DIRECTION('center_axis',(-0.627800093806562,0.778374608461208,-0.000105448247350595));
#42122=DIRECTION('ref_axis',(0.778315680171392,0.627754220578551,0.0122204969276863));
#42123=DIRECTION('center_axis',(5.15167520928809E-67,-1.18789542670764E-48,
-1.));
#42124=DIRECTION('ref_axis',(0.,1.,0.));
#42125=DIRECTION('center_axis',(0.998731574514188,-0.0503511057570843,-9.06501463742907E-5));
#42126=DIRECTION('ref_axis',(0.0503471356586318,0.998626750227146,0.0144837723587898));
#42127=DIRECTION('center_axis',(-0.686935363552425,0.726718511654798,-0.000105448247333776));
#42128=DIRECTION('ref_axis',(0.726663364192883,0.686885008275621,0.0122204969654078));
#42129=DIRECTION('center_axis',(5.15167520928809E-67,-1.18789542670764E-48,
-1.));
#42130=DIRECTION('ref_axis',(0.,1.,0.));
#42131=DIRECTION('center_axis',(0.999603320606373,0.0281636861093081,-9.0650146390368E-5));
#42132=DIRECTION('ref_axis',(0.0281594195505035,-0.99949850796739,-0.0144837723518616));
#42133=DIRECTION('center_axis',(-0.741835448352795,0.670581953565614,-0.000105448247334273));
#42134=DIRECTION('ref_axis',(0.670530926935027,0.741780921485189,0.0122204968899333));
#42135=DIRECTION('center_axis',(5.15167520928809E-67,-1.18789542670764E-48,
-1.));
#42136=DIRECTION('ref_axis',(0.,1.,0.));
#42137=DIRECTION('center_axis',(0.994312179825183,0.106504839485559,-9.06501463756277E-5));
#42138=DIRECTION('ref_axis',(0.106492362574294,-0.994208025039266,-0.0144837723286163));
#42139=DIRECTION('center_axis',(-0.792161870920044,0.610311034752874,-0.00010544824088436));
#42140=DIRECTION('ref_axis',(0.610264443527485,0.792103508609612,0.0122204997619462));
#42141=DIRECTION('center_axis',(5.15167520928809E-67,-1.18789542670764E-48,
-1.));
#42142=DIRECTION('ref_axis',(0.,1.,0.));
#42143=DIRECTION('center_axis',(0.982890773813025,0.184189355109853,-9.06501463812825E-5));
#42144=DIRECTION('ref_axis',(0.184168744770323,-0.982787919028214,-0.0144837723648623));
#42145=DIRECTION('center_axis',(-0.837604352149864,0.54627734543936,-0.00010544824728987));
#42146=DIRECTION('ref_axis',(0.546235476912709,0.837542514274935,0.0122204968788532));
#42147=DIRECTION('center_axis',(5.15167520928809E-67,-1.18789542670764E-48,
-1.));
#42148=DIRECTION('ref_axis',(0.,1.,0.));
#42149=DIRECTION('center_axis',(-0.778374608461274,-0.62780009380648,-0.000105448247267533));
#42150=DIRECTION('ref_axis',(0.627754220578446,-0.77831568017143,-0.0122204969306265));
#42151=DIRECTION('center_axis',(0.128555466313028,0.991702316153185,-9.06501463500336E-5));
#42152=DIRECTION('ref_axis',(0.991598126495177,-0.128543284034342,-0.0144837723304925));
#42153=DIRECTION('center_axis',(5.15167520928809E-67,-1.18789542670764E-48,
-1.));
#42154=DIRECTION('ref_axis',(0.,1.,0.));
#42155=DIRECTION('center_axis',(-0.825231766970672,-0.564794227717608,-0.000105448247309068));
#42156=DIRECTION('ref_axis',(0.564753119361638,-0.825169421164907,-0.012220496948613));
#42157=DIRECTION('center_axis',(0.205967239670274,0.978558883238591,-9.0650146374353E-5));
#42158=DIRECTION('ref_axis',(0.978455970572943,-0.205946920319105,-0.0144837723413512));
#42159=DIRECTION('center_axis',(5.15167520928809E-67,-1.18789542670764E-48,
-1.));
#42160=DIRECTION('ref_axis',(0.,1.,0.));
#42161=DIRECTION('center_axis',(-0.86700109721932,-0.498306217401672,-0.00010544824729092));
#42162=DIRECTION('ref_axis',(0.498270127364739,-0.8669357182807,-0.0122204969233888));
#42163=DIRECTION('center_axis',(0.282109156504052,0.959382309404923,-9.06501464701313E-5));
#42164=DIRECTION('ref_axis',(0.959281308222407,-0.282080825355923,-0.0144837723548786));
#42165=DIRECTION('center_axis',(5.15167520928809E-67,-1.18789542670764E-48,
-1.));
#42166=DIRECTION('ref_axis',(0.,1.,0.));
#42167=DIRECTION('center_axis',(-0.903425077396529,-0.428745983551733,-0.000105448247249315));
#42168=DIRECTION('ref_axis',(0.428715134340504,-0.903357068407182,-0.0122204969696425));
#42169=DIRECTION('center_axis',(0.356511776576785,0.934290824606886,-9.06501464239672E-5));
#42170=DIRECTION('ref_axis',(0.934192357613866,-0.356475608302793,-0.0144837723332318));
#42171=DIRECTION('center_axis',(5.15167520928809E-67,-1.18789542670764E-48,
-1.));
#42172=DIRECTION('ref_axis',(0.,1.,0.));
#42173=DIRECTION('center_axis',(-0.934279141552621,-0.356542388139705,-0.000105448246733279));
#42174=DIRECTION('ref_axis',(0.356516969949183,-0.934208921808614,-0.0122204971846563));
#42175=DIRECTION('center_axis',(0.428716382994808,0.903439126191909,-9.06501463770139E-5));
#42176=DIRECTION('ref_axis',(0.903343800469329,-0.428672600584064,-0.0144837723720362));
#42177=DIRECTION('center_axis',(5.15167520928809E-67,-1.18789542670764E-48,
-1.));
#42178=DIRECTION('ref_axis',(0.,1.,0.));
#42179=DIRECTION('center_axis',(-0.959373064120865,-0.282140590344618,-0.000105448247270857));
#42180=DIRECTION('ref_axis',(0.282120759888191,-0.959301066555013,-0.0122204969835453));
#42181=DIRECTION('center_axis',(0.498277810349034,0.867017425139958,-9.06501463569771E-5));
#42182=DIRECTION('ref_axis',(0.866925828403698,-0.498226683735182,-0.0144837723264648));
#42183=DIRECTION('center_axis',(5.15167520928809E-67,-1.18789542670764E-48,
-1.));
#42184=DIRECTION('ref_axis',(0.,1.,0.));
#42185=DIRECTION('center_axis',(-0.978552132725285,-0.205999301987804,-0.000105448247338301));
#42186=DIRECTION('ref_axis',(0.205985181526041,-0.978478801224581,-0.0122204969535068));
#42187=DIRECTION('center_axis',(0.564767189308271,0.825250273349477,-9.06501463565956E-5));
#42188=DIRECTION('ref_axis',(0.825162970322881,-0.564709033703342,-0.0144837723594094));
#42189=DIRECTION('center_axis',(5.15167520928809E-67,-1.18789542670764E-48,
-1.));
#42190=DIRECTION('ref_axis',(0.,1.,0.));
#42191=DIRECTION('center_axis',(-0.991698102030424,-0.128587959428258,-0.000105448245434831));
#42192=DIRECTION('ref_axis',(0.128579636017166,-0.991623888697594,-0.0122204977785004));
#42193=DIRECTION('center_axis',(0.627774590741263,0.778395179200251,-9.06501463298504E-5));
#42194=DIRECTION('ref_axis',(0.778312708136619,-0.627709764694687,-0.0144837722981268));
#42195=DIRECTION('center_axis',(5.15167520928809E-67,-1.18789542670764E-48,
-1.));
#42196=DIRECTION('ref_axis',(0.,1.,0.));
#42197=DIRECTION('center_axis',(-0.998729922762387,-0.0503838293473624,
-0.000105448247373321));
#42198=DIRECTION('ref_axis',(0.0503813543060242,-0.998655285167869,-0.0122204969036645));
#42199=DIRECTION('center_axis',(0.686911553066443,0.726741019928282,-9.06501464895761E-5));
#42200=DIRECTION('ref_axis',(0.726663889287984,-0.686840456251464,-0.0144837723380814));
#42201=DIRECTION('center_axis',(5.15167520928809E-67,-1.18789542670764E-48,
-1.));
#42202=DIRECTION('ref_axis',(0.,1.,0.));
#42203=DIRECTION('center_axis',(-0.999604241409666,0.0281309338002504,-0.00010544824728445));
#42204=DIRECTION('ref_axis',(0.0281275452136831,0.999529639708247,0.0122204969192793));
#42205=DIRECTION('center_axis',(0.741813477245179,0.670606260603021,-9.06501463486941E-5));
#42206=DIRECTION('ref_axis',(0.670534945922386,-0.741736547997471,-0.0144837723559454));
#42207=DIRECTION('center_axis',(5.15167520928809E-67,-1.18789542670764E-48,
-1.));
#42208=DIRECTION('ref_axis',(0.,1.,0.));
#42209=DIRECTION('center_axis',(-0.994315667506492,0.106472260386385,-0.000105448247246095));
#42210=DIRECTION('ref_axis',(0.106463029063669,0.99424156164268,0.0122204969176238));
#42211=DIRECTION('center_axis',(0.792141874658893,0.610336990681743,-9.06501463537118E-5));
#42212=DIRECTION('ref_axis',(0.610271931639807,-0.792059587273192,-0.0144837723414781));
#42213=DIRECTION('center_axis',(5.15167520928809E-67,-1.18789542670764E-48,
-1.));
#42214=DIRECTION('ref_axis',(0.,1.,0.));
#42215=DIRECTION('center_axis',(-0.98289680686965,0.184157150081429,-0.000105448247288298));
#42216=DIRECTION('ref_axis',(0.184142132936832,0.982823653731204,0.0122204968770007));
#42217=DIRECTION('center_axis',(0.837586454001503,0.546304790255165,-9.06501464022278E-5));
#42218=DIRECTION('ref_axis',(0.546246387962582,-0.837499315807004,-0.0144837723204838));
#42219=DIRECTION('center_axis',(5.15167520928809E-67,-1.18789542670764E-48,
-1.));
#42220=DIRECTION('ref_axis',(0.,1.,0.));
#42221=DIRECTION('center_axis',(-0.965418060567323,0.260706649725506,-0.000105448239021929));
#42222=DIRECTION('ref_axis',(0.260685939332638,0.965346311123758,0.0122205005631217));
#42223=DIRECTION('center_axis',(0.877867034329392,0.478904439131931,-9.06501464072983E-5));
#42224=DIRECTION('ref_axis',(0.478853053658107,-0.87777558256187,-0.0144837723150808));
#42225=DIRECTION('center_axis',(5.15167520928809E-67,-1.18789542670764E-48,
-1.));
#42226=DIRECTION('ref_axis',(0.,1.,0.));
#42227=DIRECTION('center_axis',(-0.94198719089703,0.335648806145038,-0.000105448247300868));
#42228=DIRECTION('ref_axis',(0.335622530213848,0.941917287592769,0.0122204969921728));
#42229=DIRECTION('center_axis',(0.912735272470196,0.40855148288962,-9.06501464040206E-5));
#42230=DIRECTION('ref_axis',(0.408507431043198,-0.912640070960478,-0.01448377228974));
#42231=DIRECTION('center_axis',(5.15167520928809E-67,-1.18789542670764E-48,
-1.));
#42232=DIRECTION('ref_axis',(0.,1.,0.));
#42233=DIRECTION('center_axis',(0.965409519335958,0.260738282110751,-9.06501464007405E-5));
#42234=DIRECTION('ref_axis',(0.260709665412327,-0.965308598685698,-0.0144837724383535));
#42235=DIRECTION('center_axis',(-0.87788272400828,0.478875674646843,-0.000105448247307507));
#42236=DIRECTION('ref_axis',(0.478838786930294,0.877817791791527,0.0122204969363654));
#42237=DIRECTION('center_axis',(5.15167520928809E-67,-1.18789542670764E-48,
-1.));
#42238=DIRECTION('ref_axis',(-4.33680868994202E-19,1.,-1.18789542670764E-48));
#42239=DIRECTION('center_axis',(5.15167520928809E-67,-1.18789542670764E-48,
-1.));
#42240=DIRECTION('ref_axis',(-4.33680868994202E-19,1.,-1.18789542670764E-48));
#42241=DIRECTION('center_axis',(5.15167520928809E-67,-1.18789542670764E-48,
-1.));
#42242=DIRECTION('ref_axis',(0.,1.,0.));
#42243=DIRECTION('center_axis',(0.941987190897879,0.335648806142656,0.000105448247691596));
#42244=DIRECTION('ref_axis',(0.335622530211987,-0.941917287595053,0.0122204968672344));
#42245=DIRECTION('center_axis',(-0.912735272471169,0.408551482887447,9.06501467246596E-5));
#42246=DIRECTION('ref_axis',(0.408507431040732,0.912640070960819,-0.0144837723377799));
#42247=DIRECTION('center_axis',(5.15167520928809E-67,-1.18789542670764E-48,
-1.));
#42248=DIRECTION('ref_axis',(-4.33680868994202E-19,1.,-1.18789542670764E-48));
#42249=DIRECTION('center_axis',(5.15167520928809E-67,-1.18789542670764E-48,
-1.));
#42250=DIRECTION('ref_axis',(-4.33680868994202E-19,1.,-1.18789542670764E-48));
#42251=DIRECTION('',(-5.15167520928809E-67,1.18789542670764E-48,1.));
#42252=DIRECTION('',(5.15167520928809E-67,-1.18789542670764E-48,-1.));
#42253=DIRECTION('center_axis',(5.15167520928809E-67,-1.18789542670764E-48,
-1.));
#42254=DIRECTION('ref_axis',(-4.33680868994202E-19,1.,-1.18789542670764E-48));
#42255=DIRECTION('center_axis',(5.15167520928809E-67,-1.18789542670764E-48,
-1.));
#42256=DIRECTION('ref_axis',(0.,1.,0.));
#42257=DIRECTION('center_axis',(0.941976194140935,0.33567967089818,-9.06501463865783E-5));
#42258=DIRECTION('ref_axis',(0.335643224273153,-0.94187782983736,-0.014483772312066));
#42259=DIRECTION('center_axis',(-0.912748656947277,0.408521576078436,-0.000105448246989675));
#42260=DIRECTION('ref_axis',(0.408489896596946,0.91268103071696,0.012220497029356));
#42261=DIRECTION('center_axis',(-5.15167520928809E-67,1.18789542670764E-48,
1.));
#42262=DIRECTION('ref_axis',(4.33680868994202E-19,-1.,1.18789542670764E-48));
#42263=DIRECTION('center_axis',(0.,0.,1.));
#42264=DIRECTION('ref_axis',(1.,4.33680868994202E-19,0.));
#42265=DIRECTION('',(0.866025403784438,0.5,0.));
#42266=DIRECTION('',(-4.33680868994202E-19,1.,0.));
#42267=DIRECTION('',(-0.866025403784439,0.499999999999999,0.));
#42268=DIRECTION('',(-0.866025403784439,-0.5,0.));
#42269=DIRECTION('',(6.01359520363859E-16,-1.,0.));
#42270=DIRECTION('',(0.866025403784439,-0.5,0.));
#42271=DIRECTION('center_axis',(1.,4.33680868994202E-19,0.));
#42272=DIRECTION('ref_axis',(0.,0.,-1.));
#42273=DIRECTION('',(0.,0.,1.));
#42274=DIRECTION('',(0.,0.,1.));
#42275=DIRECTION('center_axis',(0.499999999999999,0.866025403784439,0.));
#42276=DIRECTION('ref_axis',(-0.866025403784439,0.499999999999999,0.));
#42277=DIRECTION('',(0.,0.,1.));
#42278=DIRECTION('center_axis',(-0.5,0.866025403784439,0.));
#42279=DIRECTION('ref_axis',(-0.866025403784439,-0.5,0.));
#42280=DIRECTION('',(0.,0.,1.));
#42281=DIRECTION('center_axis',(-1.,-6.01359520363859E-16,0.));
#42282=DIRECTION('ref_axis',(6.01359520363859E-16,-1.,0.));
#42283=DIRECTION('',(0.,0.,1.));
#42284=DIRECTION('center_axis',(-0.5,-0.866025403784439,0.));
#42285=DIRECTION('ref_axis',(0.866025403784439,-0.5,0.));
#42286=DIRECTION('',(0.,0.,1.));
#42287=DIRECTION('center_axis',(0.5,-0.866025403784439,0.));
#42288=DIRECTION('ref_axis',(0.866025403784439,0.5,0.));
#42289=DIRECTION('',(1.0568194522281E-16,0.866025403784468,-0.499999999999949));
#42290=DIRECTION('center_axis',(4.70261923768679E-35,-1.08435016942139E-16,
1.));
#42291=DIRECTION('ref_axis',(0.378466979033695,0.925614793410903,1.00369055805406E-16));
#42292=DIRECTION('center_axis',(0.912653256146669,-0.408734674385332,0.));
#42293=DIRECTION('ref_axis',(0.408734674385332,0.912653256146669,0.));
#42294=DIRECTION('',(0.,0.,1.));
#42295=DIRECTION('center_axis',(0.,0.,1.));
#42296=DIRECTION('ref_axis',(1.,4.33680868994202E-19,0.));
#42297=DIRECTION('',(0.,0.,1.));
#42298=DIRECTION('center_axis',(-0.912653256146668,-0.408734674385334,0.));
#42299=DIRECTION('ref_axis',(0.408734674385334,-0.912653256146668,0.));
#42300=DIRECTION('center_axis',(0.877770897795706,-0.479080630982844,8.35636401295593E-50));
#42301=DIRECTION('ref_axis',(0.479080630982844,0.877770897795706,2.97282767021015E-66));
#42302=DIRECTION('',(-9.32012009987243E-50,3.66188516048321E-51,1.));
#42303=DIRECTION('center_axis',(-9.32012009987243E-50,3.66188516048321E-51,
1.));
#42304=DIRECTION('ref_axis',(1.,4.33680868994202E-19,9.32012009987243E-50));
#42305=DIRECTION('',(-9.32012009987243E-50,3.66188516048321E-51,1.));
#42306=DIRECTION('center_axis',(-0.941908803685482,-0.335868732602165,-8.65571190069724E-50));
#42307=DIRECTION('ref_axis',(0.335868732602165,-0.941908803685482,-2.86613947502886E-66));
#42308=DIRECTION('center_axis',(0.941908803685478,-0.335868732602176,-8.65571190069562E-50));
#42309=DIRECTION('ref_axis',(0.335868732602176,0.941908803685478,5.69318196416785E-66));
#42310=DIRECTION('',(9.32012009987071E-50,3.66188516048189E-51,1.));
#42311=DIRECTION('center_axis',(9.32012009987071E-50,3.66188516048189E-51,
1.));
#42312=DIRECTION('ref_axis',(1.,4.33680868994202E-19,-9.32012009987071E-50));
#42313=DIRECTION('',(9.32012009987071E-50,3.66188516048189E-51,1.));
#42314=DIRECTION('center_axis',(-0.877770897795712,-0.479080630982834,8.35636401295441E-50));
#42315=DIRECTION('ref_axis',(0.479080630982834,-0.877770897795712,-1.78392693329902E-66));
#42316=DIRECTION('center_axis',(0.965357170233111,-0.260932048394827,-1.75574063469501E-49));
#42317=DIRECTION('ref_axis',(0.260932048394827,0.965357170233111,-8.03239509524584E-66));
#42318=DIRECTION('',(1.85827785600731E-49,1.46249639022155E-50,1.));
#42319=DIRECTION('center_axis',(1.8582778560073E-49,1.46249639022155E-50,
1.));
#42320=DIRECTION('ref_axis',(1.,4.33680868994202E-19,-1.8582778560073E-49));
#42321=DIRECTION('',(1.85827785600731E-49,1.46249639022155E-50,1.));
#42322=DIRECTION('center_axis',(-0.837476789971396,-0.546472896179862,1.63618603752562E-49));
#42323=DIRECTION('ref_axis',(0.546472896179862,-0.837476789971396,1.23627039651628E-65));
#42324=DIRECTION('center_axis',(0.982853788812423,-0.184386631340412,-2.66502014323869E-49));
#42325=DIRECTION('ref_axis',(0.184386631340412,0.982853788812423,-4.59929189808117E-66));
#42326=DIRECTION('',(2.77308680110516E-49,3.28216451991643E-50,1.));
#42327=DIRECTION('center_axis',(2.77308680110516E-49,3.28216451991643E-50,
1.));
#42328=DIRECTION('ref_axis',(1.,4.33680868994202E-19,-2.77308680110516E-49));
#42329=DIRECTION('',(2.77308680110516E-49,3.28216451991643E-50,1.));
#42330=DIRECTION('center_axis',(-0.792019359247614,-0.610495974251263,2.39671325397326E-49));
#42331=DIRECTION('ref_axis',(0.610495974251263,-0.792019359247614,-2.26955332198497E-65));
#42332=DIRECTION('center_axis',(0.994290786951656,-0.106704409389008,-3.5878037051643E-49));
#42333=DIRECTION('ref_axis',(0.106704409389008,0.994290786951656,1.37166247450949E-66));
#42334=DIRECTION('',(3.67079874392927E-49,5.81397404601223E-50,1.));
#42335=DIRECTION('center_axis',(3.67079874392927E-49,5.81397404601223E-50,
1.));
#42336=DIRECTION('ref_axis',(1.,4.33680868994202E-19,-3.67079874392927E-49));
#42337=DIRECTION('',(3.67079874392927E-49,5.81397404601223E-50,1.));
#42338=DIRECTION('center_axis',(-0.741678865800908,-0.670755141630892,3.11252914744798E-49));
#42339=DIRECTION('ref_axis',(0.670755141630892,-0.741678865800908,-3.59898235302298E-65));
#42340=DIRECTION('center_axis',(0.999597651754094,-0.028364319270904,-4.5184020529559E-49));
#42341=DIRECTION('ref_axis',(0.028364319270904,0.999597651754094,-3.26521667006146E-66));
#42342=DIRECTION('',(4.54587899183259E-49,9.04231552086841E-50,1.));
#42343=DIRECTION('center_axis',(4.54587899183259E-49,9.04231552086841E-50,
1.));
#42344=DIRECTION('ref_axis',(1.,4.33680868994202E-19,-4.54587899183259E-49));
#42345=DIRECTION('',(4.54587899183259E-49,9.04231552086841E-50,1.));
#42346=DIRECTION('center_axis',(-0.68676567551329,-0.726878880513649,3.77922047493358E-49));
#42347=DIRECTION('ref_axis',(0.726878880513649,-0.68676567551329,8.44347396578498E-67));
#42348=DIRECTION('center_axis',(0.998741664633518,0.0501506463075991,-5.45107773834402E-49));
#42349=DIRECTION('ref_axis',(-0.0501506463075991,0.998741664633518,-5.68155672720376E-65));
#42350=DIRECTION('center_axis',(-0.62761834646337,-0.778521169386283,4.39267686269876E-49));
#42351=DIRECTION('ref_axis',(0.778521169386283,-0.62761834646337,2.86838711888421E-65));
#42352=DIRECTION('center_axis',(0.991728103035171,0.128356416474834,-6.38008050558209E-49));
#42353=DIRECTION('ref_axis',(-0.128356416474834,0.991728103035171,2.64164793875071E-66));
#42354=DIRECTION('center_axis',(-0.564601541603225,-0.825363616365092,4.94911614811798E-49));
#42355=DIRECTION('ref_axis',(0.825363616365092,-0.564601541603225,-1.21982614064914E-65));
#42356=DIRECTION('center_axis',(0.978600207898554,0.20577082665166,-7.29968274368531E-49));
#42357=DIRECTION('ref_axis',(-0.20577082665166,0.978600207898554,7.99368498149713E-66));
#42358=DIRECTION('center_axis',(-0.498103780490032,-0.867117422187756,5.44510769796179E-49));
#42359=DIRECTION('ref_axis',(0.867117422187756,-0.498103780490032,-1.67935322369464E-65));
#42360=DIRECTION('center_axis',(0.95943891706265,0.281916591256437,-8.20421479905702E-49));
#42361=DIRECTION('ref_axis',(-0.281916591256437,0.95943891706265,1.24589067679861E-65));
#42362=DIRECTION('center_axis',(-0.428535043933802,-0.903525160756829,5.87759355939149E-49));
#42363=DIRECTION('ref_axis',(0.903525160756829,-0.428535043933802,-8.86364012879408E-65));
#42364=DIRECTION('center_axis',(0.93436236625724,0.356324246329338,-9.08809993078841E-49));
#42365=DIRECTION('ref_axis',(-0.356324246329338,0.93436236625724,-2.69950222050985E-65));
#42366=DIRECTION('center_axis',(-0.356324246329358,-0.934362366257233,6.24390731325522E-49));
#42367=DIRECTION('ref_axis',(0.934362366257233,-0.356324246329358,4.50754916861586E-65));
#42368=DIRECTION('center_axis',(0.903525160756839,0.428535043933782,-9.94588869312071E-49));
#42369=DIRECTION('ref_axis',(-0.428535043933782,0.903525160756839,-3.06876799885187E-65));
#42370=DIRECTION('center_axis',(-0.281916591256458,-0.959438917062644,6.54179051344872E-49));
#42371=DIRECTION('ref_axis',(0.959438917062644,-0.281916591256458,5.46345068117847E-65));
#42372=DIRECTION('center_axis',(0.867117422187767,0.498103780490012,-1.07722925330905E-48));
#42373=DIRECTION('ref_axis',(-0.498103780490012,0.867117422187767,2.63677046246647E-65));
#42374=DIRECTION('center_axis',(-0.205770826651682,-0.978600207898549,6.76940661098659E-49));
#42375=DIRECTION('ref_axis',(0.978600207898549,-0.205770826651682,1.20007194121145E-65));
#42376=DIRECTION('center_axis',(0.825363616365104,0.564601541603207,-1.15622163962171E-48));
#42377=DIRECTION('ref_axis',(-0.564601541603207,0.825363616365104,5.34857418276646E-65));
#42378=DIRECTION('center_axis',(-0.128356416474855,-0.991728103035168,6.92535227693746E-49));
#42379=DIRECTION('ref_axis',(0.991728103035168,-0.128356416474855,1.05782428992148E-64));
#42380=DIRECTION('center_axis',(0.778521169386297,0.627618346463353,-1.2310790139208E-48));
#42381=DIRECTION('ref_axis',(-0.627618346463353,0.778521169386297,-3.24299836420865E-65));
#42382=DIRECTION('center_axis',(-0.0501506463076206,-0.998741664633517,
7.00866605441356E-49));
#42383=DIRECTION('ref_axis',(0.998741664633517,-0.0501506463076206,5.61717615944791E-66));
#42384=DIRECTION('center_axis',(0.83747678997139,-0.546472896179871,1.63618603752577E-49));
#42385=DIRECTION('ref_axis',(0.546472896179871,0.83747678997139,8.18221406165844E-66));
#42386=DIRECTION('',(-1.85827785600747E-49,1.46249639022181E-50,1.));
#42387=DIRECTION('center_axis',(-1.85827785600747E-49,1.46249639022181E-50,
1.));
#42388=DIRECTION('ref_axis',(1.,4.33680868994202E-19,1.85827785600747E-49));
#42389=DIRECTION('',(-1.85827785600747E-49,1.46249639022181E-50,1.));
#42390=DIRECTION('center_axis',(-0.965357170233114,-0.260932048394816,-1.75574063469517E-49));
#42391=DIRECTION('ref_axis',(0.260932048394816,-0.965357170233114,4.85072620126884E-66));
#42392=DIRECTION('center_axis',(0.792019359247608,-0.610495974251272,2.39671325397339E-49));
#42393=DIRECTION('ref_axis',(0.610495974251272,0.792019359247608,6.86514884131891E-66));
#42394=DIRECTION('',(-2.77308680110532E-49,3.28216451991683E-50,1.));
#42395=DIRECTION('center_axis',(-2.77308680110532E-49,3.28216451991683E-50,
1.));
#42396=DIRECTION('ref_axis',(1.,4.33680868994202E-19,2.77308680110532E-49));
#42397=DIRECTION('',(-2.77308680110532E-49,3.28216451991683E-50,1.));
#42398=DIRECTION('center_axis',(-0.982853788812425,-0.184386631340402,-2.66502014323885E-49));
#42399=DIRECTION('ref_axis',(0.184386631340402,-0.982853788812425,5.0100483719309E-66));
#42400=DIRECTION('center_axis',(0.741678865800901,-0.6707551416309,3.11252914744811E-49));
#42401=DIRECTION('ref_axis',(0.6707551416309,0.741678865800901,2.48321099822104E-65));
#42402=DIRECTION('',(-3.67079874392942E-49,5.81397404601274E-50,1.));
#42403=DIRECTION('center_axis',(-3.67079874392942E-49,5.81397404601274E-50,
1.));
#42404=DIRECTION('ref_axis',(1.,4.33680868994202E-19,3.67079874392942E-49));
#42405=DIRECTION('',(-3.67079874392942E-49,5.81397404601274E-50,1.));
#42406=DIRECTION('center_axis',(-0.994290786951657,-0.106704409388997,-3.58780370516446E-49));
#42407=DIRECTION('ref_axis',(0.106704409388997,-0.994290786951657,8.97464790050996E-66));
#42408=DIRECTION('center_axis',(0.686765675513281,-0.726878880513656,3.77922047493371E-49));
#42409=DIRECTION('ref_axis',(0.726878880513657,0.686765675513281,3.1589153081368E-66));
#42410=DIRECTION('',(-4.54587899183275E-49,9.04231552086907E-50,1.));
#42411=DIRECTION('center_axis',(-4.54587899183275E-49,9.04231552086907E-50,
1.));
#42412=DIRECTION('ref_axis',(1.,4.33680868994202E-19,4.54587899183275E-49));
#42413=DIRECTION('',(-4.54587899183275E-49,9.04231552086907E-50,1.));
#42414=DIRECTION('center_axis',(-0.999597651754094,-0.0283643192708926,
-4.51840205295607E-49));
#42415=DIRECTION('ref_axis',(0.0283643192708926,-0.999597651754094,-3.99287521021606E-67));
#42416=DIRECTION('center_axis',(0.627618346463361,-0.77852116938629,4.39267686269887E-49));
#42417=DIRECTION('ref_axis',(0.77852116938629,0.627618346463361,3.8324092947301E-66));
#42418=DIRECTION('',(-5.39293238409326E-49,1.29472851457609E-49,1.));
#42419=DIRECTION('center_axis',(-5.39293238409326E-49,1.29472851457609E-49,
1.));
#42420=DIRECTION('ref_axis',(-0.453990499739606,-0.891006524188338,-1.29472851457643E-49));
#42421=DIRECTION('',(-5.39293238409326E-49,1.29472851457609E-49,1.));
#42422=DIRECTION('center_axis',(-0.998741664633517,0.0501506463076103,-5.45107773834419E-49));
#42423=DIRECTION('ref_axis',(-0.0501506463076103,-0.998741664633517,1.75141110323522E-67));
#42424=DIRECTION('center_axis',(0.564601541603216,-0.825363616365098,4.94911614811808E-49));
#42425=DIRECTION('ref_axis',(0.825363616365098,0.564601541603216,-2.63676715352381E-65));
#42426=DIRECTION('',(-6.20673655487384E-49,1.75048074844164E-49,1.));
#42427=DIRECTION('center_axis',(-6.20673655487384E-49,1.75048074844164E-49,
1.));
#42428=DIRECTION('ref_axis',(-0.52249856471585,-0.852640164354153,-1.75048074844092E-49));
#42429=DIRECTION('',(-6.20673655487384E-49,1.75048074844164E-49,1.));
#42430=DIRECTION('center_axis',(-0.99172810303517,0.128356416474844,-6.38008050558225E-49));
#42431=DIRECTION('ref_axis',(-0.128356416474844,-0.99172810303517,-6.45104663994926E-66));
#42432=DIRECTION('center_axis',(0.498103780490022,-0.867117422187761,5.44510769796189E-49));
#42433=DIRECTION('ref_axis',(0.867117422187761,0.498103780490022,4.62928424055004E-65));
#42434=DIRECTION('',(-6.98227413084428E-49,2.26867838960881E-49,1.));
#42435=DIRECTION('center_axis',(-6.98227413084428E-49,2.26867838960881E-49,
1.));
#42436=DIRECTION('ref_axis',(-0.587785252292493,-0.809016994374933,-2.26867838960897E-49));
#42437=DIRECTION('',(-6.98227413084428E-49,2.26867838960881E-49,1.));
#42438=DIRECTION('center_axis',(-0.978600207898551,0.205770826651671,-7.29968274368548E-49));
#42439=DIRECTION('ref_axis',(-0.205770826651671,-0.978600207898551,-8.37640359713844E-66));
#42440=DIRECTION('center_axis',(0.428535043933792,-0.903525160756834,5.87759355939158E-49));
#42441=DIRECTION('ref_axis',(0.903525160756834,0.428535043933792,-6.0990810847752E-65));
#42442=DIRECTION('',(-7.71476366495631E-49,2.84612657730158E-49,1.));
#42443=DIRECTION('center_axis',(-7.71476366495631E-49,2.84612657730158E-49,
1.));
#42444=DIRECTION('ref_axis',(-0.649448048330161,-0.76040596560005,-2.84612657730134E-49));
#42445=DIRECTION('',(-7.71476366495631E-49,2.84612657730158E-49,1.));
#42446=DIRECTION('center_axis',(-0.959438917062647,0.281916591256448,-8.20421479905718E-49));
#42447=DIRECTION('ref_axis',(-0.281916591256448,-0.959438917062647,-3.25299225253391E-65));
#42448=DIRECTION('center_axis',(0.356324246329348,-0.934362366257237,6.2439073132553E-49));
#42449=DIRECTION('ref_axis',(0.934362366257237,0.356324246329348,-6.3916346242107E-66));
#42450=DIRECTION('',(-8.39968911565463E-49,3.47926515142182E-49,1.));
#42451=DIRECTION('center_axis',(-8.39968911565463E-49,3.47926515142182E-49,
1.));
#42452=DIRECTION('ref_axis',(-0.707106781186566,-0.707106781186529,-3.47926515142204E-49));
#42453=DIRECTION('',(-8.39968911565463E-49,3.47926515142182E-49,1.));
#42454=DIRECTION('center_axis',(-0.934362366257236,0.356324246329348,-9.08809993078856E-49));
#42455=DIRECTION('ref_axis',(-0.356324246329348,-0.934362366257236,-6.41640199023417E-65));
#42456=DIRECTION('center_axis',(0.281916591256447,-0.959438917062647,6.54179051344879E-49));
#42457=DIRECTION('ref_axis',(0.959438917062647,0.281916591256447,-1.09781434718078E-65));
#42458=DIRECTION('',(-9.03282768977487E-49,4.16419060212015E-49,1.));
#42459=DIRECTION('center_axis',(-9.03282768977487E-49,4.16419060212015E-49,
1.));
#42460=DIRECTION('ref_axis',(-0.760405965599942,-0.649448048330288,-4.16419060211889E-49));
#42461=DIRECTION('',(-9.03282768977487E-49,4.16419060212015E-49,1.));
#42462=DIRECTION('center_axis',(-0.903525160756834,0.428535043933793,-9.94588869312087E-49));
#42463=DIRECTION('ref_axis',(-0.428535043933793,-0.903525160756834,3.14193955482054E-65));
#42464=DIRECTION('center_axis',(0.205770826651671,-0.978600207898551,6.76940661098664E-49));
#42465=DIRECTION('ref_axis',(0.978600207898551,0.205770826651671,1.21103353553181E-65));
#42466=DIRECTION('',(-9.61027587746764E-49,4.89668013623218E-49,1.));
#42467=DIRECTION('center_axis',(-9.61027587746764E-49,4.89668013623218E-49,
1.));
#42468=DIRECTION('ref_axis',(-0.809016994374948,-0.587785252292472,-4.89668013623217E-49));
#42469=DIRECTION('',(-9.61027587746764E-49,4.89668013623218E-49,1.));
#42470=DIRECTION('center_axis',(-0.867117422187761,0.498103780490022,-1.07722925330906E-48));
#42471=DIRECTION('ref_axis',(-0.498103780490022,-0.867117422187761,1.20400755006059E-65));
#42472=DIRECTION('center_axis',(0.128356416474844,-0.99172810303517,6.92535227693751E-49));
#42473=DIRECTION('ref_axis',(0.99172810303517,0.128356416474844,1.37955244398014E-65));
#42474=DIRECTION('',(-1.01284735186348E-48,5.67221771220262E-49,1.));
#42475=DIRECTION('center_axis',(-1.01284735186348E-48,5.67221771220262E-49,
1.));
#42476=DIRECTION('ref_axis',(-0.852640164354111,-0.522498564715917,-5.67221771220297E-49));
#42477=DIRECTION('',(-1.01284735186348E-48,5.67221771220262E-49,1.));
#42478=DIRECTION('center_axis',(-0.825363616365097,0.564601541603216,-1.15622163962172E-48));
#42479=DIRECTION('ref_axis',(-0.564601541603216,-0.825363616365097,3.75089637720347E-65));
#42480=DIRECTION('center_axis',(0.0501506463076098,-0.998741664633517,7.0086660544136E-49));
#42481=DIRECTION('ref_axis',(0.998741664633517,0.0501506463076098,-1.39822384050416E-65));
#42482=DIRECTION('',(-1.05842257525004E-48,6.4860218829832E-49,1.));
#42483=DIRECTION('center_axis',(-1.05842257525004E-48,6.4860218829832E-49,
1.));
#42484=DIRECTION('ref_axis',(-0.891006524188326,-0.453990499739629,-6.48602188298224E-49));
#42485=DIRECTION('',(-1.05842257525004E-48,6.4860218829832E-49,1.));
#42486=DIRECTION('center_axis',(-0.77852116938629,0.627618346463361,-1.23107901392082E-48));
#42487=DIRECTION('ref_axis',(-0.627618346463361,-0.77852116938629,-1.0235164758246E-65));
#42488=DIRECTION('center_axis',(-0.0283643192708931,-0.999597651754094,
7.01883428627214E-49));
#42489=DIRECTION('ref_axis',(0.999597651754094,-0.0283643192708931,-4.40612052675408E-66));
#42490=DIRECTION('',(-1.09747227149895E-48,7.33307527524372E-49,1.));
#42491=DIRECTION('center_axis',(-1.09747227149895E-48,7.33307527524372E-49,
1.));
#42492=DIRECTION('ref_axis',(-0.923879532511259,-0.382683432365157,-7.33307527524286E-49));
#42493=DIRECTION('',(-1.09747227149895E-48,7.33307527524372E-49,1.));
#42494=DIRECTION('center_axis',(-0.726878880513656,0.686765675513282,-1.30133985560119E-48));
#42495=DIRECTION('ref_axis',(-0.686765675513282,-0.726878880513656,-1.0460740182702E-64));
#42496=DIRECTION('center_axis',(-0.106704409388998,-0.994290786951657,6.95579428198243E-49));
#42497=DIRECTION('ref_axis',(0.994290786951657,-0.106704409388998,-7.09717408543387E-66));
#42498=DIRECTION('',(-1.12975568624752E-48,8.20815552314704E-49,1.));
#42499=DIRECTION('center_axis',(-1.12975568624752E-48,8.20815552314704E-49,
1.));
#42500=DIRECTION('ref_axis',(-0.951056516295187,-0.309016994374844,-8.20815552314827E-49));
#42501=DIRECTION('',(-1.12975568624752E-48,8.20815552314704E-49,1.));
#42502=DIRECTION('center_axis',(-0.6707551416309,0.741678865800901,-1.36657098320978E-48));
#42503=DIRECTION('ref_axis',(-0.741678865800901,-0.6707551416309,3.57211103088032E-65));
#42504=DIRECTION('center_axis',(-0.184386631340402,-0.982853788812425,6.81993470413386E-49));
#42505=DIRECTION('ref_axis',(0.982853788812425,-0.184386631340402,2.71684956354986E-65));
#42506=DIRECTION('',(-1.15507378150848E-48,9.10586746597114E-49,1.));
#42507=DIRECTION('center_axis',(-1.15507378150848E-48,9.10586746597114E-49,
1.));
#42508=DIRECTION('ref_axis',(-0.972369920397692,-0.233445363855843,-9.1058674659719E-49));
#42509=DIRECTION('',(-1.15507378150848E-48,9.10586746597114E-49,1.));
#42510=DIRECTION('center_axis',(-0.610495974251271,0.792019359247608,-1.42637022515333E-48));
#42511=DIRECTION('ref_axis',(-0.792019359247608,-0.610495974251271,3.09249712984754E-64));
#42512=DIRECTION('center_axis',(-0.260932048394816,-0.965357170233114,6.61209317220174E-49));
#42513=DIRECTION('ref_axis',(0.965357170233114,-0.260932048394816,1.42679734120621E-65));
#42514=DIRECTION('',(-1.17327046280543E-48,1.0020676411069E-48,1.));
#42515=DIRECTION('center_axis',(-1.17327046280543E-48,1.0020676411069E-48,
1.));
#42516=DIRECTION('ref_axis',(-0.987688340595155,-0.156434465040119,-1.00206764110703E-48));
#42517=DIRECTION('',(-1.17327046280543E-48,1.0020676411069E-48,1.));
#42518=DIRECTION('center_axis',(-0.546472896179871,0.83747678997139,-1.48036889921999E-48));
#42519=DIRECTION('ref_axis',(-0.83747678997139,-0.546472896179871,5.98336102584152E-65));
#42520=DIRECTION('center_axis',(-0.335868732602165,-0.941908803685482,6.33355109834478E-49));
#42521=DIRECTION('ref_axis',(0.941908803685482,-0.335868732602165,5.83703495410428E-65));
#42522=DIRECTION('',(-1.18423354154716E-48,1.09469422570892E-48,1.));
#42523=DIRECTION('center_axis',(-1.18423354154716E-48,1.09469422570892E-48,
1.));
#42524=DIRECTION('ref_axis',(-0.996917333733132,-0.0784590957277897,-1.09469422570898E-48));
#42525=DIRECTION('',(-1.18423354154716E-48,1.09469422570892E-48,1.));
#42526=DIRECTION('center_axis',(-0.479080630982844,0.877770897795706,-1.52823408562776E-48));
#42527=DIRECTION('ref_axis',(-0.877770897795706,-0.479080630982844,-1.85065299173653E-65));
#42528=DIRECTION('center_axis',(-0.408734674385335,-0.912653256146667,5.98602578707292E-49));
#42529=DIRECTION('ref_axis',(0.912653256146667,-0.408734674385335,-4.742731066544E-66));
#42530=DIRECTION('',(-1.18789542670764E-48,1.18789542670765E-48,1.));
#42531=DIRECTION('center_axis',(-1.18789542670764E-48,1.18789542670765E-48,
1.));
#42532=DIRECTION('ref_axis',(4.33680868994202E-19,-1.,1.18789542670765E-48));
#42533=DIRECTION('',(-1.18789542670764E-48,1.18789542670765E-48,1.));
#42534=DIRECTION('center_axis',(-0.408734674385331,0.912653256146669,-1.56967067958564E-48));
#42535=DIRECTION('ref_axis',(-0.912653256146669,-0.408734674385331,-1.44539080722799E-64));
#42536=DIRECTION('center_axis',(-0.479080630982847,-0.877770897795704,5.57165984749406E-49));
#42537=DIRECTION('ref_axis',(0.877770897795704,-0.479080630982847,-3.32989513528092E-65));
#42538=DIRECTION('',(-1.18423354154716E-48,1.28109662770637E-48,1.));
#42539=DIRECTION('center_axis',(-1.18423354154716E-48,1.28109662770637E-48,
1.));
#42540=DIRECTION('ref_axis',(4.33680868994202E-19,-1.,1.28109662770637E-48));
#42541=DIRECTION('',(-1.18423354154716E-48,1.28109662770637E-48,1.));
#42542=DIRECTION('center_axis',(-0.335868732602161,0.941908803685483,-1.60442321071283E-48));
#42543=DIRECTION('ref_axis',(-0.941908803685483,-0.335868732602161,-1.10077185323049E-64));
#42544=DIRECTION('center_axis',(-0.546472896179874,-0.837476789971388,5.09300798341636E-49));
#42545=DIRECTION('ref_axis',(0.837476789971388,-0.546472896179874,-4.24396990687181E-65));
#42546=DIRECTION('',(-1.17327046280542E-48,1.37372321230839E-48,1.));
#42547=DIRECTION('center_axis',(-1.17327046280542E-48,1.37372321230839E-48,
1.));
#42548=DIRECTION('ref_axis',(4.33680868994202E-19,-1.,1.37372321230839E-48));
#42549=DIRECTION('',(-1.17327046280542E-48,1.37372321230839E-48,1.));
#42550=DIRECTION('center_axis',(-0.260932048394812,0.965357170233115,-1.63227741809852E-48));
#42551=DIRECTION('ref_axis',(-0.965357170233115,-0.260932048394812,1.79840374663787E-65));
#42552=DIRECTION('center_axis',(-0.610495974251274,-0.792019359247605,4.55302124274975E-49));
#42553=DIRECTION('ref_axis',(0.792019359247605,-0.610495974251274,-1.92107929694605E-65));
#42554=DIRECTION('',(-1.15507378150847E-48,1.46520410681818E-48,1.));
#42555=DIRECTION('center_axis',(-1.15507378150847E-48,1.46520410681818E-48,
1.));
#42556=DIRECTION('ref_axis',(4.33680868994202E-19,-1.,1.46520410681818E-48));
#42557=DIRECTION('',(-1.15507378150847E-48,1.46520410681818E-48,1.));
#42558=DIRECTION('center_axis',(-0.184386631340398,0.982853788812426,-1.65306157129174E-48));
#42559=DIRECTION('ref_axis',(-0.982853788812426,-0.184386631340398,3.00112067034686E-65));
#42560=DIRECTION('center_axis',(-0.670755141630903,-0.741678865800898,3.95502882331426E-49));
#42561=DIRECTION('ref_axis',(0.741678865800898,-0.670755141630903,1.84878394507284E-65));
#42562=DIRECTION('',(-1.12975568624751E-48,1.55497530110059E-48,1.));
#42563=DIRECTION('center_axis',(-1.12975568624751E-48,1.55497530110059E-48,
1.));
#42564=DIRECTION('ref_axis',(4.33680868994202E-19,-1.,1.55497530110059E-48));
#42565=DIRECTION('',(-1.12975568624751E-48,1.55497530110059E-48,1.));
#42566=DIRECTION('center_axis',(-0.106704409388993,0.994290786951657,-1.66664752907659E-48));
#42567=DIRECTION('ref_axis',(-0.994290786951658,-0.106704409388993,-2.84767254643969E-65));
#42568=DIRECTION('center_axis',(-0.726878880513659,-0.686765675513279,3.30271754722836E-49));
#42569=DIRECTION('ref_axis',(0.686765675513279,-0.726878880513659,1.35737227185702E-66));
#42570=DIRECTION('',(-1.09747227149895E-48,1.64248332589092E-48,1.));
#42571=DIRECTION('center_axis',(-1.09747227149895E-48,1.64248332589092E-48,
1.));
#42572=DIRECTION('ref_axis',(4.33680868994202E-19,-1.,1.64248332589092E-48));
#42573=DIRECTION('',(-1.09747227149895E-48,1.64248332589092E-48,1.));
#42574=DIRECTION('center_axis',(-0.0283643192708891,0.999597651754094,-1.67295152950556E-48));
#42575=DIRECTION('ref_axis',(-0.999597651754094,-0.0283643192708891,-1.01926051780483E-65));
#42576=DIRECTION('center_axis',(-0.778521169386292,-0.627618346463358,2.60010913042463E-49));
#42577=DIRECTION('ref_axis',(0.627618346463358,-0.778521169386292,-1.77736454987801E-64));
#42578=DIRECTION('',(-1.05842257525003E-48,1.72718866511697E-48,1.));
#42579=DIRECTION('center_axis',(-1.05842257525003E-48,1.72718866511697E-48,
1.));
#42580=DIRECTION('ref_axis',(-0.891006524188322,0.453990499739636,-1.72718866511707E-48));
#42581=DIRECTION('',(-1.05842257525003E-48,1.72718866511697E-48,1.));
#42582=DIRECTION('center_axis',(0.050150646307614,0.998741664633517,-1.67193470631971E-48));
#42583=DIRECTION('ref_axis',(-0.998741664633517,0.050150646307614,1.52017605534737E-65));
#42584=DIRECTION('center_axis',(-0.8253636163651,-0.564601541603213,1.85153538743368E-49));
#42585=DIRECTION('ref_axis',(0.564601541603213,-0.8253636163651,-7.9609822926636E-66));
#42586=DIRECTION('',(-1.01284735186348E-48,1.80856908219503E-48,1.));
#42587=DIRECTION('center_axis',(-1.01284735186348E-48,1.80856908219503E-48,
1.));
#42588=DIRECTION('ref_axis',(-0.852640164354107,0.522498564715924,-1.808569082195E-48));
#42589=DIRECTION('',(-1.01284735186348E-48,1.80856908219503E-48,1.));
#42590=DIRECTION('center_axis',(0.128356416474848,0.991728103035169,-1.6636033285721E-48));
#42591=DIRECTION('ref_axis',(-0.991728103035169,0.128356416474848,-6.99057875847398E-66));
#42592=DIRECTION('center_axis',(-0.867117422187763,-0.498103780490019,1.06161152430708E-49));
#42593=DIRECTION('ref_axis',(0.498103780490019,-0.867117422187763,1.00088346227585E-65));
#42594=DIRECTION('',(-9.61027587746759E-49,1.88612283979207E-48,1.));
#42595=DIRECTION('center_axis',(-9.61027587746759E-49,1.88612283979207E-48,
1.));
#42596=DIRECTION('ref_axis',(-0.809016994374894,0.587785252292546,-1.88612283979215E-48));
#42597=DIRECTION('',(-9.61027587746759E-49,1.88612283979207E-48,1.));
#42598=DIRECTION('center_axis',(0.205770826651675,0.978600207898551,-1.64800876197701E-48));
#42599=DIRECTION('ref_axis',(-0.978600207898551,0.205770826651675,2.0991990898783E-65));
#42600=DIRECTION('center_axis',(-0.903525160756836,-0.428535043933789,2.35207684337335E-50));
#42601=DIRECTION('ref_axis',(0.428535043933789,-0.903525160756836,-9.18347163738211E-68));
#42602=DIRECTION('',(-9.03282768977482E-49,1.95937179320328E-48,1.));
#42603=DIRECTION('center_axis',(-9.03282768977482E-49,1.95937179320328E-48,
1.));
#42604=DIRECTION('ref_axis',(-0.760405965599999,0.649448048330221,-1.95937179320332E-48));
#42605=DIRECTION('',(-9.03282768977482E-49,1.95937179320328E-48,1.));
#42606=DIRECTION('center_axis',(0.281916591256451,0.959438917062646,-1.62524715222323E-48));
#42607=DIRECTION('ref_axis',(-0.959438917062646,0.281916591256451,8.99283719863503E-66));
#42608=DIRECTION('center_axis',(-0.934362366257238,-0.356324246329344,-6.22581077994971E-50));
#42609=DIRECTION('ref_axis',(0.356324246329344,-0.934362366257238,-2.14283631075808E-67));
#42610=DIRECTION('',(-8.39968911565457E-49,2.02786433827311E-48,1.));
#42611=DIRECTION('center_axis',(-8.39968911565457E-49,2.02786433827311E-48,
1.));
#42612=DIRECTION('ref_axis',(-0.707106781186559,0.707106781186536,-2.02786433827309E-48));
#42613=DIRECTION('',(-8.39968911565457E-49,2.02786433827311E-48,1.));
#42614=DIRECTION('center_axis',(0.356324246329351,0.934362366257235,-1.59545883220388E-48));
#42615=DIRECTION('ref_axis',(-0.934362366257235,0.356324246329351,6.60900149289003E-65));
#42616=DIRECTION('center_axis',(-0.959438917062648,-0.281916591256444,-1.50646620972636E-49));
#42617=DIRECTION('ref_axis',(0.281916591256444,-0.959438917062648,3.84808191287826E-66));
#42618=DIRECTION('',(-7.71476366495624E-49,2.09117819568513E-48,1.));
#42619=DIRECTION('center_axis',(-7.71476366495624E-49,2.09117819568513E-48,
1.));
#42620=DIRECTION('ref_axis',(-0.649448048330135,0.760405965600073,-2.09117819568518E-48));
#42621=DIRECTION('',(-7.71476366495624E-49,2.09117819568513E-48,1.));
#42622=DIRECTION('center_axis',(0.428535043933796,0.903525160756832,-1.5588274568175E-48));
#42623=DIRECTION('ref_axis',(-0.903525160756832,0.428535043933796,-3.10862492143316E-66));
#42624=DIRECTION('center_axis',(-0.978600207898552,-0.205770826651667,-2.41099826509806E-49));
#42625=DIRECTION('ref_axis',(0.205770826651667,-0.978600207898552,1.22158844253494E-66));
#42626=DIRECTION('',(-6.98227413084421E-49,2.14892301445441E-48,1.));
#42627=DIRECTION('center_axis',(-6.98227413084421E-49,2.14892301445441E-48,
1.));
#42628=DIRECTION('ref_axis',(-0.587785252292501,0.809016994374927,-2.14892301445438E-48));
#42629=DIRECTION('',(-6.98227413084421E-49,2.14892301445441E-48,1.));
#42630=DIRECTION('center_axis',(0.498103780490025,0.867117422187759,-1.51557887067454E-48));
#42631=DIRECTION('ref_axis',(-0.867117422187759,0.498103780490025,2.99504754920617E-65));
#42632=DIRECTION('center_axis',(-0.99172810303517,-0.128356416474841,-3.33060050320128E-49));
#42633=DIRECTION('ref_axis',(0.128356416474841,-0.99172810303517,-3.10963647347836E-66));
#42634=DIRECTION('',(-6.20673655487377E-49,2.20074277857113E-48,1.));
#42635=DIRECTION('center_axis',(-6.20673655487377E-49,2.20074277857113E-48,
1.));
#42636=DIRECTION('ref_axis',(-0.522498564715884,0.852640164354132,-2.20074277857117E-48));
#42637=DIRECTION('',(-6.20673655487377E-49,2.20074277857113E-48,1.));
#42638=DIRECTION('center_axis',(0.564601541603219,0.825363616365096,-1.46597971569015E-48));
#42639=DIRECTION('ref_axis',(-0.825363616365096,0.564601541603219,-1.28895308917342E-64));
#42640=DIRECTION('center_axis',(-0.998741664633517,-0.0501506463076061,
-4.25960327043935E-49));
#42641=DIRECTION('ref_axis',(0.0501506463076061,-0.998741664633517,-2.80568036684895E-66));
#42642=DIRECTION('',(-5.39293238409318E-49,2.24631800195768E-48,1.));
#42643=DIRECTION('center_axis',(-5.39293238409318E-49,2.24631800195768E-48,
1.));
#42644=DIRECTION('ref_axis',(-0.453990499739489,0.891006524188397,-2.24631800195771E-48));
#42645=DIRECTION('',(-5.39293238409318E-49,2.24631800195768E-48,1.));
#42646=DIRECTION('center_axis',(0.627618346463364,0.778521169386287,-1.41033578714823E-48));
#42647=DIRECTION('ref_axis',(-0.778521169386288,0.627618346463364,5.07659402759256E-65));
#42648=DIRECTION('center_axis',(-0.999597651754094,0.0283643192708965,-5.19227895582746E-49));
#42649=DIRECTION('ref_axis',(-0.0283643192708965,-0.999597651754094,2.50391620144835E-67));
#42650=DIRECTION('',(-4.54587899183267E-49,2.2853676982066E-48,1.));
#42651=DIRECTION('center_axis',(-4.54587899183267E-49,2.2853676982066E-48,
1.));
#42652=DIRECTION('ref_axis',(-0.382683432365006,0.923879532511321,-2.28536769820664E-48));
#42653=DIRECTION('',(-4.54587899183267E-49,2.2853676982066E-48,1.));
#42654=DIRECTION('center_axis',(0.686765675513284,0.726878880513654,-1.34899014837172E-48));
#42655=DIRECTION('ref_axis',(-0.726878880513654,0.686765675513284,4.51664321804638E-65));
#42656=DIRECTION('center_axis',(-0.994290786951657,0.106704409389001,-6.12287730361908E-49));
#42657=DIRECTION('ref_axis',(-0.106704409389001,-0.994290786951657,-3.36897451344462E-66));
#42658=DIRECTION('',(-3.67079874392934E-49,2.31765111295516E-48,1.));
#42659=DIRECTION('center_axis',(-3.67079874392934E-49,2.31765111295516E-48,
1.));
#42660=DIRECTION('ref_axis',(-0.309016994374936,0.951056516295157,-2.31765111295516E-48));
#42661=DIRECTION('',(-3.67079874392934E-49,2.31765111295516E-48,1.));
#42662=DIRECTION('center_axis',(0.741678865800904,0.670755141630897,-1.28232101562316E-48));
#42663=DIRECTION('ref_axis',(-0.670755141630897,0.741678865800904,-7.13448931820408E-65));
#42664=DIRECTION('center_axis',(-0.982853788812424,0.184386631340406,-7.04566086554469E-49));
#42665=DIRECTION('ref_axis',(-0.184386631340406,-0.982853788812424,1.03257498418151E-65));
#42666=DIRECTION('',(-2.77308680110524E-49,2.34296920821612E-48,1.));
#42667=DIRECTION('center_axis',(-2.77308680110524E-49,2.34296920821612E-48,
1.));
#42668=DIRECTION('ref_axis',(-0.233445363855831,0.972369920397695,-2.34296920821614E-48));
#42669=DIRECTION('',(-2.77308680110524E-49,2.34296920821612E-48,1.));
#42670=DIRECTION('center_axis',(0.79201935924761,0.610495974251268,-1.21073942627568E-48));
#42671=DIRECTION('ref_axis',(-0.610495974251268,0.79201935924761,-4.36775682720849E-65));
#42672=DIRECTION('center_axis',(-0.965357170233113,0.260932048394819,-7.95494037408836E-49));
#42673=DIRECTION('ref_axis',(-0.260932048394819,-0.965357170233113,-3.47978634051958E-65));
#42674=DIRECTION('',(-1.85827785600739E-49,2.36116588951307E-48,1.));
#42675=DIRECTION('center_axis',(-1.85827785600739E-49,2.36116588951307E-48,
1.));
#42676=DIRECTION('ref_axis',(-0.156434465040246,0.987688340595135,-2.36116588951307E-48));
#42677=DIRECTION('',(-1.85827785600739E-49,2.36116588951307E-48,1.));
#42678=DIRECTION('center_axis',(0.837476789971392,0.546472896179868,-1.13468670463092E-48));
#42679=DIRECTION('ref_axis',(-0.546472896179868,0.837476789971392,7.35185048458512E-65));
#42680=DIRECTION('center_axis',(-0.94190880368548,0.335868732602169,-8.84510981871381E-49));
#42681=DIRECTION('ref_axis',(-0.335868732602169,-0.94190880368548,-2.80378683690505E-64));
#42682=DIRECTION('',(-9.32012009987159E-50,2.3721289682548E-48,1.));
#42683=DIRECTION('center_axis',(-9.32012009987159E-50,2.3721289682548E-48,
1.));
#42684=DIRECTION('ref_axis',(-0.0784590957277844,0.996917333733133,-2.3721289682548E-48));
#42685=DIRECTION('',(-9.32012009987159E-50,2.3721289682548E-48,1.));
#42686=DIRECTION('center_axis',(0.877770897795708,0.47908063098284,-1.0546317410079E-48));
#42687=DIRECTION('ref_axis',(-0.47908063098284,0.877770897795708,-1.46432166581228E-64));
#42688=DIRECTION('center_axis',(-0.912653256146669,0.408734674385332,-9.71068100878346E-49));
#42689=DIRECTION('ref_axis',(-0.408734674385332,-0.912653256146669,4.78015562106795E-65));
#42690=DIRECTION('',(-1.03033504185762E-66,2.37579085341529E-48,1.));
#42691=DIRECTION('center_axis',(-1.03033504185762E-66,2.37579085341529E-48,
1.));
#42692=DIRECTION('ref_axis',(-5.51899603821915E-14,1.,-2.37579085341529E-48));
#42693=DIRECTION('',(-1.03033504185762E-66,2.37579085341529E-48,1.));
#42694=DIRECTION('center_axis',(0.912653256146668,0.408734674385334,-9.71068100878352E-49));
#42695=DIRECTION('ref_axis',(-0.408734674385334,0.912653256146668,-3.97320112854764E-64));
#42696=DIRECTION('center_axis',(-0.877770897795703,0.47908063098285,-1.05463174100791E-48));
#42697=DIRECTION('ref_axis',(-0.47908063098285,-0.877770897795703,8.5181126283276E-66));
#42698=DIRECTION('',(9.32012009987329E-50,2.3721289682548E-48,1.));
#42699=DIRECTION('center_axis',(9.32012009987329E-50,2.3721289682548E-48,
1.));
#42700=DIRECTION('ref_axis',(0.078459095727909,0.996917333733123,-2.37212896825479E-48));
#42701=DIRECTION('',(9.32012009987329E-50,2.3721289682548E-48,1.));
#42702=DIRECTION('center_axis',(0.941908803685484,0.335868732602158,-8.84510981871371E-49));
#42703=DIRECTION('ref_axis',(-0.335868732602158,0.941908803685484,-1.44601818635795E-65));
#42704=DIRECTION('center_axis',(-0.837476789971386,0.546472896179877,-1.13468670463093E-48));
#42705=DIRECTION('ref_axis',(-0.546472896179877,-0.837476789971386,1.1507371701338E-64));
#42706=DIRECTION('',(1.85827785600756E-49,2.36116588951307E-48,1.));
#42707=DIRECTION('center_axis',(1.85827785600756E-49,2.36116588951307E-48,
1.));
#42708=DIRECTION('ref_axis',(0.156434465040226,0.987688340595138,-2.36116588951307E-48));
#42709=DIRECTION('',(1.85827785600756E-49,2.36116588951307E-48,1.));
#42710=DIRECTION('center_axis',(0.965357170233116,0.260932048394809,-7.95494037408827E-49));
#42711=DIRECTION('ref_axis',(-0.260932048394809,0.965357170233116,-4.20694512990981E-65));
#42712=DIRECTION('center_axis',(-0.792019359247603,0.610495974251277,-1.21073942627569E-48));
#42713=DIRECTION('ref_axis',(-0.610495974251277,-0.792019359247603,-2.13945998802071E-65));
#42714=DIRECTION('',(2.7730868011054E-49,2.34296920821612E-48,1.));
#42715=DIRECTION('center_axis',(2.7730868011054E-49,2.34296920821612E-48,
1.));
#42716=DIRECTION('ref_axis',(0.233445363855898,0.972369920397678,-2.34296920821612E-48));
#42717=DIRECTION('',(2.7730868011054E-49,2.34296920821612E-48,1.));
#42718=DIRECTION('center_axis',(0.982853788812426,0.184386631340395,-7.04566086554459E-49));
#42719=DIRECTION('ref_axis',(-0.184386631340395,0.982853788812426,-1.76256118611904E-65));
#42720=DIRECTION('center_axis',(-0.741678865800896,0.670755141630906,-1.28232101562316E-48));
#42721=DIRECTION('ref_axis',(-0.670755141630906,-0.741678865800896,1.75561258236883E-65));
#42722=DIRECTION('',(3.6707987439295E-49,2.31765111295516E-48,1.));
#42723=DIRECTION('center_axis',(3.6707987439295E-49,2.31765111295516E-48,
1.));
#42724=DIRECTION('ref_axis',(0.309016994374949,0.951056516295153,-2.31765111295516E-48));
#42725=DIRECTION('',(3.6707987439295E-49,2.31765111295516E-48,1.));
#42726=DIRECTION('center_axis',(0.994290786951658,0.10670440938899,-6.12287730361897E-49));
#42727=DIRECTION('ref_axis',(-0.10670440938899,0.994290786951658,-7.83421067979577E-66));
#42728=DIRECTION('center_axis',(-0.686765675513276,0.726878880513661,-1.34899014837172E-48));
#42729=DIRECTION('ref_axis',(-0.726878880513661,-0.686765675513276,5.3563970103269E-65));
#42730=DIRECTION('',(4.54587899183282E-49,2.28536769820659E-48,1.));
#42731=DIRECTION('center_axis',(4.54587899183282E-49,2.28536769820659E-48,
1.));
#42732=DIRECTION('ref_axis',(0.382683432365024,0.923879532511314,-2.28536769820663E-48));
#42733=DIRECTION('',(4.54587899183282E-49,2.28536769820659E-48,1.));
#42734=DIRECTION('center_axis',(0.999597651754094,0.0283643192708856,-5.19227895582736E-49));
#42735=DIRECTION('ref_axis',(-0.0283643192708856,0.999597651754094,1.94568536261846E-66));
#42736=DIRECTION('center_axis',(-0.627618346463355,0.778521169386295,-1.41033578714824E-48));
#42737=DIRECTION('ref_axis',(-0.778521169386295,-0.627618346463355,-4.32781502974933E-65));
#42738=DIRECTION('',(5.39293238409334E-49,2.24631800195767E-48,1.));
#42739=DIRECTION('center_axis',(5.39293238409334E-49,2.24631800195767E-48,
1.));
#42740=DIRECTION('ref_axis',(0.45399049973962,0.89100652418833,-2.24631800195763E-48));
#42741=DIRECTION('',(5.39293238409334E-49,2.24631800195767E-48,1.));
#42742=DIRECTION('center_axis',(0.998741664633517,-0.0501506463076175,-4.25960327043925E-49));
#42743=DIRECTION('ref_axis',(0.0501506463076175,0.998741664633517,-4.14088422014228E-66));
#42744=DIRECTION('center_axis',(-0.56460154160321,0.825363616365102,-1.46597971569016E-48));
#42745=DIRECTION('ref_axis',(-0.825363616365102,-0.56460154160321,7.97777118454868E-65));
#42746=DIRECTION('',(6.20673655487391E-49,2.20074277857112E-48,1.));
#42747=DIRECTION('center_axis',(6.20673655487391E-49,2.20074277857112E-48,
1.));
#42748=DIRECTION('ref_axis',(0.522498564715976,0.852640164354076,-2.20074277857111E-48));
#42749=DIRECTION('',(6.20673655487391E-49,2.20074277857112E-48,1.));
#42750=DIRECTION('center_axis',(0.991728103035169,-0.128356416474851,-3.33060050320119E-49));
#42751=DIRECTION('ref_axis',(0.128356416474851,0.991728103035169,2.08257490756294E-67));
#42752=DIRECTION('center_axis',(-0.498103780490015,0.867117422187765,-1.51557887067454E-48));
#42753=DIRECTION('ref_axis',(-0.867117422187765,-0.498103780490015,2.18779707200991E-65));
#42754=DIRECTION('',(6.98227413084436E-49,2.1489230144544E-48,1.));
#42755=DIRECTION('center_axis',(6.98227413084435E-49,2.1489230144544E-48,
1.));
#42756=DIRECTION('ref_axis',(0.587785252292489,0.809016994374936,-2.14892301445439E-48));
#42757=DIRECTION('',(6.98227413084436E-49,2.1489230144544E-48,1.));
#42758=DIRECTION('center_axis',(0.97860020789855,-0.205770826651679,-2.41099826509796E-49));
#42759=DIRECTION('ref_axis',(0.205770826651679,0.97860020789855,-2.74077973100627E-66));
#42760=DIRECTION('center_axis',(-0.428535043933785,0.903525160756837,-1.55882745681751E-48));
#42761=DIRECTION('ref_axis',(-0.903525160756837,-0.428535043933785,-8.73188639847288E-65));
#42762=DIRECTION('',(7.71476366495637E-49,2.09117819568512E-48,1.));
#42763=DIRECTION('center_axis',(7.71476366495637E-49,2.09117819568512E-48,
1.));
#42764=DIRECTION('ref_axis',(0.649448048330186,0.760405965600029,-2.09117819568512E-48));
#42765=DIRECTION('',(7.71476366495637E-49,2.09117819568512E-48,1.));
#42766=DIRECTION('center_axis',(0.959438917062645,-0.281916591256455,-1.50646620972626E-49));
#42767=DIRECTION('ref_axis',(0.281916591256455,0.959438917062645,-2.91844467010393E-67));
#42768=DIRECTION('center_axis',(-0.356324246329341,0.934362366257239,-1.59545883220388E-48));
#42769=DIRECTION('ref_axis',(-0.934362366257239,-0.356324246329341,1.49301625507406E-64));
#42770=DIRECTION('',(8.39968911565469E-49,2.0278643382731E-48,1.));
#42771=DIRECTION('center_axis',(8.39968911565469E-49,2.0278643382731E-48,
1.));
#42772=DIRECTION('ref_axis',(0.707106781186573,0.707106781186522,-2.02786433827308E-48));
#42773=DIRECTION('',(8.39968911565469E-49,2.0278643382731E-48,1.));
#42774=DIRECTION('center_axis',(0.934362366257234,-0.356324246329355,-6.22581077994883E-50));
#42775=DIRECTION('ref_axis',(0.356324246329355,0.934362366257234,-4.97582464336991E-66));
#42776=DIRECTION('center_axis',(-0.28191659125644,0.959438917062649,-1.62524715222323E-48));
#42777=DIRECTION('ref_axis',(-0.959438917062649,-0.28191659125644,-5.29515836320384E-66));
#42778=DIRECTION('',(9.03282768977493E-49,1.95937179320326E-48,1.));
#42779=DIRECTION('center_axis',(9.03282768977493E-49,1.95937179320326E-48,
1.));
#42780=DIRECTION('ref_axis',(0.760405965600079,0.649448048330127,-1.9593717932032E-48));
#42781=DIRECTION('',(9.03282768977493E-49,1.95937179320326E-48,1.));
#42782=DIRECTION('center_axis',(0.903525160756831,-0.428535043933799,2.35207684337425E-50));
#42783=DIRECTION('ref_axis',(0.428535043933799,0.903525160756831,3.46790681006673E-67));
#42784=DIRECTION('center_axis',(-0.205770826651664,0.978600207898553,-1.64800876197701E-48));
#42785=DIRECTION('ref_axis',(-0.978600207898553,-0.205770826651664,-5.70930081633759E-65));
#42786=DIRECTION('',(9.61027587746769E-49,1.88612283979206E-48,1.));
#42787=DIRECTION('center_axis',(9.61027587746769E-49,1.88612283979206E-48,
1.));
#42788=DIRECTION('ref_axis',(0.809016994374978,0.587785252292432,-1.88612283979202E-48));
#42789=DIRECTION('',(9.61027587746769E-49,1.88612283979206E-48,1.));
#42790=DIRECTION('center_axis',(0.867117422187757,-0.498103780490029,1.06161152430717E-49));
#42791=DIRECTION('ref_axis',(0.498103780490029,0.867117422187757,8.6756046158998E-66));
#42792=DIRECTION('center_axis',(-0.128356416474837,0.991728103035171,-1.6636033285721E-48));
#42793=DIRECTION('ref_axis',(-0.991728103035171,-0.128356416474837,3.98742758462882E-65));
#42794=DIRECTION('',(1.01284735186348E-48,1.80856908219502E-48,1.));
#42795=DIRECTION('center_axis',(1.01284735186348E-48,1.80856908219502E-48,
1.));
#42796=DIRECTION('ref_axis',(0.852640164354111,0.522498564715918,-1.80856908219499E-48));
#42797=DIRECTION('',(1.01284735186348E-48,1.80856908219502E-48,1.));
#42798=DIRECTION('center_axis',(0.825363616365094,-0.564601541603222,1.85153538743376E-49));
#42799=DIRECTION('ref_axis',(0.564601541603222,0.825363616365094,-1.20460226317478E-65));
#42800=DIRECTION('center_axis',(-0.0501506463076026,0.998741664633518,-1.67193470631971E-48));
#42801=DIRECTION('ref_axis',(-0.998741664633518,-0.0501506463076026,9.17993822873344E-66));
#42802=DIRECTION('',(1.05842257525004E-48,1.72718866511696E-48,1.));
#42803=DIRECTION('center_axis',(1.05842257525004E-48,1.72718866511696E-48,
1.));
#42804=DIRECTION('ref_axis',(0.891006524188331,0.453990499739619,-1.72718866511705E-48));
#42805=DIRECTION('',(1.05842257525004E-48,1.72718866511696E-48,1.));
#42806=DIRECTION('center_axis',(0.778521169386285,-0.627618346463367,2.6001091304247E-49));
#42807=DIRECTION('ref_axis',(0.627618346463367,0.778521169386285,-2.38387219843189E-65));
#42808=DIRECTION('center_axis',(0.0283643192709005,0.999597651754094,-1.67295152950556E-48));
#42809=DIRECTION('ref_axis',(-0.999597651754094,0.0283643192709005,5.71503284305285E-66));
#42810=DIRECTION('',(1.09747227149896E-48,1.6424833258909E-48,1.));
#42811=DIRECTION('center_axis',(1.09747227149896E-48,1.6424833258909E-48,
1.));
#42812=DIRECTION('ref_axis',(4.33680868994202E-19,-1.,1.6424833258909E-48));
#42813=DIRECTION('',(1.09747227149896E-48,1.6424833258909E-48,1.));
#42814=DIRECTION('center_axis',(0.726878880513651,-0.686765675513287,3.30271754722842E-49));
#42815=DIRECTION('ref_axis',(0.686765675513287,0.726878880513651,-2.02185804836064E-65));
#42816=DIRECTION('center_axis',(0.106704409389004,0.994290786951656,-1.66664752907659E-48));
#42817=DIRECTION('ref_axis',(-0.994290786951656,0.106704409389004,-7.60908949083185E-66));
#42818=DIRECTION('',(1.12975568624752E-48,1.55497530110057E-48,1.));
#42819=DIRECTION('center_axis',(1.12975568624752E-48,1.55497530110057E-48,
1.));
#42820=DIRECTION('ref_axis',(4.33680868994202E-19,-1.,1.55497530110057E-48));
#42821=DIRECTION('',(1.12975568624752E-48,1.55497530110057E-48,1.));
#42822=DIRECTION('center_axis',(0.670755141630895,-0.741678865800906,3.95502882331431E-49));
#42823=DIRECTION('ref_axis',(0.741678865800906,0.670755141630895,-5.99583083400171E-67));
#42824=DIRECTION('center_axis',(0.184386631340409,0.982853788812424,-1.65306157129173E-48));
#42825=DIRECTION('ref_axis',(-0.982853788812424,0.184386631340409,2.90870213757036E-65));
#42826=DIRECTION('',(1.15507378150848E-48,1.46520410681816E-48,1.));
#42827=DIRECTION('center_axis',(1.15507378150848E-48,1.46520410681816E-48,
1.));
#42828=DIRECTION('ref_axis',(4.33680868994202E-19,-1.,1.46520410681816E-48));
#42829=DIRECTION('',(1.15507378150848E-48,1.46520410681816E-48,1.));
#42830=DIRECTION('center_axis',(0.610495974251266,-0.792019359247612,4.5530212427498E-49));
#42831=DIRECTION('ref_axis',(0.792019359247612,0.610495974251266,2.91962028883906E-65));
#42832=DIRECTION('center_axis',(0.260932048394823,0.965357170233112,-1.63227741809852E-48));
#42833=DIRECTION('ref_axis',(-0.965357170233112,0.260932048394823,3.06323067308603E-65));
#42834=DIRECTION('',(1.17327046280543E-48,1.37372321230838E-48,1.));
#42835=DIRECTION('center_axis',(1.17327046280543E-48,1.37372321230838E-48,
1.));
#42836=DIRECTION('ref_axis',(4.33680868994202E-19,-1.,1.37372321230838E-48));
#42837=DIRECTION('',(1.17327046280543E-48,1.37372321230838E-48,1.));
#42838=DIRECTION('center_axis',(0.546472896179865,-0.837476789971394,5.0930079834164E-49));
#42839=DIRECTION('ref_axis',(0.837476789971394,0.546472896179865,-4.56422939014991E-65));
#42840=DIRECTION('center_axis',(0.335868732602171,0.94190880368548,-1.60442321071282E-48));
#42841=DIRECTION('ref_axis',(-0.94190880368548,0.335868732602171,4.87630450545203E-65));
#42842=DIRECTION('',(1.18423354154716E-48,1.28109662770635E-48,1.));
#42843=DIRECTION('center_axis',(1.18423354154716E-48,1.28109662770635E-48,
1.));
#42844=DIRECTION('ref_axis',(4.33680868994202E-19,-1.,1.28109662770635E-48));
#42845=DIRECTION('',(1.18423354154716E-48,1.28109662770635E-48,1.));
#42846=DIRECTION('center_axis',(0.479080630982838,-0.87777089779571,5.57165984749409E-49));
#42847=DIRECTION('ref_axis',(0.87777089779571,0.479080630982838,-3.73128804317402E-67));
#42848=DIRECTION('center_axis',(0.408734674385341,0.912653256146664,-1.56967067958563E-48));
#42849=DIRECTION('ref_axis',(-0.912653256146664,0.408734674385341,1.45818743306131E-64));
#42850=DIRECTION('center_axis',(0.408734674385325,-0.912653256146672,5.98602578707294E-49));
#42851=DIRECTION('ref_axis',(0.912653256146672,0.408734674385325,1.90174553100142E-65));
#42852=DIRECTION('center_axis',(0.479080630982853,0.877770897795701,-1.52823408562775E-48));
#42853=DIRECTION('ref_axis',(-0.877770897795701,0.479080630982853,5.61428358120402E-65));
#42854=DIRECTION('center_axis',(0.335868732602155,-0.941908803685485,6.33355109834479E-49));
#42855=DIRECTION('ref_axis',(0.941908803685485,0.335868732602155,-2.18452554190007E-64));
#42856=DIRECTION('center_axis',(0.54647289617988,0.837476789971384,-1.48036889921998E-48));
#42857=DIRECTION('ref_axis',(-0.837476789971384,0.54647289617988,1.0038841655118E-64));
#42858=DIRECTION('center_axis',(0.260932048394805,-0.965357170233117,6.61209317220175E-49));
#42859=DIRECTION('ref_axis',(0.965357170233117,0.260932048394805,-1.34731391844263E-65));
#42860=DIRECTION('center_axis',(0.61049597425128,0.792019359247601,-1.42637022515332E-48));
#42861=DIRECTION('ref_axis',(-0.792019359247601,0.61049597425128,4.68595517840464E-65));
#42862=DIRECTION('center_axis',(0.184386631340391,-0.982853788812427,6.81993470413385E-49));
#42863=DIRECTION('ref_axis',(0.982853788812427,0.184386631340391,-4.82159387328582E-66));
#42864=DIRECTION('center_axis',(0.670755141630908,0.741678865800894,-1.36657098320977E-48));
#42865=DIRECTION('ref_axis',(-0.741678865800894,0.670755141630908,-1.20021806126158E-65));
#42866=DIRECTION('center_axis',(0.106704409388986,-0.994290786951658,6.95579428198241E-49));
#42867=DIRECTION('ref_axis',(0.994290786951658,0.106704409388986,-5.2899598259714E-66));
#42868=DIRECTION('center_axis',(0.726878880513664,0.686765675513273,-1.30133985560118E-48));
#42869=DIRECTION('ref_axis',(-0.686765675513273,0.726878880513664,8.56568901676031E-65));
#42870=DIRECTION('center_axis',(0.0283643192708817,-0.999597651754094,7.01883428627211E-49));
#42871=DIRECTION('ref_axis',(0.999597651754094,0.0283643192708817,4.29698701010715E-68));
#42872=DIRECTION('axis',(0.,0.,1.));
#42873=DIRECTION('refdir',(1.,0.,0.));
#42874=DIRECTION('center_axis',(5.15167520928809E-67,-1.18789542670764E-48,
-1.));
#42875=DIRECTION('ref_axis',(-4.33680868994202E-19,1.,-1.18789542670764E-48));
#42876=DIRECTION('',(-5.15167520928809E-67,1.18789542670764E-48,1.));
#42877=DIRECTION('',(-5.15167520928809E-67,1.18789542670764E-48,1.));
#42878=DIRECTION('center_axis',(5.15167520928809E-67,-1.18789542670764E-48,
-1.));
#42879=DIRECTION('ref_axis',(-4.33680868994202E-19,1.,-1.18789542670764E-48));
#42880=DIRECTION('center_axis',(-4.70261923768679E-35,1.08435016942139E-16,
-1.));
#42881=DIRECTION('ref_axis',(-4.33680868994202E-19,1.,1.08435016942139E-16));
#42882=DIRECTION('center_axis',(5.15167520928809E-67,-1.18789542670764E-48,
-1.));
#42883=DIRECTION('ref_axis',(-4.33680868994202E-19,1.,-1.18789542670764E-48));
#42884=DIRECTION('',(-5.15167520928809E-67,1.18789542670764E-48,1.));
#42885=DIRECTION('center_axis',(5.15167520928809E-67,-1.18789542670764E-48,
-1.));
#42886=DIRECTION('ref_axis',(-4.33680868994202E-19,1.,-1.18789542670764E-48));
#42887=DIRECTION('',(-5.15167520928809E-67,1.18789542670764E-48,1.));
#42888=DIRECTION('center_axis',(5.15167520928809E-67,-1.18789542670764E-48,
-1.));
#42889=DIRECTION('ref_axis',(-4.33680868994202E-19,1.,-1.18789542670764E-48));
#42890=DIRECTION('',(-5.15167520928809E-67,1.18789542670764E-48,1.));
#42891=DIRECTION('center_axis',(5.15167520928809E-67,-1.18789542670764E-48,
-1.));
#42892=DIRECTION('ref_axis',(-4.33680868994202E-19,1.,-1.18789542670764E-48));
#42893=DIRECTION('',(-5.15167520928809E-67,1.18789542670764E-48,1.));
#42894=DIRECTION('center_axis',(5.15167520928809E-67,-1.18789542670764E-48,
-1.));
#42895=DIRECTION('ref_axis',(-4.33680868994202E-19,1.,-1.18789542670764E-48));
#42896=DIRECTION('',(-5.15167520928809E-67,1.18789542670764E-48,1.));
#42897=DIRECTION('center_axis',(5.15167520928809E-67,-1.18789542670764E-48,
-1.));
#42898=DIRECTION('ref_axis',(-4.33680868994202E-19,1.,-1.18789542670764E-48));
#42899=DIRECTION('',(-5.15167520928809E-67,1.18789542670764E-48,1.));
#42900=DIRECTION('center_axis',(5.15167520928809E-67,-1.18789542670764E-48,
-1.));
#42901=DIRECTION('ref_axis',(-4.33680868994202E-19,1.,-1.18789542670764E-48));
#42902=DIRECTION('',(-5.15167520928809E-67,1.18789542670764E-48,1.));
#42903=DIRECTION('center_axis',(5.15167520928809E-67,-1.18789542670764E-48,
-1.));
#42904=DIRECTION('ref_axis',(-4.33680868994202E-19,1.,-1.18789542670764E-48));
#42905=DIRECTION('',(-5.15167520928809E-67,1.18789542670764E-48,1.));
#42906=DIRECTION('center_axis',(5.15167520928809E-67,-1.18789542670764E-48,
-1.));
#42907=DIRECTION('ref_axis',(-4.33680868994202E-19,1.,-1.18789542670764E-48));
#42908=DIRECTION('',(-5.15167520928809E-67,1.18789542670764E-48,1.));
#42909=DIRECTION('center_axis',(5.15167520928809E-67,-1.18789542670764E-48,
-1.));
#42910=DIRECTION('ref_axis',(-4.33680868994202E-19,1.,-1.18789542670764E-48));
#42911=DIRECTION('',(-5.15167520928809E-67,1.18789542670764E-48,1.));
#42912=DIRECTION('center_axis',(5.15167520928809E-67,-1.18789542670764E-48,
-1.));
#42913=DIRECTION('ref_axis',(-4.33680868994202E-19,1.,-1.18789542670764E-48));
#42914=DIRECTION('',(-5.15167520928809E-67,1.18789542670764E-48,1.));
#42915=DIRECTION('center_axis',(5.15167520928809E-67,-1.18789542670764E-48,
-1.));
#42916=DIRECTION('ref_axis',(-4.33680868994202E-19,1.,-1.18789542670764E-48));
#42917=DIRECTION('',(-5.15167520928809E-67,1.18789542670764E-48,1.));
#42918=DIRECTION('center_axis',(5.15167520928809E-67,-1.18789542670764E-48,
-1.));
#42919=DIRECTION('ref_axis',(-4.33680868994202E-19,1.,-1.18789542670764E-48));
#42920=DIRECTION('',(-5.15167520928809E-67,1.18789542670764E-48,1.));
#42921=DIRECTION('center_axis',(5.15167520928809E-67,-1.18789542670764E-48,
-1.));
#42922=DIRECTION('ref_axis',(-4.33680868994202E-19,1.,-1.18789542670764E-48));
#42923=DIRECTION('',(-5.15167520928809E-67,1.18789542670764E-48,1.));
#42924=DIRECTION('center_axis',(5.15167520928809E-67,-1.18789542670764E-48,
-1.));
#42925=DIRECTION('ref_axis',(-4.33680868994202E-19,1.,-1.18789542670764E-48));
#42926=DIRECTION('',(-5.15167520928809E-67,1.18789542670764E-48,1.));
#42927=DIRECTION('center_axis',(5.15167520928809E-67,-1.18789542670764E-48,
-1.));
#42928=DIRECTION('ref_axis',(-4.33680868994202E-19,1.,-1.18789542670764E-48));
#42929=DIRECTION('',(-5.15167520928809E-67,1.18789542670764E-48,1.));
#42930=DIRECTION('center_axis',(5.15167520928809E-67,-1.18789542670764E-48,
-1.));
#42931=DIRECTION('ref_axis',(-4.33680868994202E-19,1.,-1.18789542670764E-48));
#42932=DIRECTION('',(-5.15167520928809E-67,1.18789542670764E-48,1.));
#42933=DIRECTION('center_axis',(5.15167520928809E-67,-1.18789542670764E-48,
-1.));
#42934=DIRECTION('ref_axis',(-4.33680868994202E-19,1.,-1.18789542670764E-48));
#42935=DIRECTION('',(-5.15167520928809E-67,1.18789542670764E-48,1.));
#42936=DIRECTION('center_axis',(5.15167520928809E-67,-1.18789542670764E-48,
-1.));
#42937=DIRECTION('ref_axis',(-4.33680868994202E-19,1.,-1.18789542670764E-48));
#42938=DIRECTION('',(-5.15167520928809E-67,1.18789542670764E-48,1.));
#42939=DIRECTION('center_axis',(5.15167520928809E-67,-1.18789542670764E-48,
-1.));
#42940=DIRECTION('ref_axis',(-4.33680868994202E-19,1.,-1.18789542670764E-48));
#42941=DIRECTION('',(-5.15167520928809E-67,1.18789542670764E-48,1.));
#42942=DIRECTION('center_axis',(5.15167520928809E-67,-1.18789542670764E-48,
-1.));
#42943=DIRECTION('ref_axis',(-4.33680868994202E-19,1.,-1.18789542670764E-48));
#42944=DIRECTION('',(-5.15167520928809E-67,1.18789542670764E-48,1.));
#42945=DIRECTION('center_axis',(5.15167520928809E-67,-1.18789542670764E-48,
-1.));
#42946=DIRECTION('ref_axis',(-4.33680868994202E-19,1.,-1.18789542670764E-48));
#42947=DIRECTION('',(-5.15167520928809E-67,1.18789542670764E-48,1.));
#42948=DIRECTION('center_axis',(5.15167520928809E-67,-1.18789542670764E-48,
-1.));
#42949=DIRECTION('ref_axis',(-4.33680868994202E-19,1.,-1.18789542670764E-48));
#42950=DIRECTION('',(-5.15167520928809E-67,1.18789542670764E-48,1.));
#42951=DIRECTION('center_axis',(5.15167520928809E-67,-1.18789542670764E-48,
-1.));
#42952=DIRECTION('ref_axis',(-4.33680868994202E-19,1.,-1.18789542670764E-48));
#42953=DIRECTION('',(-5.15167520928809E-67,1.18789542670764E-48,1.));
#42954=DIRECTION('center_axis',(5.15167520928809E-67,-1.18789542670764E-48,
-1.));
#42955=DIRECTION('ref_axis',(-4.33680868994202E-19,1.,-1.18789542670764E-48));
#42956=DIRECTION('',(-5.15167520928809E-67,1.18789542670764E-48,1.));
#42957=DIRECTION('center_axis',(5.15167520928809E-67,-1.18789542670764E-48,
-1.));
#42958=DIRECTION('ref_axis',(-4.33680868994202E-19,1.,-1.18789542670764E-48));
#42959=DIRECTION('',(-5.15167520928809E-67,1.18789542670764E-48,1.));
#42960=DIRECTION('center_axis',(5.15167520928809E-67,-1.18789542670764E-48,
-1.));
#42961=DIRECTION('ref_axis',(-4.33680868994202E-19,1.,-1.18789542670764E-48));
#42962=DIRECTION('',(-5.15167520928809E-67,1.18789542670764E-48,1.));
#42963=DIRECTION('center_axis',(-5.15167520928809E-67,1.18789542670764E-48,
1.));
#42964=DIRECTION('ref_axis',(4.33680868994202E-19,-1.,1.18789542670764E-48));
#42965=DIRECTION('',(8.69022643068855E-17,-0.707106781186544,-0.707106781186551));
#42966=DIRECTION('center_axis',(5.15167520928809E-67,-1.18789542670764E-48,
-1.));
#42967=DIRECTION('ref_axis',(-4.33680868994202E-19,1.,-1.18789542670764E-48));
#42968=DIRECTION('center_axis',(0.,0.,1.));
#42969=DIRECTION('ref_axis',(5.30947313395831E-16,1.,0.));
#42970=DIRECTION('',(0.,0.,-1.));
#42971=DIRECTION('center_axis',(5.15167520928809E-67,-1.18789542670764E-48,
-1.));
#42972=DIRECTION('ref_axis',(-4.33680868994202E-19,1.,-1.18789542670764E-48));
#42973=DIRECTION('center_axis',(0.,0.,1.));
#42974=DIRECTION('ref_axis',(5.30947313395831E-16,1.,0.));
#42975=DIRECTION('',(0.,0.,-1.));
#42976=DIRECTION('center_axis',(0.,0.,1.));
#42977=DIRECTION('ref_axis',(5.30947313395831E-16,1.,0.));
#42978=DIRECTION('',(0.,0.,-1.));
#42979=DIRECTION('center_axis',(0.,0.,1.));
#42980=DIRECTION('ref_axis',(5.30947313395831E-16,1.,0.));
#42981=DIRECTION('',(0.,0.,-1.));
#42982=DIRECTION('center_axis',(0.,0.,1.));
#42983=DIRECTION('ref_axis',(5.30947313395831E-16,1.,0.));
#42984=DIRECTION('',(0.,0.,-1.));
#42985=DIRECTION('center_axis',(0.,0.,1.));
#42986=DIRECTION('ref_axis',(5.30947313395831E-16,1.,0.));
#42987=DIRECTION('',(0.,0.,-1.));
#42988=DIRECTION('center_axis',(0.,0.,1.));
#42989=DIRECTION('ref_axis',(5.30947313395831E-16,1.,0.));
#42990=DIRECTION('',(0.,0.,-1.));
#42991=DIRECTION('center_axis',(0.,0.,1.));
#42992=DIRECTION('ref_axis',(5.30947313395831E-16,1.,0.));
#42993=DIRECTION('',(0.,0.,-1.));
#42994=DIRECTION('center_axis',(0.,0.,1.));
#42995=DIRECTION('ref_axis',(5.30947313395831E-16,1.,0.));
#42996=DIRECTION('',(0.,0.,-1.));
#42997=DIRECTION('center_axis',(0.,0.,1.));
#42998=DIRECTION('ref_axis',(5.30947313395831E-16,1.,0.));
#42999=DIRECTION('',(0.,0.,-1.));
#43000=DIRECTION('center_axis',(0.,0.,1.));
#43001=DIRECTION('ref_axis',(5.30947313395831E-16,1.,0.));
#43002=DIRECTION('',(0.,0.,-1.));
#43003=DIRECTION('center_axis',(0.,0.,1.));
#43004=DIRECTION('ref_axis',(5.30947313395831E-16,1.,0.));
#43005=DIRECTION('',(0.,0.,-1.));
#43006=DIRECTION('center_axis',(0.,0.,1.));
#43007=DIRECTION('ref_axis',(5.30947313395831E-16,1.,0.));
#43008=DIRECTION('',(0.,0.,-1.));
#43009=DIRECTION('center_axis',(0.,0.,1.));
#43010=DIRECTION('ref_axis',(5.30947313395831E-16,1.,0.));
#43011=DIRECTION('',(0.,0.,-1.));
#43012=DIRECTION('center_axis',(0.,0.,1.));
#43013=DIRECTION('ref_axis',(5.30947313395831E-16,1.,0.));
#43014=DIRECTION('',(0.,0.,-1.));
#43015=DIRECTION('center_axis',(0.,0.,1.));
#43016=DIRECTION('ref_axis',(5.30947313395831E-16,1.,0.));
#43017=DIRECTION('',(0.,0.,-1.));
#43018=DIRECTION('center_axis',(0.,0.,1.));
#43019=DIRECTION('ref_axis',(5.30947313395831E-16,1.,0.));
#43020=DIRECTION('',(0.,0.,-1.));
#43021=DIRECTION('center_axis',(0.,0.,1.));
#43022=DIRECTION('ref_axis',(5.30947313395831E-16,1.,0.));
#43023=DIRECTION('',(0.,0.,-1.));
#43024=DIRECTION('center_axis',(0.,0.,1.));
#43025=DIRECTION('ref_axis',(5.30947313395831E-16,1.,0.));
#43026=DIRECTION('',(0.,0.,-1.));
#43027=DIRECTION('center_axis',(0.,0.,1.));
#43028=DIRECTION('ref_axis',(5.30947313395831E-16,1.,0.));
#43029=DIRECTION('',(0.,0.,-1.));
#43030=DIRECTION('center_axis',(0.,0.,1.));
#43031=DIRECTION('ref_axis',(5.30947313395831E-16,1.,0.));
#43032=DIRECTION('',(0.,0.,-1.));
#43033=DIRECTION('center_axis',(0.,0.,1.));
#43034=DIRECTION('ref_axis',(5.30947313395831E-16,1.,0.));
#43035=DIRECTION('',(0.,0.,-1.));
#43036=DIRECTION('center_axis',(0.,0.,1.));
#43037=DIRECTION('ref_axis',(5.30947313395831E-16,1.,0.));
#43038=DIRECTION('',(0.,0.,-1.));
#43039=DIRECTION('center_axis',(0.,0.,1.));
#43040=DIRECTION('ref_axis',(5.30947313395831E-16,1.,0.));
#43041=DIRECTION('',(0.,0.,-1.));
#43042=DIRECTION('center_axis',(0.,0.,1.));
#43043=DIRECTION('ref_axis',(5.30947313395831E-16,1.,0.));
#43044=DIRECTION('',(0.,0.,-1.));
#43045=DIRECTION('center_axis',(0.,0.,1.));
#43046=DIRECTION('ref_axis',(5.30947313395831E-16,1.,0.));
#43047=DIRECTION('',(0.,0.,-1.));
#43048=DIRECTION('center_axis',(0.,0.,1.));
#43049=DIRECTION('ref_axis',(5.30947313395831E-16,1.,0.));
#43050=DIRECTION('',(0.,0.,-1.));
#43051=DIRECTION('center_axis',(0.,0.,1.));
#43052=DIRECTION('ref_axis',(5.30947313395831E-16,1.,0.));
#43053=DIRECTION('',(0.,0.,-1.));
#43054=DIRECTION('center_axis',(0.,0.,1.));
#43055=DIRECTION('ref_axis',(5.30947313395831E-16,1.,0.));
#43056=DIRECTION('',(0.,0.,-1.));
#43057=DIRECTION('center_axis',(0.,0.,1.));
#43058=DIRECTION('ref_axis',(5.30947313395831E-16,1.,0.));
#43059=DIRECTION('',(0.,0.,-1.));
#43060=DIRECTION('center_axis',(0.,0.,1.));
#43061=DIRECTION('ref_axis',(5.30947313395831E-16,1.,0.));
#43062=DIRECTION('center_axis',(0.,0.,1.));
#43063=DIRECTION('ref_axis',(0.700629269222058,-0.7135254915624,0.));
#43064=DIRECTION('center_axis',(-5.15167520928809E-67,1.18789542670764E-48,
1.));
#43065=DIRECTION('ref_axis',(4.33680868994202E-19,-1.,1.18789542670764E-48));
#43066=DIRECTION('center_axis',(5.15167520928809E-67,-1.18789542670764E-48,
-1.));
#43067=DIRECTION('ref_axis',(-4.33680868994202E-19,1.,-1.18789542670764E-48));
#43068=DIRECTION('center_axis',(5.15167520928809E-67,-1.18789542670764E-48,
-1.));
#43069=DIRECTION('ref_axis',(-4.33680868994202E-19,1.,-1.18789542670764E-48));
#43070=DIRECTION('center_axis',(5.15167520928809E-67,-1.18789542670764E-48,
-1.));
#43071=DIRECTION('ref_axis',(-4.33680868994202E-19,1.,-1.18789542670764E-48));
#43072=DIRECTION('center_axis',(1.09747227149895E-48,7.33307527524356E-49,
1.));
#43073=DIRECTION('ref_axis',(1.,4.33680868994202E-19,-1.09747227149895E-48));
#43074=DIRECTION('center_axis',(-0.654448706060852,0.271081529927754,-0.705841126081008));
#43075=DIRECTION('ref_axis',(0.652112169591586,-0.270113704831613,-0.708370174931649));
#43076=DIRECTION('',(1.09747227149895E-48,7.33307527524356E-49,1.));
#43077=DIRECTION('center_axis',(-0.654448706060939,0.271081529927973,0.705841126080843));
#43078=DIRECTION('ref_axis',(0.652112169592024,-0.270113704830126,0.708370174931813));
#43079=DIRECTION('',(1.09747227149895E-48,7.33307527524356E-49,1.));
#43080=DIRECTION('center_axis',(1.12975568624751E-48,8.20815552314688E-49,
1.));
#43081=DIRECTION('ref_axis',(1.,4.33680868994202E-19,-1.12975568624751E-48));
#43082=DIRECTION('center_axis',(-0.673700070814156,0.218898422362917,-0.705841126084352));
#43083=DIRECTION('ref_axis',(0.671294802430975,-0.218116903290839,-0.708370174928316));
#43084=DIRECTION('',(1.12975568624751E-48,8.20815552314688E-49,1.));
#43085=DIRECTION('center_axis',(-0.673700070814201,0.218898422363249,0.705841126084207));
#43086=DIRECTION('ref_axis',(0.671294802430673,-0.218116903291296,0.708370174928462));
#43087=DIRECTION('',(1.12975568624751E-48,8.20815552314688E-49,1.));
#43088=DIRECTION('center_axis',(1.15507378150847E-48,9.10586746597098E-49,
1.));
#43089=DIRECTION('ref_axis',(1.,4.33680868994202E-19,-1.15507378150847E-48));
#43090=DIRECTION('center_axis',(-0.688797850611722,0.165365733230951,-0.705841126079843));
#43091=DIRECTION('ref_axis',(0.686338679579581,-0.164775338502517,-0.708370174932809));
#43092=DIRECTION('',(1.15507378150847E-48,9.10586746597098E-49,1.));
#43093=DIRECTION('center_axis',(-0.688797850609436,0.165365733233163,0.705841126081556));
#43094=DIRECTION('ref_axis',(0.68633867958204,-0.164775338499612,0.708370174931102));
#43095=DIRECTION('',(1.15507378150847E-48,9.10586746597098E-49,1.));
#43096=DIRECTION('center_axis',(1.17327046280542E-48,1.00206764110688E-48,
1.));
#43097=DIRECTION('ref_axis',(1.,4.33680868994202E-19,-1.17327046280542E-48));
#43098=DIRECTION('center_axis',(-0.699648962604041,0.110813509366852,-0.705841126082132));
#43099=DIRECTION('ref_axis',(0.697151050543932,-0.11041787896162,-0.708370174930529));
#43100=DIRECTION('',(1.17327046280542E-48,1.00206764110688E-48,1.));
#43101=DIRECTION('center_axis',(-0.699648962604175,0.110813509367011,0.705841126081974));
#43102=DIRECTION('ref_axis',(0.697151050543496,-0.110417878963368,0.708370174930686));
#43103=DIRECTION('',(1.17327046280542E-48,1.00206764110688E-48,1.));
#43104=DIRECTION('center_axis',(1.18423354154716E-48,1.09469422570891E-48,
1.));
#43105=DIRECTION('ref_axis',(1.,4.33680868994202E-19,-1.18423354154716E-48));
#43106=DIRECTION('center_axis',(-0.706186506088737,0.0555780833649064,-0.705841126081264));
#43107=DIRECTION('ref_axis',(0.703665253451942,-0.0553796564821394,-0.708370174931394));
#43108=DIRECTION('',(1.18423354154716E-48,1.09469422570891E-48,1.));
#43109=DIRECTION('center_axis',(-0.706186506088284,0.0555780833648712,0.705841126081719));
#43110=DIRECTION('ref_axis',(0.703665253452317,-0.0553796564831855,0.70837017493094));
#43111=DIRECTION('',(1.18423354154716E-48,1.09469422570891E-48,1.));
#43112=DIRECTION('center_axis',(1.18789542670764E-48,1.18789542670763E-48,
1.));
#43113=DIRECTION('ref_axis',(1.,4.33680868994202E-19,-1.18789542670764E-48));
#43114=DIRECTION('center_axis',(-0.70837017493089,-1.25340662871076E-13,
-0.70584112608177));
#43115=DIRECTION('ref_axis',(0.70584112608177,-2.88506822019813E-13,-0.708370174930889));
#43116=DIRECTION('',(1.18789542670764E-48,1.18789542670763E-48,1.));
#43117=DIRECTION('center_axis',(-0.70837017493089,1.25340662871076E-13,
0.70584112608177));
#43118=DIRECTION('ref_axis',(0.70584112608177,2.61497947465894E-13,0.708370174930889));
#43119=DIRECTION('',(1.18789542670764E-48,1.18789542670763E-48,1.));
#43120=DIRECTION('center_axis',(1.05842257525003E-48,6.48602188298306E-49,
1.));
#43121=DIRECTION('ref_axis',(1.,4.33680868994202E-19,-1.05842257525003E-48));
#43122=DIRECTION('center_axis',(-0.631162447404585,0.321593329715507,-0.70584112608203));
#43123=DIRECTION('ref_axis',(0.628909048379288,-0.320445165567225,-0.708370174930631));
#43124=DIRECTION('',(1.05842257525003E-48,6.48602188298306E-49,1.));
#43125=DIRECTION('center_axis',(-0.631162447404969,0.32159332971786,0.705841126080614));
#43126=DIRECTION('ref_axis',(0.628909048378923,-0.320445165564824,0.708370174932041));
#43127=DIRECTION('',(1.05842257525003E-48,6.48602188298306E-49,1.));
#43128=DIRECTION('center_axis',(1.01284735186347E-48,5.67221771220248E-49,
1.));
#43129=DIRECTION('ref_axis',(1.,4.33680868994202E-19,-1.01284735186347E-48));
#43130=DIRECTION('center_axis',(-0.603984862377595,0.370122399687911,-0.705841126081486));
#43131=DIRECTION('ref_axis',(0.601828493750374,-0.368800975294447,-0.708370174931173));
#43132=DIRECTION('',(1.01284735186347E-48,5.67221771220248E-49,1.));
#43133=DIRECTION('center_axis',(-0.603984862377492,0.370122399687834,0.705841126081615));
#43134=DIRECTION('ref_axis',(0.60182849375054,-0.368800975294424,0.708370174931044));
#43135=DIRECTION('',(1.01284735186347E-48,5.67221771220248E-49,1.));
#43136=DIRECTION('center_axis',(9.61027587746754E-49,4.89668013623204E-49,
1.));
#43137=DIRECTION('ref_axis',(1.,4.33680868994202E-19,-9.61027587746754E-49));
#43138=DIRECTION('center_axis',(-0.57308350982942,0.416369541987989,-0.705841126080299));
#43139=DIRECTION('ref_axis',(-0.571037466327478,0.414883004371834,0.708370174932355));
#43140=DIRECTION('',(9.61027587746754E-49,4.89668013623204E-49,1.));
#43141=DIRECTION('center_axis',(-0.573083509826005,0.416369541988967,0.705841126082495));
#43142=DIRECTION('ref_axis',(0.571037466331126,-0.41488300437055,0.708370174930167));
#43143=DIRECTION('',(9.61027587746754E-49,4.89668013623204E-49,1.));
#43144=DIRECTION('center_axis',(9.03282768977476E-49,4.16419060212002E-49,
1.));
#43145=DIRECTION('ref_axis',(1.,4.33680868994202E-19,-9.03282768977476E-49));
#43146=DIRECTION('center_axis',(-0.538648906869708,0.460049627603881,-0.705841126082633));
#43147=DIRECTION('ref_axis',(-0.536725803041031,0.458407141763258,0.70837017493003));
#43148=DIRECTION('',(9.03282768977476E-49,4.16419060212002E-49,1.));
#43149=DIRECTION('center_axis',(-0.53864890686968,0.460049627604191,0.705841126082452));
#43150=DIRECTION('ref_axis',(0.536725803040381,-0.45840714176374,0.70837017493021));
#43151=DIRECTION('',(9.03282768977476E-49,4.16419060212002E-49,1.));
#43152=DIRECTION('center_axis',(8.39968911565451E-49,3.47926515142171E-49,
1.));
#43153=DIRECTION('ref_axis',(1.,4.33680868994202E-19,-8.39968911565451E-49));
#43154=DIRECTION('center_axis',(-0.500893354284786,0.500893354283015,-0.705841126081816));
#43155=DIRECTION('ref_axis',(-0.499105046691526,0.499105046694076,0.708370174930843));
#43156=DIRECTION('',(8.39968911565451E-49,3.47926515142171E-49,1.));
#43157=DIRECTION('center_axis',(-0.500893354285066,0.500893354283687,0.70584112608114));
#43158=DIRECTION('ref_axis',(0.49910504669045,-0.499105046694196,0.708370174931517));
#43159=DIRECTION('',(8.39968911565451E-49,3.47926515142171E-49,1.));
#43160=DIRECTION('center_axis',(7.71476366495618E-49,2.84612657730147E-49,
1.));
#43161=DIRECTION('ref_axis',(1.,4.33680868994202E-19,-7.71476366495618E-49));
#43162=DIRECTION('center_axis',(-0.460049627606723,0.538648906869542,-0.705841126080907));
#43163=DIRECTION('ref_axis',(-0.458407141764148,0.536725803038001,0.708370174931749));
#43164=DIRECTION('',(7.71476366495618E-49,2.84612657730147E-49,1.));
#43165=DIRECTION('center_axis',(-0.460049627603276,0.538648906871872,0.705841126081376));
#43166=DIRECTION('ref_axis',(0.458407141768044,-0.53672580303529,0.708370174931282));
#43167=DIRECTION('',(7.71476366495618E-49,2.84612657730147E-49,1.));
#43168=DIRECTION('center_axis',(6.98227413084414E-49,2.26867838960871E-49,
1.));
#43169=DIRECTION('ref_axis',(1.,4.33680868994202E-19,-6.98227413084414E-49));
#43170=DIRECTION('center_axis',(-0.416369541989573,0.573083509826983,-0.705841126081344));
#43171=DIRECTION('ref_axis',(-0.414883004369422,0.571037466330522,0.708370174931314));
#43172=DIRECTION('',(6.98227413084414E-49,2.26867838960871E-49,1.));
#43173=DIRECTION('center_axis',(-0.416369541986537,0.573083509827722,0.705841126082535));
#43174=DIRECTION('ref_axis',(0.414883004374377,-0.571037466328393,0.708370174930127));
#43175=DIRECTION('',(6.98227413084414E-49,2.26867838960871E-49,1.));
#43176=DIRECTION('center_axis',(6.2067365548737E-49,1.75048074844156E-49,
1.));
#43177=DIRECTION('ref_axis',(1.,4.33680868994202E-19,-6.2067365548737E-49));
#43178=DIRECTION('center_axis',(-0.370122399687787,0.603984862376041,-0.70584112608288));
#43179=DIRECTION('ref_axis',(-0.368800975294937,0.60182849375171,0.708370174929783));
#43180=DIRECTION('',(6.2067365548737E-49,1.75048074844156E-49,1.));
#43181=DIRECTION('center_axis',(-0.370122399687792,0.603984862376936,0.705841126082112));
#43182=DIRECTION('ref_axis',(0.368800975294942,-0.601828493750806,0.708370174930549));
#43183=DIRECTION('',(6.2067365548737E-49,1.75048074844156E-49,1.));
#43184=DIRECTION('center_axis',(5.39293238409311E-49,1.29472851457601E-49,
1.));
#43185=DIRECTION('ref_axis',(1.,4.33680868994202E-19,-5.39293238409311E-49));
#43186=DIRECTION('center_axis',(-0.321593329717153,0.63116244740346,-0.705841126082286));
#43187=DIRECTION('ref_axis',(-0.320445165567263,0.628909048379556,0.708370174930376));
#43188=DIRECTION('',(5.39293238409311E-49,1.29472851457601E-49,1.));
#43189=DIRECTION('center_axis',(-0.321593329716558,0.631162447403966,0.705841126082104));
#43190=DIRECTION('ref_axis',(0.320445165566995,-0.628909048379489,0.708370174930556));
#43191=DIRECTION('',(5.39293238409311E-49,1.29472851457601E-49,1.));
#43192=DIRECTION('center_axis',(0.,0.,1.));
#43193=DIRECTION('ref_axis',(1.,4.33680868994202E-19,0.));
#43194=DIRECTION('',(-0.707106781186549,-8.69022643068862E-17,0.707106781186546));
#43195=DIRECTION('center_axis',(0.,0.,1.));
#43196=DIRECTION('ref_axis',(1.,4.33680868994202E-19,0.));
#43197=DIRECTION('center_axis',(5.15167520928809E-67,-1.18789542670764E-48,
-1.));
#43198=DIRECTION('ref_axis',(0.,1.,0.));
#43199=DIRECTION('center_axis',(5.15167520928809E-67,-1.18789542670764E-48,
-1.));
#43200=DIRECTION('ref_axis',(-4.33680868994202E-19,1.,-1.18789542670764E-48));
#43201=DIRECTION('center_axis',(-1.,0.,-5.15167520928809E-67));
#43202=DIRECTION('ref_axis',(0.,-1.,0.));
#43203=DIRECTION('center_axis',(5.15167520928809E-67,-1.18789542670764E-48,
-1.));
#43204=DIRECTION('ref_axis',(-4.33680868994202E-19,1.,-1.18789542670764E-48));
#43205=DIRECTION('center_axis',(5.15167520928809E-67,-1.18789542670764E-48,
-1.));
#43206=DIRECTION('ref_axis',(-4.33680868994202E-19,1.,-1.18789542670764E-48));
#43207=DIRECTION('center_axis',(5.15167520928809E-67,-1.18789542670764E-48,
-1.));
#43208=DIRECTION('ref_axis',(-4.33680868994202E-19,1.,-1.18789542670764E-48));
#43209=DIRECTION('center_axis',(0.0555758110363288,-0.706157633406642,0.705870190622316));
#43210=DIRECTION('ref_axis',(0.0553775799352608,-0.703694571287346,-0.708341212962532));
#43211=DIRECTION('center_axis',(5.15167520928809E-67,-1.18789542670764E-48,
-1.));
#43212=DIRECTION('ref_axis',(-4.33680868994202E-19,1.,-1.18789542670764E-48));
#43213=DIRECTION('center_axis',(0.11080862020158,-0.699618093636883,0.705872490429338));
#43214=DIRECTION('ref_axis',(0.110419233095995,-0.697182591373234,-0.708338921173046));
#43215=DIRECTION('center_axis',(5.15167520928809E-67,-1.18789542670764E-48,
-1.));
#43216=DIRECTION('ref_axis',(-4.33680868994202E-19,1.,-1.18789542670764E-48));
#43217=DIRECTION('center_axis',(0.165358045050138,-0.688765827029971,0.705874176077378));
#43218=DIRECTION('ref_axis',(0.164780094681068,-0.686371526838389,-0.708337241391723));
#43219=DIRECTION('center_axis',(5.15167520928809E-67,-1.18789542670764E-48,
-1.));
#43220=DIRECTION('ref_axis',(-4.33680868994202E-19,1.,-1.18789542670764E-48));
#43221=DIRECTION('center_axis',(0.218887852522913,-0.673667540197498,0.705875451692549));
#43222=DIRECTION('ref_axis',(0.218125006053852,-0.671328261761447,-0.708335970210719));
#43223=DIRECTION('center_axis',(5.15167520928809E-67,-1.18789542670764E-48,
-1.));
#43224=DIRECTION('ref_axis',(-4.33680868994202E-19,1.,-1.18789542670764E-48));
#43225=DIRECTION('center_axis',(0.271068063822855,-0.654416196007407,0.705876439030603));
#43226=DIRECTION('ref_axis',(0.270125073931967,-0.65214568281518,-0.708334986301518));
#43227=DIRECTION('center_axis',(5.15167520928809E-67,-1.18789542670764E-48,
-1.));
#43228=DIRECTION('ref_axis',(-4.33680868994202E-19,1.,-1.18789542670764E-48));
#43229=DIRECTION('center_axis',(0.321577003370555,-0.631130405143931,0.705877214964523));
#43230=DIRECTION('ref_axis',(0.320459697262731,-0.628942147608601,-0.708334213060304));
#43231=DIRECTION('center_axis',(5.15167520928809E-67,-1.18789542670764E-48,
-1.));
#43232=DIRECTION('ref_axis',(-4.33680868994202E-19,1.,-1.18789542670764E-48));
#43233=DIRECTION('center_axis',(0.370103289326652,-0.603953677099404,0.705877830185721));
#43234=DIRECTION('ref_axis',(0.368818543504099,-0.601860775526205,-0.708333599972859));
#43235=DIRECTION('center_axis',(5.15167520928809E-67,-1.18789542670764E-48,
-1.));
#43236=DIRECTION('ref_axis',(-4.33680868994202E-19,1.,-1.18789542670764E-48));
#43237=DIRECTION('center_axis',(0.416347757295498,-0.573053525770462,0.705878319256975));
#43238=DIRECTION('ref_axis',(0.414903461782555,-0.571068576441932,-0.708333112597058));
#43239=DIRECTION('center_axis',(5.15167520928809E-67,-1.18789542670764E-48,
-1.));
#43240=DIRECTION('ref_axis',(-4.33680868994202E-19,1.,-1.18789542670764E-48));
#43241=DIRECTION('center_axis',(0.460025307051016,-0.538620431161506,0.705878706300177));
#43242=DIRECTION('ref_axis',(0.458430320957564,-0.536755427393206,-0.708332726895123));
#43243=DIRECTION('center_axis',(5.15167520928809E-67,-1.18789542670764E-48,
-1.));
#43244=DIRECTION('ref_axis',(-4.33680868994202E-19,1.,-1.18789542670764E-48));
#43245=DIRECTION('center_axis',(0.500866661619323,-0.500866661619323,0.705879008440277));
#43246=DIRECTION('ref_axis',(0.499130761357991,-0.499132905771573,-0.708332425801768));
#43247=DIRECTION('center_axis',(5.15167520928809E-67,-1.18789542670764E-48,
-1.));
#43248=DIRECTION('ref_axis',(-4.33680868994202E-19,1.,-1.18789542670764E-48));
#43249=DIRECTION('center_axis',(0.53862002836901,-0.46002496303376,0.705879237848482));
#43250=DIRECTION('ref_axis',(0.536753849182443,-0.458432987266868,-0.708332197188161));
#43251=DIRECTION('center_axis',(5.15167520928809E-67,-1.18789542670764E-48,
-1.));
#43252=DIRECTION('ref_axis',(-4.33680868994202E-19,1.,-1.18789542670764E-48));
#43253=DIRECTION('center_axis',(0.573052651970297,-0.416347122442612,0.705879403087785));
#43254=DIRECTION('ref_axis',(0.571067623542823,-0.414906617259439,-0.708332032521106));
#43255=DIRECTION('center_axis',(5.15167520928809E-67,-1.18789542670764E-48,
-1.));
#43256=DIRECTION('ref_axis',(-4.33680868994202E-19,1.,-1.18789542670764E-48));
#43257=DIRECTION('center_axis',(0.603952249837211,-0.370102414699222,0.705879509938047));
#43258=DIRECTION('ref_axis',(0.601860526500507,-0.368822164724135,-0.708331926040847));
#43259=DIRECTION('center_axis',(5.15167520928809E-67,-1.18789542670764E-48,
-1.));
#43260=DIRECTION('ref_axis',(-4.33680868994202E-19,1.,-1.18789542670764E-48));
#43261=DIRECTION('center_axis',(0.631128321247012,-0.321575941572045,0.705879561909807));
#43262=DIRECTION('ref_axis',(0.628942707293582,-0.320463768412346,-0.708331874249054));
#43263=DIRECTION('center_axis',(5.15167520928809E-67,-1.18789542670764E-48,
-1.));
#43264=DIRECTION('ref_axis',(-4.33680868994202E-19,1.,-1.18789542670764E-48));
#43265=DIRECTION('center_axis',(0.654413322126613,-0.271066873422487,0.70587956051735));
#43266=DIRECTION('ref_axis',(0.652147192704133,-0.270129585579022,-0.708331875636714));
#43267=DIRECTION('center_axis',(5.15167520928809E-67,-1.18789542670764E-48,
-1.));
#43268=DIRECTION('ref_axis',(-4.33680868994202E-19,1.,-1.18789542670764E-48));
#43269=DIRECTION('center_axis',(0.673663698306673,-0.218886604216949,0.705879505353533));
#43270=DIRECTION('ref_axis',(0.671330916306432,-0.218129954133086,-0.708331930609559));
#43271=DIRECTION('center_axis',(5.15167520928809E-67,-1.18789542670764E-48,
-1.));
#43272=DIRECTION('ref_axis',(-4.33680868994202E-19,1.,-1.18789542670764E-48));
#43273=DIRECTION('center_axis',(0.688760770927107,-0.165356831187235,0.705879393955946));
#43274=DIRECTION('ref_axis',(0.686375600198304,-0.164785479532649,-0.708332041621451));
#43275=DIRECTION('center_axis',(5.15167520928809E-67,-1.18789542670764E-48,
-1.));
#43276=DIRECTION('ref_axis',(-4.33680868994202E-19,1.,-1.18789542670764E-48));
#43277=DIRECTION('center_axis',(0.699611468639781,-0.110807570905153,0.705879221381242));
#43278=DIRECTION('ref_axis',(0.697188483633051,-0.110425058152577,-0.708332213598567));
#43279=DIRECTION('center_axis',(5.15167520928809E-67,-1.18789542670764E-48,
-1.));
#43280=DIRECTION('ref_axis',(-4.33680868994202E-19,1.,-1.18789542670764E-48));
#43281=DIRECTION('center_axis',(0.706148902304913,-0.0555751238837372,0.705878979272562));
#43282=DIRECTION('ref_axis',(0.703702893729778,-0.0553838490533553,-0.708332454868737));
#43283=DIRECTION('center_axis',(5.15167520928809E-67,-1.18789542670764E-48,
-1.));
#43284=DIRECTION('ref_axis',(-4.33680868994202E-19,1.,-1.18789542670764E-48));
#43285=DIRECTION('center_axis',(0.708332577472403,3.07190287735134E-19,
0.705878856243267));
#43286=DIRECTION('ref_axis',(0.705878856242412,-1.55615277571261E-6,-0.708332577471545));
#43287=DIRECTION('center_axis',(5.15167520928809E-67,-1.18789542670764E-48,
-1.));
#43288=DIRECTION('ref_axis',(-4.33680868994202E-19,1.,-1.18789542670764E-48));
#43289=DIRECTION('center_axis',(0.706157633406551,0.0555758110364317,0.705870190622399));
#43290=DIRECTION('ref_axis',(0.703694571287442,0.0553775799351074,-0.70834121296245));
#43291=DIRECTION('center_axis',(5.15167520928809E-67,-1.18789542670764E-48,
-1.));
#43292=DIRECTION('ref_axis',(-4.33680868994202E-19,1.,-1.18789542670764E-48));
#43293=DIRECTION('center_axis',(0.699618093637069,0.110808620201609,0.705872490429149));
#43294=DIRECTION('ref_axis',(0.697182591372912,0.11041923309682,-0.708338921173234));
#43295=DIRECTION('center_axis',(5.15167520928809E-67,-1.18789542670764E-48,
-1.));
#43296=DIRECTION('ref_axis',(-4.33680868994202E-19,1.,-1.18789542670764E-48));
#43297=DIRECTION('center_axis',(0.688765827030135,0.165358045050174,0.705874176077209));
#43298=DIRECTION('ref_axis',(0.686371526838244,0.16478009468095,-0.708337241391891));
#43299=DIRECTION('center_axis',(5.15167520928809E-67,-1.18789542670764E-48,
-1.));
#43300=DIRECTION('ref_axis',(-4.33680868994202E-19,1.,-1.18789542670764E-48));
#43301=DIRECTION('center_axis',(0.673667540197388,0.21888785252289,0.705875451692661));
#43302=DIRECTION('ref_axis',(0.671328261761852,0.21812500605297,-0.708335970210607));
#43303=DIRECTION('center_axis',(5.15167520928809E-67,-1.18789542670764E-48,
-1.));
#43304=DIRECTION('ref_axis',(-4.33680868994202E-19,1.,-1.18789542670764E-48));
#43305=DIRECTION('center_axis',(0.654416196007382,0.271068063822859,0.705876439030624));
#43306=DIRECTION('ref_axis',(0.652145682814771,0.270125073933009,-0.708334986301497));
#43307=DIRECTION('center_axis',(5.15167520928809E-67,-1.18789542670764E-48,
-1.));
#43308=DIRECTION('ref_axis',(-4.33680868994202E-19,1.,-1.18789542670764E-48));
#43309=DIRECTION('center_axis',(0.631130405143941,0.321577003370555,0.705877214964514));
#43310=DIRECTION('ref_axis',(0.628942147608526,0.320459697262857,-0.708334213060313));
#43311=DIRECTION('center_axis',(5.15167520928809E-67,-1.18789542670764E-48,
-1.));
#43312=DIRECTION('ref_axis',(-4.33680868994202E-19,1.,-1.18789542670764E-48));
#43313=DIRECTION('center_axis',(0.603953677099555,0.370103289326611,0.705877830185613));
#43314=DIRECTION('ref_axis',(0.601860775525942,0.368818543504321,-0.708333599972967));
#43315=DIRECTION('center_axis',(5.15167520928809E-67,-1.18789542670764E-48,
-1.));
#43316=DIRECTION('ref_axis',(-4.33680868994202E-19,1.,-1.18789542670764E-48));
#43317=DIRECTION('center_axis',(0.573053525770564,0.41634775729573,0.705878319256755));
#43318=DIRECTION('ref_axis',(-0.571068576442187,-0.414903461781831,0.708333112597277));
#43319=DIRECTION('center_axis',(5.15167520928809E-67,-1.18789542670764E-48,
-1.));
#43320=DIRECTION('ref_axis',(-4.33680868994202E-19,1.,-1.18789542670764E-48));
#43321=DIRECTION('center_axis',(0.538620431161647,0.46002530705115,0.705878706299982));
#43322=DIRECTION('ref_axis',(-0.536755427393011,-0.458430320957492,0.708332726895318));
#43323=DIRECTION('center_axis',(5.15167520928809E-67,-1.18789542670764E-48,
-1.));
#43324=DIRECTION('ref_axis',(-4.33680868994202E-19,1.,-1.18789542670764E-48));
#43325=DIRECTION('center_axis',(0.500866661619527,0.500866661619527,0.705879008439988));
#43326=DIRECTION('ref_axis',(-0.49913290577155,-0.499130761357605,0.708332425802057));
#43327=DIRECTION('center_axis',(5.15167520928809E-67,-1.18789542670764E-48,
-1.));
#43328=DIRECTION('ref_axis',(-4.33680868994202E-19,1.,-1.18789542670764E-48));
#43329=DIRECTION('center_axis',(0.460024963033642,0.538620028368862,0.705879237848672));
#43330=DIRECTION('ref_axis',(-0.45843298726639,-0.536753849183101,0.708332197187972));
#43331=DIRECTION('center_axis',(5.15167520928809E-67,-1.18789542670764E-48,
-1.));
#43332=DIRECTION('ref_axis',(-4.33680868994202E-19,1.,-1.18789542670764E-48));
#43333=DIRECTION('center_axis',(0.416347122442686,0.573052651970292,0.705879403087744));
#43334=DIRECTION('ref_axis',(-0.414906617258984,-0.571067623543104,0.708332032521146));
#43335=DIRECTION('center_axis',(5.15167520928809E-67,-1.18789542670764E-48,
-1.));
#43336=DIRECTION('ref_axis',(-4.33680868994202E-19,1.,-1.18789542670764E-48));
#43337=DIRECTION('center_axis',(0.370102414699172,0.603952249837277,0.705879509938016));
#43338=DIRECTION('ref_axis',(-0.368822164724246,-0.601860526500403,0.708331926040877));
#43339=DIRECTION('center_axis',(5.15167520928809E-67,-1.18789542670764E-48,
-1.));
#43340=DIRECTION('ref_axis',(-4.33680868994202E-19,1.,-1.18789542670764E-48));
#43341=DIRECTION('center_axis',(0.321575941571924,0.631128321246917,0.705879561909948));
#43342=DIRECTION('ref_axis',(-0.320463768412656,-0.628942707293582,0.708331874248914));
#43343=DIRECTION('center_axis',(5.15167520928809E-67,-1.18789542670764E-48,
-1.));
#43344=DIRECTION('ref_axis',(-4.33680868994202E-19,1.,-1.18789542670764E-48));
#43345=DIRECTION('center_axis',(0.271066873422485,0.654413322126598,0.705879560517365));
#43346=DIRECTION('ref_axis',(-0.270129585579224,-0.652147192704065,0.708331875636699));
#43347=DIRECTION('center_axis',(5.15167520928809E-67,-1.18789542670764E-48,
-1.));
#43348=DIRECTION('ref_axis',(-4.33680868994202E-19,1.,-1.18789542670764E-48));
#43349=DIRECTION('center_axis',(0.218886604216952,0.67366369830668,0.705879505353526));
#43350=DIRECTION('ref_axis',(-0.218129954132996,-0.671330916306453,0.708331930609566));
#43351=DIRECTION('center_axis',(5.15167520928809E-67,-1.18789542670764E-48,
-1.));
#43352=DIRECTION('ref_axis',(-4.33680868994202E-19,1.,-1.18789542670764E-48));
#43353=DIRECTION('center_axis',(0.16535683118711,0.68876077092705,0.705879393956031));
#43354=DIRECTION('ref_axis',(-0.164785479532882,-0.686375600198336,0.708332041621366));
#43355=DIRECTION('center_axis',(5.15167520928809E-67,-1.18789542670764E-48,
-1.));
#43356=DIRECTION('ref_axis',(-4.33680868994202E-19,1.,-1.18789542670764E-48));
#43357=DIRECTION('center_axis',(0.110807570905159,0.699611468639805,0.705879221381218));
#43358=DIRECTION('ref_axis',(-0.11042505815257,-0.697188483633028,0.708332213598592));
#43359=DIRECTION('center_axis',(5.15167520928809E-67,-1.18789542670764E-48,
-1.));
#43360=DIRECTION('ref_axis',(-4.33680868994202E-19,1.,-1.18789542670764E-48));
#43361=DIRECTION('center_axis',(0.055575123883674,0.706148902304893,0.705878979272587));
#43362=DIRECTION('ref_axis',(-0.0553838490533958,-0.7037028937298,0.708332454868712));
#43363=DIRECTION('center_axis',(5.15167520928809E-67,-1.18789542670764E-48,
-1.));
#43364=DIRECTION('ref_axis',(-4.33680868994202E-19,1.,-1.18789542670764E-48));
#43365=DIRECTION('center_axis',(4.84352581305682E-13,0.70837017493119,0.705841126081468));
#43366=DIRECTION('ref_axis',(-1.41156745807278E-12,-0.705841126081468,0.70837017493119));
#43367=DIRECTION('center_axis',(5.15167520928809E-67,-1.18789542670764E-48,
-1.));
#43368=DIRECTION('ref_axis',(-4.33680868994202E-19,1.,-1.18789542670764E-48));
#43369=DIRECTION('center_axis',(-0.0555758110363152,0.706157633406656,0.705870190622303));
#43370=DIRECTION('ref_axis',(0.0553775799350914,-0.703694571287347,0.708341212962545));
#43371=DIRECTION('center_axis',(5.15167520928809E-67,-1.18789542670764E-48,
-1.));
#43372=DIRECTION('ref_axis',(-4.33680868994202E-19,1.,-1.18789542670764E-48));
#43373=DIRECTION('center_axis',(-0.110808620201596,0.699618093636976,0.705872490429243));
#43374=DIRECTION('ref_axis',(0.11041923309583,-0.697182591373165,0.70833892117314));
#43375=DIRECTION('center_axis',(5.15167520928809E-67,-1.18789542670764E-48,
-1.));
#43376=DIRECTION('ref_axis',(-4.33680868994202E-19,1.,-1.18789542670764E-48));
#43377=DIRECTION('center_axis',(-0.165358045050154,0.688765827030126,0.705874176077223));
#43378=DIRECTION('ref_axis',(0.164780094680844,-0.686371526838284,0.708337241391878));
#43379=DIRECTION('center_axis',(5.15167520928809E-67,-1.18789542670764E-48,
-1.));
#43380=DIRECTION('ref_axis',(-4.33680868994202E-19,1.,-1.18789542670764E-48));
#43381=DIRECTION('center_axis',(-0.218887852522867,0.673667540197309,0.705875451692744));
#43382=DIRECTION('ref_axis',(0.218125006054104,-0.67132826176157,0.708335970210525));
#43383=DIRECTION('center_axis',(5.15167520928809E-67,-1.18789542670764E-48,
-1.));
#43384=DIRECTION('ref_axis',(-4.33680868994202E-19,1.,-1.18789542670764E-48));
#43385=DIRECTION('center_axis',(-0.271068063822887,0.654416196007496,0.705876439030507));
#43386=DIRECTION('ref_axis',(0.270125073932604,-0.652145682814813,0.708334986301614));
#43387=DIRECTION('center_axis',(5.15167520928809E-67,-1.18789542670764E-48,
-1.));
#43388=DIRECTION('ref_axis',(-4.33680868994202E-19,1.,-1.18789542670764E-48));
#43389=DIRECTION('center_axis',(5.15167520928809E-67,-1.18789542670764E-48,
-1.));
#43390=DIRECTION('ref_axis',(-4.33680868994202E-19,1.,-1.18789542670764E-48));
#43391=DIRECTION('center_axis',(5.15167520928809E-67,-1.18789542670764E-48,
-1.));
#43392=DIRECTION('ref_axis',(-4.33680868994202E-19,1.,-1.18789542670764E-48));
#43393=DIRECTION('center_axis',(5.15167520928809E-67,-1.18789542670764E-48,
-1.));
#43394=DIRECTION('ref_axis',(-4.33680868994202E-19,1.,-1.18789542670764E-48));
#43395=DIRECTION('center_axis',(5.15167520928809E-67,-1.18789542670764E-48,
-1.));
#43396=DIRECTION('ref_axis',(-4.33680868994202E-19,1.,-1.18789542670764E-48));
#43397=DIRECTION('center_axis',(5.15167520928809E-67,-1.18789542670764E-48,
-1.));
#43398=DIRECTION('ref_axis',(-4.33680868994202E-19,1.,-1.18789542670764E-48));
#43399=DIRECTION('center_axis',(5.15167520928809E-67,-1.18789542670764E-48,
-1.));
#43400=DIRECTION('ref_axis',(-4.33680868994202E-19,1.,-1.18789542670764E-48));
#43401=DIRECTION('center_axis',(5.15167520928809E-67,-1.18789542670764E-48,
-1.));
#43402=DIRECTION('ref_axis',(-4.33680868994202E-19,1.,-1.18789542670764E-48));
#43403=DIRECTION('center_axis',(5.15167520928809E-67,-1.18789542670764E-48,
-1.));
#43404=DIRECTION('ref_axis',(-4.33680868994202E-19,1.,-1.18789542670764E-48));
#43405=DIRECTION('center_axis',(5.15167520928809E-67,-1.18789542670764E-48,
-1.));
#43406=DIRECTION('ref_axis',(-4.33680868994202E-19,1.,-1.18789542670764E-48));
#43407=DIRECTION('center_axis',(5.15167520928809E-67,-1.18789542670764E-48,
-1.));
#43408=DIRECTION('ref_axis',(-4.33680868994202E-19,1.,-1.18789542670764E-48));
#43409=DIRECTION('center_axis',(5.15167520928809E-67,-1.18789542670764E-48,
-1.));
#43410=DIRECTION('ref_axis',(-4.33680868994202E-19,1.,-1.18789542670764E-48));
#43411=DIRECTION('center_axis',(5.15167520928809E-67,-1.18789542670764E-48,
-1.));
#43412=DIRECTION('ref_axis',(-4.33680868994202E-19,1.,-1.18789542670764E-48));
#43413=DIRECTION('center_axis',(5.15167520928809E-67,-1.18789542670764E-48,
-1.));
#43414=DIRECTION('ref_axis',(-4.33680868994202E-19,1.,-1.18789542670764E-48));
#43415=DIRECTION('center_axis',(5.15167520928809E-67,-1.18789542670764E-48,
-1.));
#43416=DIRECTION('ref_axis',(-4.33680868994202E-19,1.,-1.18789542670764E-48));
#43417=DIRECTION('center_axis',(5.15167520928809E-67,-1.18789542670764E-48,
-1.));
#43418=DIRECTION('ref_axis',(-4.33680868994202E-19,1.,-1.18789542670764E-48));
#43419=DIRECTION('center_axis',(-0.7061576334064,-0.0555758110363729,0.705870190622555));
#43420=DIRECTION('ref_axis',(0.703694571287618,0.0553775799348557,0.708341212962294));
#43421=DIRECTION('center_axis',(5.15167520928809E-67,-1.18789542670764E-48,
-1.));
#43422=DIRECTION('ref_axis',(-4.33680868994202E-19,1.,-1.18789542670764E-48));
#43423=DIRECTION('center_axis',(-0.699618093637056,-0.110808620201623,0.70587249042916));
#43424=DIRECTION('ref_axis',(0.697182591373085,0.110419233095803,0.708338921173223));
#43425=DIRECTION('center_axis',(5.15167520928809E-67,-1.18789542670764E-48,
-1.));
#43426=DIRECTION('ref_axis',(-4.33680868994202E-19,1.,-1.18789542670764E-48));
#43427=DIRECTION('center_axis',(-0.68876582703002,-0.165358045050145,0.705874176077329));
#43428=DIRECTION('ref_axis',(0.686371526838198,0.164780094681657,0.708337241391772));
#43429=DIRECTION('center_axis',(5.15167520928809E-67,-1.18789542670764E-48,
-1.));
#43430=DIRECTION('ref_axis',(-4.33680868994202E-19,1.,-1.18789542670764E-48));
#43431=DIRECTION('center_axis',(-0.673667540197642,-0.218887852522971,0.705875451692394));
#43432=DIRECTION('ref_axis',(0.671328261761337,0.218125006053688,0.708335970210874));
#43433=DIRECTION('center_axis',(5.15167520928809E-67,-1.18789542670764E-48,
-1.));
#43434=DIRECTION('ref_axis',(-4.33680868994202E-19,1.,-1.18789542670764E-48));
#43435=DIRECTION('center_axis',(-0.654416196007479,-0.271068063822885,0.705876439030525));
#43436=DIRECTION('ref_axis',(0.652145682815046,0.270125073932086,0.708334986301596));
#43437=DIRECTION('center_axis',(5.15167520928809E-67,-1.18789542670764E-48,
-1.));
#43438=DIRECTION('ref_axis',(-4.33680868994202E-19,1.,-1.18789542670764E-48));
#43439=DIRECTION('center_axis',(-0.631130405143739,-0.321577003370466,0.705877214964735));
#43440=DIRECTION('ref_axis',(0.628942147608447,0.3204596972635,0.708334213060093));
#43441=DIRECTION('center_axis',(5.15167520928809E-67,-1.18789542670764E-48,
-1.));
#43442=DIRECTION('ref_axis',(-4.33680868994202E-19,1.,-1.18789542670764E-48));
#43443=DIRECTION('center_axis',(-0.603953677099563,-0.37010328932661,0.705877830185607));
#43444=DIRECTION('ref_axis',(0.601860775526009,0.3688185435042,0.708333599972973));
#43445=DIRECTION('center_axis',(5.15167520928809E-67,-1.18789542670764E-48,
-1.));
#43446=DIRECTION('ref_axis',(-4.33680868994202E-19,1.,-1.18789542670764E-48));
#43447=DIRECTION('center_axis',(-0.573053525770468,-0.416347757295655,0.705878319256877));
#43448=DIRECTION('ref_axis',(-0.571068576442267,-0.414903461781928,-0.708333112597156));
#43449=DIRECTION('center_axis',(5.15167520928809E-67,-1.18789542670764E-48,
-1.));
#43450=DIRECTION('ref_axis',(-4.33680868994202E-19,1.,-1.18789542670764E-48));
#43451=DIRECTION('center_axis',(-0.5386204311615,-0.460025307051025,0.705878706300176));
#43452=DIRECTION('ref_axis',(-0.53675542739315,-0.458430320957627,-0.708332726895124));
#43453=DIRECTION('center_axis',(5.15167520928809E-67,-1.18789542670764E-48,
-1.));
#43454=DIRECTION('ref_axis',(-4.33680868994202E-19,1.,-1.18789542670764E-48));
#43455=DIRECTION('center_axis',(-0.500866661619536,-0.500866661619512,0.705879008439992));
#43456=DIRECTION('ref_axis',(-0.499132905770748,-0.499130761358414,-0.708332425802052));
#43457=DIRECTION('center_axis',(5.15167520928809E-67,-1.18789542670764E-48,
-1.));
#43458=DIRECTION('ref_axis',(-4.33680868994202E-19,1.,-1.18789542670764E-48));
#43459=DIRECTION('center_axis',(-0.460024963033767,-0.538620028369008,0.70587923784848));
#43460=DIRECTION('ref_axis',(-0.45843298726701,-0.536753849182318,-0.708332197188163));
#43461=DIRECTION('center_axis',(5.15167520928809E-67,-1.18789542670764E-48,
-1.));
#43462=DIRECTION('ref_axis',(-4.33680868994202E-19,1.,-1.18789542670764E-48));
#43463=DIRECTION('center_axis',(-0.416347122442742,-0.573052651970378,0.705879403087642));
#43464=DIRECTION('ref_axis',(-0.414906617259033,-0.571067623542942,-0.708332032521248));
#43465=DIRECTION('center_axis',(5.15167520928809E-67,-1.18789542670764E-48,
-1.));
#43466=DIRECTION('ref_axis',(-4.33680868994202E-19,1.,-1.18789542670764E-48));
#43467=DIRECTION('center_axis',(-0.370102414699178,-0.603952249837274,0.705879509938015));
#43468=DIRECTION('ref_axis',(-0.368822164723695,-0.601860526500739,-0.708331926040878));
#43469=DIRECTION('center_axis',(5.15167520928809E-67,-1.18789542670764E-48,
-1.));
#43470=DIRECTION('ref_axis',(-4.33680868994202E-19,1.,-1.18789542670764E-48));
#43471=DIRECTION('center_axis',(-0.321575941572111,-0.631128321247095,0.705879561909702));
#43472=DIRECTION('ref_axis',(-0.320463768412258,-0.628942707293509,-0.708331874249159));
#43473=DIRECTION('center_axis',(5.15167520928809E-67,-1.18789542670764E-48,
-1.));
#43474=DIRECTION('ref_axis',(-4.33680868994202E-19,1.,-1.18789542670764E-48));
#43475=DIRECTION('center_axis',(-0.271066873422704,-0.654413322126826,0.70587956051707));
#43476=DIRECTION('ref_axis',(-0.270129585579653,-0.652147192703568,-0.708331875636993));
#43477=DIRECTION('center_axis',(5.15167520928809E-67,-1.18789542670764E-48,
-1.));
#43478=DIRECTION('ref_axis',(-4.33680868994202E-19,1.,-1.18789542670764E-48));
#43479=DIRECTION('center_axis',(-0.218886604216915,-0.673663698306575,0.705879505353637));
#43480=DIRECTION('ref_axis',(-0.218129954131654,-0.671330916307006,-0.708331930609455));
#43481=DIRECTION('center_axis',(5.15167520928809E-67,-1.18789542670764E-48,
-1.));
#43482=DIRECTION('ref_axis',(-4.33680868994202E-19,1.,-1.18789542670764E-48));
#43483=DIRECTION('center_axis',(-0.165356831187205,-0.688760770926913,0.705879393956142));
#43484=DIRECTION('ref_axis',(-0.164785479532657,-0.686375600198504,-0.708332041621255));
#43485=DIRECTION('center_axis',(5.15167520928809E-67,-1.18789542670764E-48,
-1.));
#43486=DIRECTION('ref_axis',(-4.33680868994202E-19,1.,-1.18789542670764E-48));
#43487=DIRECTION('center_axis',(-0.110807570905278,-0.699611468639872,0.705879221381132));
#43488=DIRECTION('ref_axis',(-0.110425058152835,-0.697188483632899,-0.708332213598677));
#43489=DIRECTION('center_axis',(5.15167520928809E-67,-1.18789542670764E-48,
-1.));
#43490=DIRECTION('ref_axis',(-4.33680868994202E-19,1.,-1.18789542670764E-48));
#43491=DIRECTION('center_axis',(-0.0555751238837442,-0.706148902305009,
0.705878979272465));
#43492=DIRECTION('ref_axis',(-0.0553838490528384,-0.703702893729722,-0.708332454868834));
#43493=DIRECTION('center_axis',(5.15167520928809E-67,-1.18789542670764E-48,
-1.));
#43494=DIRECTION('ref_axis',(-4.33680868994202E-19,1.,-1.18789542670764E-48));
#43495=DIRECTION('',(8.62889469402126E-17,0.707106781186547,0.707106781186548));
#43496=DIRECTION('center_axis',(-5.15167520928809E-67,1.18789542670764E-48,
1.));
#43497=DIRECTION('ref_axis',(4.33680868994202E-19,-1.,1.18789542670764E-48));
#43498=DIRECTION('center_axis',(5.15167520928809E-67,-1.18789542670764E-48,
-1.));
#43499=DIRECTION('ref_axis',(-4.33680868994202E-19,1.,-1.18789542670764E-48));
#43500=DIRECTION('center_axis',(0.0555758110363494,0.706157633406676,-0.705870190622281));
#43501=DIRECTION('ref_axis',(0.0553775799347821,0.703694571287349,0.708341212962568));
#43502=DIRECTION('center_axis',(5.15167520928809E-67,-1.18789542670764E-48,
-1.));
#43503=DIRECTION('ref_axis',(-4.33680868994202E-19,1.,-1.18789542670764E-48));
#43504=DIRECTION('center_axis',(0.110808620201597,0.699618093636782,-0.705872490429435));
#43505=DIRECTION('ref_axis',(0.110419233096536,0.697182591373247,0.708338921172949));
#43506=DIRECTION('center_axis',(5.15167520928809E-67,-1.18789542670764E-48,
-1.));
#43507=DIRECTION('ref_axis',(-4.33680868994202E-19,1.,-1.18789542670764E-48));
#43508=DIRECTION('center_axis',(0.165358045050176,0.688765827030065,-0.705874176077277));
#43509=DIRECTION('ref_axis',(0.164780094681565,0.686371526838166,0.708337241391824));
#43510=DIRECTION('center_axis',(5.15167520928809E-67,-1.18789542670764E-48,
-1.));
#43511=DIRECTION('ref_axis',(-4.33680868994202E-19,1.,-1.18789542670764E-48));
#43512=DIRECTION('center_axis',(0.218887852522828,0.673667540197125,-0.705875451692931));
#43513=DIRECTION('ref_axis',(0.218125006053502,0.671328261761963,0.708335970210338));
#43514=DIRECTION('center_axis',(5.15167520928809E-67,-1.18789542670764E-48,
-1.));
#43515=DIRECTION('ref_axis',(-4.33680868994202E-19,1.,-1.18789542670764E-48));
#43516=DIRECTION('center_axis',(0.271068063822916,0.654416196007463,-0.705876439030527));
#43517=DIRECTION('ref_axis',(0.270125073931817,0.65214568281516,0.708334986301594));
#43518=DIRECTION('center_axis',(5.15167520928809E-67,-1.18789542670764E-48,
-1.));
#43519=DIRECTION('ref_axis',(-4.33680868994202E-19,1.,-1.18789542670764E-48));
#43520=DIRECTION('center_axis',(0.321577003370433,0.631130405143686,-0.705877214964798));
#43521=DIRECTION('ref_axis',(0.320459697263181,0.62894214760868,0.70833421306003));
#43522=DIRECTION('center_axis',(5.15167520928809E-67,-1.18789542670764E-48,
-1.));
#43523=DIRECTION('ref_axis',(-4.33680868994202E-19,1.,-1.18789542670764E-48));
#43524=DIRECTION('center_axis',(0.37010328932647,0.603953677099309,-0.705877830185898));
#43525=DIRECTION('ref_axis',(0.368818543504439,0.601860775526204,0.708333599972683));
#43526=DIRECTION('center_axis',(5.15167520928809E-67,-1.18789542670764E-48,
-1.));
#43527=DIRECTION('ref_axis',(-4.33680868994202E-19,1.,-1.18789542670764E-48));
#43528=DIRECTION('center_axis',(0.416347757295563,0.573053525770315,-0.705878319257056));
#43529=DIRECTION('ref_axis',(0.414903461782186,0.5710685764423,0.708333112596977));
#43530=DIRECTION('center_axis',(5.15167520928809E-67,-1.18789542670764E-48,
-1.));
#43531=DIRECTION('ref_axis',(-4.33680868994202E-19,1.,-1.18789542670764E-48));
#43532=DIRECTION('center_axis',(0.46002530705103,0.538620431161473,-0.705878706300193));
#43533=DIRECTION('ref_axis',(0.458430320957387,0.536755427393379,0.708332726895108));
#43534=DIRECTION('center_axis',(5.15167520928809E-67,-1.18789542670764E-48,
-1.));
#43535=DIRECTION('ref_axis',(-4.33680868994202E-19,1.,-1.18789542670764E-48));
#43536=DIRECTION('center_axis',(0.500866661619595,0.500866661619595,-0.705879008439891));
#43537=DIRECTION('ref_axis',(0.499130761358023,0.499132905770996,0.708332425802153));
#43538=DIRECTION('center_axis',(5.15167520928809E-67,-1.18789542670764E-48,
-1.));
#43539=DIRECTION('ref_axis',(-4.33680868994202E-19,1.,-1.18789542670764E-48));
#43540=DIRECTION('center_axis',(0.538620028368889,0.460024963033635,-0.705879237848656));
#43541=DIRECTION('ref_axis',(0.536753849182959,0.458432987266531,0.708332197187987));
#43542=DIRECTION('center_axis',(5.15167520928809E-67,-1.18789542670764E-48,
-1.));
#43543=DIRECTION('ref_axis',(-4.33680868994202E-19,1.,-1.18789542670764E-48));
#43544=DIRECTION('center_axis',(0.573052651970233,0.416347122442629,-0.705879403087826));
#43545=DIRECTION('ref_axis',(0.57106762354309,0.414906617259142,0.708332032521065));
#43546=DIRECTION('center_axis',(5.15167520928809E-67,-1.18789542670764E-48,
-1.));
#43547=DIRECTION('ref_axis',(-4.33680868994202E-19,1.,-1.18789542670764E-48));
#43548=DIRECTION('center_axis',(0.603952249837032,0.370102414699012,-0.70587950993831));
#43549=DIRECTION('ref_axis',(0.601860526500475,0.36882216472469,0.708331926040585));
#43550=DIRECTION('center_axis',(5.15167520928809E-67,-1.18789542670764E-48,
-1.));
#43551=DIRECTION('ref_axis',(-4.33680868994202E-19,1.,-1.18789542670764E-48));
#43552=DIRECTION('center_axis',(0.631128321246922,0.32157594157199,-0.705879561909913));
#43553=DIRECTION('ref_axis',(0.628942707293632,0.32046376841248,0.708331874248949));
#43554=DIRECTION('center_axis',(5.15167520928809E-67,-1.18789542670764E-48,
-1.));
#43555=DIRECTION('ref_axis',(-4.33680868994202E-19,1.,-1.18789542670764E-48));
#43556=DIRECTION('center_axis',(0.654413322126609,0.271066873422466,-0.705879560517362));
#43557=DIRECTION('ref_axis',(0.652147192704168,0.270129585578968,0.708331875636702));
#43558=DIRECTION('center_axis',(5.15167520928809E-67,-1.18789542670764E-48,
-1.));
#43559=DIRECTION('ref_axis',(-4.33680868994202E-19,1.,-1.18789542670764E-48));
#43560=DIRECTION('center_axis',(0.673663698306398,0.218886604216837,-0.70587950535383));
#43561=DIRECTION('ref_axis',(0.671330916306662,0.218129954133339,0.708331930609263));
#43562=DIRECTION('center_axis',(5.15167520928809E-67,-1.18789542670764E-48,
-1.));
#43563=DIRECTION('ref_axis',(-4.33680868994202E-19,1.,-1.18789542670764E-48));
#43564=DIRECTION('center_axis',(0.688760770927087,0.165356831187229,-0.705879393955967));
#43565=DIRECTION('ref_axis',(0.686375600198292,0.164785479532791,0.70833204162143));
#43566=DIRECTION('center_axis',(5.15167520928809E-67,-1.18789542670764E-48,
-1.));
#43567=DIRECTION('ref_axis',(-4.33680868994202E-19,1.,-1.18789542670764E-48));
#43568=DIRECTION('center_axis',(0.699611468639904,0.110807570905141,-0.705879221381122));
#43569=DIRECTION('ref_axis',(0.697188483632864,0.11042505815299,0.708332213598687));
#43570=DIRECTION('center_axis',(5.15167520928809E-67,-1.18789542670764E-48,
-1.));
#43571=DIRECTION('ref_axis',(-4.33680868994202E-19,1.,-1.18789542670764E-48));
#43572=DIRECTION('center_axis',(0.706148902304704,0.0555751238836885,-0.705878979272775));
#43573=DIRECTION('ref_axis',(0.703702893729991,0.0553838490533688,0.708332454868525));
#43574=DIRECTION('center_axis',(5.15167520928809E-67,-1.18789542670764E-48,
-1.));
#43575=DIRECTION('ref_axis',(-4.33680868994202E-19,1.,-1.18789542670764E-48));
#43576=DIRECTION('center_axis',(0.708332577472139,3.0719028773502E-19,-0.705878856243532));
#43577=DIRECTION('ref_axis',(0.705878856242677,1.5561538090606E-6,0.708332577471281));
#43578=DIRECTION('center_axis',(5.15167520928809E-67,-1.18789542670764E-48,
-1.));
#43579=DIRECTION('ref_axis',(-4.33680868994202E-19,1.,-1.18789542670764E-48));
#43580=DIRECTION('center_axis',(0.706157633406651,-0.0555758110363464,-0.705870190622306));
#43581=DIRECTION('ref_axis',(0.703694571287399,-0.0553775799344575,0.708341212962543));
#43582=DIRECTION('center_axis',(5.15167520928809E-67,-1.18789542670764E-48,
-1.));
#43583=DIRECTION('ref_axis',(-4.33680868994202E-19,1.,-1.18789542670764E-48));
#43584=DIRECTION('center_axis',(0.699618093636944,-0.110808620201621,-0.705872490429271));
#43585=DIRECTION('ref_axis',(0.697182591373154,-0.110419233096072,0.708338921173112));
#43586=DIRECTION('center_axis',(5.15167520928809E-67,-1.18789542670764E-48,
-1.));
#43587=DIRECTION('ref_axis',(-4.33680868994202E-19,1.,-1.18789542670764E-48));
#43588=DIRECTION('center_axis',(0.688765827030149,-0.165358045050179,-0.705874176077195));
#43589=DIRECTION('ref_axis',(0.686371526838092,-0.164780094681522,0.708337241391906));
#43590=DIRECTION('center_axis',(5.15167520928809E-67,-1.18789542670764E-48,
-1.));
#43591=DIRECTION('ref_axis',(-4.33680868994202E-19,1.,-1.18789542670764E-48));
#43592=DIRECTION('center_axis',(0.673667540197491,-0.218887852522947,-0.705875451692545));
#43593=DIRECTION('ref_axis',(0.671328261761432,-0.218125006053886,0.708335970210723));
#43594=DIRECTION('center_axis',(5.15167520928809E-67,-1.18789542670764E-48,
-1.));
#43595=DIRECTION('ref_axis',(-4.33680868994202E-19,1.,-1.18789542670764E-48));
#43596=DIRECTION('center_axis',(0.654416196007489,-0.271068063822922,-0.705876439030501));
#43597=DIRECTION('ref_axis',(0.652145682814786,-0.270125073932652,0.70833498630162));
#43598=DIRECTION('center_axis',(5.15167520928809E-67,-1.18789542670764E-48,
-1.));
#43599=DIRECTION('ref_axis',(-4.33680868994202E-19,1.,-1.18789542670764E-48));
#43600=DIRECTION('center_axis',(0.631130405143858,-0.321577003370522,-0.705877214964604));
#43601=DIRECTION('ref_axis',(0.628942147608515,-0.320459697263077,0.708334213060224));
#43602=DIRECTION('center_axis',(5.15167520928809E-67,-1.18789542670764E-48,
-1.));
#43603=DIRECTION('ref_axis',(-4.33680868994202E-19,1.,-1.18789542670764E-48));
#43604=DIRECTION('center_axis',(0.603953677099314,-0.37010328932649,-0.705877830185883));
#43605=DIRECTION('ref_axis',(0.60186077552563,-0.368818543505346,0.708333599972698));
#43606=DIRECTION('center_axis',(5.15167520928809E-67,-1.18789542670764E-48,
-1.));
#43607=DIRECTION('ref_axis',(-4.33680868994202E-19,1.,-1.18789542670764E-48));
#43608=DIRECTION('center_axis',(0.573053525770311,-0.416347757295561,-0.70587831925706));
#43609=DIRECTION('ref_axis',(-0.571068576442179,0.41490346178236,-0.708333112596973));
#43610=DIRECTION('center_axis',(5.15167520928809E-67,-1.18789542670764E-48,
-1.));
#43611=DIRECTION('ref_axis',(-4.33680868994202E-19,1.,-1.18789542670764E-48));
#43612=DIRECTION('center_axis',(0.53862043116148,-0.460025307051029,-0.705878706300189));
#43613=DIRECTION('ref_axis',(-0.536755427393413,0.45843032095734,-0.708332726895112));
#43614=DIRECTION('center_axis',(5.15167520928809E-67,-1.18789542670764E-48,
-1.));
#43615=DIRECTION('ref_axis',(-4.33680868994202E-19,1.,-1.18789542670764E-48));
#43616=DIRECTION('center_axis',(0.500866661619453,-0.500866661619453,-0.705879008440093));
#43617=DIRECTION('ref_axis',(-0.499132905770974,0.49913076135833,-0.708332425801952));
#43618=DIRECTION('center_axis',(5.15167520928809E-67,-1.18789542670764E-48,
-1.));
#43619=DIRECTION('ref_axis',(-4.33680868994202E-19,1.,-1.18789542670764E-48));
#43620=DIRECTION('center_axis',(0.460024963033751,-0.538620028369041,-0.705879237848464));
#43621=DIRECTION('ref_axis',(-0.458432987266724,0.536753849182542,-0.708332197188179));
#43622=DIRECTION('center_axis',(5.15167520928809E-67,-1.18789542670764E-48,
-1.));
#43623=DIRECTION('ref_axis',(-4.33680868994202E-19,1.,-1.18789542670764E-48));
#43624=DIRECTION('center_axis',(0.416347122442499,-0.573052651970059,-0.705879403088044));
#43625=DIRECTION('ref_axis',(-0.414906617258677,0.571067623543698,-0.708332032520848));
#43626=DIRECTION('center_axis',(5.15167520928809E-67,-1.18789542670764E-48,
-1.));
#43627=DIRECTION('ref_axis',(-4.33680868994202E-19,1.,-1.18789542670764E-48));
#43628=DIRECTION('center_axis',(0.370102414698996,-0.603952249837027,-0.705879509938322));
#43629=DIRECTION('ref_axis',(-0.36882216472453,0.601860526500588,-0.708331926040572));
#43630=DIRECTION('center_axis',(5.15167520928809E-67,-1.18789542670764E-48,
-1.));
#43631=DIRECTION('ref_axis',(-4.33680868994202E-19,1.,-1.18789542670764E-48));
#43632=DIRECTION('center_axis',(0.321575941571994,-0.631128321246919,-0.705879561909914));
#43633=DIRECTION('ref_axis',(-0.320463768412686,0.628942707293528,-0.708331874248948));
#43634=DIRECTION('center_axis',(5.15167520928809E-67,-1.18789542670764E-48,
-1.));
#43635=DIRECTION('ref_axis',(-4.33680868994202E-19,1.,-1.18789542670764E-48));
#43636=DIRECTION('center_axis',(0.27106687342253,-0.654413322126797,-0.705879560517163));
#43637=DIRECTION('ref_axis',(-0.270129585579053,0.652147192703917,-0.7083318756369));
#43638=DIRECTION('center_axis',(5.15167520928809E-67,-1.18789542670764E-48,
-1.));
#43639=DIRECTION('ref_axis',(-4.33680868994202E-19,1.,-1.18789542670764E-48));
#43640=DIRECTION('center_axis',(0.218886604216888,-0.673663698306596,-0.705879505353626));
#43641=DIRECTION('ref_axis',(-0.218129954133397,0.671330916306428,-0.708331930609466));
#43642=DIRECTION('center_axis',(5.15167520928809E-67,-1.18789542670764E-48,
-1.));
#43643=DIRECTION('ref_axis',(-4.33680868994202E-19,1.,-1.18789542670764E-48));
#43644=DIRECTION('center_axis',(0.165356831187193,-0.688760770926925,-0.705879393956133));
#43645=DIRECTION('ref_axis',(-0.164785479532379,0.686375600198561,-0.708332041621264));
#43646=DIRECTION('center_axis',(5.15167520928809E-67,-1.18789542670764E-48,
-1.));
#43647=DIRECTION('ref_axis',(-4.33680868994202E-19,1.,-1.18789542670764E-48));
#43648=DIRECTION('center_axis',(0.110807570905112,-0.699611468639716,-0.705879221381312));
#43649=DIRECTION('ref_axis',(-0.110425058152835,0.697188483633082,-0.708332213598497));
#43650=DIRECTION('center_axis',(5.15167520928809E-67,-1.18789542670764E-48,
-1.));
#43651=DIRECTION('ref_axis',(-4.33680868994202E-19,1.,-1.18789542670764E-48));
#43652=DIRECTION('center_axis',(0.0555751238837179,-0.706148902304883,-0.705878979272593));
#43653=DIRECTION('ref_axis',(-0.0553838490533129,0.703702893729813,-0.708332454868706));
#43654=DIRECTION('center_axis',(5.15167520928809E-67,-1.18789542670764E-48,
-1.));
#43655=DIRECTION('ref_axis',(-4.33680868994202E-19,1.,-1.18789542670764E-48));
#43656=DIRECTION('center_axis',(4.22129745643424E-13,-0.708370174930854,
-0.705841126081805));
#43657=DIRECTION('ref_axis',(-3.47233154276107E-12,0.705841126081805,-0.708370174930854));
#43658=DIRECTION('center_axis',(5.15167520928809E-67,-1.18789542670764E-48,
-1.));
#43659=DIRECTION('ref_axis',(-4.33680868994202E-19,1.,-1.18789542670764E-48));
#43660=DIRECTION('center_axis',(-0.0555758110363383,-0.706157633406556,
-0.705870190622402));
#43661=DIRECTION('ref_axis',(0.0553775799352142,0.703694571287436,-0.708341212962447));
#43662=DIRECTION('center_axis',(5.15167520928809E-67,-1.18789542670764E-48,
-1.));
#43663=DIRECTION('ref_axis',(-4.33680868994202E-19,1.,-1.18789542670764E-48));
#43664=DIRECTION('center_axis',(-0.110808620201578,-0.699618093636773,-0.705872490429447));
#43665=DIRECTION('ref_axis',(0.110419233096311,0.697182591373295,-0.708338921172937));
#43666=DIRECTION('center_axis',(5.15167520928809E-67,-1.18789542670764E-48,
-1.));
#43667=DIRECTION('ref_axis',(-4.33680868994202E-19,1.,-1.18789542670764E-48));
#43668=DIRECTION('center_axis',(-0.165358045050148,-0.688765827029952,-0.705874176077394));
#43669=DIRECTION('ref_axis',(0.164780094682061,0.686371526838168,-0.708337241391707));
#43670=DIRECTION('center_axis',(5.15167520928809E-67,-1.18789542670764E-48,
-1.));
#43671=DIRECTION('ref_axis',(-4.33680868994202E-19,1.,-1.18789542670764E-48));
#43672=DIRECTION('center_axis',(-0.218887852522884,-0.673667540197305,-0.705875451692742));
#43673=DIRECTION('ref_axis',(0.218125006053241,0.671328261761849,-0.708335970210527));
#43674=DIRECTION('center_axis',(5.15167520928809E-67,-1.18789542670764E-48,
-1.));
#43675=DIRECTION('ref_axis',(-4.33680868994202E-19,1.,-1.18789542670764E-48));
#43676=DIRECTION('center_axis',(-0.271068063822912,-0.654416196007481,-0.705876439030512));
#43677=DIRECTION('ref_axis',(0.270125073931987,0.652145682815073,-0.708334986301609));
#43678=DIRECTION('center_axis',(5.15167520928809E-67,-1.18789542670764E-48,
-1.));
#43679=DIRECTION('ref_axis',(-4.33680868994202E-19,1.,-1.18789542670764E-48));
#43680=DIRECTION('center_axis',(-0.321577003370454,-0.631130405143677,-0.705877214964797));
#43681=DIRECTION('ref_axis',(0.32045969726294,0.628942147608801,-0.708334213060031));
#43682=DIRECTION('center_axis',(5.15167520928809E-67,-1.18789542670764E-48,
-1.));
#43683=DIRECTION('ref_axis',(-4.33680868994202E-19,1.,-1.18789542670764E-48));
#43684=DIRECTION('center_axis',(-0.370103289326527,-0.60395367709939,-0.705877830185799));
#43685=DIRECTION('ref_axis',(0.368818543504467,0.601860775526071,-0.708333599972782));
#43686=DIRECTION('center_axis',(5.15167520928809E-67,-1.18789542670764E-48,
-1.));
#43687=DIRECTION('ref_axis',(-4.33680868994202E-19,1.,-1.18789542670764E-48));
#43688=DIRECTION('center_axis',(-0.41634775729562,-0.5730535257704,-0.705878319256953));
#43689=DIRECTION('ref_axis',(0.414903461781904,0.571068576442378,-0.70833311259708));
#43690=DIRECTION('center_axis',(5.15167520928809E-67,-1.18789542670764E-48,
-1.));
#43691=DIRECTION('ref_axis',(-4.33680868994202E-19,1.,-1.18789542670764E-48));
#43692=DIRECTION('center_axis',(-0.460025307050912,-0.538620431161332,-0.705878706300378));
#43693=DIRECTION('ref_axis',(0.458430320957773,0.536755427393291,-0.708332726894923));
#43694=DIRECTION('center_axis',(5.15167520928809E-67,-1.18789542670764E-48,
-1.));
#43695=DIRECTION('ref_axis',(-4.33680868994202E-19,1.,-1.18789542670764E-48));
#43696=DIRECTION('center_axis',(-0.500866661619468,-0.500866661619444,-0.705879008440089));
#43697=DIRECTION('ref_axis',(0.499130761358181,0.499132905771117,-0.708332425801956));
#43698=DIRECTION('center_axis',(5.15167520928809E-67,-1.18789542670764E-48,
-1.));
#43699=DIRECTION('ref_axis',(-4.33680868994202E-19,1.,-1.18789542670764E-48));
#43700=DIRECTION('center_axis',(-0.538620028368883,-0.46002496303363,-0.705879237848664));
#43701=DIRECTION('ref_axis',(0.536753849182796,0.458432987266734,-0.70833219718798));
#43702=DIRECTION('center_axis',(5.15167520928809E-67,-1.18789542670764E-48,
-1.));
#43703=DIRECTION('ref_axis',(-4.33680868994202E-19,1.,-1.18789542670764E-48));
#43704=DIRECTION('center_axis',(-0.573052651970218,-0.416347122442612,-0.705879403087848));
#43705=DIRECTION('ref_axis',(0.571067623543181,0.414906617259055,-0.708332032521043));
#43706=DIRECTION('center_axis',(5.15167520928809E-67,-1.18789542670764E-48,
-1.));
#43707=DIRECTION('ref_axis',(-4.33680868994202E-19,1.,-1.18789542670764E-48));
#43708=DIRECTION('center_axis',(-0.603952249837038,-0.37010241469901,-0.705879509938305));
#43709=DIRECTION('ref_axis',(0.601860526500551,0.368822164724558,-0.708331926040589));
#43710=DIRECTION('center_axis',(5.15167520928809E-67,-1.18789542670764E-48,
-1.));
#43711=DIRECTION('ref_axis',(-4.33680868994202E-19,1.,-1.18789542670764E-48));
#43712=DIRECTION('center_axis',(-0.631128321246897,-0.32157594157199,-0.705879561909935));
#43713=DIRECTION('ref_axis',(0.628942707294004,0.320463768411799,-0.708331874248927));
#43714=DIRECTION('center_axis',(5.15167520928809E-67,-1.18789542670764E-48,
-1.));
#43715=DIRECTION('ref_axis',(-4.33680868994202E-19,1.,-1.18789542670764E-48));
#43716=DIRECTION('center_axis',(-0.654413322126778,-0.271066873422522,-0.705879560517184));
#43717=DIRECTION('ref_axis',(0.65214719270402,0.270129585578859,-0.708331875636879));
#43718=DIRECTION('center_axis',(5.15167520928809E-67,-1.18789542670764E-48,
-1.));
#43719=DIRECTION('ref_axis',(-4.33680868994202E-19,1.,-1.18789542670764E-48));
#43720=DIRECTION('center_axis',(-0.673663698306464,-0.218886604216857,-0.705879505353761));
#43721=DIRECTION('ref_axis',(0.671330916306719,0.218129954132939,-0.708331930609331));
#43722=DIRECTION('center_axis',(5.15167520928809E-67,-1.18789542670764E-48,
-1.));
#43723=DIRECTION('ref_axis',(-4.33680868994202E-19,1.,-1.18789542670764E-48));
#43724=DIRECTION('center_axis',(-0.688760770927255,-0.165356831187267,-0.705879393955794));
#43725=DIRECTION('ref_axis',(0.686375600198197,0.164785479532444,-0.708332041621602));
#43726=DIRECTION('center_axis',(5.15167520928809E-67,-1.18789542670764E-48,
-1.));
#43727=DIRECTION('ref_axis',(-4.33680868994202E-19,1.,-1.18789542670764E-48));
#43728=DIRECTION('center_axis',(-0.699611468639891,-0.110807570905155,-0.705879221381132));
#43729=DIRECTION('ref_axis',(0.697188483632974,0.110425058152362,-0.708332213598677));
#43730=DIRECTION('center_axis',(5.15167520928809E-67,-1.18789542670764E-48,
-1.));
#43731=DIRECTION('ref_axis',(-4.33680868994202E-19,1.,-1.18789542670764E-48));
#43732=DIRECTION('center_axis',(-0.706148902304619,-0.0555751238836977,
-0.705878979272859));
#43733=DIRECTION('ref_axis',(0.703702893730101,0.0553838490530483,-0.708332454868441));
#43734=DIRECTION('center_axis',(5.15167520928809E-67,-1.18789542670764E-48,
-1.));
#43735=DIRECTION('ref_axis',(-4.33680868994202E-19,1.,-1.18789542670764E-48));
#43736=DIRECTION('center_axis',(5.15167520928809E-67,-1.18789542670764E-48,
-1.));
#43737=DIRECTION('ref_axis',(-4.33680868994202E-19,1.,-1.18789542670764E-48));
#43738=DIRECTION('center_axis',(5.15167520928809E-67,-1.18789542670764E-48,
-1.));
#43739=DIRECTION('ref_axis',(-4.33680868994202E-19,1.,-1.18789542670764E-48));
#43740=DIRECTION('center_axis',(5.15167520928809E-67,-1.18789542670764E-48,
-1.));
#43741=DIRECTION('ref_axis',(-4.33680868994202E-19,1.,-1.18789542670764E-48));
#43742=DIRECTION('center_axis',(5.15167520928809E-67,-1.18789542670764E-48,
-1.));
#43743=DIRECTION('ref_axis',(-4.33680868994202E-19,1.,-1.18789542670764E-48));
#43744=DIRECTION('center_axis',(5.15167520928809E-67,-1.18789542670764E-48,
-1.));
#43745=DIRECTION('ref_axis',(-4.33680868994202E-19,1.,-1.18789542670764E-48));
#43746=DIRECTION('center_axis',(5.15167520928809E-67,-1.18789542670764E-48,
-1.));
#43747=DIRECTION('ref_axis',(-4.33680868994202E-19,1.,-1.18789542670764E-48));
#43748=DIRECTION('center_axis',(5.15167520928809E-67,-1.18789542670764E-48,
-1.));
#43749=DIRECTION('ref_axis',(-4.33680868994202E-19,1.,-1.18789542670764E-48));
#43750=DIRECTION('center_axis',(5.15167520928809E-67,-1.18789542670764E-48,
-1.));
#43751=DIRECTION('ref_axis',(-4.33680868994202E-19,1.,-1.18789542670764E-48));
#43752=DIRECTION('center_axis',(5.15167520928809E-67,-1.18789542670764E-48,
-1.));
#43753=DIRECTION('ref_axis',(-4.33680868994202E-19,1.,-1.18789542670764E-48));
#43754=DIRECTION('center_axis',(5.15167520928809E-67,-1.18789542670764E-48,
-1.));
#43755=DIRECTION('ref_axis',(-4.33680868994202E-19,1.,-1.18789542670764E-48));
#43756=DIRECTION('center_axis',(5.15167520928809E-67,-1.18789542670764E-48,
-1.));
#43757=DIRECTION('ref_axis',(-4.33680868994202E-19,1.,-1.18789542670764E-48));
#43758=DIRECTION('center_axis',(5.15167520928809E-67,-1.18789542670764E-48,
-1.));
#43759=DIRECTION('ref_axis',(-4.33680868994202E-19,1.,-1.18789542670764E-48));
#43760=DIRECTION('center_axis',(5.15167520928809E-67,-1.18789542670764E-48,
-1.));
#43761=DIRECTION('ref_axis',(-4.33680868994202E-19,1.,-1.18789542670764E-48));
#43762=DIRECTION('center_axis',(5.15167520928809E-67,-1.18789542670764E-48,
-1.));
#43763=DIRECTION('ref_axis',(-4.33680868994202E-19,1.,-1.18789542670764E-48));
#43764=DIRECTION('center_axis',(5.15167520928809E-67,-1.18789542670764E-48,
-1.));
#43765=DIRECTION('ref_axis',(-4.33680868994202E-19,1.,-1.18789542670764E-48));
#43766=DIRECTION('center_axis',(-0.271066873422527,0.654413322126802,-0.70587956051716));
#43767=DIRECTION('ref_axis',(-0.270129585578839,0.652147192704003,0.708331875636903));
#43768=DIRECTION('center_axis',(5.15167520928809E-67,-1.18789542670764E-48,
-1.));
#43769=DIRECTION('ref_axis',(-4.33680868994202E-19,1.,-1.18789542670764E-48));
#43770=DIRECTION('center_axis',(-0.218886604216929,0.673663698306674,-0.705879505353539));
#43771=DIRECTION('ref_axis',(-0.218129954131946,0.671330916306808,0.708331930609553));
#43772=DIRECTION('center_axis',(5.15167520928809E-67,-1.18789542670764E-48,
-1.));
#43773=DIRECTION('ref_axis',(-4.33680868994202E-19,1.,-1.18789542670764E-48));
#43774=DIRECTION('center_axis',(-0.16535683118721,0.688760770927084,-0.705879393955974));
#43775=DIRECTION('ref_axis',(-0.164785479532737,0.686375600198312,0.708332041621423));
#43776=DIRECTION('center_axis',(5.15167520928809E-67,-1.18789542670764E-48,
-1.));
#43777=DIRECTION('ref_axis',(-4.33680868994202E-19,1.,-1.18789542670764E-48));
#43778=DIRECTION('center_axis',(-0.110807570905113,0.699611468639715,-0.705879221381313));
#43779=DIRECTION('ref_axis',(-0.110425058151779,0.69718848363325,0.708332213598496));
#43780=DIRECTION('center_axis',(5.15167520928809E-67,-1.18789542670764E-48,
-1.));
#43781=DIRECTION('ref_axis',(-4.33680868994202E-19,1.,-1.18789542670764E-48));
#43782=DIRECTION('center_axis',(-0.0555751238836985,0.706148902304822,-0.705878979272656));
#43783=DIRECTION('ref_axis',(-0.0553838490532064,0.703702893729884,0.708332454868643));
#43784=DIRECTION('center_axis',(5.15167520928809E-67,-1.18789542670764E-48,
-1.));
#43785=DIRECTION('ref_axis',(-4.33680868994202E-19,1.,-1.18789542670764E-48));
#43786=DIRECTION('',(8.69022643068848E-17,-0.707106781186538,-0.707106781186557));
#43787=DIRECTION('center_axis',(5.15167520928809E-67,-1.18789542670764E-48,
-1.));
#43788=DIRECTION('ref_axis',(-4.33680868994202E-19,1.,-1.18789542670764E-48));
#43789=DIRECTION('center_axis',(5.15167520928809E-67,-1.18789542670764E-48,
-1.));
#43790=DIRECTION('ref_axis',(-4.33680868994202E-19,1.,-1.18789542670764E-48));
#43791=DIRECTION('center_axis',(5.15167520928809E-67,-1.18789542670764E-48,
-1.));
#43792=DIRECTION('ref_axis',(0.,1.,0.));
#43793=DIRECTION('center_axis',(5.15167520928809E-67,-1.18789542670764E-48,
-1.));
#43794=DIRECTION('ref_axis',(-4.33680868994202E-19,1.,-1.18789542670764E-48));
#43795=DIRECTION('center_axis',(1.,0.,5.15167520928809E-67));
#43796=DIRECTION('ref_axis',(0.,-1.,0.));
#43797=DIRECTION('center_axis',(5.15167520928809E-67,-1.18789542670764E-48,
-1.));
#43798=DIRECTION('ref_axis',(-4.33680868994202E-19,1.,-1.18789542670764E-48));
#43799=DIRECTION('center_axis',(5.15167520928809E-67,-1.18789542670764E-48,
-1.));
#43800=DIRECTION('ref_axis',(-4.33680868994202E-19,1.,-1.18789542670764E-48));
#43801=DIRECTION('',(-5.15167520928809E-67,1.18789542670764E-48,1.));
#43802=DIRECTION('center_axis',(5.15167520928809E-67,-1.18789542670764E-48,
-1.));
#43803=DIRECTION('ref_axis',(0.,1.,0.));
#43804=DIRECTION('center_axis',(5.15167520928809E-67,-1.18789542670764E-48,
-1.));
#43805=DIRECTION('ref_axis',(-4.33680868994202E-19,1.,-1.18789542670764E-48));
#43806=DIRECTION('center_axis',(-1.,0.,-5.15167520928809E-67));
#43807=DIRECTION('ref_axis',(0.,-1.,0.));
#43808=DIRECTION('center_axis',(5.15167520928809E-67,-1.18789542670764E-48,
-1.));
#43809=DIRECTION('ref_axis',(0.,1.,0.));
#43810=DIRECTION('center_axis',(1.,0.,5.15167520928809E-67));
#43811=DIRECTION('ref_axis',(0.,-1.,0.));
#43812=DIRECTION('center_axis',(5.15167520928809E-67,-1.18789542670764E-48,
-1.));
#43813=DIRECTION('ref_axis',(-4.33680868994202E-19,1.,-1.18789542670764E-48));
#43814=DIRECTION('center_axis',(5.15167520928809E-67,-1.18789542670764E-48,
-1.));
#43815=DIRECTION('ref_axis',(0.,1.,0.));
#43816=DIRECTION('center_axis',(-0.726741019926939,-0.686911553067863,9.06501466507717E-5));
#43817=DIRECTION('ref_axis',(0.686840456252471,-0.726663889286196,0.0144837723800636));
#43818=DIRECTION('center_axis',(5.15167520928809E-67,-1.18789542670764E-48,
-1.));
#43819=DIRECTION('ref_axis',(-4.33680868994202E-19,1.,-1.18789542670764E-48));
#43820=DIRECTION('center_axis',(0.0503838293498797,0.99872992276226,0.000105448247773495));
#43821=DIRECTION('ref_axis',(0.998655285166785,-0.0503813543085061,0.012220496982052));
#43822=DIRECTION('center_axis',(5.15167520928809E-67,-1.18789542670764E-48,
-1.));
#43823=DIRECTION('ref_axis',(0.,1.,0.));
#43824=DIRECTION('center_axis',(-0.0281309337977199,0.999604241409737,0.000105448247664664));
#43825=DIRECTION('ref_axis',(0.999529639708461,0.0281275452111534,0.0122204969076063));
#43826=DIRECTION('center_axis',(-0.670606260601171,-0.741813477246852,9.06501467500846E-5));
#43827=DIRECTION('ref_axis',(0.741736547998884,-0.670534945920291,0.0144837723805249));
#43828=DIRECTION('center_axis',(5.15167520928809E-67,-1.18789542670764E-48,
-1.));
#43829=DIRECTION('ref_axis',(-4.33680868994202E-19,1.,-1.18789542670764E-48));
#43830=DIRECTION('center_axis',(5.15167520928809E-67,-1.18789542670764E-48,
-1.));
#43831=DIRECTION('ref_axis',(0.,1.,0.));
#43832=DIRECTION('center_axis',(-0.106472260383779,0.994315667506771,0.000105448247699395));
#43833=DIRECTION('ref_axis',(0.99424156164256,0.106463029061011,0.0122204969504906));
#43834=DIRECTION('center_axis',(-0.610336990679751,-0.792141874660428,9.06501467512865E-5));
#43835=DIRECTION('ref_axis',(0.792059587274889,-0.610271931637935,0.0144837723275367));
#43836=DIRECTION('center_axis',(5.15167520928809E-67,-1.18789542670764E-48,
-1.));
#43837=DIRECTION('ref_axis',(-4.33680868994202E-19,1.,-1.18789542670764E-48));
#43838=DIRECTION('center_axis',(5.15167520928809E-67,-1.18789542670764E-48,
-1.));
#43839=DIRECTION('ref_axis',(0.,1.,0.));
#43840=DIRECTION('center_axis',(-0.18415715007879,0.982896806870144,0.000105448247763879));
#43841=DIRECTION('ref_axis',(0.982823653730846,0.18414213293402,0.0122204969481005));
#43842=DIRECTION('center_axis',(-0.546304790252955,-0.837586454002944,9.06501468511952E-5));
#43843=DIRECTION('ref_axis',(0.837499315807933,-0.546246387960026,0.0144837723631749));
#43844=DIRECTION('center_axis',(5.15167520928809E-67,-1.18789542670764E-48,
-1.));
#43845=DIRECTION('ref_axis',(-4.33680868994202E-19,1.,-1.18789542670764E-48));
#43846=DIRECTION('center_axis',(5.15167520928809E-67,-1.18789542670764E-48,
-1.));
#43847=DIRECTION('ref_axis',(0.,1.,0.));
#43848=DIRECTION('center_axis',(-0.260706649705391,0.965418060572754,0.000105448247684059));
#43849=DIRECTION('ref_axis',(0.965346311171948,0.260685939324359,0.0122204969329739));
#43850=DIRECTION('center_axis',(-0.478904439129961,-0.877867034330466,9.06501466909999E-5));
#43851=DIRECTION('ref_axis',(0.877775582562065,-0.478853053655646,0.0144837723846339));
#43852=DIRECTION('center_axis',(5.15167520928809E-67,-1.18789542670764E-48,
-1.));
#43853=DIRECTION('ref_axis',(-4.33680868994202E-19,1.,-1.18789542670764E-48));
#43854=DIRECTION('center_axis',(5.15167520928809E-67,-1.18789542670764E-48,
-1.));
#43855=DIRECTION('ref_axis',(0.,1.,0.));
#43856=DIRECTION('center_axis',(-0.33564880614276,0.941987190897842,0.000105448247631265));
#43857=DIRECTION('ref_axis',(0.941917287593993,0.335622530211717,0.0122204969563928));
#43858=DIRECTION('center_axis',(-0.408551482887427,-0.912735272471178,9.06501467675252E-5));
#43859=DIRECTION('ref_axis',(0.91264007095957,-0.408507431040139,0.0144837724331839));
#43860=DIRECTION('center_axis',(5.15167520928809E-67,-1.18789542670764E-48,
-1.));
#43861=DIRECTION('ref_axis',(-4.33680868994202E-19,1.,-1.18789542670764E-48));
#43862=DIRECTION('center_axis',(5.15167520928809E-67,-1.18789542670764E-48,
-1.));
#43863=DIRECTION('ref_axis',(0.,1.,0.));
#43864=DIRECTION('center_axis',(-0.408521576075341,0.912748656948662,0.000105448247753309));
#43865=DIRECTION('ref_axis',(0.912681030719062,0.40848989659417,0.0122204969651243));
#43866=DIRECTION('center_axis',(-0.335679670896088,-0.941976194141681,9.06501466394305E-5));
#43867=DIRECTION('ref_axis',(0.941877829837658,-0.335643224270894,0.0144837723450194));
#43868=DIRECTION('center_axis',(5.15167520928809E-67,-1.18789542670764E-48,
-1.));
#43869=DIRECTION('ref_axis',(-4.33680868994202E-19,1.,-1.18789542670764E-48));
#43870=DIRECTION('center_axis',(5.15167520928809E-67,-1.18789542670764E-48,
-1.));
#43871=DIRECTION('ref_axis',(0.,1.,0.));
#43872=DIRECTION('center_axis',(-0.478875674645407,0.877882724009063,0.000105448247283112));
#43873=DIRECTION('ref_axis',(0.877817791790398,0.478838786927794,0.012220497115417));
#43874=DIRECTION('center_axis',(-0.260738282108194,-0.965409519336649,9.06501468435925E-5));
#43875=DIRECTION('ref_axis',(0.965308598687812,-0.260709665410158,0.0144837723364994));
#43876=DIRECTION('center_axis',(5.15167520928809E-67,-1.18789542670764E-48,
-1.));
#43877=DIRECTION('ref_axis',(-4.33680868994202E-19,1.,-1.18789542670764E-48));
#43878=DIRECTION('center_axis',(5.15167520928809E-67,-1.18789542670764E-48,
-1.));
#43879=DIRECTION('ref_axis',(0.,1.,0.));
#43880=DIRECTION('center_axis',(-0.546277345437336,0.837604352151184,0.000105448247639474));
#43881=DIRECTION('ref_axis',(0.837542514276272,0.546235476910692,0.0122204968773897));
#43882=DIRECTION('center_axis',(-0.184189355107295,-0.982890773813505,9.06501468099581E-5));
#43883=DIRECTION('ref_axis',(0.982787919029019,-0.184168744767822,0.0144837723419927));
#43884=DIRECTION('center_axis',(5.15167520928809E-67,-1.18789542670764E-48,
-1.));
#43885=DIRECTION('ref_axis',(-4.33680868994202E-19,1.,-1.18789542670764E-48));
#43886=DIRECTION('center_axis',(5.15167520928809E-67,-1.18789542670764E-48,
-1.));
#43887=DIRECTION('ref_axis',(0.,1.,0.));
#43888=DIRECTION('center_axis',(-0.610311034740724,0.792161870929404,0.000105448247072483));
#43889=DIRECTION('ref_axis',(0.792103508642798,0.610264443533926,0.0122204972891987));
#43890=DIRECTION('center_axis',(-0.106504839483277,-0.994312179825427,9.06501466463657E-5));
#43891=DIRECTION('ref_axis',(0.994208025037708,-0.106492362571804,0.014483772453865));
#43892=DIRECTION('center_axis',(5.15167520928809E-67,-1.18789542670764E-48,
-1.));
#43893=DIRECTION('ref_axis',(-4.33680868994202E-19,1.,-1.18789542670764E-48));
#43894=DIRECTION('center_axis',(5.15167520928809E-67,-1.18789542670764E-48,
-1.));
#43895=DIRECTION('ref_axis',(0.,1.,0.));
#43896=DIRECTION('center_axis',(-0.670581953563772,0.74183544835446,0.000105448247723866));
#43897=DIRECTION('ref_axis',(0.741780921486778,0.670530926933108,0.012220496898794));
#43898=DIRECTION('center_axis',(-0.0281636861068304,-0.999603320606443,
9.06501467794172E-5));
#43899=DIRECTION('ref_axis',(0.999498507966719,-0.0281594195479949,0.0144837724030356));
#43900=DIRECTION('center_axis',(5.15167520928809E-67,-1.18789542670764E-48,
-1.));
#43901=DIRECTION('ref_axis',(-4.33680868994202E-19,1.,-1.18789542670764E-48));
#43902=DIRECTION('center_axis',(5.15167520928809E-67,-1.18789542670764E-48,
-1.));
#43903=DIRECTION('ref_axis',(0.,1.,0.));
#43904=DIRECTION('center_axis',(-0.726718511653027,0.686935363554299,0.000105448247728815));
#43905=DIRECTION('ref_axis',(0.686885008277766,0.726663364191397,0.0122204969332444));
#43906=DIRECTION('center_axis',(0.050351105759542,-0.998731574514065,9.06501467573609E-5));
#43907=DIRECTION('ref_axis',(0.998626750226961,0.0503471356610921,0.014483772362966));
#43908=DIRECTION('center_axis',(5.15167520928809E-67,-1.18789542670764E-48,
-1.));
#43909=DIRECTION('ref_axis',(-4.33680868994202E-19,1.,-1.18789542670764E-48));
#43910=DIRECTION('center_axis',(5.15167520928809E-67,-1.18789542670764E-48,
-1.));
#43911=DIRECTION('ref_axis',(0.,1.,0.));
#43912=DIRECTION('center_axis',(-0.778374608459537,0.627800093808634,0.000105448247783041));
#43913=DIRECTION('ref_axis',(0.627754220580437,0.778315680169477,0.01222049695274));
#43914=DIRECTION('center_axis',(0.128555466315269,-0.991702316152894,9.06501465984867E-5));
#43915=DIRECTION('ref_axis',(0.99159812649388,0.128543284036463,0.0144837724004731));
#43916=DIRECTION('center_axis',(5.15167520928809E-67,-1.18789542670764E-48,
-1.));
#43917=DIRECTION('ref_axis',(-4.33680868994202E-19,1.,-1.18789542670764E-48));
#43918=DIRECTION('center_axis',(5.15167520928809E-67,-1.18789542670764E-48,
-1.));
#43919=DIRECTION('ref_axis',(0.,1.,0.));
#43920=DIRECTION('center_axis',(-0.825231766969855,0.564794227718802,0.000105448247237627));
#43921=DIRECTION('ref_axis',(0.564753119361559,0.825169421162197,0.0122204971352771));
#43922=DIRECTION('center_axis',(0.205967239672467,-0.97855888323813,9.06501466256469E-5));
#43923=DIRECTION('ref_axis',(0.978455970572454,0.205946920321296,0.0144837723432324));
#43924=DIRECTION('center_axis',(5.15167520928809E-67,-1.18789542670764E-48,
-1.));
#43925=DIRECTION('ref_axis',(-4.33680868994202E-19,1.,-1.18789542670764E-48));
#43926=DIRECTION('center_axis',(5.15167520928809E-67,-1.18789542670764E-48,
-1.));
#43927=DIRECTION('ref_axis',(0.,1.,0.));
#43928=DIRECTION('center_axis',(-0.867001097222074,0.498306217396881,0.00010544824406792));
#43929=DIRECTION('ref_axis',(0.498270127350421,0.866935718266621,0.0122204985059196));
#43930=DIRECTION('center_axis',(0.282109156506117,-0.959382309404316,9.06501467341775E-5));
#43931=DIRECTION('ref_axis',(0.959281308220891,0.282080825357731,0.0144837724201092));
#43932=DIRECTION('center_axis',(5.15167520928809E-67,-1.18789542670764E-48,
-1.));
#43933=DIRECTION('ref_axis',(-4.33680868994202E-19,1.,-1.18789542670764E-48));
#43934=DIRECTION('center_axis',(5.15167520928809E-67,-1.18789542670764E-48,
-1.));
#43935=DIRECTION('ref_axis',(0.,1.,0.));
#43936=DIRECTION('center_axis',(-0.903425077395399,0.428745983554114,0.00010544824771057));
#43937=DIRECTION('ref_axis',(0.42871513434286,0.903357068405985,0.0122204969754959));
#43938=DIRECTION('center_axis',(0.356511776578972,-0.934290824606052,9.06501467185522E-5));
#43939=DIRECTION('ref_axis',(0.934192357612503,0.356475608304786,0.0144837723720686));
#43940=DIRECTION('center_axis',(5.15167520928809E-67,-1.18789542670764E-48,
-1.));
#43941=DIRECTION('ref_axis',(-4.33680868994202E-19,1.,-1.18789542670764E-48));
#43942=DIRECTION('center_axis',(5.15167520928809E-67,-1.18789542670764E-48,
-1.));
#43943=DIRECTION('ref_axis',(0.,1.,0.));
#43944=DIRECTION('center_axis',(-0.934279141551227,0.35654238814336,0.000105448247725771));
#43945=DIRECTION('ref_axis',(0.356516969954114,0.934208921810617,0.0122204968876431));
#43946=DIRECTION('center_axis',(0.428716382996855,-0.903439126190938,9.06501466905075E-5));
#43947=DIRECTION('ref_axis',(0.903343800467886,0.428672600585895,0.0144837724078269));
#43948=DIRECTION('center_axis',(5.15167520928809E-67,-1.18789542670764E-48,
-1.));
#43949=DIRECTION('ref_axis',(-4.33680868994202E-19,1.,-1.18789542670764E-48));
#43950=DIRECTION('center_axis',(5.15167520928809E-67,-1.18789542670764E-48,
-1.));
#43951=DIRECTION('ref_axis',(0.,1.,0.));
#43952=DIRECTION('center_axis',(-0.959373064120116,0.282140590347166,0.000105448247704078));
#43953=DIRECTION('ref_axis',(0.282120759890668,0.959301066553995,0.0122204970062476));
#43954=DIRECTION('center_axis',(0.498277810351468,-0.867017425138559,9.06501469271671E-5));
#43955=DIRECTION('ref_axis',(0.86692582840188,0.498226683737388,0.0144837723593644));
#43956=DIRECTION('center_axis',(5.15167520928809E-67,-1.18789542670764E-48,
-1.));
#43957=DIRECTION('ref_axis',(-4.33680868994202E-19,1.,-1.18789542670764E-48));
#43958=DIRECTION('center_axis',(5.15167520928809E-67,-1.18789542670764E-48,
-1.));
#43959=DIRECTION('ref_axis',(0.,1.,0.));
#43960=DIRECTION('center_axis',(-0.978552132724721,0.205999301990486,0.000105448247790145));
#43961=DIRECTION('ref_axis',(0.205985181528783,0.978478801224291,0.0122204969305395));
#43962=DIRECTION('center_axis',(0.564767189310343,-0.825250273348059,9.06501467424166E-5));
#43963=DIRECTION('ref_axis',(0.825162970321744,0.56470903370561,0.0144837723356968));
#43964=DIRECTION('center_axis',(5.15167520928809E-67,-1.18789542670764E-48,
-1.));
#43965=DIRECTION('ref_axis',(-4.33680868994202E-19,1.,-1.18789542670764E-48));
#43966=DIRECTION('center_axis',(5.15167520928809E-67,-1.18789542670764E-48,
-1.));
#43967=DIRECTION('ref_axis',(0.,1.,0.));
#43968=DIRECTION('center_axis',(-0.991698102029505,0.128587959435343,0.000105448247905715));
#43969=DIRECTION('ref_axis',(0.12857963602553,0.991623888707005,0.0122204969268892));
#43970=DIRECTION('center_axis',(0.627774590743107,-0.778395179198763,9.06501466692162E-5));
#43971=DIRECTION('ref_axis',(0.778312708134479,0.627709764696018,0.0144837723553914));
#43972=DIRECTION('center_axis',(5.15167520928809E-67,-1.18789542670764E-48,
-1.));
#43973=DIRECTION('ref_axis',(-4.33680868994202E-19,1.,-1.18789542670764E-48));
#43974=DIRECTION('center_axis',(5.15167520928809E-67,-1.18789542670764E-48,
-1.));
#43975=DIRECTION('ref_axis',(0.,1.,0.));
#43976=DIRECTION('center_axis',(-0.998729922762266,0.05038382934976,0.000105448247701369));
#43977=DIRECTION('ref_axis',(0.0503813543083786,0.998655285166624,0.0122204969957313));
#43978=DIRECTION('center_axis',(0.686911553067687,-0.726741019927105,9.06501465529425E-5));
#43979=DIRECTION('ref_axis',(0.726663889286156,0.686840456252101,0.0144837723995786));
#43980=DIRECTION('center_axis',(5.15167520928809E-67,-1.18789542670764E-48,
-1.));
#43981=DIRECTION('ref_axis',(-4.33680868994202E-19,1.,-1.18789542670764E-48));
#43982=DIRECTION('center_axis',(5.15167520928809E-67,-1.18789542670764E-48,
-1.));
#43983=DIRECTION('ref_axis',(0.,1.,0.));
#43984=DIRECTION('center_axis',(-0.999604241409733,-0.0281309337978441,
0.000105448247608528));
#43985=DIRECTION('ref_axis',(0.0281275452112647,-0.999529639708088,-0.0122204969378127));
#43986=DIRECTION('center_axis',(0.741813477246663,-0.67060626060138,9.06501466416355E-5));
#43987=DIRECTION('ref_axis',(0.670534945920398,0.741736547998582,0.0144837723910712));
#43988=DIRECTION('center_axis',(5.15167520928809E-67,-1.18789542670764E-48,
-1.));
#43989=DIRECTION('ref_axis',(-4.33680868994202E-19,1.,-1.18789542670764E-48));
#43990=DIRECTION('center_axis',(5.15167520928809E-67,-1.18789542670764E-48,
-1.));
#43991=DIRECTION('ref_axis',(0.,1.,0.));
#43992=DIRECTION('center_axis',(-0.994315667506803,-0.106472260383486,0.000105448247832577));
#43993=DIRECTION('ref_axis',(0.10646302906079,-0.994241561643227,-0.0122204968981425));
#43994=DIRECTION('center_axis',(0.792141874660394,-0.610336990679795,9.06501467163515E-5));
#43995=DIRECTION('ref_axis',(0.610271931637984,0.792059587274861,0.0144837723269713));
#43996=DIRECTION('center_axis',(5.15167520928809E-67,-1.18789542670764E-48,
-1.));
#43997=DIRECTION('ref_axis',(-4.33680868994202E-19,1.,-1.18789542670764E-48));
#43998=DIRECTION('center_axis',(5.15167520928809E-67,-1.18789542670764E-48,
-1.));
#43999=DIRECTION('ref_axis',(0.,1.,0.));
#44000=DIRECTION('center_axis',(-0.982896806870098,-0.184157150079038,0.000105448247610839));
#44001=DIRECTION('ref_axis',(0.184142132934261,-0.982823653730751,-0.0122204969521754));
#44002=DIRECTION('center_axis',(0.837586454002892,-0.546304790253034,9.06501468389122E-5));
#44003=DIRECTION('ref_axis',(0.546246387959946,0.837499315807641,0.014483772383082));
#44004=DIRECTION('center_axis',(5.15167520928809E-67,-1.18789542670764E-48,
-1.));
#44005=DIRECTION('ref_axis',(-4.33680868994202E-19,1.,-1.18789542670764E-48));
#44006=DIRECTION('center_axis',(5.15167520928809E-67,-1.18789542670764E-48,
-1.));
#44007=DIRECTION('ref_axis',(0.,1.,0.));
#44008=DIRECTION('center_axis',(-0.965418060572767,-0.260706649705342,0.000105448247695262));
#44009=DIRECTION('ref_axis',(0.260685939324476,-0.965346311172558,-0.0122204968822783));
#44010=DIRECTION('center_axis',(0.877867034330398,-0.478904439130086,9.06501466177592E-5));
#44011=DIRECTION('ref_axis',(0.478853053655353,0.877775582561241,0.0144837724443041));
#44012=DIRECTION('center_axis',(5.15167520928809E-67,-1.18789542670764E-48,
-1.));
#44013=DIRECTION('ref_axis',(-4.33680868994202E-19,1.,-1.18789542670764E-48));
#44014=DIRECTION('center_axis',(5.15167520928809E-67,-1.18789542670764E-48,
-1.));
#44015=DIRECTION('ref_axis',(0.,1.,0.));
#44016=DIRECTION('center_axis',(-0.941987190897914,-0.335648806142557,0.000105448247712849));
#44017=DIRECTION('ref_axis',(0.335622530211483,-0.941917287593983,-0.0122204969636003));
#44018=DIRECTION('center_axis',(0.912735272471151,-0.408551482887487,9.06501467033935E-5));
#44019=DIRECTION('ref_axis',(0.408507431040848,0.912640070960968,0.0144837723251257));
#44020=DIRECTION('center_axis',(5.15167520928809E-67,-1.18789542670764E-48,
-1.));
#44021=DIRECTION('ref_axis',(-4.33680868994202E-19,1.,-1.18789542670764E-48));
#44022=DIRECTION('center_axis',(5.15167520928809E-67,-1.18789542670764E-48,
-1.));
#44023=DIRECTION('ref_axis',(0.,1.,0.));
#44024=DIRECTION('center_axis',(-0.912748656948201,-0.408521576076371,0.000105448247247158));
#44025=DIRECTION('ref_axis',(0.408489896594259,-0.912681030716532,-0.012220497151094));
#44026=DIRECTION('center_axis',(0.941976194141716,-0.335679670895989,9.06501466623777E-5));
#44027=DIRECTION('ref_axis',(0.335643224270751,0.941877829837572,0.0144837723539316));
#44028=DIRECTION('center_axis',(5.15167520928809E-67,-1.18789542670764E-48,
-1.));
#44029=DIRECTION('ref_axis',(-4.33680868994202E-19,1.,-1.18789542670764E-48));
#44030=DIRECTION('center_axis',(5.15167520928809E-67,-1.18789542670764E-48,
-1.));
#44031=DIRECTION('ref_axis',(0.,1.,0.));
#44032=DIRECTION('center_axis',(-0.877882724009451,-0.478875674644697,0.000105448247674909));
#44033=DIRECTION('ref_axis',(0.478838786928496,-0.877817791793333,-0.0122204968770904));
#44034=DIRECTION('center_axis',(0.965409519336493,-0.26073828210877,9.06501465579451E-5));
#44035=DIRECTION('ref_axis',(0.260709665410522,0.965308598686875,0.0144837723924504));
#44036=DIRECTION('center_axis',(5.15167520928809E-67,-1.18789542670764E-48,
-1.));
#44037=DIRECTION('ref_axis',(-4.33680868994202E-19,1.,-1.18789542670764E-48));
#44038=DIRECTION('center_axis',(5.15167520928809E-67,-1.18789542670764E-48,
-1.));
#44039=DIRECTION('ref_axis',(0.,1.,0.));
#44040=DIRECTION('center_axis',(-0.837604352151306,-0.546277345437149,0.00010544824776483));
#44041=DIRECTION('ref_axis',(0.546235476910197,-0.837542514275933,-0.0122204969227218));
#44042=DIRECTION('center_axis',(0.982890773813463,-0.184189355107518,9.06501466980053E-5));
#44043=DIRECTION('ref_axis',(0.184168744767822,0.982787919027818,0.0144837724235038));
#44044=DIRECTION('center_axis',(5.15167520928809E-67,-1.18789542670764E-48,
-1.));
#44045=DIRECTION('ref_axis',(-4.33680868994202E-19,1.,-1.18789542670764E-48));
#44046=DIRECTION('center_axis',(5.15167520928809E-67,-1.18789542670764E-48,
-1.));
#44047=DIRECTION('ref_axis',(0.,1.,0.));
#44048=DIRECTION('center_axis',(-0.792161870930109,-0.610311034739809,0.000105448247597277));
#44049=DIRECTION('ref_axis',(0.610264443535208,-0.792103508646315,-0.0122204969972532));
#44050=DIRECTION('center_axis',(0.994312179825469,-0.106504839482882,9.06501468290203E-5));
#44051=DIRECTION('ref_axis',(0.106492362571566,0.994208025039157,0.0144837723561435));
#44052=DIRECTION('center_axis',(5.15167520928809E-67,-1.18789542670764E-48,
-1.));
#44053=DIRECTION('ref_axis',(-4.33680868994202E-19,1.,-1.18789542670764E-48));
#44054=DIRECTION('center_axis',(5.15167520928809E-67,-1.18789542670764E-48,
-1.));
#44055=DIRECTION('ref_axis',(0.,1.,0.));
#44056=DIRECTION('center_axis',(-0.741835448354634,-0.670581953563579,0.000105448247853962));
#44057=DIRECTION('ref_axis',(0.67053092693267,-0.741780921486687,-0.0122204969283275));
#44058=DIRECTION('center_axis',(0.99960332060645,-0.0281636861065795,9.06501468718404E-5));
#44059=DIRECTION('ref_axis',(0.0281594195477731,0.999498507967606,0.014483772342229));
#44060=DIRECTION('center_axis',(5.15167520928809E-67,-1.18789542670764E-48,
-1.));
#44061=DIRECTION('ref_axis',(-4.33680868994202E-19,1.,-1.18789542670764E-48));
#44062=DIRECTION('center_axis',(5.15167520928809E-67,-1.18789542670764E-48,
-1.));
#44063=DIRECTION('ref_axis',(0.,1.,0.));
#44064=DIRECTION('center_axis',(-0.686935363552547,-0.726718511654683,0.000105448246665782));
#44065=DIRECTION('ref_axis',(0.726663364188996,-0.686885008272227,-0.0122204973873402));
#44066=DIRECTION('center_axis',(0.998731574514055,0.0503511057597249,9.06501467982717E-5));
#44067=DIRECTION('ref_axis',(0.050347135661256,-0.998626750226507,-0.0144837723936806));
#44068=DIRECTION('center_axis',(5.15167520928809E-67,-1.18789542670764E-48,
-1.));
#44069=DIRECTION('ref_axis',(-4.33680868994202E-19,1.,-1.18789542670764E-48));
#44070=DIRECTION('center_axis',(5.15167520928809E-67,-1.18789542670764E-48,
-1.));
#44071=DIRECTION('ref_axis',(0.,1.,0.));
#44072=DIRECTION('center_axis',(-0.627800093808639,-0.778374608459533,0.000105448247779514));
#44073=DIRECTION('ref_axis',(0.778315680170178,-0.627754220581,-0.0122204968791585));
#44074=DIRECTION('center_axis',(0.991702316152886,0.12855546631533,9.06501466251883E-5));
#44075=DIRECTION('ref_axis',(0.128543284036466,-0.991598126493403,-0.0144837724330683));
#44076=DIRECTION('center_axis',(5.15167520928809E-67,-1.18789542670764E-48,
-1.));
#44077=DIRECTION('ref_axis',(-4.33680868994202E-19,1.,-1.18789542670764E-48));
#44078=DIRECTION('center_axis',(5.15167520928809E-67,-1.18789542670764E-48,
-1.));
#44079=DIRECTION('ref_axis',(0.,1.,0.));
#44080=DIRECTION('center_axis',(-0.564794227719968,-0.825231766969057,0.000105448247863909));
#44081=DIRECTION('ref_axis',(0.825169421163414,-0.564753119364088,-0.0122204969362205));
#44082=DIRECTION('center_axis',(0.978558883238036,0.205967239672914,9.06501468463484E-5));
#44083=DIRECTION('ref_axis',(0.205946920321936,-0.978455970573291,-0.014483772277592));
#44084=DIRECTION('center_axis',(5.15167520928809E-67,-1.18789542670764E-48,
-1.));
#44085=DIRECTION('ref_axis',(-4.33680868994202E-19,1.,-1.18789542670764E-48));
#44086=DIRECTION('center_axis',(5.15167520928809E-67,-1.18789542670764E-48,
-1.));
#44087=DIRECTION('ref_axis',(0.,1.,0.));
#44088=DIRECTION('center_axis',(-0.498306217403848,-0.86700109721807,0.000105448247661773));
#44089=DIRECTION('ref_axis',(0.866935718279092,-0.498270127366718,-0.0122204969566953));
#44090=DIRECTION('center_axis',(0.959382309404258,0.282109156506314,9.06501467982869E-5));
#44091=DIRECTION('ref_axis',(0.282080825358155,-0.959281308221622,-0.014483772363392));
#44092=DIRECTION('center_axis',(5.15167520928809E-67,-1.18789542670764E-48,
-1.));
#44093=DIRECTION('ref_axis',(-4.33680868994202E-19,1.,-1.18789542670764E-48));
#44094=DIRECTION('center_axis',(5.15167520928809E-67,-1.18789542670764E-48,
-1.));
#44095=DIRECTION('ref_axis',(0.,1.,0.));
#44096=DIRECTION('center_axis',(-0.428745983554159,-0.903425077395378,0.000105448247692435));
#44097=DIRECTION('ref_axis',(0.903357068405516,-0.428715134342697,-0.0122204970158381));
#44098=DIRECTION('center_axis',(0.934290824605943,0.356511776579256,9.06501468588022E-5));
#44099=DIRECTION('ref_axis',(0.35647560830508,-0.934192357612417,-0.0144837723703894));
#44100=DIRECTION('center_axis',(5.15167520928809E-67,-1.18789542670764E-48,
-1.));
#44101=DIRECTION('ref_axis',(-4.33680868994202E-19,1.,-1.18789542670764E-48));
#44102=DIRECTION('center_axis',(5.15167520928809E-67,-1.18789542670764E-48,
-1.));
#44103=DIRECTION('ref_axis',(0.,1.,0.));
#44104=DIRECTION('center_axis',(-0.356542388142294,-0.934279141551633,0.000105448247232403));
#44105=DIRECTION('ref_axis',(0.934208921807365,-0.356516969951681,-0.0122204972072322));
#44106=DIRECTION('center_axis',(0.903439126190767,0.428716382997215,9.06501468179925E-5));
#44107=DIRECTION('ref_axis',(0.428672600586429,-0.903343800468082,-0.0144837723797852));
#44108=DIRECTION('center_axis',(5.15167520928809E-67,-1.18789542670764E-48,
-1.));
#44109=DIRECTION('ref_axis',(-4.33680868994202E-19,1.,-1.18789542670764E-48));
#44110=DIRECTION('center_axis',(5.15167520928809E-67,-1.18789542670764E-48,
-1.));
#44111=DIRECTION('ref_axis',(0.,1.,0.));
#44112=DIRECTION('center_axis',(-0.282140590347279,-0.959373064120083,0.000105448247741099));
#44113=DIRECTION('ref_axis',(0.959301066555032,-0.282120759891086,-0.012220496915153));
#44114=DIRECTION('center_axis',(0.867017425138588,0.498277810351419,9.06501468672452E-5));
#44115=DIRECTION('ref_axis',(0.498226683737162,-0.866925828401598,-0.0144837723840689));
#44116=DIRECTION('center_axis',(5.15167520928809E-67,-1.18789542670764E-48,
-1.));
#44117=DIRECTION('ref_axis',(-4.33680868994202E-19,1.,-1.18789542670764E-48));
#44118=DIRECTION('center_axis',(5.15167520928809E-67,-1.18789542670764E-48,
-1.));
#44119=DIRECTION('ref_axis',(0.,1.,0.));
#44120=DIRECTION('center_axis',(-0.20599930198994,-0.978552132724836,0.000105448247552452));
#44121=DIRECTION('ref_axis',(0.97847880122346,-0.205985181528044,-0.0122204970095074));
#44122=DIRECTION('center_axis',(0.825250273348004,0.564767189310424,9.06501467639861E-5));
#44123=DIRECTION('ref_axis',(0.56470903370563,-0.825162970321598,-0.0144837723432248));
#44124=DIRECTION('center_axis',(5.15167520928809E-67,-1.18789542670764E-48,
-1.));
#44125=DIRECTION('ref_axis',(-4.33680868994202E-19,1.,-1.18789542670764E-48));
#44126=DIRECTION('center_axis',(5.15167520928809E-67,-1.18789542670764E-48,
-1.));
#44127=DIRECTION('ref_axis',(0.,1.,0.));
#44128=DIRECTION('center_axis',(-0.128587959431095,-0.991698102030056,0.000105448246015545));
#44129=DIRECTION('ref_axis',(0.991623888697772,-0.128579636020076,-0.0122204977334817));
#44130=DIRECTION('center_axis',(0.778395179198649,0.627774590743249,9.06501467187627E-5));
#44131=DIRECTION('ref_axis',(0.62770976469618,-0.778312708134389,-0.0144837723532511));
#44132=DIRECTION('center_axis',(5.15167520928809E-67,-1.18789542670764E-48,
-1.));
#44133=DIRECTION('ref_axis',(-4.33680868994202E-19,1.,-1.18789542670764E-48));
#44134=DIRECTION('center_axis',(5.15167520928809E-67,-1.18789542670764E-48,
-1.));
#44135=DIRECTION('ref_axis',(0.,1.,0.));
#44136=DIRECTION('center_axis',(-0.0503838293498799,-0.99872992276226,0.000105448247790322));
#44137=DIRECTION('ref_axis',(0.998655285167012,-0.050381354308516,-0.0122204969634886));
#44138=DIRECTION('center_axis',(0.726741019926698,0.686911553068118,9.06501468063716E-5));
#44139=DIRECTION('ref_axis',(0.686840456253071,-0.726663889286322,-0.0144837723452766));
#44140=DIRECTION('center_axis',(5.15167520928809E-67,-1.18789542670764E-48,
-1.));
#44141=DIRECTION('ref_axis',(-4.33680868994202E-19,1.,-1.18789542670764E-48));
#44142=DIRECTION('center_axis',(5.15167520928809E-67,-1.18789542670764E-48,
-1.));
#44143=DIRECTION('ref_axis',(0.,1.,0.));
#44144=DIRECTION('center_axis',(0.0281309337977714,-0.999604241409735,0.000105448247661813));
#44145=DIRECTION('ref_axis',(0.999529639707556,0.0281275452111717,-0.0122204969816086));
#44146=DIRECTION('center_axis',(0.670606260601294,0.741813477246741,9.06501466782892E-5));
#44147=DIRECTION('ref_axis',(0.741736547997904,-0.67053494591962,-0.0144837724617815));
#44148=DIRECTION('center_axis',(5.15167520928809E-67,-1.18789542670764E-48,
-1.));
#44149=DIRECTION('ref_axis',(-4.33680868994202E-19,1.,-1.18789542670764E-48));
#44150=DIRECTION('center_axis',(5.15167520928809E-67,-1.18789542670764E-48,
-1.));
#44151=DIRECTION('ref_axis',(0.,1.,0.));
#44152=DIRECTION('center_axis',(0.106472260384112,-0.994315667506736,0.000105448247531298));
#44153=DIRECTION('ref_axis',(0.994241561642015,0.106463029061287,-0.01222049699245));
#44154=DIRECTION('center_axis',(0.610336990679746,0.792141874660432,9.06501467541659E-5));
#44155=DIRECTION('ref_axis',(0.792059587274579,-0.610271931637685,-0.0144837723550388));
#44156=DIRECTION('center_axis',(5.15167520928809E-67,-1.18789542670764E-48,
-1.));
#44157=DIRECTION('ref_axis',(-4.33680868994202E-19,1.,-1.18789542670764E-48));
#44158=DIRECTION('center_axis',(5.15167520928809E-67,-1.18789542670764E-48,
-1.));
#44159=DIRECTION('ref_axis',(0.,1.,0.));
#44160=DIRECTION('center_axis',(0.184157150078655,-0.982896806870169,0.000105448247826086));
#44161=DIRECTION('ref_axis',(0.982823653731041,0.184142132933918,-0.01222049693405));
#44162=DIRECTION('center_axis',(0.546304790253063,0.837586454002874,9.06501468026834E-5));
#44163=DIRECTION('ref_axis',(0.837499315807096,-0.546246387959628,-0.0144837724265968));
#44164=DIRECTION('center_axis',(5.15167520928809E-67,-1.18789542670764E-48,
-1.));
#44165=DIRECTION('ref_axis',(-4.33680868994202E-19,1.,-1.18789542670764E-48));
#44166=DIRECTION('center_axis',(5.15167520928809E-67,-1.18789542670764E-48,
-1.));
#44167=DIRECTION('ref_axis',(0.,1.,0.));
#44168=DIRECTION('center_axis',(0.260706649723291,-0.965418060567921,0.000105448239312411));
#44169=DIRECTION('ref_axis',(0.965346311124436,0.260685939330442,-0.0122205005564138));
#44170=DIRECTION('center_axis',(0.478904439129984,0.877867034330454,9.06501466836614E-5));
#44171=DIRECTION('ref_axis',(0.877775582561938,-0.478853053655605,-0.0144837723936657));
#44172=DIRECTION('center_axis',(5.15167520928809E-67,-1.18789542670764E-48,
-1.));
#44173=DIRECTION('ref_axis',(-4.33680868994202E-19,1.,-1.18789542670764E-48));
#44174=DIRECTION('center_axis',(5.15167520928809E-67,-1.18789542670764E-48,
-1.));
#44175=DIRECTION('ref_axis',(0.,1.,0.));
#44176=DIRECTION('center_axis',(0.335648806142683,-0.941987190897869,0.000105448247681778));
#44177=DIRECTION('ref_axis',(0.941917287594608,0.335622530211854,-0.012220496905163));
#44178=DIRECTION('center_axis',(0.408551482887321,0.912735272471225,9.06501468104788E-5));
#44179=DIRECTION('ref_axis',(0.912640070960436,-0.408507431040405,-0.014483772371131));
#44180=DIRECTION('center_axis',(5.15167520928809E-67,-1.18789542670764E-48,
-1.));
#44181=DIRECTION('ref_axis',(-4.33680868994202E-19,1.,-1.18789542670764E-48));
#44182=DIRECTION('center_axis',(5.15167520928809E-67,-1.18789542670764E-48,
-1.));
#44183=DIRECTION('ref_axis',(0.,1.,0.));
#44184=DIRECTION('center_axis',(0.408521576076219,-0.912748656948269,0.000105448247344423));
#44185=DIRECTION('ref_axis',(0.912681030717311,0.408489896594431,-0.0122204970871443));
#44186=DIRECTION('center_axis',(0.335679670895796,0.941976194141785,9.06501467685389E-5));
#44187=DIRECTION('ref_axis',(0.941877829836932,-0.335643224270299,-0.0144837724059784));
#44188=DIRECTION('center_axis',(5.15167520928809E-67,-1.18789542670764E-48,
-1.));
#44189=DIRECTION('ref_axis',(-4.33680868994202E-19,1.,-1.18789542670764E-48));
#44190=DIRECTION('center_axis',(5.15167520928809E-67,-1.18789542670764E-48,
-1.));
#44191=DIRECTION('ref_axis',(0.,1.,0.));
#44192=DIRECTION('center_axis',(0.478875674644822,-0.877882724009383,0.000105448247602163));
#44193=DIRECTION('ref_axis',(0.877817791792273,0.47883878692807,-0.0122204969699355));
#44194=DIRECTION('center_axis',(0.260738282108074,0.965409519336681,9.06501468936573E-5));
#44195=DIRECTION('ref_axis',(0.965308598687316,-0.260709665409891,-0.0144837723743816));
#44196=DIRECTION('center_axis',(5.15167520928809E-67,-1.18789542670764E-48,
-1.));
#44197=DIRECTION('ref_axis',(-4.33680868994202E-19,1.,-1.18789542670764E-48));
#44198=DIRECTION('center_axis',(5.15167520928809E-67,-1.18789542670764E-48,
-1.));
#44199=DIRECTION('ref_axis',(0.,1.,0.));
#44200=DIRECTION('center_axis',(0.546277345437349,-0.837604352151176,0.000105448247639465));
#44201=DIRECTION('ref_axis',(0.837542514275712,0.546235476910338,-0.0122204969316073));
#44202=DIRECTION('center_axis',(0.184189355107516,0.982890773813463,9.06501467024073E-5));
#44203=DIRECTION('ref_axis',(0.982787919028468,-0.184168744767946,-0.0144837723778112));
#44204=DIRECTION('center_axis',(5.15167520928809E-67,-1.18789542670764E-48,
-1.));
#44205=DIRECTION('ref_axis',(-4.33680868994202E-19,1.,-1.18789542670764E-48));
#44206=DIRECTION('center_axis',(5.15167520928809E-67,-1.18789542670764E-48,
-1.));
#44207=DIRECTION('ref_axis',(0.,1.,0.));
#44208=DIRECTION('center_axis',(0.610311034750668,-0.792161870921744,0.000105448241406271));
#44209=DIRECTION('ref_axis',(0.79210350861157,0.610264443525473,-0.0122204997355093));
#44210=DIRECTION('center_axis',(0.106504839483129,0.994312179825443,9.06501467375791E-5));
#44211=DIRECTION('ref_axis',(0.994208025038601,-0.106492362571754,-0.0144837723929676));
#44212=DIRECTION('center_axis',(5.15167520928809E-67,-1.18789542670764E-48,
-1.));
#44213=DIRECTION('ref_axis',(-4.33680868994202E-19,1.,-1.18789542670764E-48));
#44214=DIRECTION('center_axis',(5.15167520928809E-67,-1.18789542670764E-48,
-1.));
#44215=DIRECTION('ref_axis',(0.,1.,0.));
#44216=DIRECTION('center_axis',(0.670581953563674,-0.741835448354548,0.000105448247759945));
#44217=DIRECTION('ref_axis',(0.741780921486581,0.670530926932748,-0.0122204969305506));
#44218=DIRECTION('center_axis',(0.0281636861069903,0.999603320606438,9.06501466992701E-5));
#44219=DIRECTION('ref_axis',(0.999498507967367,-0.0281594195481785,-0.0144837723579484));
#44220=DIRECTION('center_axis',(5.15167520928809E-67,-1.18789542670764E-48,
-1.));
#44221=DIRECTION('ref_axis',(-4.33680868994202E-19,1.,-1.18789542670764E-48));
#44222=DIRECTION('center_axis',(5.15167520928809E-67,-1.18789542670764E-48,
-1.));
#44223=DIRECTION('ref_axis',(0.,1.,0.));
#44224=DIRECTION('center_axis',(0.726718511653026,-0.6869353635543,0.000105448247761845));
#44225=DIRECTION('ref_axis',(0.686885008277897,0.726663364191536,-0.0122204969175564));
#44226=DIRECTION('center_axis',(-0.0503511057596336,0.99873157451406,9.06501467774672E-5));
#44227=DIRECTION('ref_axis',(0.998626750226755,0.0503471356611751,-0.0144837723768601));
#44228=DIRECTION('center_axis',(5.15167520928809E-67,-1.18789542670764E-48,
-1.));
#44229=DIRECTION('ref_axis',(-4.33680868994202E-19,1.,-1.18789542670764E-48));
#44230=DIRECTION('center_axis',(5.15167520928809E-67,-1.18789542670764E-48,
-1.));
#44231=DIRECTION('ref_axis',(0.,1.,0.));
#44232=DIRECTION('center_axis',(0.778374608459656,-0.627800093808486,0.000105448247696036));
#44233=DIRECTION('ref_axis',(0.627754220580537,0.778315680169911,-0.0122204969200215));
#44234=DIRECTION('center_axis',(-0.128555466315276,0.991702316152893,9.06501466266556E-5));
#44235=DIRECTION('ref_axis',(0.991598126493641,0.128543284036441,-0.0144837724170315));
#44236=DIRECTION('center_axis',(5.15167520928809E-67,-1.18789542670764E-48,
-1.));
#44237=DIRECTION('ref_axis',(-4.33680868994202E-19,1.,-1.18789542670764E-48));
#44238=DIRECTION('center_axis',(5.15167520928809E-67,-1.18789542670764E-48,
-1.));
#44239=DIRECTION('ref_axis',(0.,1.,0.));
#44240=DIRECTION('center_axis',(0.825231766969182,-0.564794227719785,0.000105448247768853));
#44241=DIRECTION('ref_axis',(0.564753119363901,0.825169421163535,-0.0122204969367096));
#44242=DIRECTION('center_axis',(-0.205967239672835,0.978558883238052,9.06501467925213E-5));
#44243=DIRECTION('ref_axis',(0.978455970572528,0.205946920321698,-0.0144837723325158));
#44244=DIRECTION('center_axis',(5.15167520928809E-67,-1.18789542670764E-48,
-1.));
#44245=DIRECTION('ref_axis',(-4.33680868994202E-19,1.,-1.18789542670764E-48));
#44246=DIRECTION('center_axis',(5.15167520928809E-67,-1.18789542670764E-48,
-1.));
#44247=DIRECTION('ref_axis',(0.,1.,0.));
#44248=DIRECTION('center_axis',(0.867001097218019,-0.498306217403936,0.000105448247742928));
#44249=DIRECTION('ref_axis',(0.498270127367224,0.866935718279781,-0.0122204968872419));
#44250=DIRECTION('center_axis',(-0.282109156506148,0.959382309404307,9.06501467249393E-5));
#44251=DIRECTION('ref_axis',(0.959281308221143,0.282080825357837,-0.0144837724013445));
#44252=DIRECTION('center_axis',(5.15167520928809E-67,-1.18789542670764E-48,
-1.));
#44253=DIRECTION('ref_axis',(-4.33680868994202E-19,1.,-1.18789542670764E-48));
#44254=DIRECTION('center_axis',(5.15167520928809E-67,-1.18789542670764E-48,
-1.));
#44255=DIRECTION('ref_axis',(0.,1.,0.));
#44256=DIRECTION('center_axis',(0.903425077395463,-0.428745983553979,0.000105448247628158));
#44257=DIRECTION('ref_axis',(0.428715134343002,0.903357068406648,-0.0122204969215573));
#44258=DIRECTION('center_axis',(-0.356511776579108,0.934290824606,9.06501467950618E-5));
#44259=DIRECTION('ref_axis',(0.934192357613078,0.356475608305158,-0.0144837723258434));
#44260=DIRECTION('center_axis',(5.15167520928809E-67,-1.18789542670764E-48,
-1.));
#44261=DIRECTION('ref_axis',(-4.33680868994202E-19,1.,-1.18789542670764E-48));
#44262=DIRECTION('center_axis',(5.15167520928809E-67,-1.18789542670764E-48,
-1.));
#44263=DIRECTION('ref_axis',(0.,1.,0.));
#44264=DIRECTION('center_axis',(0.93427914155167,-0.356542388142199,0.000105448247170392));
#44265=DIRECTION('ref_axis',(0.356516969951772,0.934208921807903,-0.012220497163456));
#44266=DIRECTION('center_axis',(-0.428716382997142,0.903439126190801,9.06501468381065E-5));
#44267=DIRECTION('ref_axis',(0.903343800468038,0.42867260058632,-0.0144837723857595));
#44268=DIRECTION('center_axis',(5.15167520928809E-67,-1.18789542670764E-48,
-1.));
#44269=DIRECTION('ref_axis',(-4.33680868994202E-19,1.,-1.18789542670764E-48));
#44270=DIRECTION('center_axis',(5.15167520928809E-67,-1.18789542670764E-48,
-1.));
#44271=DIRECTION('ref_axis',(0.,1.,0.));
#44272=DIRECTION('center_axis',(0.959373064120116,-0.282140590347164,0.000105448247729292));
#44273=DIRECTION('ref_axis',(0.282120759890968,0.959301066555056,-0.0122204969160199));
#44274=DIRECTION('center_axis',(-0.498277810351142,0.867017425138747,9.06501467342992E-5));
#44275=DIRECTION('ref_axis',(0.866925828401964,0.498226683737,-0.0144837723677419));
#44276=DIRECTION('center_axis',(5.15167520928809E-67,-1.18789542670764E-48,
-1.));
#44277=DIRECTION('ref_axis',(-4.33680868994202E-19,1.,-1.18789542670764E-48));
#44278=DIRECTION('center_axis',(5.15167520928809E-67,-1.18789542670764E-48,
-1.));
#44279=DIRECTION('ref_axis',(0.,1.,0.));
#44280=DIRECTION('center_axis',(0.978552132724802,-0.205999301990102,0.000105448247615573));
#44281=DIRECTION('ref_axis',(0.205985181528349,0.978478801224133,-0.0122204969505153));
#44282=DIRECTION('center_axis',(-0.564767189310334,0.825250273348065,9.0650146758551E-5));
#44283=DIRECTION('ref_axis',(0.82516297032109,0.564709033705155,-0.014483772390721));
#44284=DIRECTION('center_axis',(5.15167520928809E-67,-1.18789542670764E-48,
-1.));
#44285=DIRECTION('ref_axis',(-4.33680868994202E-19,1.,-1.18789542670764E-48));
#44286=DIRECTION('center_axis',(5.15167520928809E-67,-1.18789542670764E-48,
-1.));
#44287=DIRECTION('ref_axis',(0.,1.,0.));
#44288=DIRECTION('center_axis',(0.991698102030069,-0.128587959430995,0.000105448245943976));
#44289=DIRECTION('ref_axis',(0.128579636019992,0.99162388869792,-0.0122204977223251));
#44290=DIRECTION('center_axis',(-0.627774590743336,0.778395179198579,9.06501467764949E-5));
#44291=DIRECTION('ref_axis',(0.778312708134504,0.627709764696415,-0.014483772336843));
#44292=DIRECTION('center_axis',(5.15167520928809E-67,-1.18789542670764E-48,
-1.));
#44293=DIRECTION('ref_axis',(-4.33680868994202E-19,1.,-1.18789542670764E-48));
#44294=DIRECTION('center_axis',(5.15167520928809E-67,-1.18789542670764E-48,
-1.));
#44295=DIRECTION('ref_axis',(0.,1.,0.));
#44296=DIRECTION('center_axis',(0.998729922762269,-0.0503838293497056,0.000105448247690158));
#44297=DIRECTION('ref_axis',(0.0503813543083624,0.998655285167543,-0.0122204969206726));
#44298=DIRECTION('center_axis',(-0.686911553068082,0.726741019926732,9.065014676939E-5));
#44299=DIRECTION('ref_axis',(0.726663889285701,0.686840456252424,-0.0144837724071123));
#44300=DIRECTION('center_axis',(5.15167520928809E-67,-1.18789542670764E-48,
-1.));
#44301=DIRECTION('ref_axis',(-4.33680868994202E-19,1.,-1.18789542670764E-48));
#44302=DIRECTION('center_axis',(5.15167520928809E-67,-1.18789542670764E-48,
-1.));
#44303=DIRECTION('ref_axis',(0.,1.,0.));
#44304=DIRECTION('center_axis',(0.999604241409737,0.0281309337977193,0.000105448247673278));
#44305=DIRECTION('ref_axis',(0.0281275452111183,-0.999529639707527,0.0122204969841135));
#44306=DIRECTION('center_axis',(-0.741813477246845,0.670606260601179,9.06501467534462E-5));
#44307=DIRECTION('ref_axis',(0.670534945920493,0.741736547999089,-0.0144837723606804));
#44308=DIRECTION('center_axis',(5.15167520928809E-67,-1.18789542670764E-48,
-1.));
#44309=DIRECTION('ref_axis',(-4.33680868994202E-19,1.,-1.18789542670764E-48));
#44310=DIRECTION('center_axis',(5.15167520928809E-67,-1.18789542670764E-48,
-1.));
#44311=DIRECTION('ref_axis',(0.,1.,0.));
#44312=DIRECTION('center_axis',(0.994315667506773,0.106472260383761,0.000105448247684943));
#44313=DIRECTION('ref_axis',(0.106463029060952,-0.994241561642206,0.0122204969798675));
#44314=DIRECTION('center_axis',(-0.792141874660476,0.610336990679688,9.06501468075157E-5));
#44315=DIRECTION('ref_axis',(0.610271931637649,0.792059587274653,-0.0144837723525293));
#44316=DIRECTION('center_axis',(5.15167520928809E-67,-1.18789542670764E-48,
-1.));
#44317=DIRECTION('ref_axis',(-4.33680868994202E-19,1.,-1.18789542670764E-48));
#44318=DIRECTION('center_axis',(5.15167520928809E-67,-1.18789542670764E-48,
-1.));
#44319=DIRECTION('ref_axis',(0.,1.,0.));
#44320=DIRECTION('center_axis',(0.982896806870138,0.184157150078822,0.000105448247739781));
#44321=DIRECTION('ref_axis',(0.184142132934029,-0.982823653730722,0.0122204969580191));
#44322=DIRECTION('center_axis',(-0.837586454002804,0.546304790253169,9.06501467452083E-5));
#44323=DIRECTION('ref_axis',(0.546246387960594,0.837499315808325,-0.0144837723191043));
#44324=DIRECTION('center_axis',(5.15167520928809E-67,-1.18789542670764E-48,
-1.));
#44325=DIRECTION('ref_axis',(-4.33680868994202E-19,1.,-1.18789542670764E-48));
#44326=DIRECTION('center_axis',(5.15167520928809E-67,-1.18789542670764E-48,
-1.));
#44327=DIRECTION('ref_axis',(0.,1.,0.));
#44328=DIRECTION('center_axis',(-0.778395179198544,-0.62777459074338,9.06501468008605E-5));
#44329=DIRECTION('ref_axis',(0.62770976469586,-0.778312708133716,0.0144837724032618));
#44330=DIRECTION('center_axis',(5.15167520928809E-67,-1.18789542670764E-48,
-1.));
#44331=DIRECTION('ref_axis',(-4.33680868994202E-19,1.,-1.18789542670764E-48));
#44332=DIRECTION('center_axis',(0.128587959434843,0.991698102029569,0.000105448247713068));
#44333=DIRECTION('ref_axis',(0.991623888707174,-0.128579636025041,0.0122204969182792));
#44334=DIRECTION('center_axis',(5.15167520928809E-67,-1.18789542670764E-48,
-1.));
#44335=DIRECTION('ref_axis',(0.,1.,0.));
#44336=DIRECTION('center_axis',(-0.82525027334801,-0.564767189310415,9.06501467887519E-5));
#44337=DIRECTION('ref_axis',(0.56470903370554,-0.825162970321483,0.0144837723533119));
#44338=DIRECTION('center_axis',(5.15167520928809E-67,-1.18789542670764E-48,
-1.));
#44339=DIRECTION('ref_axis',(-4.33680868994202E-19,1.,-1.18789542670764E-48));
#44340=DIRECTION('center_axis',(0.205999301990312,0.978552132724757,0.000105448247717959));
#44341=DIRECTION('ref_axis',(0.978478801224664,-0.205985181528676,0.0122204969024898));
#44342=DIRECTION('center_axis',(5.15167520928809E-67,-1.18789542670764E-48,
-1.));
#44343=DIRECTION('ref_axis',(0.,1.,0.));
#44344=DIRECTION('center_axis',(-0.867017425138643,-0.498277810351323,9.06501468256068E-5));
#44345=DIRECTION('ref_axis',(0.498226683737087,-0.866925828401692,0.014483772381015));
#44346=DIRECTION('center_axis',(5.15167520928809E-67,-1.18789542670764E-48,
-1.));
#44347=DIRECTION('ref_axis',(-4.33680868994202E-19,1.,-1.18789542670764E-48));
#44348=DIRECTION('center_axis',(0.282140590347035,0.959373064120154,0.000105448247634384));
#44349=DIRECTION('ref_axis',(0.959301066555324,-0.282120759890904,0.0122204968965099));
#44350=DIRECTION('center_axis',(5.15167520928809E-67,-1.18789542670764E-48,
-1.));
#44351=DIRECTION('ref_axis',(0.,1.,0.));
#44352=DIRECTION('center_axis',(-0.903439126190879,-0.428716382996979,9.06501467301661E-5));
#44353=DIRECTION('ref_axis',(0.428672600586422,-0.903343800468688,0.0144837723422516));
#44354=DIRECTION('center_axis',(5.15167520928809E-67,-1.18789542670764E-48,
-1.));
#44355=DIRECTION('ref_axis',(-4.33680868994202E-19,1.,-1.18789542670764E-48));
#44356=DIRECTION('center_axis',(0.356542388143256,0.934279141551266,0.000105448247681697));
#44357=DIRECTION('ref_axis',(0.934208921810558,-0.356516969953973,0.0122204968962765));
#44358=DIRECTION('center_axis',(5.15167520928809E-67,-1.18789542670764E-48,
-1.));
#44359=DIRECTION('ref_axis',(0.,1.,0.));
#44360=DIRECTION('center_axis',(-0.934290824606111,-0.356511776578816,9.06501466618288E-5));
#44361=DIRECTION('ref_axis',(0.356475608304419,-0.934192357612002,0.0144837724134131));
#44362=DIRECTION('center_axis',(5.15167520928809E-67,-1.18789542670764E-48,
-1.));
#44363=DIRECTION('ref_axis',(-4.33680868994202E-19,1.,-1.18789542670764E-48));
#44364=DIRECTION('center_axis',(0.428745983554273,0.903425077395324,0.000105448247749283));
#44365=DIRECTION('ref_axis',(0.903357068406257,-0.428715134343181,0.0122204969441668));
#44366=DIRECTION('center_axis',(5.15167520928809E-67,-1.18789542670764E-48,
-1.));
#44367=DIRECTION('ref_axis',(0.,1.,0.));
#44368=DIRECTION('center_axis',(-0.959382309404256,-0.282109156506322,9.06501468215648E-5));
#44369=DIRECTION('ref_axis',(0.282080825358184,-0.959281308221691,0.0144837723582998));
#44370=DIRECTION('center_axis',(5.15167520928809E-67,-1.18789542670764E-48,
-1.));
#44371=DIRECTION('ref_axis',(-4.33680868994202E-19,1.,-1.18789542670764E-48));
#44372=DIRECTION('center_axis',(0.498306217397306,0.86700109722183,0.000105448244261109));
#44373=DIRECTION('ref_axis',(0.866935718266673,-0.498270127351015,0.0122204984779969));
#44374=DIRECTION('center_axis',(5.15167520928809E-67,-1.18789542670764E-48,
-1.));
#44375=DIRECTION('ref_axis',(0.,1.,0.));
#44376=DIRECTION('center_axis',(-0.978558883238081,-0.205967239672699,9.06501467769327E-5));
#44377=DIRECTION('ref_axis',(0.205946920321355,-0.978455970571544,0.0144837724038677));
#44378=DIRECTION('center_axis',(5.15167520928809E-67,-1.18789542670764E-48,
-1.));
#44379=DIRECTION('ref_axis',(-4.33680868994202E-19,1.,-1.18789542670764E-48));
#44380=DIRECTION('center_axis',(0.564794227718686,0.825231766969935,0.000105448247134299));
#44381=DIRECTION('ref_axis',(0.825169421162366,-0.564753119361502,0.0122204971264834));
#44382=DIRECTION('center_axis',(5.15167520928809E-67,-1.18789542670764E-48,
-1.));
#44383=DIRECTION('ref_axis',(0.,1.,0.));
#44384=DIRECTION('center_axis',(-0.991702316152861,-0.128555466315523,9.06501467288715E-5));
#44385=DIRECTION('ref_axis',(0.12854328403675,-0.991598126494102,0.0144837723826971));
#44386=DIRECTION('center_axis',(5.15167520928809E-67,-1.18789542670764E-48,
-1.));
#44387=DIRECTION('ref_axis',(-4.33680868994202E-19,1.,-1.18789542670764E-48));
#44388=DIRECTION('center_axis',(0.627800093808552,0.778374608459603,0.000105448247728723));
#44389=DIRECTION('ref_axis',(0.778315680170199,-0.627754220580874,0.0122204968843025));
#44390=DIRECTION('center_axis',(5.15167520928809E-67,-1.18789542670764E-48,
-1.));
#44391=DIRECTION('ref_axis',(0.,1.,0.));
#44392=DIRECTION('center_axis',(-0.998731574514058,-0.0503511057596628,
9.06501468007229E-5));
#44393=DIRECTION('ref_axis',(0.0503471356611987,-0.998626750226619,0.0144837723861814));
#44394=DIRECTION('center_axis',(5.15167520928809E-67,-1.18789542670764E-48,
-1.));
#44395=DIRECTION('ref_axis',(-4.33680868994202E-19,1.,-1.18789542670764E-48));
#44396=DIRECTION('center_axis',(0.686935363554282,0.726718511653043,0.000105448247718559));
#44397=DIRECTION('ref_axis',(0.726663364191442,-0.686885008277775,0.012220496930023));
#44398=DIRECTION('center_axis',(5.15167520928809E-67,-1.18789542670764E-48,
-1.));
#44399=DIRECTION('ref_axis',(0.,1.,0.));
#44400=DIRECTION('center_axis',(-0.99960332060644,0.0281636861069471,9.06501467308329E-5));
#44401=DIRECTION('ref_axis',(0.0281594195481261,0.999498507967114,-0.0144837723754724));
#44402=DIRECTION('center_axis',(5.15167520928809E-67,-1.18789542670764E-48,
-1.));
#44403=DIRECTION('ref_axis',(-4.33680868994202E-19,1.,-1.18789542670764E-48));
#44404=DIRECTION('center_axis',(0.741835448354451,0.670581953563782,0.00010544824772104));
#44405=DIRECTION('ref_axis',(0.670530926933101,-0.74178092148675,0.0122204969008548));
#44406=DIRECTION('center_axis',(5.15167520928809E-67,-1.18789542670764E-48,
-1.));
#44407=DIRECTION('ref_axis',(0.,1.,0.));
#44408=DIRECTION('center_axis',(-0.994312179825441,0.106504839483146,9.06501467381912E-5));
#44409=DIRECTION('ref_axis',(0.106492362571802,0.99420802503887,-0.0144837723741357));
#44410=DIRECTION('center_axis',(5.15167520928809E-67,-1.18789542670764E-48,
-1.));
#44411=DIRECTION('ref_axis',(-4.33680868994202E-19,1.,-1.18789542670764E-48));
#44412=DIRECTION('center_axis',(0.792161870929241,0.610311034740936,0.000105448246928053));
#44413=DIRECTION('ref_axis',(0.610264443534212,-0.792103508642726,0.0122204972796185));
#44414=DIRECTION('center_axis',(5.15167520928809E-67,-1.18789542670764E-48,
-1.));
#44415=DIRECTION('ref_axis',(0.,1.,0.));
#44416=DIRECTION('center_axis',(-0.982890773813477,0.184189355107443,9.06501467544422E-5));
#44417=DIRECTION('ref_axis',(0.184168744767819,0.982787919028209,-0.0144837723970302));
#44418=DIRECTION('center_axis',(5.15167520928809E-67,-1.18789542670764E-48,
-1.));
#44419=DIRECTION('ref_axis',(-4.33680868994202E-19,1.,-1.18789542670764E-48));
#44420=DIRECTION('center_axis',(0.837604352151223,0.546277345437276,0.000105448247675196));
#44421=DIRECTION('ref_axis',(0.546235476910048,-0.837542514275434,0.0122204969635834));
#44422=DIRECTION('center_axis',(5.15167520928809E-67,-1.18789542670764E-48,
-1.));
#44423=DIRECTION('ref_axis',(0.,1.,0.));
#44424=DIRECTION('center_axis',(-0.96540951933663,0.260738282108263,9.06501468112521E-5));
#44425=DIRECTION('ref_axis',(0.26070966540993,0.965308598686718,-0.0144837724135372));
#44426=DIRECTION('center_axis',(5.15167520928809E-67,-1.18789542670764E-48,
-1.));
#44427=DIRECTION('ref_axis',(-4.33680868994202E-19,1.,-1.18789542670764E-48));
#44428=DIRECTION('center_axis',(0.877882724009476,0.478875674644651,0.000105448247670176));
#44429=DIRECTION('ref_axis',(0.478838786927941,-0.877817791792444,0.0122204969627255));
#44430=DIRECTION('center_axis',(5.15167520928809E-67,-1.18789542670764E-48,
-1.));
#44431=DIRECTION('ref_axis',(0.,1.,0.));
#44432=DIRECTION('center_axis',(-0.941976194141744,0.33567967089591,9.06501467361574E-5));
#44433=DIRECTION('ref_axis',(0.335643224270696,0.941877829837669,-0.0144837723488913));
#44434=DIRECTION('center_axis',(5.15167520928809E-67,-1.18789542670764E-48,
-1.));
#44435=DIRECTION('ref_axis',(-4.33680868994202E-19,1.,-1.18789542670764E-48));
#44436=DIRECTION('center_axis',(0.912748656948457,0.408521576075799,0.000105448247549386));
#44437=DIRECTION('ref_axis',(0.408489896594413,-0.912681030718381,0.0122204970078645));
#44438=DIRECTION('center_axis',(5.15167520928809E-67,-1.18789542670764E-48,
-1.));
#44439=DIRECTION('ref_axis',(0.,1.,0.));
#44440=DIRECTION('center_axis',(0.965418060567994,0.260706649723021,0.000105448239440975));
#44441=DIRECTION('ref_axis',(0.260685939330027,-0.965346311123993,0.0122205006002244));
#44442=DIRECTION('center_axis',(-0.877867034330543,0.478904439129822,9.06501467527618E-5));
#44443=DIRECTION('ref_axis',(0.478853053655558,0.877775582562237,-0.014483772377146));
#44444=DIRECTION('center_axis',(5.15167520928809E-67,-1.18789542670764E-48,
-1.));
#44445=DIRECTION('ref_axis',(-4.33680868994202E-19,1.,-1.18789542670764E-48));
#44446=DIRECTION('center_axis',(5.15167520928809E-67,-1.18789542670764E-48,
-1.));
#44447=DIRECTION('ref_axis',(-4.33680868994202E-19,1.,-1.18789542670764E-48));
#44448=DIRECTION('',(5.15167520928809E-67,-1.18789542670764E-48,-1.));
#44449=DIRECTION('center_axis',(5.15167520928809E-67,-1.18789542670764E-48,
-1.));
#44450=DIRECTION('ref_axis',(-4.33680868994202E-19,1.,-1.18789542670764E-48));
#44451=DIRECTION('',(-5.15167520928809E-67,1.18789542670764E-48,1.));
#44452=DIRECTION('center_axis',(5.15167520928809E-67,-1.18789542670764E-48,
-1.));
#44453=DIRECTION('ref_axis',(-4.33680868994202E-19,1.,-1.18789542670764E-48));
#44454=DIRECTION('',(-5.15167520928809E-67,1.18789542670764E-48,1.));
#44455=DIRECTION('',(5.15167520928809E-67,-1.18789542670764E-48,-1.));
#44456=DIRECTION('center_axis',(5.15167520928809E-67,-1.18789542670764E-48,
-1.));
#44457=DIRECTION('ref_axis',(-4.33680868994202E-19,1.,-1.18789542670764E-48));
#44458=DIRECTION('center_axis',(5.15167520928809E-67,-1.18789542670764E-48,
-1.));
#44459=DIRECTION('ref_axis',(-4.33680868994202E-19,1.,-1.18789542670764E-48));
#44460=DIRECTION('',(-5.15167520928809E-67,1.18789542670764E-48,1.));
#44461=DIRECTION('',(5.15167520928809E-67,-1.18789542670764E-48,-1.));
#44462=DIRECTION('center_axis',(5.15167520928809E-67,-1.18789542670764E-48,
-1.));
#44463=DIRECTION('ref_axis',(-4.33680868994202E-19,1.,-1.18789542670764E-48));
#44464=DIRECTION('center_axis',(5.15167520928809E-67,-1.18789542670764E-48,
-1.));
#44465=DIRECTION('ref_axis',(-4.33680868994202E-19,1.,-1.18789542670764E-48));
#44466=DIRECTION('',(-5.15167520928809E-67,1.18789542670764E-48,1.));
#44467=DIRECTION('',(5.15167520928809E-67,-1.18789542670764E-48,-1.));
#44468=DIRECTION('center_axis',(5.15167520928809E-67,-1.18789542670764E-48,
-1.));
#44469=DIRECTION('ref_axis',(-4.33680868994202E-19,1.,-1.18789542670764E-48));
#44470=DIRECTION('center_axis',(5.15167520928809E-67,-1.18789542670764E-48,
-1.));
#44471=DIRECTION('ref_axis',(-4.33680868994202E-19,1.,-1.18789542670764E-48));
#44472=DIRECTION('',(-5.15167520928809E-67,1.18789542670764E-48,1.));
#44473=DIRECTION('',(5.15167520928809E-67,-1.18789542670764E-48,-1.));
#44474=DIRECTION('center_axis',(5.15167520928809E-67,-1.18789542670764E-48,
-1.));
#44475=DIRECTION('ref_axis',(-4.33680868994202E-19,1.,-1.18789542670764E-48));
#44476=DIRECTION('center_axis',(5.15167520928809E-67,-1.18789542670764E-48,
-1.));
#44477=DIRECTION('ref_axis',(-4.33680868994202E-19,1.,-1.18789542670764E-48));
#44478=DIRECTION('',(-5.15167520928809E-67,1.18789542670764E-48,1.));
#44479=DIRECTION('',(5.15167520928809E-67,-1.18789542670764E-48,-1.));
#44480=DIRECTION('center_axis',(5.15167520928809E-67,-1.18789542670764E-48,
-1.));
#44481=DIRECTION('ref_axis',(-4.33680868994202E-19,1.,-1.18789542670764E-48));
#44482=DIRECTION('center_axis',(5.15167520928809E-67,-1.18789542670764E-48,
-1.));
#44483=DIRECTION('ref_axis',(-4.33680868994202E-19,1.,-1.18789542670764E-48));
#44484=DIRECTION('',(-5.15167520928809E-67,1.18789542670764E-48,1.));
#44485=DIRECTION('',(5.15167520928809E-67,-1.18789542670764E-48,-1.));
#44486=DIRECTION('center_axis',(5.15167520928809E-67,-1.18789542670764E-48,
-1.));
#44487=DIRECTION('ref_axis',(-4.33680868994202E-19,1.,-1.18789542670764E-48));
#44488=DIRECTION('center_axis',(5.15167520928809E-67,-1.18789542670764E-48,
-1.));
#44489=DIRECTION('ref_axis',(-4.33680868994202E-19,1.,-1.18789542670764E-48));
#44490=DIRECTION('',(-5.15167520928809E-67,1.18789542670764E-48,1.));
#44491=DIRECTION('',(5.15167520928809E-67,-1.18789542670764E-48,-1.));
#44492=DIRECTION('center_axis',(5.15167520928809E-67,-1.18789542670764E-48,
-1.));
#44493=DIRECTION('ref_axis',(-4.33680868994202E-19,1.,-1.18789542670764E-48));
#44494=DIRECTION('center_axis',(5.15167520928809E-67,-1.18789542670764E-48,
-1.));
#44495=DIRECTION('ref_axis',(-4.33680868994202E-19,1.,-1.18789542670764E-48));
#44496=DIRECTION('',(-5.15167520928809E-67,1.18789542670764E-48,1.));
#44497=DIRECTION('',(5.15167520928809E-67,-1.18789542670764E-48,-1.));
#44498=DIRECTION('center_axis',(5.15167520928809E-67,-1.18789542670764E-48,
-1.));
#44499=DIRECTION('ref_axis',(-4.33680868994202E-19,1.,-1.18789542670764E-48));
#44500=DIRECTION('center_axis',(5.15167520928809E-67,-1.18789542670764E-48,
-1.));
#44501=DIRECTION('ref_axis',(-4.33680868994202E-19,1.,-1.18789542670764E-48));
#44502=DIRECTION('',(-5.15167520928809E-67,1.18789542670764E-48,1.));
#44503=DIRECTION('',(5.15167520928809E-67,-1.18789542670764E-48,-1.));
#44504=DIRECTION('center_axis',(5.15167520928809E-67,-1.18789542670764E-48,
-1.));
#44505=DIRECTION('ref_axis',(-4.33680868994202E-19,1.,-1.18789542670764E-48));
#44506=DIRECTION('center_axis',(5.15167520928809E-67,-1.18789542670764E-48,
-1.));
#44507=DIRECTION('ref_axis',(-4.33680868994202E-19,1.,-1.18789542670764E-48));
#44508=DIRECTION('',(-5.15167520928809E-67,1.18789542670764E-48,1.));
#44509=DIRECTION('',(5.15167520928809E-67,-1.18789542670764E-48,-1.));
#44510=DIRECTION('center_axis',(5.15167520928809E-67,-1.18789542670764E-48,
-1.));
#44511=DIRECTION('ref_axis',(-4.33680868994202E-19,1.,-1.18789542670764E-48));
#44512=DIRECTION('center_axis',(5.15167520928809E-67,-1.18789542670764E-48,
-1.));
#44513=DIRECTION('ref_axis',(-4.33680868994202E-19,1.,-1.18789542670764E-48));
#44514=DIRECTION('',(-5.15167520928809E-67,1.18789542670764E-48,1.));
#44515=DIRECTION('',(5.15167520928809E-67,-1.18789542670764E-48,-1.));
#44516=DIRECTION('center_axis',(5.15167520928809E-67,-1.18789542670764E-48,
-1.));
#44517=DIRECTION('ref_axis',(-4.33680868994202E-19,1.,-1.18789542670764E-48));
#44518=DIRECTION('center_axis',(5.15167520928809E-67,-1.18789542670764E-48,
-1.));
#44519=DIRECTION('ref_axis',(-4.33680868994202E-19,1.,-1.18789542670764E-48));
#44520=DIRECTION('',(-5.15167520928809E-67,1.18789542670764E-48,1.));
#44521=DIRECTION('',(5.15167520928809E-67,-1.18789542670764E-48,-1.));
#44522=DIRECTION('center_axis',(5.15167520928809E-67,-1.18789542670764E-48,
-1.));
#44523=DIRECTION('ref_axis',(-4.33680868994202E-19,1.,-1.18789542670764E-48));
#44524=DIRECTION('center_axis',(5.15167520928809E-67,-1.18789542670764E-48,
-1.));
#44525=DIRECTION('ref_axis',(-4.33680868994202E-19,1.,-1.18789542670764E-48));
#44526=DIRECTION('',(-5.15167520928809E-67,1.18789542670764E-48,1.));
#44527=DIRECTION('',(5.15167520928809E-67,-1.18789542670764E-48,-1.));
#44528=DIRECTION('center_axis',(5.15167520928809E-67,-1.18789542670764E-48,
-1.));
#44529=DIRECTION('ref_axis',(-4.33680868994202E-19,1.,-1.18789542670764E-48));
#44530=DIRECTION('center_axis',(5.15167520928809E-67,-1.18789542670764E-48,
-1.));
#44531=DIRECTION('ref_axis',(-4.33680868994202E-19,1.,-1.18789542670764E-48));
#44532=DIRECTION('',(-5.15167520928809E-67,1.18789542670764E-48,1.));
#44533=DIRECTION('',(5.15167520928809E-67,-1.18789542670764E-48,-1.));
#44534=DIRECTION('center_axis',(5.15167520928809E-67,-1.18789542670764E-48,
-1.));
#44535=DIRECTION('ref_axis',(-4.33680868994202E-19,1.,-1.18789542670764E-48));
#44536=DIRECTION('center_axis',(5.15167520928809E-67,-1.18789542670764E-48,
-1.));
#44537=DIRECTION('ref_axis',(-4.33680868994202E-19,1.,-1.18789542670764E-48));
#44538=DIRECTION('',(-5.15167520928809E-67,1.18789542670764E-48,1.));
#44539=DIRECTION('',(5.15167520928809E-67,-1.18789542670764E-48,-1.));
#44540=DIRECTION('center_axis',(5.15167520928809E-67,-1.18789542670764E-48,
-1.));
#44541=DIRECTION('ref_axis',(-4.33680868994202E-19,1.,-1.18789542670764E-48));
#44542=DIRECTION('center_axis',(5.15167520928809E-67,-1.18789542670764E-48,
-1.));
#44543=DIRECTION('ref_axis',(-4.33680868994202E-19,1.,-1.18789542670764E-48));
#44544=DIRECTION('',(-5.15167520928809E-67,1.18789542670764E-48,1.));
#44545=DIRECTION('',(5.15167520928809E-67,-1.18789542670764E-48,-1.));
#44546=DIRECTION('center_axis',(5.15167520928809E-67,-1.18789542670764E-48,
-1.));
#44547=DIRECTION('ref_axis',(-4.33680868994202E-19,1.,-1.18789542670764E-48));
#44548=DIRECTION('center_axis',(5.15167520928809E-67,-1.18789542670764E-48,
-1.));
#44549=DIRECTION('ref_axis',(-4.33680868994202E-19,1.,-1.18789542670764E-48));
#44550=DIRECTION('',(-5.15167520928809E-67,1.18789542670764E-48,1.));
#44551=DIRECTION('',(5.15167520928809E-67,-1.18789542670764E-48,-1.));
#44552=DIRECTION('center_axis',(5.15167520928809E-67,-1.18789542670764E-48,
-1.));
#44553=DIRECTION('ref_axis',(-4.33680868994202E-19,1.,-1.18789542670764E-48));
#44554=DIRECTION('center_axis',(5.15167520928809E-67,-1.18789542670764E-48,
-1.));
#44555=DIRECTION('ref_axis',(-4.33680868994202E-19,1.,-1.18789542670764E-48));
#44556=DIRECTION('',(-5.15167520928809E-67,1.18789542670764E-48,1.));
#44557=DIRECTION('',(5.15167520928809E-67,-1.18789542670764E-48,-1.));
#44558=DIRECTION('center_axis',(5.15167520928809E-67,-1.18789542670764E-48,
-1.));
#44559=DIRECTION('ref_axis',(-4.33680868994202E-19,1.,-1.18789542670764E-48));
#44560=DIRECTION('center_axis',(5.15167520928809E-67,-1.18789542670764E-48,
-1.));
#44561=DIRECTION('ref_axis',(-4.33680868994202E-19,1.,-1.18789542670764E-48));
#44562=DIRECTION('',(-5.15167520928809E-67,1.18789542670764E-48,1.));
#44563=DIRECTION('',(5.15167520928809E-67,-1.18789542670764E-48,-1.));
#44564=DIRECTION('center_axis',(5.15167520928809E-67,-1.18789542670764E-48,
-1.));
#44565=DIRECTION('ref_axis',(-4.33680868994202E-19,1.,-1.18789542670764E-48));
#44566=DIRECTION('center_axis',(5.15167520928809E-67,-1.18789542670764E-48,
-1.));
#44567=DIRECTION('ref_axis',(-4.33680868994202E-19,1.,-1.18789542670764E-48));
#44568=DIRECTION('',(-5.15167520928809E-67,1.18789542670764E-48,1.));
#44569=DIRECTION('',(5.15167520928809E-67,-1.18789542670764E-48,-1.));
#44570=DIRECTION('center_axis',(5.15167520928809E-67,-1.18789542670764E-48,
-1.));
#44571=DIRECTION('ref_axis',(-4.33680868994202E-19,1.,-1.18789542670764E-48));
#44572=DIRECTION('center_axis',(5.15167520928809E-67,-1.18789542670764E-48,
-1.));
#44573=DIRECTION('ref_axis',(-4.33680868994202E-19,1.,-1.18789542670764E-48));
#44574=DIRECTION('',(-5.15167520928809E-67,1.18789542670764E-48,1.));
#44575=DIRECTION('',(5.15167520928809E-67,-1.18789542670764E-48,-1.));
#44576=DIRECTION('center_axis',(5.15167520928809E-67,-1.18789542670764E-48,
-1.));
#44577=DIRECTION('ref_axis',(-4.33680868994202E-19,1.,-1.18789542670764E-48));
#44578=DIRECTION('center_axis',(5.15167520928809E-67,-1.18789542670764E-48,
-1.));
#44579=DIRECTION('ref_axis',(-4.33680868994202E-19,1.,-1.18789542670764E-48));
#44580=DIRECTION('',(-5.15167520928809E-67,1.18789542670764E-48,1.));
#44581=DIRECTION('',(5.15167520928809E-67,-1.18789542670764E-48,-1.));
#44582=DIRECTION('center_axis',(5.15167520928809E-67,-1.18789542670764E-48,
-1.));
#44583=DIRECTION('ref_axis',(-4.33680868994202E-19,1.,-1.18789542670764E-48));
#44584=DIRECTION('center_axis',(5.15167520928809E-67,-1.18789542670764E-48,
-1.));
#44585=DIRECTION('ref_axis',(-4.33680868994202E-19,1.,-1.18789542670764E-48));
#44586=DIRECTION('',(-5.15167520928809E-67,1.18789542670764E-48,1.));
#44587=DIRECTION('',(5.15167520928809E-67,-1.18789542670764E-48,-1.));
#44588=DIRECTION('center_axis',(5.15167520928809E-67,-1.18789542670764E-48,
-1.));
#44589=DIRECTION('ref_axis',(-4.33680868994202E-19,1.,-1.18789542670764E-48));
#44590=DIRECTION('center_axis',(5.15167520928809E-67,-1.18789542670764E-48,
-1.));
#44591=DIRECTION('ref_axis',(-4.33680868994202E-19,1.,-1.18789542670764E-48));
#44592=DIRECTION('',(-5.15167520928809E-67,1.18789542670764E-48,1.));
#44593=DIRECTION('',(5.15167520928809E-67,-1.18789542670764E-48,-1.));
#44594=DIRECTION('center_axis',(5.15167520928809E-67,-1.18789542670764E-48,
-1.));
#44595=DIRECTION('ref_axis',(-4.33680868994202E-19,1.,-1.18789542670764E-48));
#44596=DIRECTION('center_axis',(5.15167520928809E-67,-1.18789542670764E-48,
-1.));
#44597=DIRECTION('ref_axis',(-4.33680868994202E-19,1.,-1.18789542670764E-48));
#44598=DIRECTION('',(-5.15167520928809E-67,1.18789542670764E-48,1.));
#44599=DIRECTION('',(5.15167520928809E-67,-1.18789542670764E-48,-1.));
#44600=DIRECTION('center_axis',(5.15167520928809E-67,-1.18789542670764E-48,
-1.));
#44601=DIRECTION('ref_axis',(-4.33680868994202E-19,1.,-1.18789542670764E-48));
#44602=DIRECTION('center_axis',(5.15167520928809E-67,-1.18789542670764E-48,
-1.));
#44603=DIRECTION('ref_axis',(-4.33680868994202E-19,1.,-1.18789542670764E-48));
#44604=DIRECTION('',(-5.15167520928809E-67,1.18789542670764E-48,1.));
#44605=DIRECTION('',(5.15167520928809E-67,-1.18789542670764E-48,-1.));
#44606=DIRECTION('center_axis',(5.15167520928809E-67,-1.18789542670764E-48,
-1.));
#44607=DIRECTION('ref_axis',(-4.33680868994202E-19,1.,-1.18789542670764E-48));
#44608=DIRECTION('center_axis',(5.15167520928809E-67,-1.18789542670764E-48,
-1.));
#44609=DIRECTION('ref_axis',(-4.33680868994202E-19,1.,-1.18789542670764E-48));
#44610=DIRECTION('',(-5.15167520928809E-67,1.18789542670764E-48,1.));
#44611=DIRECTION('',(5.15167520928809E-67,-1.18789542670764E-48,-1.));
#44612=DIRECTION('center_axis',(5.15167520928809E-67,-1.18789542670764E-48,
-1.));
#44613=DIRECTION('ref_axis',(-4.33680868994202E-19,1.,-1.18789542670764E-48));
#44614=DIRECTION('center_axis',(5.15167520928809E-67,-1.18789542670764E-48,
-1.));
#44615=DIRECTION('ref_axis',(-4.33680868994202E-19,1.,-1.18789542670764E-48));
#44616=DIRECTION('',(-5.15167520928809E-67,1.18789542670764E-48,1.));
#44617=DIRECTION('',(5.15167520928809E-67,-1.18789542670764E-48,-1.));
#44618=DIRECTION('center_axis',(5.15167520928809E-67,-1.18789542670764E-48,
-1.));
#44619=DIRECTION('ref_axis',(-4.33680868994202E-19,1.,-1.18789542670764E-48));
#44620=DIRECTION('center_axis',(5.15167520928809E-67,-1.18789542670764E-48,
-1.));
#44621=DIRECTION('ref_axis',(-4.33680868994202E-19,1.,-1.18789542670764E-48));
#44622=DIRECTION('',(-5.15167520928809E-67,1.18789542670764E-48,1.));
#44623=DIRECTION('',(5.15167520928809E-67,-1.18789542670764E-48,-1.));
#44624=DIRECTION('center_axis',(5.15167520928809E-67,-1.18789542670764E-48,
-1.));
#44625=DIRECTION('ref_axis',(-4.33680868994202E-19,1.,-1.18789542670764E-48));
#44626=DIRECTION('center_axis',(5.15167520928809E-67,-1.18789542670764E-48,
-1.));
#44627=DIRECTION('ref_axis',(-4.33680868994202E-19,1.,-1.18789542670764E-48));
#44628=DIRECTION('',(-5.15167520928809E-67,1.18789542670764E-48,1.));
#44629=DIRECTION('',(5.15167520928809E-67,-1.18789542670764E-48,-1.));
#44630=DIRECTION('center_axis',(5.15167520928809E-67,-1.18789542670764E-48,
-1.));
#44631=DIRECTION('ref_axis',(-4.33680868994202E-19,1.,-1.18789542670764E-48));
#44632=DIRECTION('center_axis',(5.15167520928809E-67,-1.18789542670764E-48,
-1.));
#44633=DIRECTION('ref_axis',(-4.33680868994202E-19,1.,-1.18789542670764E-48));
#44634=DIRECTION('',(-5.15167520928809E-67,1.18789542670764E-48,1.));
#44635=DIRECTION('',(5.15167520928809E-67,-1.18789542670764E-48,-1.));
#44636=DIRECTION('center_axis',(5.15167520928809E-67,-1.18789542670764E-48,
-1.));
#44637=DIRECTION('ref_axis',(-4.33680868994202E-19,1.,-1.18789542670764E-48));
#44638=DIRECTION('center_axis',(5.15167520928809E-67,-1.18789542670764E-48,
-1.));
#44639=DIRECTION('ref_axis',(-4.33680868994202E-19,1.,-1.18789542670764E-48));
#44640=DIRECTION('',(-5.15167520928809E-67,1.18789542670764E-48,1.));
#44641=DIRECTION('',(5.15167520928809E-67,-1.18789542670764E-48,-1.));
#44642=DIRECTION('center_axis',(5.15167520928809E-67,-1.18789542670764E-48,
-1.));
#44643=DIRECTION('ref_axis',(-4.33680868994202E-19,1.,-1.18789542670764E-48));
#44644=DIRECTION('center_axis',(5.15167520928809E-67,-1.18789542670764E-48,
-1.));
#44645=DIRECTION('ref_axis',(-4.33680868994202E-19,1.,-1.18789542670764E-48));
#44646=DIRECTION('',(-5.15167520928809E-67,1.18789542670764E-48,1.));
#44647=DIRECTION('',(5.15167520928809E-67,-1.18789542670764E-48,-1.));
#44648=DIRECTION('center_axis',(5.15167520928809E-67,-1.18789542670764E-48,
-1.));
#44649=DIRECTION('ref_axis',(-4.33680868994202E-19,1.,-1.18789542670764E-48));
#44650=DIRECTION('center_axis',(5.15167520928809E-67,-1.18789542670764E-48,
-1.));
#44651=DIRECTION('ref_axis',(-4.33680868994202E-19,1.,-1.18789542670764E-48));
#44652=DIRECTION('',(-5.15167520928809E-67,1.18789542670764E-48,1.));
#44653=DIRECTION('',(5.15167520928809E-67,-1.18789542670764E-48,-1.));
#44654=DIRECTION('center_axis',(5.15167520928809E-67,-1.18789542670764E-48,
-1.));
#44655=DIRECTION('ref_axis',(-4.33680868994202E-19,1.,-1.18789542670764E-48));
#44656=DIRECTION('center_axis',(5.15167520928809E-67,-1.18789542670764E-48,
-1.));
#44657=DIRECTION('ref_axis',(-4.33680868994202E-19,1.,-1.18789542670764E-48));
#44658=DIRECTION('',(-5.15167520928809E-67,1.18789542670764E-48,1.));
#44659=DIRECTION('',(5.15167520928809E-67,-1.18789542670764E-48,-1.));
#44660=DIRECTION('center_axis',(5.15167520928809E-67,-1.18789542670764E-48,
-1.));
#44661=DIRECTION('ref_axis',(-4.33680868994202E-19,1.,-1.18789542670764E-48));
#44662=DIRECTION('center_axis',(5.15167520928809E-67,-1.18789542670764E-48,
-1.));
#44663=DIRECTION('ref_axis',(-4.33680868994202E-19,1.,-1.18789542670764E-48));
#44664=DIRECTION('',(-5.15167520928809E-67,1.18789542670764E-48,1.));
#44665=DIRECTION('',(5.15167520928809E-67,-1.18789542670764E-48,-1.));
#44666=DIRECTION('center_axis',(5.15167520928809E-67,-1.18789542670764E-48,
-1.));
#44667=DIRECTION('ref_axis',(-4.33680868994202E-19,1.,-1.18789542670764E-48));
#44668=DIRECTION('center_axis',(5.15167520928809E-67,-1.18789542670764E-48,
-1.));
#44669=DIRECTION('ref_axis',(-4.33680868994202E-19,1.,-1.18789542670764E-48));
#44670=DIRECTION('',(-5.15167520928809E-67,1.18789542670764E-48,1.));
#44671=DIRECTION('',(5.15167520928809E-67,-1.18789542670764E-48,-1.));
#44672=DIRECTION('center_axis',(5.15167520928809E-67,-1.18789542670764E-48,
-1.));
#44673=DIRECTION('ref_axis',(-4.33680868994202E-19,1.,-1.18789542670764E-48));
#44674=DIRECTION('center_axis',(5.15167520928809E-67,-1.18789542670764E-48,
-1.));
#44675=DIRECTION('ref_axis',(-4.33680868994202E-19,1.,-1.18789542670764E-48));
#44676=DIRECTION('',(-5.15167520928809E-67,1.18789542670764E-48,1.));
#44677=DIRECTION('',(5.15167520928809E-67,-1.18789542670764E-48,-1.));
#44678=DIRECTION('center_axis',(5.15167520928809E-67,-1.18789542670764E-48,
-1.));
#44679=DIRECTION('ref_axis',(-4.33680868994202E-19,1.,-1.18789542670764E-48));
#44680=DIRECTION('center_axis',(5.15167520928809E-67,-1.18789542670764E-48,
-1.));
#44681=DIRECTION('ref_axis',(-4.33680868994202E-19,1.,-1.18789542670764E-48));
#44682=DIRECTION('',(-5.15167520928809E-67,1.18789542670764E-48,1.));
#44683=DIRECTION('',(5.15167520928809E-67,-1.18789542670764E-48,-1.));
#44684=DIRECTION('center_axis',(5.15167520928809E-67,-1.18789542670764E-48,
-1.));
#44685=DIRECTION('ref_axis',(-4.33680868994202E-19,1.,-1.18789542670764E-48));
#44686=DIRECTION('center_axis',(5.15167520928809E-67,-1.18789542670764E-48,
-1.));
#44687=DIRECTION('ref_axis',(-4.33680868994202E-19,1.,-1.18789542670764E-48));
#44688=DIRECTION('',(-5.15167520928809E-67,1.18789542670764E-48,1.));
#44689=DIRECTION('',(5.15167520928809E-67,-1.18789542670764E-48,-1.));
#44690=DIRECTION('center_axis',(5.15167520928809E-67,-1.18789542670764E-48,
-1.));
#44691=DIRECTION('ref_axis',(-4.33680868994202E-19,1.,-1.18789542670764E-48));
#44692=DIRECTION('center_axis',(5.15167520928809E-67,-1.18789542670764E-48,
-1.));
#44693=DIRECTION('ref_axis',(-4.33680868994202E-19,1.,-1.18789542670764E-48));
#44694=DIRECTION('',(-5.15167520928809E-67,1.18789542670764E-48,1.));
#44695=DIRECTION('',(5.15167520928809E-67,-1.18789542670764E-48,-1.));
#44696=DIRECTION('center_axis',(5.15167520928809E-67,-1.18789542670764E-48,
-1.));
#44697=DIRECTION('ref_axis',(-4.33680868994202E-19,1.,-1.18789542670764E-48));
#44698=DIRECTION('center_axis',(5.15167520928809E-67,-1.18789542670764E-48,
-1.));
#44699=DIRECTION('ref_axis',(-4.33680868994202E-19,1.,-1.18789542670764E-48));
#44700=DIRECTION('',(-5.15167520928809E-67,1.18789542670764E-48,1.));
#44701=DIRECTION('',(5.15167520928809E-67,-1.18789542670764E-48,-1.));
#44702=DIRECTION('center_axis',(5.15167520928809E-67,-1.18789542670764E-48,
-1.));
#44703=DIRECTION('ref_axis',(-4.33680868994202E-19,1.,-1.18789542670764E-48));
#44704=DIRECTION('center_axis',(5.15167520928809E-67,-1.18789542670764E-48,
-1.));
#44705=DIRECTION('ref_axis',(-4.33680868994202E-19,1.,-1.18789542670764E-48));
#44706=DIRECTION('',(-5.15167520928809E-67,1.18789542670764E-48,1.));
#44707=DIRECTION('',(5.15167520928809E-67,-1.18789542670764E-48,-1.));
#44708=DIRECTION('center_axis',(5.15167520928809E-67,-1.18789542670764E-48,
-1.));
#44709=DIRECTION('ref_axis',(-4.33680868994202E-19,1.,-1.18789542670764E-48));
#44710=DIRECTION('center_axis',(5.15167520928809E-67,-1.18789542670764E-48,
-1.));
#44711=DIRECTION('ref_axis',(-4.33680868994202E-19,1.,-1.18789542670764E-48));
#44712=DIRECTION('',(-5.15167520928809E-67,1.18789542670764E-48,1.));
#44713=DIRECTION('',(5.15167520928809E-67,-1.18789542670764E-48,-1.));
#44714=DIRECTION('center_axis',(5.15167520928809E-67,-1.18789542670764E-48,
-1.));
#44715=DIRECTION('ref_axis',(-4.33680868994202E-19,1.,-1.18789542670764E-48));
#44716=DIRECTION('center_axis',(5.15167520928809E-67,-1.18789542670764E-48,
-1.));
#44717=DIRECTION('ref_axis',(-4.33680868994202E-19,1.,-1.18789542670764E-48));
#44718=DIRECTION('',(-5.15167520928809E-67,1.18789542670764E-48,1.));
#44719=DIRECTION('',(5.15167520928809E-67,-1.18789542670764E-48,-1.));
#44720=DIRECTION('center_axis',(5.15167520928809E-67,-1.18789542670764E-48,
-1.));
#44721=DIRECTION('ref_axis',(-4.33680868994202E-19,1.,-1.18789542670764E-48));
#44722=DIRECTION('center_axis',(5.15167520928809E-67,-1.18789542670764E-48,
-1.));
#44723=DIRECTION('ref_axis',(-4.33680868994202E-19,1.,-1.18789542670764E-48));
#44724=DIRECTION('',(-5.15167520928809E-67,1.18789542670764E-48,1.));
#44725=DIRECTION('',(5.15167520928809E-67,-1.18789542670764E-48,-1.));
#44726=DIRECTION('center_axis',(5.15167520928809E-67,-1.18789542670764E-48,
-1.));
#44727=DIRECTION('ref_axis',(-4.33680868994202E-19,1.,-1.18789542670764E-48));
#44728=DIRECTION('center_axis',(5.15167520928809E-67,-1.18789542670764E-48,
-1.));
#44729=DIRECTION('ref_axis',(-4.33680868994202E-19,1.,-1.18789542670764E-48));
#44730=DIRECTION('',(-5.15167520928809E-67,1.18789542670764E-48,1.));
#44731=DIRECTION('',(5.15167520928809E-67,-1.18789542670764E-48,-1.));
#44732=DIRECTION('center_axis',(5.15167520928809E-67,-1.18789542670764E-48,
-1.));
#44733=DIRECTION('ref_axis',(-4.33680868994202E-19,1.,-1.18789542670764E-48));
#44734=DIRECTION('center_axis',(5.15167520928809E-67,-1.18789542670764E-48,
-1.));
#44735=DIRECTION('ref_axis',(-4.33680868994202E-19,1.,-1.18789542670764E-48));
#44736=DIRECTION('',(-5.15167520928809E-67,1.18789542670764E-48,1.));
#44737=DIRECTION('',(5.15167520928809E-67,-1.18789542670764E-48,-1.));
#44738=DIRECTION('center_axis',(5.15167520928809E-67,-1.18789542670764E-48,
-1.));
#44739=DIRECTION('ref_axis',(-4.33680868994202E-19,1.,-1.18789542670764E-48));
#44740=DIRECTION('center_axis',(5.15167520928809E-67,-1.18789542670764E-48,
-1.));
#44741=DIRECTION('ref_axis',(-4.33680868994202E-19,1.,-1.18789542670764E-48));
#44742=DIRECTION('',(-5.15167520928809E-67,1.18789542670764E-48,1.));
#44743=DIRECTION('',(5.15167520928809E-67,-1.18789542670764E-48,-1.));
#44744=DIRECTION('center_axis',(5.15167520928809E-67,-1.18789542670764E-48,
-1.));
#44745=DIRECTION('ref_axis',(-4.33680868994202E-19,1.,-1.18789542670764E-48));
#44746=DIRECTION('center_axis',(5.15167520928809E-67,-1.18789542670764E-48,
-1.));
#44747=DIRECTION('ref_axis',(-4.33680868994202E-19,1.,-1.18789542670764E-48));
#44748=DIRECTION('',(-5.15167520928809E-67,1.18789542670764E-48,1.));
#44749=DIRECTION('',(5.15167520928809E-67,-1.18789542670764E-48,-1.));
#44750=DIRECTION('center_axis',(5.15167520928809E-67,-1.18789542670764E-48,
-1.));
#44751=DIRECTION('ref_axis',(-4.33680868994202E-19,1.,-1.18789542670764E-48));
#44752=DIRECTION('center_axis',(5.15167520928809E-67,-1.18789542670764E-48,
-1.));
#44753=DIRECTION('ref_axis',(-4.33680868994202E-19,1.,-1.18789542670764E-48));
#44754=DIRECTION('',(-5.15167520928809E-67,1.18789542670764E-48,1.));
#44755=DIRECTION('',(5.15167520928809E-67,-1.18789542670764E-48,-1.));
#44756=DIRECTION('center_axis',(5.15167520928809E-67,-1.18789542670764E-48,
-1.));
#44757=DIRECTION('ref_axis',(-4.33680868994202E-19,1.,-1.18789542670764E-48));
#44758=DIRECTION('center_axis',(5.15167520928809E-67,-1.18789542670764E-48,
-1.));
#44759=DIRECTION('ref_axis',(-4.33680868994202E-19,1.,-1.18789542670764E-48));
#44760=DIRECTION('',(-5.15167520928809E-67,1.18789542670764E-48,1.));
#44761=DIRECTION('',(5.15167520928809E-67,-1.18789542670764E-48,-1.));
#44762=DIRECTION('center_axis',(5.15167520928809E-67,-1.18789542670764E-48,
-1.));
#44763=DIRECTION('ref_axis',(-4.33680868994202E-19,1.,-1.18789542670764E-48));
#44764=DIRECTION('center_axis',(5.15167520928809E-67,-1.18789542670764E-48,
-1.));
#44765=DIRECTION('ref_axis',(-4.33680868994202E-19,1.,-1.18789542670764E-48));
#44766=DIRECTION('',(-5.15167520928809E-67,1.18789542670764E-48,1.));
#44767=DIRECTION('',(5.15167520928809E-67,-1.18789542670764E-48,-1.));
#44768=DIRECTION('center_axis',(5.15167520928809E-67,-1.18789542670764E-48,
-1.));
#44769=DIRECTION('ref_axis',(-4.33680868994202E-19,1.,-1.18789542670764E-48));
#44770=DIRECTION('center_axis',(5.15167520928809E-67,-1.18789542670764E-48,
-1.));
#44771=DIRECTION('ref_axis',(-4.33680868994202E-19,1.,-1.18789542670764E-48));
#44772=DIRECTION('',(-5.15167520928809E-67,1.18789542670764E-48,1.));
#44773=DIRECTION('',(5.15167520928809E-67,-1.18789542670764E-48,-1.));
#44774=DIRECTION('center_axis',(5.15167520928809E-67,-1.18789542670764E-48,
-1.));
#44775=DIRECTION('ref_axis',(-4.33680868994202E-19,1.,-1.18789542670764E-48));
#44776=DIRECTION('center_axis',(5.15167520928809E-67,-1.18789542670764E-48,
-1.));
#44777=DIRECTION('ref_axis',(-4.33680868994202E-19,1.,-1.18789542670764E-48));
#44778=DIRECTION('',(-5.15167520928809E-67,1.18789542670764E-48,1.));
#44779=DIRECTION('',(5.15167520928809E-67,-1.18789542670764E-48,-1.));
#44780=DIRECTION('center_axis',(5.15167520928809E-67,-1.18789542670764E-48,
-1.));
#44781=DIRECTION('ref_axis',(-4.33680868994202E-19,1.,-1.18789542670764E-48));
#44782=DIRECTION('center_axis',(5.15167520928809E-67,-1.18789542670764E-48,
-1.));
#44783=DIRECTION('ref_axis',(-4.33680868994202E-19,1.,-1.18789542670764E-48));
#44784=DIRECTION('',(-5.15167520928809E-67,1.18789542670764E-48,1.));
#44785=DIRECTION('',(5.15167520928809E-67,-1.18789542670764E-48,-1.));
#44786=DIRECTION('center_axis',(5.15167520928809E-67,-1.18789542670764E-48,
-1.));
#44787=DIRECTION('ref_axis',(-4.33680868994202E-19,1.,-1.18789542670764E-48));
#44788=DIRECTION('center_axis',(5.15167520928809E-67,-1.18789542670764E-48,
-1.));
#44789=DIRECTION('ref_axis',(-4.33680868994202E-19,1.,-1.18789542670764E-48));
#44790=DIRECTION('',(-5.15167520928809E-67,1.18789542670764E-48,1.));
#44791=DIRECTION('',(5.15167520928809E-67,-1.18789542670764E-48,-1.));
#44792=DIRECTION('center_axis',(5.15167520928809E-67,-1.18789542670764E-48,
-1.));
#44793=DIRECTION('ref_axis',(-4.33680868994202E-19,1.,-1.18789542670764E-48));
#44794=DIRECTION('center_axis',(5.15167520928809E-67,-1.18789542670764E-48,
-1.));
#44795=DIRECTION('ref_axis',(-4.33680868994202E-19,1.,-1.18789542670764E-48));
#44796=DIRECTION('',(-5.15167520928809E-67,1.18789542670764E-48,1.));
#44797=DIRECTION('',(5.15167520928809E-67,-1.18789542670764E-48,-1.));
#44798=DIRECTION('center_axis',(5.15167520928809E-67,-1.18789542670764E-48,
-1.));
#44799=DIRECTION('ref_axis',(-4.33680868994202E-19,1.,-1.18789542670764E-48));
#44800=DIRECTION('center_axis',(5.15167520928809E-67,-1.18789542670764E-48,
-1.));
#44801=DIRECTION('ref_axis',(-4.33680868994202E-19,1.,-1.18789542670764E-48));
#44802=DIRECTION('',(-5.15167520928809E-67,1.18789542670764E-48,1.));
#44803=DIRECTION('',(5.15167520928809E-67,-1.18789542670764E-48,-1.));
#44804=DIRECTION('center_axis',(5.15167520928809E-67,-1.18789542670764E-48,
-1.));
#44805=DIRECTION('ref_axis',(-4.33680868994202E-19,1.,-1.18789542670764E-48));
#44806=DIRECTION('center_axis',(5.15167520928809E-67,-1.18789542670764E-48,
-1.));
#44807=DIRECTION('ref_axis',(-4.33680868994202E-19,1.,-1.18789542670764E-48));
#44808=DIRECTION('',(-5.15167520928809E-67,1.18789542670764E-48,1.));
#44809=DIRECTION('',(5.15167520928809E-67,-1.18789542670764E-48,-1.));
#44810=DIRECTION('center_axis',(5.15167520928809E-67,-1.18789542670764E-48,
-1.));
#44811=DIRECTION('ref_axis',(-4.33680868994202E-19,1.,-1.18789542670764E-48));
#44812=DIRECTION('center_axis',(5.15167520928809E-67,-1.18789542670764E-48,
-1.));
#44813=DIRECTION('ref_axis',(-4.33680868994202E-19,1.,-1.18789542670764E-48));
#44814=DIRECTION('',(-5.15167520928809E-67,1.18789542670764E-48,1.));
#44815=DIRECTION('',(5.15167520928809E-67,-1.18789542670764E-48,-1.));
#44816=DIRECTION('center_axis',(5.15167520928809E-67,-1.18789542670764E-48,
-1.));
#44817=DIRECTION('ref_axis',(-4.33680868994202E-19,1.,-1.18789542670764E-48));
#44818=DIRECTION('center_axis',(5.15167520928809E-67,-1.18789542670764E-48,
-1.));
#44819=DIRECTION('ref_axis',(-4.33680868994202E-19,1.,-1.18789542670764E-48));
#44820=DIRECTION('',(-5.15167520928809E-67,1.18789542670764E-48,1.));
#44821=DIRECTION('',(5.15167520928809E-67,-1.18789542670764E-48,-1.));
#44822=DIRECTION('center_axis',(5.15167520928809E-67,-1.18789542670764E-48,
-1.));
#44823=DIRECTION('ref_axis',(-4.33680868994202E-19,1.,-1.18789542670764E-48));
#44824=DIRECTION('center_axis',(5.15167520928809E-67,-1.18789542670764E-48,
-1.));
#44825=DIRECTION('ref_axis',(-4.33680868994202E-19,1.,-1.18789542670764E-48));
#44826=DIRECTION('',(-5.15167520928809E-67,1.18789542670764E-48,1.));
#44827=DIRECTION('',(5.15167520928809E-67,-1.18789542670764E-48,-1.));
#44828=DIRECTION('center_axis',(5.15167520928809E-67,-1.18789542670764E-48,
-1.));
#44829=DIRECTION('ref_axis',(-4.33680868994202E-19,1.,-1.18789542670764E-48));
#44830=DIRECTION('center_axis',(5.15167520928809E-67,-1.18789542670764E-48,
-1.));
#44831=DIRECTION('ref_axis',(-4.33680868994202E-19,1.,-1.18789542670764E-48));
#44832=DIRECTION('',(5.15167520928809E-67,-1.18789542670764E-48,-1.));
#44833=DIRECTION('center_axis',(5.15167520928809E-67,-1.18789542670764E-48,
-1.));
#44834=DIRECTION('ref_axis',(-4.33680868994202E-19,1.,-1.18789542670764E-48));
#44835=DIRECTION('',(-5.15167520928809E-67,1.18789542670764E-48,1.));
#44836=DIRECTION('center_axis',(5.15167520928809E-67,-1.18789542670764E-48,
-1.));
#44837=DIRECTION('ref_axis',(-4.33680868994202E-19,1.,-1.18789542670764E-48));
#44838=DIRECTION('',(5.15167520928809E-67,-1.18789542670764E-48,-1.));
#44839=DIRECTION('center_axis',(5.15167520928809E-67,-1.18789542670764E-48,
-1.));
#44840=DIRECTION('ref_axis',(-4.33680868994202E-19,1.,-1.18789542670764E-48));
#44841=DIRECTION('',(-5.15167520928809E-67,1.18789542670764E-48,1.));
#44842=DIRECTION('center_axis',(5.15167520928809E-67,-1.18789542670764E-48,
-1.));
#44843=DIRECTION('ref_axis',(-4.33680868994202E-19,1.,-1.18789542670764E-48));
#44844=DIRECTION('',(5.15167520928809E-67,-1.18789542670764E-48,-1.));
#44845=DIRECTION('center_axis',(5.15167520928809E-67,-1.18789542670764E-48,
-1.));
#44846=DIRECTION('ref_axis',(-4.33680868994202E-19,1.,-1.18789542670764E-48));
#44847=DIRECTION('',(-5.15167520928809E-67,1.18789542670764E-48,1.));
#44848=DIRECTION('center_axis',(5.15167520928809E-67,-1.18789542670764E-48,
-1.));
#44849=DIRECTION('ref_axis',(-4.33680868994202E-19,1.,-1.18789542670764E-48));
#44850=DIRECTION('',(5.15167520928809E-67,-1.18789542670764E-48,-1.));
#44851=DIRECTION('center_axis',(5.15167520928809E-67,-1.18789542670764E-48,
-1.));
#44852=DIRECTION('ref_axis',(-4.33680868994202E-19,1.,-1.18789542670764E-48));
#44853=DIRECTION('',(-5.15167520928809E-67,1.18789542670764E-48,1.));
#44854=DIRECTION('center_axis',(5.15167520928809E-67,-1.18789542670764E-48,
-1.));
#44855=DIRECTION('ref_axis',(-4.33680868994202E-19,1.,-1.18789542670764E-48));
#44856=DIRECTION('',(5.15167520928809E-67,-1.18789542670764E-48,-1.));
#44857=DIRECTION('center_axis',(5.15167520928809E-67,-1.18789542670764E-48,
-1.));
#44858=DIRECTION('ref_axis',(-4.33680868994202E-19,1.,-1.18789542670764E-48));
#44859=DIRECTION('',(-5.15167520928809E-67,1.18789542670764E-48,1.));
#44860=DIRECTION('center_axis',(5.15167520928809E-67,-1.18789542670764E-48,
-1.));
#44861=DIRECTION('ref_axis',(-4.33680868994202E-19,1.,-1.18789542670764E-48));
#44862=DIRECTION('',(5.15167520928809E-67,-1.18789542670764E-48,-1.));
#44863=DIRECTION('center_axis',(5.15167520928809E-67,-1.18789542670764E-48,
-1.));
#44864=DIRECTION('ref_axis',(-4.33680868994202E-19,1.,-1.18789542670764E-48));
#44865=DIRECTION('',(-5.15167520928809E-67,1.18789542670764E-48,1.));
#44866=DIRECTION('center_axis',(5.15167520928809E-67,-1.18789542670764E-48,
-1.));
#44867=DIRECTION('ref_axis',(-4.33680868994202E-19,1.,-1.18789542670764E-48));
#44868=DIRECTION('',(5.15167520928809E-67,-1.18789542670764E-48,-1.));
#44869=DIRECTION('center_axis',(5.15167520928809E-67,-1.18789542670764E-48,
-1.));
#44870=DIRECTION('ref_axis',(-4.33680868994202E-19,1.,-1.18789542670764E-48));
#44871=DIRECTION('',(-5.15167520928809E-67,1.18789542670764E-48,1.));
#44872=DIRECTION('center_axis',(5.15167520928809E-67,-1.18789542670764E-48,
-1.));
#44873=DIRECTION('ref_axis',(-4.33680868994202E-19,1.,-1.18789542670764E-48));
#44874=DIRECTION('',(5.15167520928809E-67,-1.18789542670764E-48,-1.));
#44875=DIRECTION('center_axis',(5.15167520928809E-67,-1.18789542670764E-48,
-1.));
#44876=DIRECTION('ref_axis',(-4.33680868994202E-19,1.,-1.18789542670764E-48));
#44877=DIRECTION('',(-5.15167520928809E-67,1.18789542670764E-48,1.));
#44878=DIRECTION('center_axis',(5.15167520928809E-67,-1.18789542670764E-48,
-1.));
#44879=DIRECTION('ref_axis',(-4.33680868994202E-19,1.,-1.18789542670764E-48));
#44880=DIRECTION('',(5.15167520928809E-67,-1.18789542670764E-48,-1.));
#44881=DIRECTION('center_axis',(5.15167520928809E-67,-1.18789542670764E-48,
-1.));
#44882=DIRECTION('ref_axis',(-4.33680868994202E-19,1.,-1.18789542670764E-48));
#44883=DIRECTION('',(-5.15167520928809E-67,1.18789542670764E-48,1.));
#44884=DIRECTION('center_axis',(5.15167520928809E-67,-1.18789542670764E-48,
-1.));
#44885=DIRECTION('ref_axis',(-4.33680868994202E-19,1.,-1.18789542670764E-48));
#44886=DIRECTION('',(5.15167520928809E-67,-1.18789542670764E-48,-1.));
#44887=DIRECTION('center_axis',(5.15167520928809E-67,-1.18789542670764E-48,
-1.));
#44888=DIRECTION('ref_axis',(-4.33680868994202E-19,1.,-1.18789542670764E-48));
#44889=DIRECTION('',(-5.15167520928809E-67,1.18789542670764E-48,1.));
#44890=DIRECTION('center_axis',(5.15167520928809E-67,-1.18789542670764E-48,
-1.));
#44891=DIRECTION('ref_axis',(-4.33680868994202E-19,1.,-1.18789542670764E-48));
#44892=DIRECTION('',(5.15167520928809E-67,-1.18789542670764E-48,-1.));
#44893=DIRECTION('center_axis',(5.15167520928809E-67,-1.18789542670764E-48,
-1.));
#44894=DIRECTION('ref_axis',(-4.33680868994202E-19,1.,-1.18789542670764E-48));
#44895=DIRECTION('',(-5.15167520928809E-67,1.18789542670764E-48,1.));
#44896=DIRECTION('center_axis',(5.15167520928809E-67,-1.18789542670764E-48,
-1.));
#44897=DIRECTION('ref_axis',(-4.33680868994202E-19,1.,-1.18789542670764E-48));
#44898=DIRECTION('',(5.15167520928809E-67,-1.18789542670764E-48,-1.));
#44899=DIRECTION('center_axis',(5.15167520928809E-67,-1.18789542670764E-48,
-1.));
#44900=DIRECTION('ref_axis',(-4.33680868994202E-19,1.,-1.18789542670764E-48));
#44901=DIRECTION('',(-5.15167520928809E-67,1.18789542670764E-48,1.));
#44902=DIRECTION('center_axis',(5.15167520928809E-67,-1.18789542670764E-48,
-1.));
#44903=DIRECTION('ref_axis',(-4.33680868994202E-19,1.,-1.18789542670764E-48));
#44904=DIRECTION('',(5.15167520928809E-67,-1.18789542670764E-48,-1.));
#44905=DIRECTION('center_axis',(5.15167520928809E-67,-1.18789542670764E-48,
-1.));
#44906=DIRECTION('ref_axis',(-4.33680868994202E-19,1.,-1.18789542670764E-48));
#44907=DIRECTION('',(-5.15167520928809E-67,1.18789542670764E-48,1.));
#44908=DIRECTION('center_axis',(5.15167520928809E-67,-1.18789542670764E-48,
-1.));
#44909=DIRECTION('ref_axis',(-4.33680868994202E-19,1.,-1.18789542670764E-48));
#44910=DIRECTION('',(5.15167520928809E-67,-1.18789542670764E-48,-1.));
#44911=DIRECTION('center_axis',(5.15167520928809E-67,-1.18789542670764E-48,
-1.));
#44912=DIRECTION('ref_axis',(-4.33680868994202E-19,1.,-1.18789542670764E-48));
#44913=DIRECTION('',(-5.15167520928809E-67,1.18789542670764E-48,1.));
#44914=DIRECTION('center_axis',(5.15167520928809E-67,-1.18789542670764E-48,
-1.));
#44915=DIRECTION('ref_axis',(-4.33680868994202E-19,1.,-1.18789542670764E-48));
#44916=DIRECTION('',(-5.15167520928809E-67,1.18789542670764E-48,1.));
#44917=DIRECTION('',(5.15167520928809E-67,-1.18789542670764E-48,-1.));
#44918=DIRECTION('center_axis',(5.15167520928809E-67,-1.18789542670764E-48,
-1.));
#44919=DIRECTION('ref_axis',(-4.33680868994202E-19,1.,-1.18789542670764E-48));
#44920=DIRECTION('center_axis',(5.15167520928809E-67,-1.18789542670764E-48,
-1.));
#44921=DIRECTION('ref_axis',(0.,1.,0.));
#44922=DIRECTION('center_axis',(-0.726718511656259,-0.686935363550879,-0.000105448246390915));
#44923=DIRECTION('ref_axis',(0.686885008270217,-0.726663364190208,-0.0122204974282148));
#44924=DIRECTION('center_axis',(0.0503511057571476,0.998731574514185,-9.06501463958382E-5));
#44925=DIRECTION('ref_axis',(0.998626750226923,-0.0503471356586858,-0.0144837723739379));
#44926=DIRECTION('center_axis',(5.15167520928809E-67,-1.18789542670764E-48,
-1.));
#44927=DIRECTION('ref_axis',(0.,1.,0.));
#44928=DIRECTION('center_axis',(-0.0281636861094737,0.999603320606368,-9.06501463234301E-5));
#44929=DIRECTION('ref_axis',(0.999498507968587,0.0281594195507115,-0.0144837722688343));
#44930=DIRECTION('center_axis',(-0.670581953565459,-0.741835448352935,-0.000105448247414229));
#44931=DIRECTION('ref_axis',(0.741780921484837,-0.670530926934418,-0.0122204969447688));
#44932=DIRECTION('center_axis',(5.15167520928809E-67,-1.18789542670764E-48,
-1.));
#44933=DIRECTION('ref_axis',(0.,1.,0.));
#44934=DIRECTION('center_axis',(-0.106504839485416,0.994312179825198,-9.06501464431132E-5));
#44935=DIRECTION('ref_axis',(0.994208025038947,0.106492362574112,-0.014483772351861));
#44936=DIRECTION('center_axis',(-0.610311034741592,-0.792161870928735,-0.000105448247339917));
#44937=DIRECTION('ref_axis',(0.792103508645573,-0.610264443537491,-0.0122204969313235));
#44938=DIRECTION('center_axis',(5.15167520928809E-67,-1.18789542670764E-48,
-1.));
#44939=DIRECTION('ref_axis',(0.,1.,0.));
#44940=DIRECTION('center_axis',(-0.184189355109993,0.982890773812999,-9.06501463311491E-5));
#44941=DIRECTION('ref_axis',(0.982787919029266,0.184168744770673,-0.0144837722890199));
#44942=DIRECTION('center_axis',(-0.546277345439217,-0.837604352149957,-0.000105448247410497));
#44943=DIRECTION('ref_axis',(0.837542514274823,-0.546235476912428,-0.0122204968991007));
#44944=DIRECTION('center_axis',(5.15167520928809E-67,-1.18789542670764E-48,
-1.));
#44945=DIRECTION('ref_axis',(0.,1.,0.));
#44946=DIRECTION('center_axis',(-0.260738282110594,0.965409519336,-9.0650146457266E-5));
#44947=DIRECTION('ref_axis',(0.965308598686112,0.260709665412272,-0.0144837724117514));
#44948=DIRECTION('center_axis',(-0.478875674647023,-0.877882724008182,-0.000105448247224529));
#44949=DIRECTION('ref_axis',(0.877817791791478,-0.478838786930502,-0.0122204969317693));
#44950=DIRECTION('center_axis',(5.15167520928809E-67,-1.18789542670764E-48,
-1.));
#44951=DIRECTION('ref_axis',(0.,1.,0.));
#44952=DIRECTION('center_axis',(-0.335679670898074,0.941976194140973,-9.06501464082373E-5));
#44953=DIRECTION('ref_axis',(0.941877829837014,0.335643224272907,-0.014483772340284));
#44954=DIRECTION('center_axis',(-0.40852157607848,-0.912748656947257,-0.000105448246964389));
#44955=DIRECTION('ref_axis',(0.912681030716442,-0.408489896596762,-0.0122204970741974));
#44956=DIRECTION('center_axis',(5.15167520928809E-67,-1.18789542670764E-48,
-1.));
#44957=DIRECTION('ref_axis',(0.,1.,0.));
#44958=DIRECTION('center_axis',(-0.408551482889657,0.91273527247018,-9.06501463992171E-5));
#44959=DIRECTION('ref_axis',(0.91264007096006,0.408507431043052,-0.014483772320157));
#44960=DIRECTION('center_axis',(-0.335648806144879,-0.941987190897087,-0.000105448247367288));
#44961=DIRECTION('ref_axis',(0.941917287594001,-0.335622530214118,-0.0122204968897907));
#44962=DIRECTION('center_axis',(5.15167520928809E-67,-1.18789542670764E-48,
-1.));
#44963=DIRECTION('ref_axis',(0.,1.,0.));
#44964=DIRECTION('center_axis',(-0.478904439132113,0.877867034329292,-9.06501463430316E-5));
#44965=DIRECTION('ref_axis',(0.877775582560928,0.478853053657823,-0.0144837723815965));
#44966=DIRECTION('center_axis',(-0.260706649707894,-0.965418060572078,-0.000105448247265905));
#44967=DIRECTION('ref_axis',(0.965346311170054,-0.260685939326527,-0.0122204970363453));
#44968=DIRECTION('center_axis',(5.15167520928809E-67,-1.18789542670764E-48,
-1.));
#44969=DIRECTION('ref_axis',(0.,1.,0.));
#44970=DIRECTION('center_axis',(-0.546304790255147,0.837586454001514,-9.06501464163507E-5));
#44971=DIRECTION('ref_axis',(0.837499315806636,0.546246387962313,-0.0144837723519214));
#44972=DIRECTION('center_axis',(-0.184157150081311,-0.982896806869672,-0.00010544824733539));
#44973=DIRECTION('ref_axis',(0.982823653730718,-0.184142132936614,-0.012220496919376));
#44974=DIRECTION('center_axis',(5.15167520928809E-67,-1.18789542670764E-48,
-1.));
#44975=DIRECTION('ref_axis',(0.,1.,0.));
#44976=DIRECTION('center_axis',(-0.610336990681852,0.792141874658809,-9.06501463120476E-5));
#44977=DIRECTION('ref_axis',(0.792059587273495,0.610271931640219,-0.0144837723075503));
#44978=DIRECTION('center_axis',(-0.106472260385922,-0.994315667506542,-0.000105448247451369));
#44979=DIRECTION('ref_axis',(0.994241561642557,-0.106463029063183,-0.0122204969318448));
#44980=DIRECTION('center_axis',(5.15167520928809E-67,-1.18789542670764E-48,
-1.));
#44981=DIRECTION('ref_axis',(0.,1.,0.));
#44982=DIRECTION('center_axis',(-0.670606260603123,0.741813477245087,-9.06501463072396E-5));
#44983=DIRECTION('ref_axis',(0.741736547997548,0.670534945922644,-0.0144837723400245));
#44984=DIRECTION('center_axis',(-0.0281309338001256,-0.999604241409669,
-0.000105448247349234));
#44985=DIRECTION('ref_axis',(0.999529639708615,-0.0281275452135709,-0.012220496889411));
#44986=DIRECTION('center_axis',(5.15167520928809E-67,-1.18789542670764E-48,
-1.));
#44987=DIRECTION('ref_axis',(0.,1.,0.));
#44988=DIRECTION('center_axis',(-0.726741019928497,0.686911553066215,-9.0650146372247E-5));
#44989=DIRECTION('ref_axis',(0.686840456250864,0.726663889287803,-0.014483772375632));
#44990=DIRECTION('center_axis',(0.0503838293471008,-0.9987299227624,-0.000105448247268434));
#44991=DIRECTION('ref_axis',(0.998655285167451,0.0503813543057433,-0.0122204969390446));
#44992=DIRECTION('center_axis',(5.15167520928809E-67,-1.18789542670764E-48,
-1.));
#44993=DIRECTION('ref_axis',(0.,1.,0.));
#44994=DIRECTION('center_axis',(-0.77839517919999,0.627774590741587,-9.06501465192481E-5));
#44995=DIRECTION('ref_axis',(0.62770976469511,0.778312708136478,-0.0144837722873138));
#44996=DIRECTION('center_axis',(0.128587959432554,-0.991698102029866,-0.000105448247403937));
#44997=DIRECTION('ref_axis',(0.991623888707038,0.128579636022696,-0.0122204969540051));
#44998=DIRECTION('center_axis',(5.15167520928809E-67,-1.18789542670764E-48,
-1.));
#44999=DIRECTION('ref_axis',(0.,1.,0.));
#45000=DIRECTION('center_axis',(-0.825250273349494,0.564767189308247,-9.06501463546308E-5));
#45001=DIRECTION('ref_axis',(0.564709033703414,0.82516297032304,-0.0144837723475052));
#45002=DIRECTION('center_axis',(0.205999301987418,-0.978552132725367,-0.000105448247113811));
#45003=DIRECTION('ref_axis',(0.978478801224233,0.205985181525565,-0.0122204969893998));
#45004=DIRECTION('center_axis',(5.15167520928809E-67,-1.18789542670764E-48,
-1.));
#45005=DIRECTION('ref_axis',(0.,1.,0.));
#45006=DIRECTION('center_axis',(-0.867017425140065,0.498277810348848,-9.06501462870057E-5));
#45007=DIRECTION('ref_axis',(0.498226683734515,0.866925828402957,-0.0144837723937473));
#45008=DIRECTION('center_axis',(0.282140590344591,-0.959373064120873,-0.000105448247263863));
#45009=DIRECTION('ref_axis',(0.959301066555575,0.282120759888322,-0.0122204969363817));
#45010=DIRECTION('center_axis',(5.15167520928809E-67,-1.18789542670764E-48,
-1.));
#45011=DIRECTION('ref_axis',(0.,1.,0.));
#45012=DIRECTION('center_axis',(-0.903439126191882,0.428716382994866,-9.06501464245823E-5));
#45013=DIRECTION('ref_axis',(0.42867260058449,0.903343800470088,-0.0144837723120868));
#45014=DIRECTION('center_axis',(0.356542388140961,-0.934279141552142,-0.000105448247299974));
#45015=DIRECTION('ref_axis',(0.934208921811354,0.356516969951643,-0.0122204969034503));
#45016=DIRECTION('center_axis',(5.15167520928809E-67,-1.18789542670764E-48,
-1.));
#45017=DIRECTION('ref_axis',(0.,1.,0.));
#45018=DIRECTION('center_axis',(-0.934290824606917,0.356511776576704,-9.06501463905499E-5));
#45019=DIRECTION('ref_axis',(0.356475608302988,0.934192357614636,-0.0144837722787681));
#45020=DIRECTION('center_axis',(0.428745983551553,-0.903425077396614,-0.000105448247174382));
#45021=DIRECTION('ref_axis',(0.903357068407879,0.428715134340607,-0.0122204969145006));
#45022=DIRECTION('center_axis',(5.15167520928809E-67,-1.18789542670764E-48,
-1.));
#45023=DIRECTION('ref_axis',(0.,1.,0.));
#45024=DIRECTION('center_axis',(-0.959382309405018,0.282109156503729,-9.06501463332588E-5));
#45025=DIRECTION('ref_axis',(0.282080825355611,0.959281308222547,-0.0144837723517365));
#45026=DIRECTION('center_axis',(0.498306217395032,-0.867001097223137,-0.000105448243846677));
#45027=DIRECTION('ref_axis',(0.866935718268405,0.498270127348975,-0.0122204984383232));
#45028=DIRECTION('center_axis',(5.15167520928809E-67,-1.18789542670764E-48,
-1.));
#45029=DIRECTION('ref_axis',(0.,1.,0.));
#45030=DIRECTION('center_axis',(-0.978558883238511,0.205967239670656,-9.06501465473592E-5));
#45031=DIRECTION('ref_axis',(0.205946920319669,0.978455970573743,-0.0144837722792749));
#45032=DIRECTION('center_axis',(0.564794227716619,-0.825231766971349,-0.000105448246777006));
#45033=DIRECTION('ref_axis',(0.825169421163283,0.564753119359096,-0.01222049717581));
#45034=DIRECTION('center_axis',(5.15167520928809E-67,-1.18789542670764E-48,
-1.));
#45035=DIRECTION('ref_axis',(0.,1.,0.));
#45036=DIRECTION('center_axis',(-0.991702316153162,0.128555466313202,-9.0650146420716E-5));
#45037=DIRECTION('ref_axis',(0.128543284034494,0.991598126494967,-0.0144837723435229));
#45038=DIRECTION('center_axis',(0.627800093806525,-0.778374608461238,-0.000105448247294656));
#45039=DIRECTION('ref_axis',(0.778315680171741,0.627754220578766,-0.012220496894383));
#45040=DIRECTION('center_axis',(5.15167520928809E-67,-1.18789542670764E-48,
-1.));
#45041=DIRECTION('ref_axis',(0.,1.,0.));
#45042=DIRECTION('center_axis',(-0.998731574514195,0.0503511057569474,-9.06501463044587E-5));
#45043=DIRECTION('ref_axis',(0.0503471356585215,0.998626750227776,-0.0144837723156803));
#45044=DIRECTION('center_axis',(0.686935363552588,-0.726718511654644,-0.000105448247440854));
#45045=DIRECTION('ref_axis',(0.726663364192637,0.6868850082757,-0.0122204969756106));
#45046=DIRECTION('center_axis',(5.15167520928809E-67,-1.18789542670764E-48,
-1.));
#45047=DIRECTION('ref_axis',(0.,1.,0.));
#45048=DIRECTION('center_axis',(-0.99960332060638,-0.0281636861090561,-9.06501465204533E-5));
#45049=DIRECTION('ref_axis',(0.0281594195503036,-0.999498507968962,0.0144837722437162));
#45050=DIRECTION('center_axis',(0.741835448352776,-0.670581953565635,-0.000105448247295083));
#45051=DIRECTION('ref_axis',(0.67053092693442,0.741780921484487,-0.0122204969658991));
#45052=DIRECTION('center_axis',(5.15167520928809E-67,-1.18789542670764E-48,
-1.));
#45053=DIRECTION('ref_axis',(0.,1.,0.));
#45054=DIRECTION('center_axis',(-0.994312179825187,-0.106504839485521,-9.0650146389517E-5));
#45055=DIRECTION('ref_axis',(0.106492362574174,-0.994208025038546,0.0144837723789195));
#45056=DIRECTION('center_axis',(0.792161870927703,-0.610311034742932,-0.000105448246562834));
#45057=DIRECTION('ref_axis',(0.610264443536631,0.792103508641721,-0.0122204972240042));
#45058=DIRECTION('center_axis',(5.15167520928809E-67,-1.18789542670764E-48,
-1.));
#45059=DIRECTION('ref_axis',(0.,1.,0.));
#45060=DIRECTION('center_axis',(-0.982890773812962,-0.18418935511019,-9.06501462458389E-5));
#45061=DIRECTION('ref_axis',(0.184168744770736,-0.982787919028534,0.0144837723378535));
#45062=DIRECTION('center_axis',(0.837604352149828,-0.546277345439416,-0.000105448247288724));
#45063=DIRECTION('ref_axis',(0.546235476912052,0.837542514273825,-0.0122204969843265));
#45064=DIRECTION('center_axis',(5.15167520928809E-67,-1.18789542670764E-48,
-1.));
#45065=DIRECTION('ref_axis',(0.,1.,0.));
#45066=DIRECTION('center_axis',(-0.965409519335916,-0.260738282110905,-9.06501463158079E-5));
#45067=DIRECTION('ref_axis',(0.260709665413015,-0.965308598687581,0.0144837723005081));
#45068=DIRECTION('center_axis',(0.877882724007609,-0.478875674648073,-0.000105448246644854));
#45069=DIRECTION('ref_axis',(0.47883878693024,0.877817791788535,-0.012220497153411));
#45070=DIRECTION('center_axis',(5.15167520928809E-67,-1.18789542670764E-48,
-1.));
#45071=DIRECTION('ref_axis',(0.,1.,0.));
#45072=DIRECTION('center_axis',(-0.941976194141077,-0.335679670897783,-9.06501465752214E-5));
#45073=DIRECTION('ref_axis',(0.335643224272825,-0.941877829837701,0.0144837722974511));
#45074=DIRECTION('center_axis',(0.912748656947635,-0.408521576077636,-0.000105448247395522));
#45075=DIRECTION('ref_axis',(0.408489896596716,0.912681030718573,-0.0122204969165703));
#45076=DIRECTION('center_axis',(5.15167520928809E-67,-1.18789542670764E-48,
-1.));
#45077=DIRECTION('ref_axis',(0.,1.,0.));
#45078=DIRECTION('center_axis',(-0.912735272470059,-0.408551482889927,-9.0650146236208E-5));
#45079=DIRECTION('ref_axis',(0.408507431042893,-0.912640070958992,0.0144837723919199));
#45080=DIRECTION('center_axis',(0.941987190897161,-0.335648806144671,-0.000105448247475279));
#45081=DIRECTION('ref_axis',(0.335622530214028,0.941917287594399,-0.0122204968616106));
#45082=DIRECTION('center_axis',(5.15167520928809E-67,-1.18789542670764E-48,
-1.));
#45083=DIRECTION('ref_axis',(0.,1.,0.));
#45084=DIRECTION('center_axis',(-0.877867034329361,-0.478904439131988,-9.06501463610722E-5));
#45085=DIRECTION('ref_axis',(0.478853053657853,-0.877775582561276,0.0144837723595397));
#45086=DIRECTION('center_axis',(0.965418060572122,-0.260706649707733,-0.000105448247352975));
#45087=DIRECTION('ref_axis',(0.260685939326823,0.965346311171741,-0.012220496896787));
#45088=DIRECTION('center_axis',(5.15167520928809E-67,-1.18789542670764E-48,
-1.));
#45089=DIRECTION('ref_axis',(0.,1.,0.));
#45090=DIRECTION('center_axis',(-0.837586454001461,-0.546304790255229,-9.06501463408637E-5));
#45091=DIRECTION('ref_axis',(0.54624638796239,-0.837499315806573,0.0144837723526967));
#45092=DIRECTION('center_axis',(0.982896806869685,-0.184157150081241,-0.000105448247384682));
#45093=DIRECTION('ref_axis',(0.184142132936524,0.982823653730634,-0.0122204969274716));
#45094=DIRECTION('center_axis',(5.15167520928809E-67,-1.18789542670764E-48,
-1.));
#45095=DIRECTION('ref_axis',(0.,1.,0.));
#45096=DIRECTION('center_axis',(-0.792141874658961,-0.610336990681655,-9.06501464140886E-5));
#45097=DIRECTION('ref_axis',(0.610271931639049,-0.792059587272402,0.0144837724166105));
#45098=DIRECTION('center_axis',(0.994315667506523,-0.1064722603861,-0.000105448247372999));
#45099=DIRECTION('ref_axis',(0.106463029063429,0.994241561643113,-0.0122204968844733));
#45100=DIRECTION('center_axis',(5.15167520928809E-67,-1.18789542670764E-48,
-1.));
#45101=DIRECTION('ref_axis',(0.,1.,0.));
#45102=DIRECTION('center_axis',(-0.741813477245026,-0.670606260603191,-9.06501462657205E-5));
#45103=DIRECTION('ref_axis',(0.670534945922615,-0.741736547997381,0.0144837723499451));
#45104=DIRECTION('center_axis',(0.999604241409683,-0.0281309337996267,-0.000105448247542078));
#45105=DIRECTION('ref_axis',(0.0281275452130772,0.999529639708833,-0.0122204968727785));
#45106=DIRECTION('center_axis',(5.15167520928809E-67,-1.18789542670764E-48,
-1.));
#45107=DIRECTION('ref_axis',(0.,1.,0.));
#45108=DIRECTION('center_axis',(-0.686911553066313,-0.726741019928404,-9.0650146445407E-5));
#45109=DIRECTION('ref_axis',(0.726663889287897,-0.686840456251137,0.0144837723579623));
#45110=DIRECTION('center_axis',(0.998729922762429,0.0503838293465177,-0.00010544824700806));
#45111=DIRECTION('ref_axis',(0.0503813543051317,-0.998655285166875,0.0122204969886123));
#45112=DIRECTION('center_axis',(5.15167520928809E-67,-1.18789542670764E-48,
-1.));
#45113=DIRECTION('ref_axis',(0.,1.,0.));
#45114=DIRECTION('center_axis',(-0.627774590741284,-0.778395179200234,-9.06501463091932E-5));
#45115=DIRECTION('ref_axis',(0.778312708136324,-0.627709764694486,0.014483772322638));
#45116=DIRECTION('center_axis',(0.991698102029894,0.128587959432343,-0.000105448247307732));
#45117=DIRECTION('ref_axis',(0.128579636022594,-0.991623888707978,0.0122204968787672));
#45118=DIRECTION('center_axis',(5.15167520928809E-67,-1.18789542670764E-48,
-1.));
#45119=DIRECTION('ref_axis',(0.,1.,0.));
#45120=DIRECTION('center_axis',(-0.564767189308512,-0.825250273349312,-9.06501464604225E-5));
#45121=DIRECTION('ref_axis',(0.825162970323365,-0.564709033704023,0.014483772305219));
#45122=DIRECTION('center_axis',(0.978552132725239,0.205999301988023,-0.000105448247439453));
#45123=DIRECTION('ref_axis',(0.205985181526365,-0.978478801225051,0.0122204969104439));
#45124=DIRECTION('center_axis',(5.15167520928809E-67,-1.18789542670764E-48,
-1.));
#45125=DIRECTION('ref_axis',(0.,1.,0.));
#45126=DIRECTION('center_axis',(-0.498277810349565,-0.867017425139653,-9.06501466563663E-5));
#45127=DIRECTION('ref_axis',(0.86692582840462,-0.498226683736414,0.0144837722289047));
#45128=DIRECTION('center_axis',(0.959373064120893,0.282140590344525,-0.00010544824722367));
#45129=DIRECTION('ref_axis',(0.282120759888269,-0.959301066555644,0.0122204969322086));
#45130=DIRECTION('center_axis',(5.15167520928809E-67,-1.18789542670764E-48,
-1.));
#45131=DIRECTION('ref_axis',(0.,1.,0.));
#45132=DIRECTION('center_axis',(-0.428716382994794,-0.903439126191916,-9.06501464376821E-5));
#45133=DIRECTION('ref_axis',(0.903343800470677,-0.428672600584677,0.0144837722698243));
#45134=DIRECTION('center_axis',(0.934279141552165,0.356542388140901,-0.000105448247303552));
#45135=DIRECTION('ref_axis',(0.356516969951467,-0.934208921811066,0.0122204969306124));
#45136=DIRECTION('center_axis',(5.15167520928809E-67,-1.18789542670764E-48,
-1.));
#45137=DIRECTION('ref_axis',(0.,1.,0.));
#45138=DIRECTION('center_axis',(-0.356511776576584,-0.934290824606963,-9.06501462973138E-5));
#45139=DIRECTION('ref_axis',(0.9341923576135,-0.356475608302424,0.0144837723659048));
#45140=DIRECTION('center_axis',(0.903425077396469,0.42874598355186,-0.000105448247323971));
#45141=DIRECTION('ref_axis',(0.428715134340782,-0.903357068407445,0.0122204969404582));
#45142=DIRECTION('center_axis',(5.15167520928809E-67,-1.18789542670764E-48,
-1.));
#45143=DIRECTION('ref_axis',(0.,1.,0.));
#45144=DIRECTION('center_axis',(-0.282109156503611,-0.959382309405053,-9.06501462853803E-5));
#45145=DIRECTION('ref_axis',(0.959281308222382,-0.282080825355435,0.0144837723660616));
#45146=DIRECTION('center_axis',(0.867001097223284,0.498306217394775,-0.000105448243705777));
#45147=DIRECTION('ref_axis',(0.498270127348596,-0.86693571826834,0.0122204984583659));
#45148=DIRECTION('center_axis',(5.15167520928809E-67,-1.18789542670764E-48,
-1.));
#45149=DIRECTION('ref_axis',(0.,1.,0.));
#45150=DIRECTION('center_axis',(-0.205967239670074,-0.978558883238633,-9.06501462899978E-5));
#45151=DIRECTION('ref_axis',(0.978455970573443,-0.205946920318997,0.0144837723091262));
#45152=DIRECTION('center_axis',(0.825231766971361,0.564794227716602,-0.000105448246768021));
#45153=DIRECTION('ref_axis',(0.56475311935916,-0.825169421163415,0.0122204971638891));
#45154=DIRECTION('center_axis',(5.15167520928809E-67,-1.18789542670764E-48,
-1.));
#45155=DIRECTION('ref_axis',(0.,1.,0.));
#45156=DIRECTION('center_axis',(-0.128555466313085,-0.991702316153177,-9.06501463759606E-5));
#45157=DIRECTION('ref_axis',(0.991598126495219,-0.128543284034406,0.014483772327091));
#45158=DIRECTION('center_axis',(0.778374608461285,0.627800093806467,-0.000105448247278628));
#45159=DIRECTION('ref_axis',(0.627754220578617,-0.778315680171672,0.0122204969064386));
#45160=DIRECTION('center_axis',(5.15167520928809E-67,-1.18789542670764E-48,
-1.));
#45161=DIRECTION('ref_axis',(0.,1.,0.));
#45162=DIRECTION('center_axis',(-0.0503511057568215,-0.998731574514202,
-9.06501462140748E-5));
#45163=DIRECTION('ref_axis',(0.998626750226433,-0.0503471356583347,0.0144837724089729));
#45164=DIRECTION('center_axis',(0.72671851165485,0.686935363552371,-0.000105448247305609));
#45165=DIRECTION('ref_axis',(0.68688500827568,-0.726663364193057,0.0122204969517677));
#45166=DIRECTION('center_axis',(5.15167520928809E-67,-1.18789542670764E-48,
-1.));
#45167=DIRECTION('ref_axis',(0.,1.,0.));
#45168=DIRECTION('center_axis',(0.028163686109212,-0.999603320606376,-9.06501464412085E-5));
#45169=DIRECTION('ref_axis',(0.999498507967367,0.0281594195504058,0.0144837723535955));
#45170=DIRECTION('center_axis',(0.670581953565646,0.741835448352765,-0.000105448247317749));
#45171=DIRECTION('ref_axis',(0.741780921484837,-0.670530926934763,0.0122204969257884));
#45172=DIRECTION('center_axis',(5.15167520928809E-67,-1.18789542670764E-48,
-1.));
#45173=DIRECTION('ref_axis',(0.,1.,0.));
#45174=DIRECTION('center_axis',(0.106504839485654,-0.994312179825173,-9.06501463242885E-5));
#45175=DIRECTION('ref_axis',(0.994208025039066,0.106492362574368,0.0144837723417732));
#45176=DIRECTION('center_axis',(0.610311034742769,0.792161870927829,-0.000105448246632335));
#45177=DIRECTION('ref_axis',(0.792103508641049,-0.610264443535841,0.012220497306985));
#45178=DIRECTION('center_axis',(5.15167520928809E-67,-1.18789542670764E-48,
-1.));
#45179=DIRECTION('ref_axis',(0.,1.,0.));
#45180=DIRECTION('center_axis',(0.184189355110076,-0.982890773812984,-9.06501463014399E-5));
#45181=DIRECTION('ref_axis',(0.982787919027527,0.184168744770422,0.0144837724102069));
#45182=DIRECTION('center_axis',(0.546277345439608,0.837604352149702,-0.000105448247164003));
#45183=DIRECTION('ref_axis',(0.837542514274121,-0.546235476912526,0.0122204969428009));
#45184=DIRECTION('center_axis',(5.15167520928809E-67,-1.18789542670764E-48,
-1.));
#45185=DIRECTION('ref_axis',(0.,1.,0.));
#45186=DIRECTION('center_axis',(0.260738282110494,-0.965409519336027,-9.06501465102787E-5));
#45187=DIRECTION('ref_axis',(0.965308598687087,0.260709665412434,0.0144837723438797));
#45188=DIRECTION('center_axis',(0.47887567464682,0.877882724008293,-0.000105448247318393));
#45189=DIRECTION('ref_axis',(0.877817791791359,-0.47883878693017,0.0122204969532827));
#45190=DIRECTION('center_axis',(5.15167520928809E-67,-1.18789542670764E-48,
-1.));
#45191=DIRECTION('ref_axis',(0.,1.,0.));
#45192=DIRECTION('center_axis',(0.335679670898317,-0.941976194140886,-9.06501463025926E-5));
#45193=DIRECTION('ref_axis',(0.941877829837149,0.335643224273232,0.0144837723239312));
#45194=DIRECTION('center_axis',(0.408521576078182,0.912748656947391,-0.000105448247109452));
#45195=DIRECTION('ref_axis',(0.912681030717227,-0.408489896596761,0.0122204970155898));
#45196=DIRECTION('center_axis',(5.15167520928809E-67,-1.18789542670764E-48,
-1.));
#45197=DIRECTION('ref_axis',(0.,1.,0.));
#45198=DIRECTION('center_axis',(0.40855148288974,-0.912735272470143,-9.06501463607514E-5));
#45199=DIRECTION('ref_axis',(0.912640070959719,0.408507431042997,0.0144837723432182));
#45200=DIRECTION('center_axis',(0.33564880614496,0.941987190897058,-0.00010544824731253));
#45201=DIRECTION('ref_axis',(0.941917287593217,-0.335622530213924,0.0122204969555834));
#45202=DIRECTION('center_axis',(5.15167520928809E-67,-1.18789542670764E-48,
-1.));
#45203=DIRECTION('ref_axis',(0.,1.,0.));
#45204=DIRECTION('center_axis',(0.47890443913187,-0.877867034329425,-9.06501464476592E-5));
#45205=DIRECTION('ref_axis',(0.877775582561568,0.47885305365786,0.0144837723415746));
#45206=DIRECTION('center_axis',(0.260706649725499,0.965418060567325,-0.000105448239035086));
#45207=DIRECTION('ref_axis',(0.965346311123191,-0.260685939332472,0.0122205006114622));
#45208=DIRECTION('center_axis',(5.15167520928809E-67,-1.18789542670764E-48,
-1.));
#45209=DIRECTION('ref_axis',(0.,1.,0.));
#45210=DIRECTION('center_axis',(0.546304790255255,-0.837586454001444,-9.0650146342598E-5));
#45211=DIRECTION('ref_axis',(0.837499315807156,0.546246387962813,0.0144837723030219));
#45212=DIRECTION('center_axis',(0.184157150081292,0.982896806869675,-0.000105448247335927));
#45213=DIRECTION('ref_axis',(0.982823653730575,-0.184142132936566,0.0122204969315608));
#45214=DIRECTION('center_axis',(5.15167520928809E-67,-1.18789542670764E-48,
-1.));
#45215=DIRECTION('ref_axis',(0.,1.,0.));
#45216=DIRECTION('center_axis',(0.610336990681674,-0.792141874658946,-9.06501464101343E-5));
#45217=DIRECTION('ref_axis',(0.792059587273886,0.610271931640238,0.0144837722853376));
#45218=DIRECTION('center_axis',(0.106472260386401,0.99431566750649,-0.000105448247238185));
#45219=DIRECTION('ref_axis',(0.994241561642249,-0.106463029063635,0.0122204969529716));
#45220=DIRECTION('center_axis',(5.15167520928809E-67,-1.18789542670764E-48,
-1.));
#45221=DIRECTION('ref_axis',(0.,1.,0.));
#45222=DIRECTION('center_axis',(0.670606260602894,-0.741813477245294,-9.06501464627064E-5));
#45223=DIRECTION('ref_axis',(0.741736547997723,0.670534945922382,0.0144837723432088));
#45224=DIRECTION('center_axis',(0.0281309337999561,0.999604241409674,-0.000105448247417899));
#45225=DIRECTION('ref_axis',(0.999529639708026,-0.0281275452133787,0.0122204969380853));
#45226=DIRECTION('center_axis',(5.15167520928809E-67,-1.18789542670764E-48,
-1.));
#45227=DIRECTION('ref_axis',(0.,1.,0.));
#45228=DIRECTION('center_axis',(0.726741019928368,-0.686911553066351,-9.0650146471134E-5));
#45229=DIRECTION('ref_axis',(0.686840456251459,0.726663889288164,0.0144837723292476));
#45230=DIRECTION('center_axis',(-0.050383829347144,0.998729922762398,-0.000105448247269544));
#45231=DIRECTION('ref_axis',(0.998655285167744,0.0503813543057988,0.0122204969148411));
#45232=DIRECTION('center_axis',(5.15167520928809E-67,-1.18789542670764E-48,
-1.));
#45233=DIRECTION('ref_axis',(0.,1.,0.));
#45234=DIRECTION('center_axis',(0.778395179200218,-0.627774590741304,-9.06501463631465E-5));
#45235=DIRECTION('ref_axis',(0.627709764694807,0.778312708136684,0.0144837722894029));
#45236=DIRECTION('center_axis',(-0.12858795942834,0.991698102030413,-0.000105448245500489));
#45237=DIRECTION('ref_axis',(0.991623888698102,0.128579636017312,0.0122204977357358));
#45238=DIRECTION('center_axis',(5.15167520928809E-67,-1.18789542670764E-48,
-1.));
#45239=DIRECTION('ref_axis',(0.,1.,0.));
#45240=DIRECTION('center_axis',(0.825250273349428,-0.564767189308343,-9.06501464028957E-5));
#45241=DIRECTION('ref_axis',(0.564709033703531,0.825162970323003,0.0144837723450398));
#45242=DIRECTION('center_axis',(-0.205999301987628,0.978552132725322,-0.000105448247257059));
#45243=DIRECTION('ref_axis',(0.978478801225208,0.205985181525983,0.0122204969042825));
#45244=DIRECTION('center_axis',(5.15167520928809E-67,-1.18789542670764E-48,
-1.));
#45245=DIRECTION('ref_axis',(0.,1.,0.));
#45246=DIRECTION('center_axis',(0.867017425139937,-0.498277810349071,-9.06501464136658E-5));
#45247=DIRECTION('ref_axis',(0.498226683735389,0.866925828403975,0.0144837723027363));
#45248=DIRECTION('center_axis',(-0.282140590344626,0.959373064120863,-0.000105448247277017));
#45249=DIRECTION('ref_axis',(0.959301066555094,0.282120759888223,0.0122204969764503));
#45250=DIRECTION('center_axis',(5.15167520928809E-67,-1.18789542670764E-48,
-1.));
#45251=DIRECTION('ref_axis',(0.,1.,0.));
#45252=DIRECTION('center_axis',(0.90343912619187,-0.42871638299489,-9.06501464260602E-5));
#45253=DIRECTION('ref_axis',(0.428672600584421,0.903343800469878,0.0144837723272369));
#45254=DIRECTION('center_axis',(-0.356542388139781,0.934279141552593,-0.000105448246761887));
#45255=DIRECTION('ref_axis',(0.934208921809314,0.35651696994953,0.012220497120973));
#45256=DIRECTION('center_axis',(5.15167520928809E-67,-1.18789542670764E-48,
-1.));
#45257=DIRECTION('ref_axis',(0.,1.,0.));
#45258=DIRECTION('center_axis',(0.934290824606888,-0.35651177657678,-9.06501464134324E-5));
#45259=DIRECTION('ref_axis',(0.356475608302711,0.934192357613664,0.0144837723482609));
#45260=DIRECTION('center_axis',(-0.428745983551679,0.903425077396555,-0.000105448247222545));
#45261=DIRECTION('ref_axis',(0.903357068407448,0.428715134340562,0.0122204969479439));
#45262=DIRECTION('center_axis',(5.15167520928809E-67,-1.18789542670764E-48,
-1.));
#45263=DIRECTION('ref_axis',(0.,1.,0.));
#45264=DIRECTION('center_axis',(0.959382309405034,-0.282109156503675,-9.06501462956451E-5));
#45265=DIRECTION('ref_axis',(0.282080825355574,0.959281308222623,0.0144837723473633));
#45266=DIRECTION('center_axis',(-0.498306217401744,0.867001097219279,-0.000105448247347347));
#45267=DIRECTION('ref_axis',(0.866935718280794,0.498270127364887,0.0122204969106369));
#45268=DIRECTION('center_axis',(5.15167520928809E-67,-1.18789542670764E-48,
-1.));
#45269=DIRECTION('ref_axis',(0.,1.,0.));
#45270=DIRECTION('center_axis',(0.978558883238587,-0.205967239670296,-9.06501464061553E-5));
#45271=DIRECTION('ref_axis',(0.205946920319019,0.978455970572407,0.0144837723787919));
#45272=DIRECTION('center_axis',(-0.564794227717559,0.825231766970706,-0.000105448247271081));
#45273=DIRECTION('ref_axis',(0.825169421165301,0.564753119361831,0.0122204969131223));
#45274=DIRECTION('center_axis',(5.15167520928809E-67,-1.18789542670764E-48,
-1.));
#45275=DIRECTION('ref_axis',(0.,1.,0.));
#45276=DIRECTION('center_axis',(0.99170231615319,-0.128555466312983,-9.06501463191467E-5));
#45277=DIRECTION('ref_axis',(0.128543284034309,0.991598126495285,0.014483772323378));
#45278=DIRECTION('center_axis',(-0.627800093806562,0.778374608461208,-0.000105448247350595));
#45279=DIRECTION('ref_axis',(0.778315680171392,0.627754220578551,0.0122204969276863));
#45280=DIRECTION('center_axis',(5.15167520928809E-67,-1.18789542670764E-48,
-1.));
#45281=DIRECTION('ref_axis',(0.,1.,0.));
#45282=DIRECTION('center_axis',(0.998731574514188,-0.0503511057570843,-9.06501463742907E-5));
#45283=DIRECTION('ref_axis',(0.0503471356586318,0.998626750227146,0.0144837723587898));
#45284=DIRECTION('center_axis',(-0.686935363552425,0.726718511654798,-0.000105448247333776));
#45285=DIRECTION('ref_axis',(0.726663364192883,0.686885008275621,0.0122204969654078));
#45286=DIRECTION('center_axis',(5.15167520928809E-67,-1.18789542670764E-48,
-1.));
#45287=DIRECTION('ref_axis',(0.,1.,0.));
#45288=DIRECTION('center_axis',(0.999603320606373,0.0281636861093081,-9.0650146390368E-5));
#45289=DIRECTION('ref_axis',(0.0281594195505035,-0.99949850796739,-0.0144837723518616));
#45290=DIRECTION('center_axis',(-0.741835448352795,0.670581953565614,-0.000105448247334273));
#45291=DIRECTION('ref_axis',(0.670530926935027,0.741780921485189,0.0122204968899333));
#45292=DIRECTION('center_axis',(5.15167520928809E-67,-1.18789542670764E-48,
-1.));
#45293=DIRECTION('ref_axis',(0.,1.,0.));
#45294=DIRECTION('center_axis',(0.994312179825183,0.106504839485559,-9.06501463756277E-5));
#45295=DIRECTION('ref_axis',(0.106492362574294,-0.994208025039266,-0.0144837723286163));
#45296=DIRECTION('center_axis',(-0.792161870920044,0.610311034752874,-0.00010544824088436));
#45297=DIRECTION('ref_axis',(0.610264443527485,0.792103508609612,0.0122204997619462));
#45298=DIRECTION('center_axis',(5.15167520928809E-67,-1.18789542670764E-48,
-1.));
#45299=DIRECTION('ref_axis',(0.,1.,0.));
#45300=DIRECTION('center_axis',(0.982890773813025,0.184189355109853,-9.06501463812825E-5));
#45301=DIRECTION('ref_axis',(0.184168744770323,-0.982787919028214,-0.0144837723648623));
#45302=DIRECTION('center_axis',(-0.837604352149864,0.54627734543936,-0.00010544824728987));
#45303=DIRECTION('ref_axis',(0.546235476912709,0.837542514274935,0.0122204968788532));
#45304=DIRECTION('center_axis',(5.15167520928809E-67,-1.18789542670764E-48,
-1.));
#45305=DIRECTION('ref_axis',(0.,1.,0.));
#45306=DIRECTION('center_axis',(-0.778374608461274,-0.62780009380648,-0.000105448247267533));
#45307=DIRECTION('ref_axis',(0.627754220578446,-0.77831568017143,-0.0122204969306265));
#45308=DIRECTION('center_axis',(0.128555466313028,0.991702316153185,-9.06501463500336E-5));
#45309=DIRECTION('ref_axis',(0.991598126495177,-0.128543284034342,-0.0144837723304925));
#45310=DIRECTION('center_axis',(5.15167520928809E-67,-1.18789542670764E-48,
-1.));
#45311=DIRECTION('ref_axis',(0.,1.,0.));
#45312=DIRECTION('center_axis',(-0.825231766970672,-0.564794227717608,-0.000105448247309068));
#45313=DIRECTION('ref_axis',(0.564753119361638,-0.825169421164907,-0.012220496948613));
#45314=DIRECTION('center_axis',(0.205967239670274,0.978558883238591,-9.0650146374353E-5));
#45315=DIRECTION('ref_axis',(0.978455970572943,-0.205946920319105,-0.0144837723413512));
#45316=DIRECTION('center_axis',(5.15167520928809E-67,-1.18789542670764E-48,
-1.));
#45317=DIRECTION('ref_axis',(0.,1.,0.));
#45318=DIRECTION('center_axis',(-0.86700109721932,-0.498306217401672,-0.00010544824729092));
#45319=DIRECTION('ref_axis',(0.498270127364739,-0.8669357182807,-0.0122204969233888));
#45320=DIRECTION('center_axis',(0.282109156504052,0.959382309404923,-9.06501464701313E-5));
#45321=DIRECTION('ref_axis',(0.959281308222407,-0.282080825355923,-0.0144837723548786));
#45322=DIRECTION('center_axis',(5.15167520928809E-67,-1.18789542670764E-48,
-1.));
#45323=DIRECTION('ref_axis',(0.,1.,0.));
#45324=DIRECTION('center_axis',(-0.903425077396529,-0.428745983551733,-0.000105448247249315));
#45325=DIRECTION('ref_axis',(0.428715134340504,-0.903357068407182,-0.0122204969696425));
#45326=DIRECTION('center_axis',(0.356511776576785,0.934290824606886,-9.06501464239672E-5));
#45327=DIRECTION('ref_axis',(0.934192357613866,-0.356475608302793,-0.0144837723332318));
#45328=DIRECTION('center_axis',(5.15167520928809E-67,-1.18789542670764E-48,
-1.));
#45329=DIRECTION('ref_axis',(0.,1.,0.));
#45330=DIRECTION('center_axis',(-0.934279141552621,-0.356542388139705,-0.000105448246733279));
#45331=DIRECTION('ref_axis',(0.356516969949183,-0.934208921808614,-0.0122204971846563));
#45332=DIRECTION('center_axis',(0.428716382994808,0.903439126191909,-9.06501463770139E-5));
#45333=DIRECTION('ref_axis',(0.903343800469329,-0.428672600584064,-0.0144837723720362));
#45334=DIRECTION('center_axis',(5.15167520928809E-67,-1.18789542670764E-48,
-1.));
#45335=DIRECTION('ref_axis',(0.,1.,0.));
#45336=DIRECTION('center_axis',(-0.959373064120865,-0.282140590344618,-0.000105448247270857));
#45337=DIRECTION('ref_axis',(0.282120759888191,-0.959301066555013,-0.0122204969835453));
#45338=DIRECTION('center_axis',(0.498277810349034,0.867017425139958,-9.06501463569771E-5));
#45339=DIRECTION('ref_axis',(0.866925828403698,-0.498226683735182,-0.0144837723264648));
#45340=DIRECTION('center_axis',(5.15167520928809E-67,-1.18789542670764E-48,
-1.));
#45341=DIRECTION('ref_axis',(0.,1.,0.));
#45342=DIRECTION('center_axis',(-0.978552132725285,-0.205999301987804,-0.000105448247338301));
#45343=DIRECTION('ref_axis',(0.205985181526041,-0.978478801224581,-0.0122204969535068));
#45344=DIRECTION('center_axis',(0.564767189308271,0.825250273349477,-9.06501463565956E-5));
#45345=DIRECTION('ref_axis',(0.825162970322881,-0.564709033703342,-0.0144837723594094));
#45346=DIRECTION('center_axis',(5.15167520928809E-67,-1.18789542670764E-48,
-1.));
#45347=DIRECTION('ref_axis',(0.,1.,0.));
#45348=DIRECTION('center_axis',(-0.991698102030424,-0.128587959428258,-0.000105448245434831));
#45349=DIRECTION('ref_axis',(0.128579636017166,-0.991623888697594,-0.0122204977785004));
#45350=DIRECTION('center_axis',(0.627774590741263,0.778395179200251,-9.06501463298504E-5));
#45351=DIRECTION('ref_axis',(0.778312708136619,-0.627709764694687,-0.0144837722981268));
#45352=DIRECTION('center_axis',(5.15167520928809E-67,-1.18789542670764E-48,
-1.));
#45353=DIRECTION('ref_axis',(0.,1.,0.));
#45354=DIRECTION('center_axis',(-0.998729922762387,-0.0503838293473624,
-0.000105448247373321));
#45355=DIRECTION('ref_axis',(0.0503813543060242,-0.998655285167869,-0.0122204969036645));
#45356=DIRECTION('center_axis',(0.686911553066443,0.726741019928282,-9.06501464895761E-5));
#45357=DIRECTION('ref_axis',(0.726663889287984,-0.686840456251464,-0.0144837723380814));
#45358=DIRECTION('center_axis',(5.15167520928809E-67,-1.18789542670764E-48,
-1.));
#45359=DIRECTION('ref_axis',(0.,1.,0.));
#45360=DIRECTION('center_axis',(-0.999604241409666,0.0281309338002504,-0.00010544824728445));
#45361=DIRECTION('ref_axis',(0.0281275452136831,0.999529639708247,0.0122204969192793));
#45362=DIRECTION('center_axis',(0.741813477245179,0.670606260603021,-9.06501463486941E-5));
#45363=DIRECTION('ref_axis',(0.670534945922386,-0.741736547997471,-0.0144837723559454));
#45364=DIRECTION('center_axis',(5.15167520928809E-67,-1.18789542670764E-48,
-1.));
#45365=DIRECTION('ref_axis',(0.,1.,0.));
#45366=DIRECTION('center_axis',(-0.994315667506492,0.106472260386385,-0.000105448247246095));
#45367=DIRECTION('ref_axis',(0.106463029063669,0.99424156164268,0.0122204969176238));
#45368=DIRECTION('center_axis',(0.792141874658893,0.610336990681743,-9.06501463537118E-5));
#45369=DIRECTION('ref_axis',(0.610271931639807,-0.792059587273192,-0.0144837723414781));
#45370=DIRECTION('center_axis',(5.15167520928809E-67,-1.18789542670764E-48,
-1.));
#45371=DIRECTION('ref_axis',(0.,1.,0.));
#45372=DIRECTION('center_axis',(-0.98289680686965,0.184157150081429,-0.000105448247288298));
#45373=DIRECTION('ref_axis',(0.184142132936832,0.982823653731204,0.0122204968770007));
#45374=DIRECTION('center_axis',(0.837586454001503,0.546304790255165,-9.06501464022278E-5));
#45375=DIRECTION('ref_axis',(0.546246387962582,-0.837499315807004,-0.0144837723204838));
#45376=DIRECTION('center_axis',(5.15167520928809E-67,-1.18789542670764E-48,
-1.));
#45377=DIRECTION('ref_axis',(0.,1.,0.));
#45378=DIRECTION('center_axis',(-0.965418060567323,0.260706649725506,-0.000105448239021929));
#45379=DIRECTION('ref_axis',(0.260685939332638,0.965346311123758,0.0122205005631217));
#45380=DIRECTION('center_axis',(0.877867034329392,0.478904439131931,-9.06501464072983E-5));
#45381=DIRECTION('ref_axis',(0.478853053658107,-0.87777558256187,-0.0144837723150808));
#45382=DIRECTION('center_axis',(5.15167520928809E-67,-1.18789542670764E-48,
-1.));
#45383=DIRECTION('ref_axis',(0.,1.,0.));
#45384=DIRECTION('center_axis',(-0.94198719089703,0.335648806145038,-0.000105448247300868));
#45385=DIRECTION('ref_axis',(0.335622530213848,0.941917287592769,0.0122204969921728));
#45386=DIRECTION('center_axis',(0.912735272470196,0.40855148288962,-9.06501464040206E-5));
#45387=DIRECTION('ref_axis',(0.408507431043198,-0.912640070960478,-0.01448377228974));
#45388=DIRECTION('center_axis',(5.15167520928809E-67,-1.18789542670764E-48,
-1.));
#45389=DIRECTION('ref_axis',(0.,1.,0.));
#45390=DIRECTION('center_axis',(0.965409519335958,0.260738282110751,-9.06501464007405E-5));
#45391=DIRECTION('ref_axis',(0.260709665412327,-0.965308598685698,-0.0144837724383535));
#45392=DIRECTION('center_axis',(-0.87788272400828,0.478875674646843,-0.000105448247307507));
#45393=DIRECTION('ref_axis',(0.478838786930294,0.877817791791527,0.0122204969363654));
#45394=DIRECTION('center_axis',(5.15167520928809E-67,-1.18789542670764E-48,
-1.));
#45395=DIRECTION('ref_axis',(-4.33680868994202E-19,1.,-1.18789542670764E-48));
#45396=DIRECTION('center_axis',(5.15167520928809E-67,-1.18789542670764E-48,
-1.));
#45397=DIRECTION('ref_axis',(-4.33680868994202E-19,1.,-1.18789542670764E-48));
#45398=DIRECTION('center_axis',(5.15167520928809E-67,-1.18789542670764E-48,
-1.));
#45399=DIRECTION('ref_axis',(0.,1.,0.));
#45400=DIRECTION('center_axis',(0.941987190897879,0.335648806142656,0.000105448247691596));
#45401=DIRECTION('ref_axis',(0.335622530211987,-0.941917287595053,0.0122204968672344));
#45402=DIRECTION('center_axis',(-0.912735272471169,0.408551482887447,9.06501467246596E-5));
#45403=DIRECTION('ref_axis',(0.408507431040732,0.912640070960819,-0.0144837723377799));
#45404=DIRECTION('center_axis',(5.15167520928809E-67,-1.18789542670764E-48,
-1.));
#45405=DIRECTION('ref_axis',(-4.33680868994202E-19,1.,-1.18789542670764E-48));
#45406=DIRECTION('center_axis',(5.15167520928809E-67,-1.18789542670764E-48,
-1.));
#45407=DIRECTION('ref_axis',(-4.33680868994202E-19,1.,-1.18789542670764E-48));
#45408=DIRECTION('',(-5.15167520928809E-67,1.18789542670764E-48,1.));
#45409=DIRECTION('',(5.15167520928809E-67,-1.18789542670764E-48,-1.));
#45410=DIRECTION('center_axis',(5.15167520928809E-67,-1.18789542670764E-48,
-1.));
#45411=DIRECTION('ref_axis',(-4.33680868994202E-19,1.,-1.18789542670764E-48));
#45412=DIRECTION('center_axis',(5.15167520928809E-67,-1.18789542670764E-48,
-1.));
#45413=DIRECTION('ref_axis',(0.,1.,0.));
#45414=DIRECTION('center_axis',(0.941976194140935,0.33567967089818,-9.06501463865783E-5));
#45415=DIRECTION('ref_axis',(0.335643224273153,-0.94187782983736,-0.014483772312066));
#45416=DIRECTION('center_axis',(-0.912748656947277,0.408521576078436,-0.000105448246989675));
#45417=DIRECTION('ref_axis',(0.408489896596946,0.91268103071696,0.012220497029356));
#45418=DIRECTION('center_axis',(-5.15167520928809E-67,1.18789542670764E-48,
1.));
#45419=DIRECTION('ref_axis',(4.33680868994202E-19,-1.,1.18789542670764E-48));
#45420=DIRECTION('center_axis',(0.,0.,1.));
#45421=DIRECTION('ref_axis',(1.,4.33680868994202E-19,0.));
#45422=DIRECTION('',(0.866025403784438,0.5,0.));
#45423=DIRECTION('',(-4.33680868994202E-19,1.,0.));
#45424=DIRECTION('',(-0.866025403784439,0.499999999999999,0.));
#45425=DIRECTION('',(-0.866025403784439,-0.5,0.));
#45426=DIRECTION('',(6.01359520363859E-16,-1.,0.));
#45427=DIRECTION('',(0.866025403784439,-0.5,0.));
#45428=DIRECTION('center_axis',(1.,4.33680868994202E-19,0.));
#45429=DIRECTION('ref_axis',(0.,0.,-1.));
#45430=DIRECTION('',(0.,0.,1.));
#45431=DIRECTION('',(0.,0.,1.));
#45432=DIRECTION('center_axis',(0.499999999999999,0.866025403784439,0.));
#45433=DIRECTION('ref_axis',(-0.866025403784439,0.499999999999999,0.));
#45434=DIRECTION('',(0.,0.,1.));
#45435=DIRECTION('center_axis',(-0.5,0.866025403784439,0.));
#45436=DIRECTION('ref_axis',(-0.866025403784439,-0.5,0.));
#45437=DIRECTION('',(0.,0.,1.));
#45438=DIRECTION('center_axis',(-1.,-6.01359520363859E-16,0.));
#45439=DIRECTION('ref_axis',(6.01359520363859E-16,-1.,0.));
#45440=DIRECTION('',(0.,0.,1.));
#45441=DIRECTION('center_axis',(-0.5,-0.866025403784439,0.));
#45442=DIRECTION('ref_axis',(0.866025403784439,-0.5,0.));
#45443=DIRECTION('',(0.,0.,1.));
#45444=DIRECTION('center_axis',(0.5,-0.866025403784439,0.));
#45445=DIRECTION('ref_axis',(0.866025403784439,0.5,0.));
#45446=DIRECTION('',(1.0568194522281E-16,0.866025403784468,-0.499999999999949));
#45447=DIRECTION('center_axis',(4.70261923768679E-35,-1.08435016942139E-16,
1.));
#45448=DIRECTION('ref_axis',(0.378466979033695,0.925614793410903,1.00369055805406E-16));
#45449=DIRECTION('center_axis',(0.912653256146669,-0.408734674385332,0.));
#45450=DIRECTION('ref_axis',(0.408734674385332,0.912653256146669,0.));
#45451=DIRECTION('',(0.,0.,1.));
#45452=DIRECTION('center_axis',(0.,0.,1.));
#45453=DIRECTION('ref_axis',(1.,4.33680868994202E-19,0.));
#45454=DIRECTION('',(0.,0.,1.));
#45455=DIRECTION('center_axis',(-0.912653256146668,-0.408734674385334,0.));
#45456=DIRECTION('ref_axis',(0.408734674385334,-0.912653256146668,0.));
#45457=DIRECTION('center_axis',(0.877770897795706,-0.479080630982844,8.35636401295593E-50));
#45458=DIRECTION('ref_axis',(0.479080630982844,0.877770897795706,2.97282767021015E-66));
#45459=DIRECTION('',(-9.32012009987243E-50,3.66188516048321E-51,1.));
#45460=DIRECTION('center_axis',(-9.32012009987243E-50,3.66188516048321E-51,
1.));
#45461=DIRECTION('ref_axis',(1.,4.33680868994202E-19,9.32012009987243E-50));
#45462=DIRECTION('',(-9.32012009987243E-50,3.66188516048321E-51,1.));
#45463=DIRECTION('center_axis',(-0.941908803685482,-0.335868732602165,-8.65571190069724E-50));
#45464=DIRECTION('ref_axis',(0.335868732602165,-0.941908803685482,-2.86613947502886E-66));
#45465=DIRECTION('center_axis',(0.941908803685478,-0.335868732602176,-8.65571190069562E-50));
#45466=DIRECTION('ref_axis',(0.335868732602176,0.941908803685478,5.69318196416785E-66));
#45467=DIRECTION('',(9.32012009987071E-50,3.66188516048189E-51,1.));
#45468=DIRECTION('center_axis',(9.32012009987071E-50,3.66188516048189E-51,
1.));
#45469=DIRECTION('ref_axis',(1.,4.33680868994202E-19,-9.32012009987071E-50));
#45470=DIRECTION('',(9.32012009987071E-50,3.66188516048189E-51,1.));
#45471=DIRECTION('center_axis',(-0.877770897795712,-0.479080630982834,8.35636401295441E-50));
#45472=DIRECTION('ref_axis',(0.479080630982834,-0.877770897795712,-1.78392693329902E-66));
#45473=DIRECTION('center_axis',(0.965357170233111,-0.260932048394827,-1.75574063469501E-49));
#45474=DIRECTION('ref_axis',(0.260932048394827,0.965357170233111,-8.03239509524584E-66));
#45475=DIRECTION('',(1.85827785600731E-49,1.46249639022155E-50,1.));
#45476=DIRECTION('center_axis',(1.8582778560073E-49,1.46249639022155E-50,
1.));
#45477=DIRECTION('ref_axis',(1.,4.33680868994202E-19,-1.8582778560073E-49));
#45478=DIRECTION('',(1.85827785600731E-49,1.46249639022155E-50,1.));
#45479=DIRECTION('center_axis',(-0.837476789971396,-0.546472896179862,1.63618603752562E-49));
#45480=DIRECTION('ref_axis',(0.546472896179862,-0.837476789971396,1.23627039651628E-65));
#45481=DIRECTION('center_axis',(0.982853788812423,-0.184386631340412,-2.66502014323869E-49));
#45482=DIRECTION('ref_axis',(0.184386631340412,0.982853788812423,-4.59929189808117E-66));
#45483=DIRECTION('',(2.77308680110516E-49,3.28216451991643E-50,1.));
#45484=DIRECTION('center_axis',(2.77308680110516E-49,3.28216451991643E-50,
1.));
#45485=DIRECTION('ref_axis',(1.,4.33680868994202E-19,-2.77308680110516E-49));
#45486=DIRECTION('',(2.77308680110516E-49,3.28216451991643E-50,1.));
#45487=DIRECTION('center_axis',(-0.792019359247614,-0.610495974251263,2.39671325397326E-49));
#45488=DIRECTION('ref_axis',(0.610495974251263,-0.792019359247614,-2.26955332198497E-65));
#45489=DIRECTION('center_axis',(0.994290786951656,-0.106704409389008,-3.5878037051643E-49));
#45490=DIRECTION('ref_axis',(0.106704409389008,0.994290786951656,1.37166247450949E-66));
#45491=DIRECTION('',(3.67079874392927E-49,5.81397404601223E-50,1.));
#45492=DIRECTION('center_axis',(3.67079874392927E-49,5.81397404601223E-50,
1.));
#45493=DIRECTION('ref_axis',(1.,4.33680868994202E-19,-3.67079874392927E-49));
#45494=DIRECTION('',(3.67079874392927E-49,5.81397404601223E-50,1.));
#45495=DIRECTION('center_axis',(-0.741678865800908,-0.670755141630892,3.11252914744798E-49));
#45496=DIRECTION('ref_axis',(0.670755141630892,-0.741678865800908,-3.59898235302298E-65));
#45497=DIRECTION('center_axis',(0.999597651754094,-0.028364319270904,-4.5184020529559E-49));
#45498=DIRECTION('ref_axis',(0.028364319270904,0.999597651754094,-3.26521667006146E-66));
#45499=DIRECTION('',(4.54587899183259E-49,9.04231552086841E-50,1.));
#45500=DIRECTION('center_axis',(4.54587899183259E-49,9.04231552086841E-50,
1.));
#45501=DIRECTION('ref_axis',(1.,4.33680868994202E-19,-4.54587899183259E-49));
#45502=DIRECTION('',(4.54587899183259E-49,9.04231552086841E-50,1.));
#45503=DIRECTION('center_axis',(-0.68676567551329,-0.726878880513649,3.77922047493358E-49));
#45504=DIRECTION('ref_axis',(0.726878880513649,-0.68676567551329,8.44347396578498E-67));
#45505=DIRECTION('center_axis',(0.998741664633518,0.0501506463075991,-5.45107773834402E-49));
#45506=DIRECTION('ref_axis',(-0.0501506463075991,0.998741664633518,-5.68155672720376E-65));
#45507=DIRECTION('center_axis',(-0.62761834646337,-0.778521169386283,4.39267686269876E-49));
#45508=DIRECTION('ref_axis',(0.778521169386283,-0.62761834646337,2.86838711888421E-65));
#45509=DIRECTION('center_axis',(0.991728103035171,0.128356416474834,-6.38008050558209E-49));
#45510=DIRECTION('ref_axis',(-0.128356416474834,0.991728103035171,2.64164793875071E-66));
#45511=DIRECTION('center_axis',(-0.564601541603225,-0.825363616365092,4.94911614811798E-49));
#45512=DIRECTION('ref_axis',(0.825363616365092,-0.564601541603225,-1.21982614064914E-65));
#45513=DIRECTION('center_axis',(0.978600207898554,0.20577082665166,-7.29968274368531E-49));
#45514=DIRECTION('ref_axis',(-0.20577082665166,0.978600207898554,7.99368498149713E-66));
#45515=DIRECTION('center_axis',(-0.498103780490032,-0.867117422187756,5.44510769796179E-49));
#45516=DIRECTION('ref_axis',(0.867117422187756,-0.498103780490032,-1.67935322369464E-65));
#45517=DIRECTION('center_axis',(0.95943891706265,0.281916591256437,-8.20421479905702E-49));
#45518=DIRECTION('ref_axis',(-0.281916591256437,0.95943891706265,1.24589067679861E-65));
#45519=DIRECTION('center_axis',(-0.428535043933802,-0.903525160756829,5.87759355939149E-49));
#45520=DIRECTION('ref_axis',(0.903525160756829,-0.428535043933802,-8.86364012879408E-65));
#45521=DIRECTION('center_axis',(0.93436236625724,0.356324246329338,-9.08809993078841E-49));
#45522=DIRECTION('ref_axis',(-0.356324246329338,0.93436236625724,-2.69950222050985E-65));
#45523=DIRECTION('center_axis',(-0.356324246329358,-0.934362366257233,6.24390731325522E-49));
#45524=DIRECTION('ref_axis',(0.934362366257233,-0.356324246329358,4.50754916861586E-65));
#45525=DIRECTION('center_axis',(0.903525160756839,0.428535043933782,-9.94588869312071E-49));
#45526=DIRECTION('ref_axis',(-0.428535043933782,0.903525160756839,-3.06876799885187E-65));
#45527=DIRECTION('center_axis',(-0.281916591256458,-0.959438917062644,6.54179051344872E-49));
#45528=DIRECTION('ref_axis',(0.959438917062644,-0.281916591256458,5.46345068117847E-65));
#45529=DIRECTION('center_axis',(0.867117422187767,0.498103780490012,-1.07722925330905E-48));
#45530=DIRECTION('ref_axis',(-0.498103780490012,0.867117422187767,2.63677046246647E-65));
#45531=DIRECTION('center_axis',(-0.205770826651682,-0.978600207898549,6.76940661098659E-49));
#45532=DIRECTION('ref_axis',(0.978600207898549,-0.205770826651682,1.20007194121145E-65));
#45533=DIRECTION('center_axis',(0.825363616365104,0.564601541603207,-1.15622163962171E-48));
#45534=DIRECTION('ref_axis',(-0.564601541603207,0.825363616365104,5.34857418276646E-65));
#45535=DIRECTION('center_axis',(-0.128356416474855,-0.991728103035168,6.92535227693746E-49));
#45536=DIRECTION('ref_axis',(0.991728103035168,-0.128356416474855,1.05782428992148E-64));
#45537=DIRECTION('center_axis',(0.778521169386297,0.627618346463353,-1.2310790139208E-48));
#45538=DIRECTION('ref_axis',(-0.627618346463353,0.778521169386297,-3.24299836420865E-65));
#45539=DIRECTION('center_axis',(-0.0501506463076206,-0.998741664633517,
7.00866605441356E-49));
#45540=DIRECTION('ref_axis',(0.998741664633517,-0.0501506463076206,5.61717615944791E-66));
#45541=DIRECTION('center_axis',(0.83747678997139,-0.546472896179871,1.63618603752577E-49));
#45542=DIRECTION('ref_axis',(0.546472896179871,0.83747678997139,8.18221406165844E-66));
#45543=DIRECTION('',(-1.85827785600747E-49,1.46249639022181E-50,1.));
#45544=DIRECTION('center_axis',(-1.85827785600747E-49,1.46249639022181E-50,
1.));
#45545=DIRECTION('ref_axis',(1.,4.33680868994202E-19,1.85827785600747E-49));
#45546=DIRECTION('',(-1.85827785600747E-49,1.46249639022181E-50,1.));
#45547=DIRECTION('center_axis',(-0.965357170233114,-0.260932048394816,-1.75574063469517E-49));
#45548=DIRECTION('ref_axis',(0.260932048394816,-0.965357170233114,4.85072620126884E-66));
#45549=DIRECTION('center_axis',(0.792019359247608,-0.610495974251272,2.39671325397339E-49));
#45550=DIRECTION('ref_axis',(0.610495974251272,0.792019359247608,6.86514884131891E-66));
#45551=DIRECTION('',(-2.77308680110532E-49,3.28216451991683E-50,1.));
#45552=DIRECTION('center_axis',(-2.77308680110532E-49,3.28216451991683E-50,
1.));
#45553=DIRECTION('ref_axis',(1.,4.33680868994202E-19,2.77308680110532E-49));
#45554=DIRECTION('',(-2.77308680110532E-49,3.28216451991683E-50,1.));
#45555=DIRECTION('center_axis',(-0.982853788812425,-0.184386631340402,-2.66502014323885E-49));
#45556=DIRECTION('ref_axis',(0.184386631340402,-0.982853788812425,5.0100483719309E-66));
#45557=DIRECTION('center_axis',(0.741678865800901,-0.6707551416309,3.11252914744811E-49));
#45558=DIRECTION('ref_axis',(0.6707551416309,0.741678865800901,2.48321099822104E-65));
#45559=DIRECTION('',(-3.67079874392942E-49,5.81397404601274E-50,1.));
#45560=DIRECTION('center_axis',(-3.67079874392942E-49,5.81397404601274E-50,
1.));
#45561=DIRECTION('ref_axis',(1.,4.33680868994202E-19,3.67079874392942E-49));
#45562=DIRECTION('',(-3.67079874392942E-49,5.81397404601274E-50,1.));
#45563=DIRECTION('center_axis',(-0.994290786951657,-0.106704409388997,-3.58780370516446E-49));
#45564=DIRECTION('ref_axis',(0.106704409388997,-0.994290786951657,8.97464790050996E-66));
#45565=DIRECTION('center_axis',(0.686765675513281,-0.726878880513656,3.77922047493371E-49));
#45566=DIRECTION('ref_axis',(0.726878880513657,0.686765675513281,3.1589153081368E-66));
#45567=DIRECTION('',(-4.54587899183275E-49,9.04231552086907E-50,1.));
#45568=DIRECTION('center_axis',(-4.54587899183275E-49,9.04231552086907E-50,
1.));
#45569=DIRECTION('ref_axis',(1.,4.33680868994202E-19,4.54587899183275E-49));
#45570=DIRECTION('',(-4.54587899183275E-49,9.04231552086907E-50,1.));
#45571=DIRECTION('center_axis',(-0.999597651754094,-0.0283643192708926,
-4.51840205295607E-49));
#45572=DIRECTION('ref_axis',(0.0283643192708926,-0.999597651754094,-3.99287521021606E-67));
#45573=DIRECTION('center_axis',(0.627618346463361,-0.77852116938629,4.39267686269887E-49));
#45574=DIRECTION('ref_axis',(0.77852116938629,0.627618346463361,3.8324092947301E-66));
#45575=DIRECTION('',(-5.39293238409326E-49,1.29472851457609E-49,1.));
#45576=DIRECTION('center_axis',(-5.39293238409326E-49,1.29472851457609E-49,
1.));
#45577=DIRECTION('ref_axis',(-0.453990499739606,-0.891006524188338,-1.29472851457643E-49));
#45578=DIRECTION('',(-5.39293238409326E-49,1.29472851457609E-49,1.));
#45579=DIRECTION('center_axis',(-0.998741664633517,0.0501506463076103,-5.45107773834419E-49));
#45580=DIRECTION('ref_axis',(-0.0501506463076103,-0.998741664633517,1.75141110323522E-67));
#45581=DIRECTION('center_axis',(0.564601541603216,-0.825363616365098,4.94911614811808E-49));
#45582=DIRECTION('ref_axis',(0.825363616365098,0.564601541603216,-2.63676715352381E-65));
#45583=DIRECTION('',(-6.20673655487384E-49,1.75048074844164E-49,1.));
#45584=DIRECTION('center_axis',(-6.20673655487384E-49,1.75048074844164E-49,
1.));
#45585=DIRECTION('ref_axis',(-0.52249856471585,-0.852640164354153,-1.75048074844092E-49));
#45586=DIRECTION('',(-6.20673655487384E-49,1.75048074844164E-49,1.));
#45587=DIRECTION('center_axis',(-0.99172810303517,0.128356416474844,-6.38008050558225E-49));
#45588=DIRECTION('ref_axis',(-0.128356416474844,-0.99172810303517,-6.45104663994926E-66));
#45589=DIRECTION('center_axis',(0.498103780490022,-0.867117422187761,5.44510769796189E-49));
#45590=DIRECTION('ref_axis',(0.867117422187761,0.498103780490022,4.62928424055004E-65));
#45591=DIRECTION('',(-6.98227413084428E-49,2.26867838960881E-49,1.));
#45592=DIRECTION('center_axis',(-6.98227413084428E-49,2.26867838960881E-49,
1.));
#45593=DIRECTION('ref_axis',(-0.587785252292493,-0.809016994374933,-2.26867838960897E-49));
#45594=DIRECTION('',(-6.98227413084428E-49,2.26867838960881E-49,1.));
#45595=DIRECTION('center_axis',(-0.978600207898551,0.205770826651671,-7.29968274368548E-49));
#45596=DIRECTION('ref_axis',(-0.205770826651671,-0.978600207898551,-8.37640359713844E-66));
#45597=DIRECTION('center_axis',(0.428535043933792,-0.903525160756834,5.87759355939158E-49));
#45598=DIRECTION('ref_axis',(0.903525160756834,0.428535043933792,-6.0990810847752E-65));
#45599=DIRECTION('',(-7.71476366495631E-49,2.84612657730158E-49,1.));
#45600=DIRECTION('center_axis',(-7.71476366495631E-49,2.84612657730158E-49,
1.));
#45601=DIRECTION('ref_axis',(-0.649448048330161,-0.76040596560005,-2.84612657730134E-49));
#45602=DIRECTION('',(-7.71476366495631E-49,2.84612657730158E-49,1.));
#45603=DIRECTION('center_axis',(-0.959438917062647,0.281916591256448,-8.20421479905718E-49));
#45604=DIRECTION('ref_axis',(-0.281916591256448,-0.959438917062647,-3.25299225253391E-65));
#45605=DIRECTION('center_axis',(0.356324246329348,-0.934362366257237,6.2439073132553E-49));
#45606=DIRECTION('ref_axis',(0.934362366257237,0.356324246329348,-6.3916346242107E-66));
#45607=DIRECTION('',(-8.39968911565463E-49,3.47926515142182E-49,1.));
#45608=DIRECTION('center_axis',(-8.39968911565463E-49,3.47926515142182E-49,
1.));
#45609=DIRECTION('ref_axis',(-0.707106781186566,-0.707106781186529,-3.47926515142204E-49));
#45610=DIRECTION('',(-8.39968911565463E-49,3.47926515142182E-49,1.));
#45611=DIRECTION('center_axis',(-0.934362366257236,0.356324246329348,-9.08809993078856E-49));
#45612=DIRECTION('ref_axis',(-0.356324246329348,-0.934362366257236,-6.41640199023417E-65));
#45613=DIRECTION('center_axis',(0.281916591256447,-0.959438917062647,6.54179051344879E-49));
#45614=DIRECTION('ref_axis',(0.959438917062647,0.281916591256447,-1.09781434718078E-65));
#45615=DIRECTION('',(-9.03282768977487E-49,4.16419060212015E-49,1.));
#45616=DIRECTION('center_axis',(-9.03282768977487E-49,4.16419060212015E-49,
1.));
#45617=DIRECTION('ref_axis',(-0.760405965599942,-0.649448048330288,-4.16419060211889E-49));
#45618=DIRECTION('',(-9.03282768977487E-49,4.16419060212015E-49,1.));
#45619=DIRECTION('center_axis',(-0.903525160756834,0.428535043933793,-9.94588869312087E-49));
#45620=DIRECTION('ref_axis',(-0.428535043933793,-0.903525160756834,3.14193955482054E-65));
#45621=DIRECTION('center_axis',(0.205770826651671,-0.978600207898551,6.76940661098664E-49));
#45622=DIRECTION('ref_axis',(0.978600207898551,0.205770826651671,1.21103353553181E-65));
#45623=DIRECTION('',(-9.61027587746764E-49,4.89668013623218E-49,1.));
#45624=DIRECTION('center_axis',(-9.61027587746764E-49,4.89668013623218E-49,
1.));
#45625=DIRECTION('ref_axis',(-0.809016994374948,-0.587785252292472,-4.89668013623217E-49));
#45626=DIRECTION('',(-9.61027587746764E-49,4.89668013623218E-49,1.));
#45627=DIRECTION('center_axis',(-0.867117422187761,0.498103780490022,-1.07722925330906E-48));
#45628=DIRECTION('ref_axis',(-0.498103780490022,-0.867117422187761,1.20400755006059E-65));
#45629=DIRECTION('center_axis',(0.128356416474844,-0.99172810303517,6.92535227693751E-49));
#45630=DIRECTION('ref_axis',(0.99172810303517,0.128356416474844,1.37955244398014E-65));
#45631=DIRECTION('',(-1.01284735186348E-48,5.67221771220262E-49,1.));
#45632=DIRECTION('center_axis',(-1.01284735186348E-48,5.67221771220262E-49,
1.));
#45633=DIRECTION('ref_axis',(-0.852640164354111,-0.522498564715917,-5.67221771220297E-49));
#45634=DIRECTION('',(-1.01284735186348E-48,5.67221771220262E-49,1.));
#45635=DIRECTION('center_axis',(-0.825363616365097,0.564601541603216,-1.15622163962172E-48));
#45636=DIRECTION('ref_axis',(-0.564601541603216,-0.825363616365097,3.75089637720347E-65));
#45637=DIRECTION('center_axis',(0.0501506463076098,-0.998741664633517,7.0086660544136E-49));
#45638=DIRECTION('ref_axis',(0.998741664633517,0.0501506463076098,-1.39822384050416E-65));
#45639=DIRECTION('',(-1.05842257525004E-48,6.4860218829832E-49,1.));
#45640=DIRECTION('center_axis',(-1.05842257525004E-48,6.4860218829832E-49,
1.));
#45641=DIRECTION('ref_axis',(-0.891006524188326,-0.453990499739629,-6.48602188298224E-49));
#45642=DIRECTION('',(-1.05842257525004E-48,6.4860218829832E-49,1.));
#45643=DIRECTION('center_axis',(-0.77852116938629,0.627618346463361,-1.23107901392082E-48));
#45644=DIRECTION('ref_axis',(-0.627618346463361,-0.77852116938629,-1.0235164758246E-65));
#45645=DIRECTION('center_axis',(-0.0283643192708931,-0.999597651754094,
7.01883428627214E-49));
#45646=DIRECTION('ref_axis',(0.999597651754094,-0.0283643192708931,-4.40612052675408E-66));
#45647=DIRECTION('',(-1.09747227149895E-48,7.33307527524372E-49,1.));
#45648=DIRECTION('center_axis',(-1.09747227149895E-48,7.33307527524372E-49,
1.));
#45649=DIRECTION('ref_axis',(-0.923879532511259,-0.382683432365157,-7.33307527524286E-49));
#45650=DIRECTION('',(-1.09747227149895E-48,7.33307527524372E-49,1.));
#45651=DIRECTION('center_axis',(-0.726878880513656,0.686765675513282,-1.30133985560119E-48));
#45652=DIRECTION('ref_axis',(-0.686765675513282,-0.726878880513656,-1.0460740182702E-64));
#45653=DIRECTION('center_axis',(-0.106704409388998,-0.994290786951657,6.95579428198243E-49));
#45654=DIRECTION('ref_axis',(0.994290786951657,-0.106704409388998,-7.09717408543387E-66));
#45655=DIRECTION('',(-1.12975568624752E-48,8.20815552314704E-49,1.));
#45656=DIRECTION('center_axis',(-1.12975568624752E-48,8.20815552314704E-49,
1.));
#45657=DIRECTION('ref_axis',(-0.951056516295187,-0.309016994374844,-8.20815552314827E-49));
#45658=DIRECTION('',(-1.12975568624752E-48,8.20815552314704E-49,1.));
#45659=DIRECTION('center_axis',(-0.6707551416309,0.741678865800901,-1.36657098320978E-48));
#45660=DIRECTION('ref_axis',(-0.741678865800901,-0.6707551416309,3.57211103088032E-65));
#45661=DIRECTION('center_axis',(-0.184386631340402,-0.982853788812425,6.81993470413386E-49));
#45662=DIRECTION('ref_axis',(0.982853788812425,-0.184386631340402,2.71684956354986E-65));
#45663=DIRECTION('',(-1.15507378150848E-48,9.10586746597114E-49,1.));
#45664=DIRECTION('center_axis',(-1.15507378150848E-48,9.10586746597114E-49,
1.));
#45665=DIRECTION('ref_axis',(-0.972369920397692,-0.233445363855843,-9.1058674659719E-49));
#45666=DIRECTION('',(-1.15507378150848E-48,9.10586746597114E-49,1.));
#45667=DIRECTION('center_axis',(-0.610495974251271,0.792019359247608,-1.42637022515333E-48));
#45668=DIRECTION('ref_axis',(-0.792019359247608,-0.610495974251271,3.09249712984754E-64));
#45669=DIRECTION('center_axis',(-0.260932048394816,-0.965357170233114,6.61209317220174E-49));
#45670=DIRECTION('ref_axis',(0.965357170233114,-0.260932048394816,1.42679734120621E-65));
#45671=DIRECTION('',(-1.17327046280543E-48,1.0020676411069E-48,1.));
#45672=DIRECTION('center_axis',(-1.17327046280543E-48,1.0020676411069E-48,
1.));
#45673=DIRECTION('ref_axis',(-0.987688340595155,-0.156434465040119,-1.00206764110703E-48));
#45674=DIRECTION('',(-1.17327046280543E-48,1.0020676411069E-48,1.));
#45675=DIRECTION('center_axis',(-0.546472896179871,0.83747678997139,-1.48036889921999E-48));
#45676=DIRECTION('ref_axis',(-0.83747678997139,-0.546472896179871,5.98336102584152E-65));
#45677=DIRECTION('center_axis',(-0.335868732602165,-0.941908803685482,6.33355109834478E-49));
#45678=DIRECTION('ref_axis',(0.941908803685482,-0.335868732602165,5.83703495410428E-65));
#45679=DIRECTION('',(-1.18423354154716E-48,1.09469422570892E-48,1.));
#45680=DIRECTION('center_axis',(-1.18423354154716E-48,1.09469422570892E-48,
1.));
#45681=DIRECTION('ref_axis',(-0.996917333733132,-0.0784590957277897,-1.09469422570898E-48));
#45682=DIRECTION('',(-1.18423354154716E-48,1.09469422570892E-48,1.));
#45683=DIRECTION('center_axis',(-0.479080630982844,0.877770897795706,-1.52823408562776E-48));
#45684=DIRECTION('ref_axis',(-0.877770897795706,-0.479080630982844,-1.85065299173653E-65));
#45685=DIRECTION('center_axis',(-0.408734674385335,-0.912653256146667,5.98602578707292E-49));
#45686=DIRECTION('ref_axis',(0.912653256146667,-0.408734674385335,-4.742731066544E-66));
#45687=DIRECTION('',(-1.18789542670764E-48,1.18789542670765E-48,1.));
#45688=DIRECTION('center_axis',(-1.18789542670764E-48,1.18789542670765E-48,
1.));
#45689=DIRECTION('ref_axis',(4.33680868994202E-19,-1.,1.18789542670765E-48));
#45690=DIRECTION('',(-1.18789542670764E-48,1.18789542670765E-48,1.));
#45691=DIRECTION('center_axis',(-0.408734674385331,0.912653256146669,-1.56967067958564E-48));
#45692=DIRECTION('ref_axis',(-0.912653256146669,-0.408734674385331,-1.44539080722799E-64));
#45693=DIRECTION('center_axis',(-0.479080630982847,-0.877770897795704,5.57165984749406E-49));
#45694=DIRECTION('ref_axis',(0.877770897795704,-0.479080630982847,-3.32989513528092E-65));
#45695=DIRECTION('',(-1.18423354154716E-48,1.28109662770637E-48,1.));
#45696=DIRECTION('center_axis',(-1.18423354154716E-48,1.28109662770637E-48,
1.));
#45697=DIRECTION('ref_axis',(4.33680868994202E-19,-1.,1.28109662770637E-48));
#45698=DIRECTION('',(-1.18423354154716E-48,1.28109662770637E-48,1.));
#45699=DIRECTION('center_axis',(-0.335868732602161,0.941908803685483,-1.60442321071283E-48));
#45700=DIRECTION('ref_axis',(-0.941908803685483,-0.335868732602161,-1.10077185323049E-64));
#45701=DIRECTION('center_axis',(-0.546472896179874,-0.837476789971388,5.09300798341636E-49));
#45702=DIRECTION('ref_axis',(0.837476789971388,-0.546472896179874,-4.24396990687181E-65));
#45703=DIRECTION('',(-1.17327046280542E-48,1.37372321230839E-48,1.));
#45704=DIRECTION('center_axis',(-1.17327046280542E-48,1.37372321230839E-48,
1.));
#45705=DIRECTION('ref_axis',(4.33680868994202E-19,-1.,1.37372321230839E-48));
#45706=DIRECTION('',(-1.17327046280542E-48,1.37372321230839E-48,1.));
#45707=DIRECTION('center_axis',(-0.260932048394812,0.965357170233115,-1.63227741809852E-48));
#45708=DIRECTION('ref_axis',(-0.965357170233115,-0.260932048394812,1.79840374663787E-65));
#45709=DIRECTION('center_axis',(-0.610495974251274,-0.792019359247605,4.55302124274975E-49));
#45710=DIRECTION('ref_axis',(0.792019359247605,-0.610495974251274,-1.92107929694605E-65));
#45711=DIRECTION('',(-1.15507378150847E-48,1.46520410681818E-48,1.));
#45712=DIRECTION('center_axis',(-1.15507378150847E-48,1.46520410681818E-48,
1.));
#45713=DIRECTION('ref_axis',(4.33680868994202E-19,-1.,1.46520410681818E-48));
#45714=DIRECTION('',(-1.15507378150847E-48,1.46520410681818E-48,1.));
#45715=DIRECTION('center_axis',(-0.184386631340398,0.982853788812426,-1.65306157129174E-48));
#45716=DIRECTION('ref_axis',(-0.982853788812426,-0.184386631340398,3.00112067034686E-65));
#45717=DIRECTION('center_axis',(-0.670755141630903,-0.741678865800898,3.95502882331426E-49));
#45718=DIRECTION('ref_axis',(0.741678865800898,-0.670755141630903,1.84878394507284E-65));
#45719=DIRECTION('',(-1.12975568624751E-48,1.55497530110059E-48,1.));
#45720=DIRECTION('center_axis',(-1.12975568624751E-48,1.55497530110059E-48,
1.));
#45721=DIRECTION('ref_axis',(4.33680868994202E-19,-1.,1.55497530110059E-48));
#45722=DIRECTION('',(-1.12975568624751E-48,1.55497530110059E-48,1.));
#45723=DIRECTION('center_axis',(-0.106704409388993,0.994290786951657,-1.66664752907659E-48));
#45724=DIRECTION('ref_axis',(-0.994290786951658,-0.106704409388993,-2.84767254643969E-65));
#45725=DIRECTION('center_axis',(-0.726878880513659,-0.686765675513279,3.30271754722836E-49));
#45726=DIRECTION('ref_axis',(0.686765675513279,-0.726878880513659,1.35737227185702E-66));
#45727=DIRECTION('',(-1.09747227149895E-48,1.64248332589092E-48,1.));
#45728=DIRECTION('center_axis',(-1.09747227149895E-48,1.64248332589092E-48,
1.));
#45729=DIRECTION('ref_axis',(4.33680868994202E-19,-1.,1.64248332589092E-48));
#45730=DIRECTION('',(-1.09747227149895E-48,1.64248332589092E-48,1.));
#45731=DIRECTION('center_axis',(-0.0283643192708891,0.999597651754094,-1.67295152950556E-48));
#45732=DIRECTION('ref_axis',(-0.999597651754094,-0.0283643192708891,-1.01926051780483E-65));
#45733=DIRECTION('center_axis',(-0.778521169386292,-0.627618346463358,2.60010913042463E-49));
#45734=DIRECTION('ref_axis',(0.627618346463358,-0.778521169386292,-1.77736454987801E-64));
#45735=DIRECTION('',(-1.05842257525003E-48,1.72718866511697E-48,1.));
#45736=DIRECTION('center_axis',(-1.05842257525003E-48,1.72718866511697E-48,
1.));
#45737=DIRECTION('ref_axis',(-0.891006524188322,0.453990499739636,-1.72718866511707E-48));
#45738=DIRECTION('',(-1.05842257525003E-48,1.72718866511697E-48,1.));
#45739=DIRECTION('center_axis',(0.050150646307614,0.998741664633517,-1.67193470631971E-48));
#45740=DIRECTION('ref_axis',(-0.998741664633517,0.050150646307614,1.52017605534737E-65));
#45741=DIRECTION('center_axis',(-0.8253636163651,-0.564601541603213,1.85153538743368E-49));
#45742=DIRECTION('ref_axis',(0.564601541603213,-0.8253636163651,-7.9609822926636E-66));
#45743=DIRECTION('',(-1.01284735186348E-48,1.80856908219503E-48,1.));
#45744=DIRECTION('center_axis',(-1.01284735186348E-48,1.80856908219503E-48,
1.));
#45745=DIRECTION('ref_axis',(-0.852640164354107,0.522498564715924,-1.808569082195E-48));
#45746=DIRECTION('',(-1.01284735186348E-48,1.80856908219503E-48,1.));
#45747=DIRECTION('center_axis',(0.128356416474848,0.991728103035169,-1.6636033285721E-48));
#45748=DIRECTION('ref_axis',(-0.991728103035169,0.128356416474848,-6.99057875847398E-66));
#45749=DIRECTION('center_axis',(-0.867117422187763,-0.498103780490019,1.06161152430708E-49));
#45750=DIRECTION('ref_axis',(0.498103780490019,-0.867117422187763,1.00088346227585E-65));
#45751=DIRECTION('',(-9.61027587746759E-49,1.88612283979207E-48,1.));
#45752=DIRECTION('center_axis',(-9.61027587746759E-49,1.88612283979207E-48,
1.));
#45753=DIRECTION('ref_axis',(-0.809016994374894,0.587785252292546,-1.88612283979215E-48));
#45754=DIRECTION('',(-9.61027587746759E-49,1.88612283979207E-48,1.));
#45755=DIRECTION('center_axis',(0.205770826651675,0.978600207898551,-1.64800876197701E-48));
#45756=DIRECTION('ref_axis',(-0.978600207898551,0.205770826651675,2.0991990898783E-65));
#45757=DIRECTION('center_axis',(-0.903525160756836,-0.428535043933789,2.35207684337335E-50));
#45758=DIRECTION('ref_axis',(0.428535043933789,-0.903525160756836,-9.18347163738211E-68));
#45759=DIRECTION('',(-9.03282768977482E-49,1.95937179320328E-48,1.));
#45760=DIRECTION('center_axis',(-9.03282768977482E-49,1.95937179320328E-48,
1.));
#45761=DIRECTION('ref_axis',(-0.760405965599999,0.649448048330221,-1.95937179320332E-48));
#45762=DIRECTION('',(-9.03282768977482E-49,1.95937179320328E-48,1.));
#45763=DIRECTION('center_axis',(0.281916591256451,0.959438917062646,-1.62524715222323E-48));
#45764=DIRECTION('ref_axis',(-0.959438917062646,0.281916591256451,8.99283719863503E-66));
#45765=DIRECTION('center_axis',(-0.934362366257238,-0.356324246329344,-6.22581077994971E-50));
#45766=DIRECTION('ref_axis',(0.356324246329344,-0.934362366257238,-2.14283631075808E-67));
#45767=DIRECTION('',(-8.39968911565457E-49,2.02786433827311E-48,1.));
#45768=DIRECTION('center_axis',(-8.39968911565457E-49,2.02786433827311E-48,
1.));
#45769=DIRECTION('ref_axis',(-0.707106781186559,0.707106781186536,-2.02786433827309E-48));
#45770=DIRECTION('',(-8.39968911565457E-49,2.02786433827311E-48,1.));
#45771=DIRECTION('center_axis',(0.356324246329351,0.934362366257235,-1.59545883220388E-48));
#45772=DIRECTION('ref_axis',(-0.934362366257235,0.356324246329351,6.60900149289003E-65));
#45773=DIRECTION('center_axis',(-0.959438917062648,-0.281916591256444,-1.50646620972636E-49));
#45774=DIRECTION('ref_axis',(0.281916591256444,-0.959438917062648,3.84808191287826E-66));
#45775=DIRECTION('',(-7.71476366495624E-49,2.09117819568513E-48,1.));
#45776=DIRECTION('center_axis',(-7.71476366495624E-49,2.09117819568513E-48,
1.));
#45777=DIRECTION('ref_axis',(-0.649448048330135,0.760405965600073,-2.09117819568518E-48));
#45778=DIRECTION('',(-7.71476366495624E-49,2.09117819568513E-48,1.));
#45779=DIRECTION('center_axis',(0.428535043933796,0.903525160756832,-1.5588274568175E-48));
#45780=DIRECTION('ref_axis',(-0.903525160756832,0.428535043933796,-3.10862492143316E-66));
#45781=DIRECTION('center_axis',(-0.978600207898552,-0.205770826651667,-2.41099826509806E-49));
#45782=DIRECTION('ref_axis',(0.205770826651667,-0.978600207898552,1.22158844253494E-66));
#45783=DIRECTION('',(-6.98227413084421E-49,2.14892301445441E-48,1.));
#45784=DIRECTION('center_axis',(-6.98227413084421E-49,2.14892301445441E-48,
1.));
#45785=DIRECTION('ref_axis',(-0.587785252292501,0.809016994374927,-2.14892301445438E-48));
#45786=DIRECTION('',(-6.98227413084421E-49,2.14892301445441E-48,1.));
#45787=DIRECTION('center_axis',(0.498103780490025,0.867117422187759,-1.51557887067454E-48));
#45788=DIRECTION('ref_axis',(-0.867117422187759,0.498103780490025,2.99504754920617E-65));
#45789=DIRECTION('center_axis',(-0.99172810303517,-0.128356416474841,-3.33060050320128E-49));
#45790=DIRECTION('ref_axis',(0.128356416474841,-0.99172810303517,-3.10963647347836E-66));
#45791=DIRECTION('',(-6.20673655487377E-49,2.20074277857113E-48,1.));
#45792=DIRECTION('center_axis',(-6.20673655487377E-49,2.20074277857113E-48,
1.));
#45793=DIRECTION('ref_axis',(-0.522498564715884,0.852640164354132,-2.20074277857117E-48));
#45794=DIRECTION('',(-6.20673655487377E-49,2.20074277857113E-48,1.));
#45795=DIRECTION('center_axis',(0.564601541603219,0.825363616365096,-1.46597971569015E-48));
#45796=DIRECTION('ref_axis',(-0.825363616365096,0.564601541603219,-1.28895308917342E-64));
#45797=DIRECTION('center_axis',(-0.998741664633517,-0.0501506463076061,
-4.25960327043935E-49));
#45798=DIRECTION('ref_axis',(0.0501506463076061,-0.998741664633517,-2.80568036684895E-66));
#45799=DIRECTION('',(-5.39293238409318E-49,2.24631800195768E-48,1.));
#45800=DIRECTION('center_axis',(-5.39293238409318E-49,2.24631800195768E-48,
1.));
#45801=DIRECTION('ref_axis',(-0.453990499739489,0.891006524188397,-2.24631800195771E-48));
#45802=DIRECTION('',(-5.39293238409318E-49,2.24631800195768E-48,1.));
#45803=DIRECTION('center_axis',(0.627618346463364,0.778521169386287,-1.41033578714823E-48));
#45804=DIRECTION('ref_axis',(-0.778521169386288,0.627618346463364,5.07659402759256E-65));
#45805=DIRECTION('center_axis',(-0.999597651754094,0.0283643192708965,-5.19227895582746E-49));
#45806=DIRECTION('ref_axis',(-0.0283643192708965,-0.999597651754094,2.50391620144835E-67));
#45807=DIRECTION('',(-4.54587899183267E-49,2.2853676982066E-48,1.));
#45808=DIRECTION('center_axis',(-4.54587899183267E-49,2.2853676982066E-48,
1.));
#45809=DIRECTION('ref_axis',(-0.382683432365006,0.923879532511321,-2.28536769820664E-48));
#45810=DIRECTION('',(-4.54587899183267E-49,2.2853676982066E-48,1.));
#45811=DIRECTION('center_axis',(0.686765675513284,0.726878880513654,-1.34899014837172E-48));
#45812=DIRECTION('ref_axis',(-0.726878880513654,0.686765675513284,4.51664321804638E-65));
#45813=DIRECTION('center_axis',(-0.994290786951657,0.106704409389001,-6.12287730361908E-49));
#45814=DIRECTION('ref_axis',(-0.106704409389001,-0.994290786951657,-3.36897451344462E-66));
#45815=DIRECTION('',(-3.67079874392934E-49,2.31765111295516E-48,1.));
#45816=DIRECTION('center_axis',(-3.67079874392934E-49,2.31765111295516E-48,
1.));
#45817=DIRECTION('ref_axis',(-0.309016994374936,0.951056516295157,-2.31765111295516E-48));
#45818=DIRECTION('',(-3.67079874392934E-49,2.31765111295516E-48,1.));
#45819=DIRECTION('center_axis',(0.741678865800904,0.670755141630897,-1.28232101562316E-48));
#45820=DIRECTION('ref_axis',(-0.670755141630897,0.741678865800904,-7.13448931820408E-65));
#45821=DIRECTION('center_axis',(-0.982853788812424,0.184386631340406,-7.04566086554469E-49));
#45822=DIRECTION('ref_axis',(-0.184386631340406,-0.982853788812424,1.03257498418151E-65));
#45823=DIRECTION('',(-2.77308680110524E-49,2.34296920821612E-48,1.));
#45824=DIRECTION('center_axis',(-2.77308680110524E-49,2.34296920821612E-48,
1.));
#45825=DIRECTION('ref_axis',(-0.233445363855831,0.972369920397695,-2.34296920821614E-48));
#45826=DIRECTION('',(-2.77308680110524E-49,2.34296920821612E-48,1.));
#45827=DIRECTION('center_axis',(0.79201935924761,0.610495974251268,-1.21073942627568E-48));
#45828=DIRECTION('ref_axis',(-0.610495974251268,0.79201935924761,-4.36775682720849E-65));
#45829=DIRECTION('center_axis',(-0.965357170233113,0.260932048394819,-7.95494037408836E-49));
#45830=DIRECTION('ref_axis',(-0.260932048394819,-0.965357170233113,-3.47978634051958E-65));
#45831=DIRECTION('',(-1.85827785600739E-49,2.36116588951307E-48,1.));
#45832=DIRECTION('center_axis',(-1.85827785600739E-49,2.36116588951307E-48,
1.));
#45833=DIRECTION('ref_axis',(-0.156434465040246,0.987688340595135,-2.36116588951307E-48));
#45834=DIRECTION('',(-1.85827785600739E-49,2.36116588951307E-48,1.));
#45835=DIRECTION('center_axis',(0.837476789971392,0.546472896179868,-1.13468670463092E-48));
#45836=DIRECTION('ref_axis',(-0.546472896179868,0.837476789971392,7.35185048458512E-65));
#45837=DIRECTION('center_axis',(-0.94190880368548,0.335868732602169,-8.84510981871381E-49));
#45838=DIRECTION('ref_axis',(-0.335868732602169,-0.94190880368548,-2.80378683690505E-64));
#45839=DIRECTION('',(-9.32012009987159E-50,2.3721289682548E-48,1.));
#45840=DIRECTION('center_axis',(-9.32012009987159E-50,2.3721289682548E-48,
1.));
#45841=DIRECTION('ref_axis',(-0.0784590957277844,0.996917333733133,-2.3721289682548E-48));
#45842=DIRECTION('',(-9.32012009987159E-50,2.3721289682548E-48,1.));
#45843=DIRECTION('center_axis',(0.877770897795708,0.47908063098284,-1.0546317410079E-48));
#45844=DIRECTION('ref_axis',(-0.47908063098284,0.877770897795708,-1.46432166581228E-64));
#45845=DIRECTION('center_axis',(-0.912653256146669,0.408734674385332,-9.71068100878346E-49));
#45846=DIRECTION('ref_axis',(-0.408734674385332,-0.912653256146669,4.78015562106795E-65));
#45847=DIRECTION('',(-1.03033504185762E-66,2.37579085341529E-48,1.));
#45848=DIRECTION('center_axis',(-1.03033504185762E-66,2.37579085341529E-48,
1.));
#45849=DIRECTION('ref_axis',(-5.51899603821915E-14,1.,-2.37579085341529E-48));
#45850=DIRECTION('',(-1.03033504185762E-66,2.37579085341529E-48,1.));
#45851=DIRECTION('center_axis',(0.912653256146668,0.408734674385334,-9.71068100878352E-49));
#45852=DIRECTION('ref_axis',(-0.408734674385334,0.912653256146668,-3.97320112854764E-64));
#45853=DIRECTION('center_axis',(-0.877770897795703,0.47908063098285,-1.05463174100791E-48));
#45854=DIRECTION('ref_axis',(-0.47908063098285,-0.877770897795703,8.5181126283276E-66));
#45855=DIRECTION('',(9.32012009987329E-50,2.3721289682548E-48,1.));
#45856=DIRECTION('center_axis',(9.32012009987329E-50,2.3721289682548E-48,
1.));
#45857=DIRECTION('ref_axis',(0.078459095727909,0.996917333733123,-2.37212896825479E-48));
#45858=DIRECTION('',(9.32012009987329E-50,2.3721289682548E-48,1.));
#45859=DIRECTION('center_axis',(0.941908803685484,0.335868732602158,-8.84510981871371E-49));
#45860=DIRECTION('ref_axis',(-0.335868732602158,0.941908803685484,-1.44601818635795E-65));
#45861=DIRECTION('center_axis',(-0.837476789971386,0.546472896179877,-1.13468670463093E-48));
#45862=DIRECTION('ref_axis',(-0.546472896179877,-0.837476789971386,1.1507371701338E-64));
#45863=DIRECTION('',(1.85827785600756E-49,2.36116588951307E-48,1.));
#45864=DIRECTION('center_axis',(1.85827785600756E-49,2.36116588951307E-48,
1.));
#45865=DIRECTION('ref_axis',(0.156434465040226,0.987688340595138,-2.36116588951307E-48));
#45866=DIRECTION('',(1.85827785600756E-49,2.36116588951307E-48,1.));
#45867=DIRECTION('center_axis',(0.965357170233116,0.260932048394809,-7.95494037408827E-49));
#45868=DIRECTION('ref_axis',(-0.260932048394809,0.965357170233116,-4.20694512990981E-65));
#45869=DIRECTION('center_axis',(-0.792019359247603,0.610495974251277,-1.21073942627569E-48));
#45870=DIRECTION('ref_axis',(-0.610495974251277,-0.792019359247603,-2.13945998802071E-65));
#45871=DIRECTION('',(2.7730868011054E-49,2.34296920821612E-48,1.));
#45872=DIRECTION('center_axis',(2.7730868011054E-49,2.34296920821612E-48,
1.));
#45873=DIRECTION('ref_axis',(0.233445363855898,0.972369920397678,-2.34296920821612E-48));
#45874=DIRECTION('',(2.7730868011054E-49,2.34296920821612E-48,1.));
#45875=DIRECTION('center_axis',(0.982853788812426,0.184386631340395,-7.04566086554459E-49));
#45876=DIRECTION('ref_axis',(-0.184386631340395,0.982853788812426,-1.76256118611904E-65));
#45877=DIRECTION('center_axis',(-0.741678865800896,0.670755141630906,-1.28232101562316E-48));
#45878=DIRECTION('ref_axis',(-0.670755141630906,-0.741678865800896,1.75561258236883E-65));
#45879=DIRECTION('',(3.6707987439295E-49,2.31765111295516E-48,1.));
#45880=DIRECTION('center_axis',(3.6707987439295E-49,2.31765111295516E-48,
1.));
#45881=DIRECTION('ref_axis',(0.309016994374949,0.951056516295153,-2.31765111295516E-48));
#45882=DIRECTION('',(3.6707987439295E-49,2.31765111295516E-48,1.));
#45883=DIRECTION('center_axis',(0.994290786951658,0.10670440938899,-6.12287730361897E-49));
#45884=DIRECTION('ref_axis',(-0.10670440938899,0.994290786951658,-7.83421067979577E-66));
#45885=DIRECTION('center_axis',(-0.686765675513276,0.726878880513661,-1.34899014837172E-48));
#45886=DIRECTION('ref_axis',(-0.726878880513661,-0.686765675513276,5.3563970103269E-65));
#45887=DIRECTION('',(4.54587899183282E-49,2.28536769820659E-48,1.));
#45888=DIRECTION('center_axis',(4.54587899183282E-49,2.28536769820659E-48,
1.));
#45889=DIRECTION('ref_axis',(0.382683432365024,0.923879532511314,-2.28536769820663E-48));
#45890=DIRECTION('',(4.54587899183282E-49,2.28536769820659E-48,1.));
#45891=DIRECTION('center_axis',(0.999597651754094,0.0283643192708856,-5.19227895582736E-49));
#45892=DIRECTION('ref_axis',(-0.0283643192708856,0.999597651754094,1.94568536261846E-66));
#45893=DIRECTION('center_axis',(-0.627618346463355,0.778521169386295,-1.41033578714824E-48));
#45894=DIRECTION('ref_axis',(-0.778521169386295,-0.627618346463355,-4.32781502974933E-65));
#45895=DIRECTION('',(5.39293238409334E-49,2.24631800195767E-48,1.));
#45896=DIRECTION('center_axis',(5.39293238409334E-49,2.24631800195767E-48,
1.));
#45897=DIRECTION('ref_axis',(0.45399049973962,0.89100652418833,-2.24631800195763E-48));
#45898=DIRECTION('',(5.39293238409334E-49,2.24631800195767E-48,1.));
#45899=DIRECTION('center_axis',(0.998741664633517,-0.0501506463076175,-4.25960327043925E-49));
#45900=DIRECTION('ref_axis',(0.0501506463076175,0.998741664633517,-4.14088422014228E-66));
#45901=DIRECTION('center_axis',(-0.56460154160321,0.825363616365102,-1.46597971569016E-48));
#45902=DIRECTION('ref_axis',(-0.825363616365102,-0.56460154160321,7.97777118454868E-65));
#45903=DIRECTION('',(6.20673655487391E-49,2.20074277857112E-48,1.));
#45904=DIRECTION('center_axis',(6.20673655487391E-49,2.20074277857112E-48,
1.));
#45905=DIRECTION('ref_axis',(0.522498564715976,0.852640164354076,-2.20074277857111E-48));
#45906=DIRECTION('',(6.20673655487391E-49,2.20074277857112E-48,1.));
#45907=DIRECTION('center_axis',(0.991728103035169,-0.128356416474851,-3.33060050320119E-49));
#45908=DIRECTION('ref_axis',(0.128356416474851,0.991728103035169,2.08257490756294E-67));
#45909=DIRECTION('center_axis',(-0.498103780490015,0.867117422187765,-1.51557887067454E-48));
#45910=DIRECTION('ref_axis',(-0.867117422187765,-0.498103780490015,2.18779707200991E-65));
#45911=DIRECTION('',(6.98227413084436E-49,2.1489230144544E-48,1.));
#45912=DIRECTION('center_axis',(6.98227413084435E-49,2.1489230144544E-48,
1.));
#45913=DIRECTION('ref_axis',(0.587785252292489,0.809016994374936,-2.14892301445439E-48));
#45914=DIRECTION('',(6.98227413084436E-49,2.1489230144544E-48,1.));
#45915=DIRECTION('center_axis',(0.97860020789855,-0.205770826651679,-2.41099826509796E-49));
#45916=DIRECTION('ref_axis',(0.205770826651679,0.97860020789855,-2.74077973100627E-66));
#45917=DIRECTION('center_axis',(-0.428535043933785,0.903525160756837,-1.55882745681751E-48));
#45918=DIRECTION('ref_axis',(-0.903525160756837,-0.428535043933785,-8.73188639847288E-65));
#45919=DIRECTION('',(7.71476366495637E-49,2.09117819568512E-48,1.));
#45920=DIRECTION('center_axis',(7.71476366495637E-49,2.09117819568512E-48,
1.));
#45921=DIRECTION('ref_axis',(0.649448048330186,0.760405965600029,-2.09117819568512E-48));
#45922=DIRECTION('',(7.71476366495637E-49,2.09117819568512E-48,1.));
#45923=DIRECTION('center_axis',(0.959438917062645,-0.281916591256455,-1.50646620972626E-49));
#45924=DIRECTION('ref_axis',(0.281916591256455,0.959438917062645,-2.91844467010393E-67));
#45925=DIRECTION('center_axis',(-0.356324246329341,0.934362366257239,-1.59545883220388E-48));
#45926=DIRECTION('ref_axis',(-0.934362366257239,-0.356324246329341,1.49301625507406E-64));
#45927=DIRECTION('',(8.39968911565469E-49,2.0278643382731E-48,1.));
#45928=DIRECTION('center_axis',(8.39968911565469E-49,2.0278643382731E-48,
1.));
#45929=DIRECTION('ref_axis',(0.707106781186573,0.707106781186522,-2.02786433827308E-48));
#45930=DIRECTION('',(8.39968911565469E-49,2.0278643382731E-48,1.));
#45931=DIRECTION('center_axis',(0.934362366257234,-0.356324246329355,-6.22581077994883E-50));
#45932=DIRECTION('ref_axis',(0.356324246329355,0.934362366257234,-4.97582464336991E-66));
#45933=DIRECTION('center_axis',(-0.28191659125644,0.959438917062649,-1.62524715222323E-48));
#45934=DIRECTION('ref_axis',(-0.959438917062649,-0.28191659125644,-5.29515836320384E-66));
#45935=DIRECTION('',(9.03282768977493E-49,1.95937179320326E-48,1.));
#45936=DIRECTION('center_axis',(9.03282768977493E-49,1.95937179320326E-48,
1.));
#45937=DIRECTION('ref_axis',(0.760405965600079,0.649448048330127,-1.9593717932032E-48));
#45938=DIRECTION('',(9.03282768977493E-49,1.95937179320326E-48,1.));
#45939=DIRECTION('center_axis',(0.903525160756831,-0.428535043933799,2.35207684337425E-50));
#45940=DIRECTION('ref_axis',(0.428535043933799,0.903525160756831,3.46790681006673E-67));
#45941=DIRECTION('center_axis',(-0.205770826651664,0.978600207898553,-1.64800876197701E-48));
#45942=DIRECTION('ref_axis',(-0.978600207898553,-0.205770826651664,-5.70930081633759E-65));
#45943=DIRECTION('',(9.61027587746769E-49,1.88612283979206E-48,1.));
#45944=DIRECTION('center_axis',(9.61027587746769E-49,1.88612283979206E-48,
1.));
#45945=DIRECTION('ref_axis',(0.809016994374978,0.587785252292432,-1.88612283979202E-48));
#45946=DIRECTION('',(9.61027587746769E-49,1.88612283979206E-48,1.));
#45947=DIRECTION('center_axis',(0.867117422187757,-0.498103780490029,1.06161152430717E-49));
#45948=DIRECTION('ref_axis',(0.498103780490029,0.867117422187757,8.6756046158998E-66));
#45949=DIRECTION('center_axis',(-0.128356416474837,0.991728103035171,-1.6636033285721E-48));
#45950=DIRECTION('ref_axis',(-0.991728103035171,-0.128356416474837,3.98742758462882E-65));
#45951=DIRECTION('',(1.01284735186348E-48,1.80856908219502E-48,1.));
#45952=DIRECTION('center_axis',(1.01284735186348E-48,1.80856908219502E-48,
1.));
#45953=DIRECTION('ref_axis',(0.852640164354111,0.522498564715918,-1.80856908219499E-48));
#45954=DIRECTION('',(1.01284735186348E-48,1.80856908219502E-48,1.));
#45955=DIRECTION('center_axis',(0.825363616365094,-0.564601541603222,1.85153538743376E-49));
#45956=DIRECTION('ref_axis',(0.564601541603222,0.825363616365094,-1.20460226317478E-65));
#45957=DIRECTION('center_axis',(-0.0501506463076026,0.998741664633518,-1.67193470631971E-48));
#45958=DIRECTION('ref_axis',(-0.998741664633518,-0.0501506463076026,9.17993822873344E-66));
#45959=DIRECTION('',(1.05842257525004E-48,1.72718866511696E-48,1.));
#45960=DIRECTION('center_axis',(1.05842257525004E-48,1.72718866511696E-48,
1.));
#45961=DIRECTION('ref_axis',(0.891006524188331,0.453990499739619,-1.72718866511705E-48));
#45962=DIRECTION('',(1.05842257525004E-48,1.72718866511696E-48,1.));
#45963=DIRECTION('center_axis',(0.778521169386285,-0.627618346463367,2.6001091304247E-49));
#45964=DIRECTION('ref_axis',(0.627618346463367,0.778521169386285,-2.38387219843189E-65));
#45965=DIRECTION('center_axis',(0.0283643192709005,0.999597651754094,-1.67295152950556E-48));
#45966=DIRECTION('ref_axis',(-0.999597651754094,0.0283643192709005,5.71503284305285E-66));
#45967=DIRECTION('',(1.09747227149896E-48,1.6424833258909E-48,1.));
#45968=DIRECTION('center_axis',(1.09747227149896E-48,1.6424833258909E-48,
1.));
#45969=DIRECTION('ref_axis',(4.33680868994202E-19,-1.,1.6424833258909E-48));
#45970=DIRECTION('',(1.09747227149896E-48,1.6424833258909E-48,1.));
#45971=DIRECTION('center_axis',(0.726878880513651,-0.686765675513287,3.30271754722842E-49));
#45972=DIRECTION('ref_axis',(0.686765675513287,0.726878880513651,-2.02185804836064E-65));
#45973=DIRECTION('center_axis',(0.106704409389004,0.994290786951656,-1.66664752907659E-48));
#45974=DIRECTION('ref_axis',(-0.994290786951656,0.106704409389004,-7.60908949083185E-66));
#45975=DIRECTION('',(1.12975568624752E-48,1.55497530110057E-48,1.));
#45976=DIRECTION('center_axis',(1.12975568624752E-48,1.55497530110057E-48,
1.));
#45977=DIRECTION('ref_axis',(4.33680868994202E-19,-1.,1.55497530110057E-48));
#45978=DIRECTION('',(1.12975568624752E-48,1.55497530110057E-48,1.));
#45979=DIRECTION('center_axis',(0.670755141630895,-0.741678865800906,3.95502882331431E-49));
#45980=DIRECTION('ref_axis',(0.741678865800906,0.670755141630895,-5.99583083400171E-67));
#45981=DIRECTION('center_axis',(0.184386631340409,0.982853788812424,-1.65306157129173E-48));
#45982=DIRECTION('ref_axis',(-0.982853788812424,0.184386631340409,2.90870213757036E-65));
#45983=DIRECTION('',(1.15507378150848E-48,1.46520410681816E-48,1.));
#45984=DIRECTION('center_axis',(1.15507378150848E-48,1.46520410681816E-48,
1.));
#45985=DIRECTION('ref_axis',(4.33680868994202E-19,-1.,1.46520410681816E-48));
#45986=DIRECTION('',(1.15507378150848E-48,1.46520410681816E-48,1.));
#45987=DIRECTION('center_axis',(0.610495974251266,-0.792019359247612,4.5530212427498E-49));
#45988=DIRECTION('ref_axis',(0.792019359247612,0.610495974251266,2.91962028883906E-65));
#45989=DIRECTION('center_axis',(0.260932048394823,0.965357170233112,-1.63227741809852E-48));
#45990=DIRECTION('ref_axis',(-0.965357170233112,0.260932048394823,3.06323067308603E-65));
#45991=DIRECTION('',(1.17327046280543E-48,1.37372321230838E-48,1.));
#45992=DIRECTION('center_axis',(1.17327046280543E-48,1.37372321230838E-48,
1.));
#45993=DIRECTION('ref_axis',(4.33680868994202E-19,-1.,1.37372321230838E-48));
#45994=DIRECTION('',(1.17327046280543E-48,1.37372321230838E-48,1.));
#45995=DIRECTION('center_axis',(0.546472896179865,-0.837476789971394,5.0930079834164E-49));
#45996=DIRECTION('ref_axis',(0.837476789971394,0.546472896179865,-4.56422939014991E-65));
#45997=DIRECTION('center_axis',(0.335868732602171,0.94190880368548,-1.60442321071282E-48));
#45998=DIRECTION('ref_axis',(-0.94190880368548,0.335868732602171,4.87630450545203E-65));
#45999=DIRECTION('',(1.18423354154716E-48,1.28109662770635E-48,1.));
#46000=DIRECTION('center_axis',(1.18423354154716E-48,1.28109662770635E-48,
1.));
#46001=DIRECTION('ref_axis',(4.33680868994202E-19,-1.,1.28109662770635E-48));
#46002=DIRECTION('',(1.18423354154716E-48,1.28109662770635E-48,1.));
#46003=DIRECTION('center_axis',(0.479080630982838,-0.87777089779571,5.57165984749409E-49));
#46004=DIRECTION('ref_axis',(0.87777089779571,0.479080630982838,-3.73128804317402E-67));
#46005=DIRECTION('center_axis',(0.408734674385341,0.912653256146664,-1.56967067958563E-48));
#46006=DIRECTION('ref_axis',(-0.912653256146664,0.408734674385341,1.45818743306131E-64));
#46007=DIRECTION('center_axis',(0.408734674385325,-0.912653256146672,5.98602578707294E-49));
#46008=DIRECTION('ref_axis',(0.912653256146672,0.408734674385325,1.90174553100142E-65));
#46009=DIRECTION('center_axis',(0.479080630982853,0.877770897795701,-1.52823408562775E-48));
#46010=DIRECTION('ref_axis',(-0.877770897795701,0.479080630982853,5.61428358120402E-65));
#46011=DIRECTION('center_axis',(0.335868732602155,-0.941908803685485,6.33355109834479E-49));
#46012=DIRECTION('ref_axis',(0.941908803685485,0.335868732602155,-2.18452554190007E-64));
#46013=DIRECTION('center_axis',(0.54647289617988,0.837476789971384,-1.48036889921998E-48));
#46014=DIRECTION('ref_axis',(-0.837476789971384,0.54647289617988,1.0038841655118E-64));
#46015=DIRECTION('center_axis',(0.260932048394805,-0.965357170233117,6.61209317220175E-49));
#46016=DIRECTION('ref_axis',(0.965357170233117,0.260932048394805,-1.34731391844263E-65));
#46017=DIRECTION('center_axis',(0.61049597425128,0.792019359247601,-1.42637022515332E-48));
#46018=DIRECTION('ref_axis',(-0.792019359247601,0.61049597425128,4.68595517840464E-65));
#46019=DIRECTION('center_axis',(0.184386631340391,-0.982853788812427,6.81993470413385E-49));
#46020=DIRECTION('ref_axis',(0.982853788812427,0.184386631340391,-4.82159387328582E-66));
#46021=DIRECTION('center_axis',(0.670755141630908,0.741678865800894,-1.36657098320977E-48));
#46022=DIRECTION('ref_axis',(-0.741678865800894,0.670755141630908,-1.20021806126158E-65));
#46023=DIRECTION('center_axis',(0.106704409388986,-0.994290786951658,6.95579428198241E-49));
#46024=DIRECTION('ref_axis',(0.994290786951658,0.106704409388986,-5.2899598259714E-66));
#46025=DIRECTION('center_axis',(0.726878880513664,0.686765675513273,-1.30133985560118E-48));
#46026=DIRECTION('ref_axis',(-0.686765675513273,0.726878880513664,8.56568901676031E-65));
#46027=DIRECTION('center_axis',(0.0283643192708817,-0.999597651754094,7.01883428627211E-49));
#46028=DIRECTION('ref_axis',(0.999597651754094,0.0283643192708817,4.29698701010715E-68));
#46029=DIRECTION('',(0.,0.,1.));
#46030=DIRECTION('',(1.,0.,0.));
#46031=DIRECTION('',(-0.163575574020309,-0.060536595683074,0.98467169765716));
#46032=DIRECTION('',(0.982142874169732,-0.104027305303185,0.156759990013316));
#46033=DIRECTION('',(-0.0968071433172138,0.405176423927354,0.909098697884999));
#46034=DIRECTION('',(0.993373280453531,-0.0175195400607767,0.113589574332551));
#46035=DIRECTION('',(-0.0937297357406718,-0.0309243576449071,0.995117289942363));
#46036=DIRECTION('',(0.995214165618203,-0.0306505416385188,0.0927863613368385));
#46037=DIRECTION('',(-1.34745000483458E-16,1.48415263953167E-16,1.));
#46038=DIRECTION('',(1.,1.39598772945223E-16,1.34745000483458E-16));
#46039=DIRECTION('',(-4.78228900381487E-16,1.48408514308746E-16,0.999999999999998));
#46040=DIRECTION('',(0.999999999782535,2.08549463822771E-5,2.48761105950712E-16));
#46041=DIRECTION('',(8.06699589630575E-16,1.48433763848581E-16,1.));
#46042=DIRECTION('',(0.999999999782534,2.08549463826532E-5,5.81828013331679E-16));
#46043=DIRECTION('',(-1.14795680305951E-16,1.48415655968099E-16,1.));
#46044=DIRECTION('',(1.,1.39215914053064E-16,9.48463603322175E-17));
#46045=CARTESIAN_POINT('',(0.,0.,0.));
#46046=CARTESIAN_POINT('',(0.,0.,0.));
#46047=CARTESIAN_POINT('Origin',(7.4208747252167,4.28444402022635,12.));
#46048=CARTESIAN_POINT('',(4.94724981681114,8.56888804045271,12.));
#46049=CARTESIAN_POINT('',(0.,0.,6.));
#46050=CARTESIAN_POINT('',(2.02148035019019,3.50130667303153,8.45164132604064));
#46051=CARTESIAN_POINT('',(-11.5791252747833,37.193409364035,12.));
#46052=CARTESIAN_POINT('',(7.4208747252167,4.28444402022635,12.));
#46053=CARTESIAN_POINT('',(-19.,32.9089653438087,6.));
#46054=CARTESIAN_POINT('',(-19.,32.9089653438087,6.));
#46055=CARTESIAN_POINT('',(0.,0.,6.));
#46056=CARTESIAN_POINT('Origin',(-7.4208747252167,4.28444402022636,12.));
#46057=CARTESIAN_POINT('',(-9.89449963362226,3.88578058618805E-15,12.));
#46058=CARTESIAN_POINT('',(-4.04296070038038,1.66533453693773E-15,8.45164132604064));
#46059=CARTESIAN_POINT('',(-26.4208747252167,-28.6245213235823,12.));
#46060=CARTESIAN_POINT('',(-7.4208747252167,4.28444402022635,12.));
#46061=CARTESIAN_POINT('',(-19.,-32.9089653438087,6.));
#46062=CARTESIAN_POINT('',(-19.,-32.9089653438087,6.));
#46063=CARTESIAN_POINT('',(0.,0.,6.));
#46064=CARTESIAN_POINT('Origin',(0.,0.,6.));
#46065=CARTESIAN_POINT('',(4.94724981681113,-8.5688880404527,12.));
#46066=CARTESIAN_POINT('',(2.02148035019019,-3.50130667303154,8.45164132604064));
#46067=CARTESIAN_POINT('',(-11.5791252747833,-37.193409364035,12.));
#46068=CARTESIAN_POINT('',(-19.,-32.9089653438087,6.));
#46069=CARTESIAN_POINT('',(7.4208747252167,-4.28444402022635,12.));
#46070=CARTESIAN_POINT('Origin',(-19.,-32.9089653438087,9.));
#46071=CARTESIAN_POINT('',(-19.,-32.9089653438087,12.));
#46072=CARTESIAN_POINT('Origin',(0.,0.,6.));
#46073=CARTESIAN_POINT('',(-26.4208747252167,28.6245213235823,12.));
#46074=CARTESIAN_POINT('',(-19.,32.9089653438087,6.));
#46075=CARTESIAN_POINT('',(-7.4208747252167,-4.28444402022635,12.));
#46076=CARTESIAN_POINT('Origin',(-19.,32.9089653438087,9.));
#46077=CARTESIAN_POINT('',(-19.,32.9089653438087,12.));
#46078=CARTESIAN_POINT('Origin',(0.,0.,6.));
#46079=CARTESIAN_POINT('',(38.,0.,6.));
#46080=CARTESIAN_POINT('',(0.,0.,6.));
#46081=CARTESIAN_POINT('',(38.,8.5688880404527,12.));
#46082=CARTESIAN_POINT('',(38.,0.,6.));
#46083=CARTESIAN_POINT('',(0.,8.5688880404527,12.));
#46084=CARTESIAN_POINT('Origin',(0.,-8.56888804045271,12.));
#46085=CARTESIAN_POINT('',(38.,-8.56888804045271,12.));
#46086=CARTESIAN_POINT('',(0.,-8.5688880404527,12.));
#46087=CARTESIAN_POINT('',(38.,0.,6.));
#46088=CARTESIAN_POINT('Origin',(38.,1.11022302462516E-15,9.));
#46089=CARTESIAN_POINT('',(38.,5.55111512312578E-16,12.));
#46090=CARTESIAN_POINT('Origin',(0.,0.,0.));
#46091=CARTESIAN_POINT('',(-40.,-4.89858719658941E-15,12.));
#46092=CARTESIAN_POINT('Origin',(0.,0.,12.));
#46093=CARTESIAN_POINT('',(-40.,-4.89858719658941E-15,0.));
#46094=CARTESIAN_POINT('',(-40.,-4.89858719658941E-15,0.));
#46095=CARTESIAN_POINT('Origin',(0.,0.,0.));
#46096=CARTESIAN_POINT('Origin',(0.,0.,12.));
#46097=CARTESIAN_POINT('Origin',(0.,0.,0.));
#46098=CARTESIAN_POINT('',(0.,0.,0.));
#46099=CARTESIAN_POINT('Origin',(30.,-9.99200722162641E-15,13.));
#46100=CARTESIAN_POINT('',(30.,-9.99200722162641E-15,19.));
#46101=CARTESIAN_POINT('',(30.,-9.99200722162641E-15,7.));
#46102=CARTESIAN_POINT('Origin',(30.,-9.99200722162641E-15,13.));
#46103=CARTESIAN_POINT('',(0.,0.,0.));
#46104=CARTESIAN_POINT('Origin',(-15.,25.9807621135332,13.));
#46105=CARTESIAN_POINT('',(-15.,25.9807621135332,19.));
#46106=CARTESIAN_POINT('',(-15.,25.9807621135332,7.));
#46107=CARTESIAN_POINT('Origin',(-15.,25.9807621135332,13.));
#46108=CARTESIAN_POINT('',(0.,0.,0.));
#46109=CARTESIAN_POINT('Origin',(-15.,-25.9807621135331,13.));
#46110=CARTESIAN_POINT('',(-15.,-25.9807621135331,19.));
#46111=CARTESIAN_POINT('',(-15.,-25.9807621135331,6.99999999999999));
#46112=CARTESIAN_POINT('Origin',(-15.,-25.9807621135331,13.));
#46113=CARTESIAN_POINT('',(0.,0.,0.));
#46114=CARTESIAN_POINT('Origin',(-15.,-25.9807621135332,31.));
#46115=CARTESIAN_POINT('',(-15.75,-27.2798002192098,31.));
#46116=CARTESIAN_POINT('Origin',(-15.,-25.9807621135332,31.));
#46117=CARTESIAN_POINT('',(-15.75,-27.2798002192098,19.));
#46118=CARTESIAN_POINT('',(-15.75,-27.2798002192099,31.));
#46119=CARTESIAN_POINT('Origin',(-15.,-25.9807621135332,19.));
#46120=CARTESIAN_POINT('Origin',(-15.,25.9807621135332,31.));
#46121=CARTESIAN_POINT('',(-15.75,27.2798002192098,31.));
#46122=CARTESIAN_POINT('Origin',(-15.,25.9807621135332,31.));
#46123=CARTESIAN_POINT('',(-15.75,27.2798002192098,19.));
#46124=CARTESIAN_POINT('',(-15.75,27.2798002192099,31.));
#46125=CARTESIAN_POINT('Origin',(-15.,25.9807621135332,19.));
#46126=CARTESIAN_POINT('Origin',(30.,-9.99200722162641E-15,31.));
#46127=CARTESIAN_POINT('',(31.5,-9.8083102017543E-15,31.));
#46128=CARTESIAN_POINT('Origin',(30.,-9.99200722162641E-15,31.));
#46129=CARTESIAN_POINT('',(31.5,-9.8083102017543E-15,19.));
#46130=CARTESIAN_POINT('',(31.5,-1.01757042414985E-14,31.));
#46131=CARTESIAN_POINT('Origin',(30.,-9.99200722162641E-15,19.));
#46132=CARTESIAN_POINT('Origin',(8.66025403784439,15.,19.));
#46133=CARTESIAN_POINT('',(8.66025403784439,10.,19.));
#46134=CARTESIAN_POINT('',(4.3301270189222,12.5,19.));
#46135=CARTESIAN_POINT('Origin',(8.66025403784439,15.,19.));
#46136=CARTESIAN_POINT('',(4.3301270189222,12.5,31.));
#46137=CARTESIAN_POINT('',(4.3301270189222,12.5,19.));
#46138=CARTESIAN_POINT('',(8.66025403784439,10.,31.));
#46139=CARTESIAN_POINT('Origin',(8.66025403784439,15.,31.));
#46140=CARTESIAN_POINT('',(8.66025403784439,10.,19.));
#46141=CARTESIAN_POINT('Origin',(5.77350269189626,10.,19.));
#46142=CARTESIAN_POINT('',(-8.66025403784437,35.,19.));
#46143=CARTESIAN_POINT('',(8.66025403784439,5.,19.));
#46144=CARTESIAN_POINT('',(-8.66025403784437,35.,31.));
#46145=CARTESIAN_POINT('',(-8.66025403784438,35.,19.));
#46146=CARTESIAN_POINT('',(8.66025403784439,5.,31.));
#46147=CARTESIAN_POINT('Origin',(8.66025403784438,-15.,19.));
#46148=CARTESIAN_POINT('',(4.33012701892219,-12.5,19.));
#46149=CARTESIAN_POINT('',(8.66025403784438,-10.,19.));
#46150=CARTESIAN_POINT('Origin',(8.66025403784438,-15.,19.));
#46151=CARTESIAN_POINT('',(8.66025403784438,-10.,31.));
#46152=CARTESIAN_POINT('',(8.66025403784438,-10.,19.));
#46153=CARTESIAN_POINT('',(4.33012701892219,-12.5,31.));
#46154=CARTESIAN_POINT('Origin',(8.66025403784438,-15.,31.));
#46155=CARTESIAN_POINT('',(4.33012701892219,-12.5,19.));
#46156=CARTESIAN_POINT('Origin',(5.77350269189626,-10.,19.));
#46157=CARTESIAN_POINT('',(34.6410161513775,-10.,19.));
#46158=CARTESIAN_POINT('',(0.,-10.,19.));
#46159=CARTESIAN_POINT('',(34.6410161513775,-10.,31.));
#46160=CARTESIAN_POINT('',(34.6410161513775,-10.,19.));
#46161=CARTESIAN_POINT('',(0.,-10.,31.));
#46162=CARTESIAN_POINT('Origin',(-17.3205080756888,-2.22044604925031E-15,
19.));
#46163=CARTESIAN_POINT('',(-12.9903810567666,2.5,19.));
#46164=CARTESIAN_POINT('',(-12.9903810567666,-2.5,19.));
#46165=CARTESIAN_POINT('Origin',(-17.3205080756888,-2.22044604925031E-15,
19.));
#46166=CARTESIAN_POINT('',(-12.9903810567666,-2.5,31.));
#46167=CARTESIAN_POINT('',(-12.9903810567666,-2.5,19.));
#46168=CARTESIAN_POINT('',(-12.9903810567666,2.5,31.));
#46169=CARTESIAN_POINT('Origin',(-17.3205080756888,-2.22044604925031E-15,
31.));
#46170=CARTESIAN_POINT('',(-12.9903810567666,2.5,19.));
#46171=CARTESIAN_POINT('Origin',(-11.5470053837925,1.11022302462516E-15,
19.));
#46172=CARTESIAN_POINT('',(-25.9807621135332,-25.,19.));
#46173=CARTESIAN_POINT('',(-8.66025403784438,5.,19.));
#46174=CARTESIAN_POINT('',(-25.9807621135332,-25.,31.));
#46175=CARTESIAN_POINT('',(-25.9807621135332,-25.,19.));
#46176=CARTESIAN_POINT('',(-8.66025403784438,5.,31.));
#46177=CARTESIAN_POINT('Origin',(-12.9903810567666,-32.5,19.));
#46178=CARTESIAN_POINT('',(-8.6602540378444,-35.,31.));
#46179=CARTESIAN_POINT('',(-14.8461497791618,-37.1428571428571,31.));
#46180=CARTESIAN_POINT('Origin',(-12.9903810567666,-32.5,31.));
#46181=CARTESIAN_POINT('',(-14.8461497791618,-37.1428571428571,19.));
#46182=CARTESIAN_POINT('',(-14.8461497791618,-37.1428571428571,19.));
#46183=CARTESIAN_POINT('',(-8.6602540378444,-35.,19.));
#46184=CARTESIAN_POINT('Origin',(-12.9903810567666,-32.5,19.));
#46185=CARTESIAN_POINT('',(-8.6602540378444,-35.,19.));
#46186=CARTESIAN_POINT('Origin',(0.,0.,19.));
#46187=CARTESIAN_POINT('',(-24.7435829652697,-31.4285714285714,31.));
#46188=CARTESIAN_POINT('Origin',(0.,0.,31.));
#46189=CARTESIAN_POINT('',(-24.7435829652697,-31.4285714285714,19.));
#46190=CARTESIAN_POINT('',(-24.7435829652697,-31.4285714285714,19.));
#46191=CARTESIAN_POINT('Origin',(0.,0.,19.));
#46192=CARTESIAN_POINT('Origin',(5.98741461555926,0.,31.));
#46193=CARTESIAN_POINT('',(-10.7046626931927,-38.5410196624968,31.));
#46194=CARTESIAN_POINT('',(39.5897327444315,-5.71428571428572,31.));
#46195=CARTESIAN_POINT('Origin',(34.6410161513775,-5.,31.));
#46196=CARTESIAN_POINT('',(39.5897327444315,5.71428571428572,31.));
#46197=CARTESIAN_POINT('Origin',(0.,0.,31.));
#46198=CARTESIAN_POINT('',(34.6410161513775,10.,31.));
#46199=CARTESIAN_POINT('Origin',(34.6410161513775,5.,31.));
#46200=CARTESIAN_POINT('',(38.7298334620742,10.,31.));
#46201=CARTESIAN_POINT('',(-14.8461497791618,37.1428571428571,31.));
#46202=CARTESIAN_POINT('Origin',(-12.9903810567666,32.5,31.));
#46203=CARTESIAN_POINT('',(-24.7435829652697,31.4285714285714,31.));
#46204=CARTESIAN_POINT('Origin',(0.,0.,31.));
#46205=CARTESIAN_POINT('',(-25.9807621135332,25.,31.));
#46206=CARTESIAN_POINT('Origin',(-21.650635094611,27.5,31.));
#46207=CARTESIAN_POINT('',(-28.0251707688815,28.5410196624969,31.));
#46208=CARTESIAN_POINT('Origin',(-21.650635094611,-27.5,31.));
#46209=CARTESIAN_POINT('Origin',(34.6410161513775,-5.,19.));
#46210=CARTESIAN_POINT('',(39.5897327444315,-5.71428571428572,19.));
#46211=CARTESIAN_POINT('Origin',(34.6410161513775,-5.,19.));
#46212=CARTESIAN_POINT('',(39.5897327444315,-5.71428571428572,19.));
#46213=CARTESIAN_POINT('Origin',(0.,0.,19.));
#46214=CARTESIAN_POINT('',(39.5897327444315,5.71428571428572,19.));
#46215=CARTESIAN_POINT('Origin',(0.,0.,19.));
#46216=CARTESIAN_POINT('',(39.5897327444315,5.71428571428572,19.));
#46217=CARTESIAN_POINT('Origin',(34.6410161513775,5.,19.));
#46218=CARTESIAN_POINT('',(34.6410161513775,10.,19.));
#46219=CARTESIAN_POINT('Origin',(34.6410161513775,5.,19.));
#46220=CARTESIAN_POINT('',(34.6410161513775,10.,19.));
#46221=CARTESIAN_POINT('Origin',(-12.9903810567666,32.5,19.));
#46222=CARTESIAN_POINT('',(-14.8461497791618,37.1428571428571,19.));
#46223=CARTESIAN_POINT('Origin',(-12.9903810567666,32.5,19.));
#46224=CARTESIAN_POINT('',(-14.8461497791618,37.1428571428571,19.));
#46225=CARTESIAN_POINT('Origin',(-21.650635094611,-27.5,19.));
#46226=CARTESIAN_POINT('Origin',(-21.650635094611,-27.5,19.));
#46227=CARTESIAN_POINT('Origin',(-21.650635094611,27.5,19.));
#46228=CARTESIAN_POINT('',(-24.7435829652697,31.4285714285714,19.));
#46229=CARTESIAN_POINT('',(-24.7435829652697,31.4285714285714,19.));
#46230=CARTESIAN_POINT('',(-25.9807621135332,25.,19.));
#46231=CARTESIAN_POINT('Origin',(-21.650635094611,27.5,19.));
#46232=CARTESIAN_POINT('',(-25.9807621135332,25.,19.));
#46233=CARTESIAN_POINT('Origin',(-28.0251707688815,28.5410196624969,19.));
#46234=CARTESIAN_POINT('',(-28.0251707688815,28.5410196624969,19.));
#46235=CARTESIAN_POINT('Origin',(0.,0.,19.));
#46236=CARTESIAN_POINT('Origin',(0.,0.,19.));
#46237=CARTESIAN_POINT('Origin',(38.7298334620742,10.,19.));
#46238=CARTESIAN_POINT('',(38.7298334620742,10.,19.));
#46239=CARTESIAN_POINT('Origin',(-10.7046626931927,-38.5410196624968,19.));
#46240=CARTESIAN_POINT('',(-10.7046626931927,-38.5410196624968,19.));
#46241=CARTESIAN_POINT('Origin',(5.98741461555926,0.,19.));
#46242=CARTESIAN_POINT('',(0.,0.,0.));
#46243=CARTESIAN_POINT('Origin',(30.,-1.32966554433622E-14,16.));
#46244=CARTESIAN_POINT('',(29.9999999999999,-1.50000000000001,30.25));
#46245=CARTESIAN_POINT('',(30.,-1.50000000000001,30.3125));
#46246=CARTESIAN_POINT('',(30.,-1.50000000000001,16.));
#46247=CARTESIAN_POINT('',(30.,-1.50000000000002,30.75));
#46248=CARTESIAN_POINT('Ctrl Pts',(29.9999999999999,-1.50000000000001,30.25));
#46249=CARTESIAN_POINT('Ctrl Pts',(30.1658036138247,-1.50000000000003,30.2579772300895));
#46250=CARTESIAN_POINT('Ctrl Pts',(30.3306771390814,-1.47251502213024,30.2666731828795));
#46251=CARTESIAN_POINT('Ctrl Pts',(30.6740051197163,-1.35441705513551,30.2864720571327));
#46252=CARTESIAN_POINT('Ctrl Pts',(30.8456956760641,-1.25440329321601,30.2975106829297));
#46253=CARTESIAN_POINT('Ctrl Pts',(31.1355371924707,-0.998320157723232,
30.31856910982));
#46254=CARTESIAN_POINT('Ctrl Pts',(31.2526807741055,-0.846671576374736,
30.3279626902015));
#46255=CARTESIAN_POINT('Ctrl Pts',(31.4282014939959,-0.499786966349004,
30.3472340574251));
#46256=CARTESIAN_POINT('Ctrl Pts',(31.4817951924464,-0.306278304449559,
30.3579845386417));
#46257=CARTESIAN_POINT('Ctrl Pts',(31.5101111597472,0.0860175204635018,
30.3797787511369));
#46258=CARTESIAN_POINT('Ctrl Pts',(31.4862462216493,0.280921846793951,30.3906067692664));
#46259=CARTESIAN_POINT('Ctrl Pts',(31.3664146176937,0.647698903970874,30.4109832724428));
#46260=CARTESIAN_POINT('Ctrl Pts',(31.2727727808063,0.816486916731949,30.4197772164968));
#46261=CARTESIAN_POINT('Ctrl Pts',(31.0215777110749,1.11639419547156,30.440193602667));
#46262=CARTESIAN_POINT('Ctrl Pts',(30.8638920671928,1.2424306705166,30.4512812699412));
#46263=CARTESIAN_POINT('Ctrl Pts',(30.51519869364,1.4218077371841,30.4730404839947));
#46264=CARTESIAN_POINT('Ctrl Pts',(30.3288784064271,1.47608428096084,30.4835125047644));
#46265=CARTESIAN_POINT('Ctrl Pts',(29.9417076474062,1.51169090841865,30.5031293395779));
#46266=CARTESIAN_POINT('Ctrl Pts',(29.7444133180912,1.49107258678014,30.5125449036674));
#46267=CARTESIAN_POINT('Ctrl Pts',(29.3680874803138,1.37464650826943,30.5338849467157));
#46268=CARTESIAN_POINT('Ctrl Pts',(29.192868275455,1.27964935682832,30.5449539944024));
#46269=CARTESIAN_POINT('Ctrl Pts',(28.8948089362382,1.03185947909864,30.5661774332058));
#46270=CARTESIAN_POINT('Ctrl Pts',(28.7730426891403,0.883581363472215,30.5759121464738));
#46271=CARTESIAN_POINT('Ctrl Pts',(28.5872420086988,0.541893735862482,30.5948947924521));
#46272=CARTESIAN_POINT('Ctrl Pts',(28.5279457886126,0.350092848014275,30.6055503973326));
#46273=CARTESIAN_POINT('Ctrl Pts',(28.4879441501424,-0.0417086531130522,
30.6273171473952));
#46274=CARTESIAN_POINT('Ctrl Pts',(28.5061747163527,-0.237794814766365,
30.6382108230426));
#46275=CARTESIAN_POINT('Ctrl Pts',(28.6154381406337,-0.60772707143957,30.65876261508));
#46276=CARTESIAN_POINT('Ctrl Pts',(28.7037802077497,-0.77855877037785,30.6675955620118));
#46277=CARTESIAN_POINT('Ctrl Pts',(28.9458348287961,-1.08578773838532,30.687775558397));
#46278=CARTESIAN_POINT('Ctrl Pts',(29.1002278810903,-1.21679626071423,30.6988429232091));
#46279=CARTESIAN_POINT('Ctrl Pts',(29.3881527190005,-1.37554036843891,30.7171052719799));
#46280=CARTESIAN_POINT('Ctrl Pts',(29.5080276522,-1.42282651307167,30.7241862614101));
#46281=CARTESIAN_POINT('Ctrl Pts',(29.7526687702711,-1.48465507368766,30.7376740227083));
#46282=CARTESIAN_POINT('Ctrl Pts',(29.8761199631302,-1.50000000000009,30.7440398189472));
#46283=CARTESIAN_POINT('Ctrl Pts',(30.0000000000009,-1.50000000000001,30.75));
#46284=CARTESIAN_POINT('',(30.,-1.50000000000001,30.85));
#46285=CARTESIAN_POINT('',(30.,-1.50000000000001,16.));
#46286=CARTESIAN_POINT('Origin',(30.,-1.32966554433622E-14,30.85));
#46287=CARTESIAN_POINT('',(28.9490560961666,-1.07028823734334,30.75));
#46288=CARTESIAN_POINT('Origin',(30.,-1.5916987375435E-14,30.75));
#46289=CARTESIAN_POINT('Ctrl Pts',(28.9490560961666,-1.07028823734332,30.75));
#46290=CARTESIAN_POINT('Ctrl Pts',(28.8761609488349,-0.998710593084209,
30.7445045626927));
#46291=CARTESIAN_POINT('Ctrl Pts',(28.8107674297946,-0.919873442584925,
30.7391683946938));
#46292=CARTESIAN_POINT('Ctrl Pts',(28.6983154051604,-0.752052754529888,
30.7290963583567));
#46293=CARTESIAN_POINT('Ctrl Pts',(28.6511686993163,-0.663795554008335,
30.7243775307781));
#46294=CARTESIAN_POINT('Ctrl Pts',(28.5395598759442,-0.392939439769756,
30.709329968876));
#46295=CARTESIAN_POINT('Ctrl Pts',(28.5011631241701,-0.201888114570883,
30.6987160063649));
#46296=CARTESIAN_POINT('Ctrl Pts',(28.4988436150777,0.191908857459164,30.6768383968077));
#46297=CARTESIAN_POINT('Ctrl Pts',(28.5379718270057,0.390884408078152,30.6657841995511));
#46298=CARTESIAN_POINT('Ctrl Pts',(28.6882496652404,0.752033457565058,30.6457203634686));
#46299=CARTESIAN_POINT('Ctrl Pts',(28.7941652988744,0.912256576314666,30.6368419553212));
#46300=CARTESIAN_POINT('Ctrl Pts',(29.0637866570552,1.18813740110581,30.6162064354332));
#46301=CARTESIAN_POINT('Ctrl Pts',(29.2263162356668,1.29983562680085,30.6052839989448));
#46302=CARTESIAN_POINT('Ctrl Pts',(29.5881540142218,1.45598200117754,30.5835376714189));
#46303=CARTESIAN_POINT('Ctrl Pts',(29.7845106480132,1.49769538170803,30.5729317534561));
#46304=CARTESIAN_POINT('Ctrl Pts',(30.1735918421599,1.5020241460186,30.5540918323215));
#46305=CARTESIAN_POINT('Ctrl Pts',(30.3626153088868,1.46791385953203,30.544162381137));
#46306=CARTESIAN_POINT('Ctrl Pts',(30.7246797057952,1.32812661690519,30.5228595707569));
#46307=CARTESIAN_POINT('Ctrl Pts',(30.8932233177541,1.2211620663456,30.5117792749302));
#46308=CARTESIAN_POINT('Ctrl Pts',(31.1776737025205,0.949411483501645,30.4905450221109));
#46309=CARTESIAN_POINT('Ctrl Pts',(31.2913339229655,0.787872571372875,30.4812706984095));
#46310=CARTESIAN_POINT('Ctrl Pts',(31.4489779041399,0.433069950768308,30.4615594417092));
#46311=CARTESIAN_POINT('Ctrl Pts',(31.4925441992832,0.243681023738972,30.451037834652));
#46312=CARTESIAN_POINT('Ctrl Pts',(31.5059639907605,-0.148777135728896,
30.4292346035705));
#46313=CARTESIAN_POINT('Ctrl Pts',(31.4726973264507,-0.348194823891665,
30.418155843117));
#46314=CARTESIAN_POINT('Ctrl Pts',(31.3331360295961,-0.713588890875335,
30.3978561727291));
#46315=CARTESIAN_POINT('Ctrl Pts',(31.2315888806866,-0.877298264710928,
30.3890521180742));
#46316=CARTESIAN_POINT('Ctrl Pts',(30.969887909143,-1.16071911064266,30.3685882229343));
#46317=CARTESIAN_POINT('Ctrl Pts',(30.8111118646049,-1.27673016594729,30.3577265776157));
#46318=CARTESIAN_POINT('Ctrl Pts',(30.4544959445291,-1.44324278722566,30.3359435355702));
#46319=CARTESIAN_POINT('Ctrl Pts',(30.2594138454525,-1.49071962728781,30.3252388425894));
#46320=CARTESIAN_POINT('Ctrl Pts',(30.0404799678322,-1.49959063127059,30.3144589647139));
#46321=CARTESIAN_POINT('Ctrl Pts',(30.0202329450965,-1.50000000000001,30.3134734580248));
#46322=CARTESIAN_POINT('Ctrl Pts',(30.,-1.50000000000001,30.3125));
#46323=CARTESIAN_POINT('Origin',(30.,-1.32966554433622E-14,16.));
#46324=CARTESIAN_POINT('',(30.0000000422953,-1.50000000000001,29.7500000040699));
#46325=CARTESIAN_POINT('',(30.0000000000001,-1.50000000000001,29.8125));
#46326=CARTESIAN_POINT('',(30.,-1.50000000000001,16.));
#46327=CARTESIAN_POINT('Ctrl Pts',(30.0000000423936,-1.50000000000001,29.7500000020397));
#46328=CARTESIAN_POINT('Ctrl Pts',(30.195284159332,-1.49999999448081,29.7593956136499));
#46329=CARTESIAN_POINT('Ctrl Pts',(30.3888046451199,-1.46186371850976,29.7697657133627));
#46330=CARTESIAN_POINT('Ctrl Pts',(30.7506676874449,-1.3133124636612,29.7913022808498));
#46331=CARTESIAN_POINT('Ctrl Pts',(30.9154176613495,-1.20428706546983,29.8022573009481));
#46332=CARTESIAN_POINT('Ctrl Pts',(31.18981388205,-0.933008136594988,29.8229947210741));
#46333=CARTESIAN_POINT('Ctrl Pts',(31.2983679232815,-0.774850228387389,
29.8319527650896));
#46334=CARTESIAN_POINT('Ctrl Pts',(31.4541476549185,-0.418353419581691,
29.8517581433566));
#46335=CARTESIAN_POINT('Ctrl Pts',(31.4967395542031,-0.22207441884915,29.8626625322862));
#46336=CARTESIAN_POINT('Ctrl Pts',(31.5028167108854,0.170195075492689,29.8844552819718));
#46337=CARTESIAN_POINT('Ctrl Pts',(31.4683656451658,0.362410265994727,29.8951339036664));
#46338=CARTESIAN_POINT('Ctrl Pts',(31.3284167977355,0.722950513431523,29.9151639174129));
#46339=CARTESIAN_POINT('Ctrl Pts',(31.2243440361084,0.887881539566768,29.9240904295301));
#46340=CARTESIAN_POINT('Ctrl Pts',(30.9555499935672,1.17320843290826,29.9449485359688));
#46341=CARTESIAN_POINT('Ctrl Pts',(30.7918896841479,1.28933944326239,29.9560485076758));
#46342=CARTESIAN_POINT('Ctrl Pts',(30.4356884609645,1.44801470954154,29.9775938933022));
#46343=CARTESIAN_POINT('Ctrl Pts',(30.24769400318,1.49172420709908,29.9878529335795));
#46344=CARTESIAN_POINT('Ctrl Pts',(29.8564383086953,1.50648133745832,30.007087152245));
#46345=CARTESIAN_POINT('Ctrl Pts',(29.6568006042803,1.4738887523207,30.0172375010609));
#46346=CARTESIAN_POINT('Ctrl Pts',(29.2858871639067,1.33362042993594,30.0389794245699));
#46347=CARTESIAN_POINT('Ctrl Pts',(29.1177424716204,1.22887149382963,30.049978982519));
#46348=CARTESIAN_POINT('Ctrl Pts',(28.8358984689122,0.964859074366596,30.0708728867402));
#46349=CARTESIAN_POINT('Ctrl Pts',(28.7232154667205,0.809870978335536,30.0800071678703));
#46350=CARTESIAN_POINT('Ctrl Pts',(28.5578456280088,0.457982195266601,30.0995565447074));
#46351=CARTESIAN_POINT('Ctrl Pts',(28.5099042682065,0.262965364708001,30.1103908130718));
#46352=CARTESIAN_POINT('Ctrl Pts',(28.4930631778567,-0.129475272168894,
30.1321930706761));
#46353=CARTESIAN_POINT('Ctrl Pts',(28.5224126203679,-0.323064053208287,
30.142948002956));
#46354=CARTESIAN_POINT('Ctrl Pts',(28.6526173206986,-0.686662322858743,
30.1631479068255));
#46355=CARTESIAN_POINT('Ctrl Pts',(28.7515795011674,-0.85345907766542,30.1719758706799));
#46356=CARTESIAN_POINT('Ctrl Pts',(29.0118186458561,-1.14595641051804,30.1926215582791));
#46357=CARTESIAN_POINT('Ctrl Pts',(29.172636650331,-1.26695599442051,30.2037200176798));
#46358=CARTESIAN_POINT('Ctrl Pts',(29.5253217759949,-1.43577307549295,30.2253779520631));
#46359=CARTESIAN_POINT('Ctrl Pts',(29.7125728326969,-1.48464476779679,30.2357446197376));
#46360=CARTESIAN_POINT('Ctrl Pts',(29.9359811243456,-1.49897644179293,30.2468914582366));
#46361=CARTESIAN_POINT('Ctrl Pts',(29.9680065223165,-1.50000000000001,30.2484607130873));
#46362=CARTESIAN_POINT('Ctrl Pts',(29.9999999999999,-1.50000000000001,30.25));
#46363=CARTESIAN_POINT('Ctrl Pts',(30.,-1.50000000000001,30.3125));
#46364=CARTESIAN_POINT('Ctrl Pts',(29.8305649734084,-1.50000000000001,30.3043480534823));
#46365=CARTESIAN_POINT('Ctrl Pts',(29.6621927434306,-1.471296371185,30.2954499177677));
#46366=CARTESIAN_POINT('Ctrl Pts',(29.3161242189391,-1.34950305066004,30.2754165403276));
#46367=CARTESIAN_POINT('Ctrl Pts',(29.1449154106261,-1.2480688680691,30.264361636514));
#46368=CARTESIAN_POINT('Ctrl Pts',(28.8512754656375,-0.984586302069753,
30.242914917907));
#46369=CARTESIAN_POINT('Ctrl Pts',(28.7318299827785,-0.825047829175388,
30.2333359905097));
#46370=CARTESIAN_POINT('Ctrl Pts',(28.5638630976012,-0.47370253085421,30.2138168072696));
#46371=CARTESIAN_POINT('Ctrl Pts',(28.5150825240157,-0.286153024679847,
30.2033973902599));
#46372=CARTESIAN_POINT('Ctrl Pts',(28.4904050702493,0.104624550291977,30.1816875249837));
#46373=CARTESIAN_POINT('Ctrl Pts',(28.5176966903753,0.304322584656878,30.1705931897412));
#46374=CARTESIAN_POINT('Ctrl Pts',(28.6462704703314,0.673930577459572,30.1500594123633));
#46375=CARTESIAN_POINT('Ctrl Pts',(28.7433931121189,0.841252262459088,30.141257075347));
#46376=CARTESIAN_POINT('Ctrl Pts',(28.9970706151381,1.13219704351489,30.1209702113185));
#46377=CARTESIAN_POINT('Ctrl Pts',(29.1519620886259,1.25242080149054,30.1101784429931));
#46378=CARTESIAN_POINT('Ctrl Pts',(29.5030294160994,1.42917820121841,30.0883777805545));
#46379=CARTESIAN_POINT('Ctrl Pts',(29.696654967539,1.48240812812318,30.0775833577866));
#46380=CARTESIAN_POINT('Ctrl Pts',(30.0844620336651,1.50960977413546,30.0581693803401));
#46381=CARTESIAN_POINT('Ctrl Pts',(30.2746950762916,1.48681483093204,30.0489174722834));
#46382=CARTESIAN_POINT('Ctrl Pts',(30.642872277816,1.3694262764412,30.0279427452356));
#46383=CARTESIAN_POINT('Ctrl Pts',(30.8165454300566,1.27352463490858,30.0169229573155));
#46384=CARTESIAN_POINT('Ctrl Pts',(31.1192034235311,1.01839257572982,29.9952743161713));
#46385=CARTESIAN_POINT('Ctrl Pts',(31.2444516003803,0.860842115189833,29.9853245619549));
#46386=CARTESIAN_POINT('Ctrl Pts',(31.4225185229473,0.51295924874081,29.9659977360411));
#46387=CARTESIAN_POINT('Ctrl Pts',(31.476317491186,0.327339595503408,29.9556855330835));
#46388=CARTESIAN_POINT('Ctrl Pts',(31.5118899575654,-0.0614966036299657,
29.9340835220205));
#46389=CARTESIAN_POINT('Ctrl Pts',(31.49041063713,-0.261302093346022,29.9229832170363));
#46390=CARTESIAN_POINT('Ctrl Pts',(31.3726040951777,-0.63490434793495,29.9022275362258));
#46391=CARTESIAN_POINT('Ctrl Pts',(31.2797800327084,-0.805795593106099,
29.8933569012793));
#46392=CARTESIAN_POINT('Ctrl Pts',(31.0338687856651,-1.10392432463312,29.873244137236));
#46393=CARTESIAN_POINT('Ctrl Pts',(30.8828092373533,-1.22807490132932,29.8625276541988));
#46394=CARTESIAN_POINT('Ctrl Pts',(30.5373473005298,-1.41449618106684,29.8407282401322));
#46395=CARTESIAN_POINT('Ctrl Pts',(30.3452845785499,-1.47320733373471,29.8298567527606));
#46396=CARTESIAN_POINT('Ctrl Pts',(30.0982962322989,-1.49758712755237,29.8172963039161));
#46397=CARTESIAN_POINT('Ctrl Pts',(30.0491225084885,-1.50000000000001,29.8148634077916));
#46398=CARTESIAN_POINT('Ctrl Pts',(30.0000000000002,-1.50000000000001,29.8125));
#46399=CARTESIAN_POINT('Origin',(30.,-1.32966554433622E-14,16.));
#46400=CARTESIAN_POINT('',(30.,-1.50000000000001,29.25));
#46401=CARTESIAN_POINT('',(30.,-1.50000000000001,29.3125));
#46402=CARTESIAN_POINT('',(30.,-1.50000000000001,16.));
#46403=CARTESIAN_POINT('Ctrl Pts',(30.0000000000001,-1.50000000000001,29.25));
#46404=CARTESIAN_POINT('Ctrl Pts',(30.0257058009192,-1.50000000000001,29.2512367709234));
#46405=CARTESIAN_POINT('Ctrl Pts',(30.0514327409082,-1.49933922123128,29.2524929138666));
#46406=CARTESIAN_POINT('Ctrl Pts',(30.2757518694164,-1.4877855903611,29.2636064071598));
#46407=CARTESIAN_POINT('Ctrl Pts',(30.4703136581261,-1.43816783024051,29.2743455366981));
#46408=CARTESIAN_POINT('Ctrl Pts',(30.8249043497727,-1.26783071251083,29.2961373759079));
#46409=CARTESIAN_POINT('Ctrl Pts',(30.9822510518058,-1.15024113589767,29.3069740997672));
#46410=CARTESIAN_POINT('Ctrl Pts',(31.2409808029183,-0.864020908483806,
29.3273728025942));
#46411=CARTESIAN_POINT('Ctrl Pts',(31.3408899715229,-0.698983488656709,
29.3361675839636));
#46412=CARTESIAN_POINT('Ctrl Pts',(31.4763980403227,-0.332018378933428,
29.3565545345038));
#46413=CARTESIAN_POINT('Ctrl Pts',(31.5074559153656,-0.132477013527386,
29.3676401659153));
#46414=CARTESIAN_POINT('Ctrl Pts',(31.4898677318573,0.259397054955175,29.3894109474976));
#46415=CARTESIAN_POINT('Ctrl Pts',(31.444367356687,0.448123046557066,29.3998957248088));
#46416=CARTESIAN_POINT('Ctrl Pts',(31.2829132867175,0.801659109129801,29.419536617174));
#46417=CARTESIAN_POINT('Ctrl Pts',(31.1671346623852,0.962462537199801,29.4289146111855));
#46418=CARTESIAN_POINT('Ctrl Pts',(30.8792964511142,1.23119218867364,29.4502279461232));
#46419=CARTESIAN_POINT('Ctrl Pts',(30.7097525390342,1.33613064071083,29.4613000883974));
#46420=CARTESIAN_POINT('Ctrl Pts',(30.346523773562,1.47177468007876,29.4825438305068));
#46421=CARTESIAN_POINT('Ctrl Pts',(30.1572989096959,1.50379960302192,29.4923264081504));
#46422=CARTESIAN_POINT('Ctrl Pts',(29.7684168962525,1.49529312487305,29.5112727938055));
#46423=CARTESIAN_POINT('Ctrl Pts',(29.5725063077327,1.45146676708809,29.5219159452176));
#46424=CARTESIAN_POINT('Ctrl Pts',(29.2125442219205,1.29150806105852,29.5436779265358));
#46425=CARTESIAN_POINT('Ctrl Pts',(29.051374885103,1.17821798386326,29.5545791364576));
#46426=CARTESIAN_POINT('Ctrl Pts',(28.784644635234,0.899571593555892,29.5751523790963));
#46427=CARTESIAN_POINT('Ctrl Pts',(28.6803243600253,0.738084850822973,29.5839952860653));
#46428=CARTESIAN_POINT('Ctrl Pts',(28.5339435846744,0.375376943196454,29.6041457253779));
#46429=CARTESIAN_POINT('Ctrl Pts',(28.4969501646145,0.176221200716502,29.6152099332935));
#46430=CARTESIAN_POINT('Ctrl Pts',(28.5033188891713,-0.217123692718195,
29.6370624273732));
#46431=CARTESIAN_POINT('Ctrl Pts',(28.5436046203998,-0.407585858885439,
29.6476436588269));
#46432=CARTESIAN_POINT('Ctrl Pts',(28.6948329707667,-0.764496194056087,
29.6674720107808));
#46433=CARTESIAN_POINT('Ctrl Pts',(28.8049699824855,-0.927268122072015,
29.6765948726435));
#46434=CARTESIAN_POINT('Ctrl Pts',(29.0837280295094,-1.20402609540407,29.6976943469156));
#46435=CARTESIAN_POINT('Ctrl Pts',(29.2505451199729,-1.31436112105669,29.7087851997463));
#46436=CARTESIAN_POINT('Ctrl Pts',(29.6105129505334,-1.46104267840857,29.7301786477734));
#46437=CARTESIAN_POINT('Ctrl Pts',(29.799201008928,-1.49868271487424,29.7403024627842));
#46438=CARTESIAN_POINT('Ctrl Pts',(29.9932712661576,-1.49998868274459,29.7496759492739));
#46439=CARTESIAN_POINT('Ctrl Pts',(29.9966359009771,-1.50000000009509,29.7498381447076));
#46440=CARTESIAN_POINT('Ctrl Pts',(30.0000000423936,-1.50000000000001,29.7500000020397));
#46441=CARTESIAN_POINT('Ctrl Pts',(30.0000000000002,-1.50000000000001,29.8125));
#46442=CARTESIAN_POINT('Ctrl Pts',(29.8597537134085,-1.50000000000001,29.8057523973903));
#46443=CARTESIAN_POINT('Ctrl Pts',(29.7199776172616,-1.48033650865739,29.798481208736));
#46444=CARTESIAN_POINT('Ctrl Pts',(29.396444095828,-1.38712528602054,29.7803259942996));
#46445=CARTESIAN_POINT('Ctrl Pts',(29.2206000446906,-1.29650603057681,29.7693484919046));
#46446=CARTESIAN_POINT('Ctrl Pts',(28.911420128637,-1.05097346611518,29.747652717245));
#46447=CARTESIAN_POINT('Ctrl Pts',(28.7818724475201,-0.897590413872414,
29.737366134104));
#46448=CARTESIAN_POINT('Ctrl Pts',(28.5939020851709,-0.556198210295242,
29.7183999005719));
#46449=CARTESIAN_POINT('Ctrl Pts',(28.5345980064858,-0.372882477899534,
29.7082156932166));
#46450=CARTESIAN_POINT('Ctrl Pts',(28.4870031451474,0.0134445146485481,
29.6867530825195));
#46451=CARTESIAN_POINT('Ctrl Pts',(28.502033993864,0.213177772539474,29.6756567904145));
#46452=CARTESIAN_POINT('Ctrl Pts',(28.6077791980133,0.591085049341038,29.6546619417033));
#46453=CARTESIAN_POINT('Ctrl Pts',(28.6958240597398,0.766015662165753,29.6456356480104));
#46454=CARTESIAN_POINT('Ctrl Pts',(28.9331445661562,1.07197536298372,29.6257186792435));
#46455=CARTESIAN_POINT('Ctrl Pts',(29.079894739921,1.20029258347643,29.6150937909803));
#46456=CARTESIAN_POINT('Ctrl Pts',(29.4205899711736,1.39807482372058,29.5932081329061));
#46457=CARTESIAN_POINT('Ctrl Pts',(29.6127784235583,1.46301280498413,29.5821576288666));
#46458=CARTESIAN_POINT('Ctrl Pts',(30.000882127086,1.51202551870596,29.5621235164545));
#46459=CARTESIAN_POINT('Ctrl Pts',(30.1924980276144,1.49972435337029,29.5532307774773));
#46460=CARTESIAN_POINT('Ctrl Pts',(30.565900986819,1.40283604422102,29.5325740773055));
#46461=CARTESIAN_POINT('Ctrl Pts',(30.7436552900603,1.31725598082702,29.5216446454201));
#46462=CARTESIAN_POINT('Ctrl Pts',(31.0589827795059,1.08076551025951,29.4999042647726));
#46463=CARTESIAN_POINT('Ctrl Pts',(31.1927323157941,0.931082658468895,29.4893113802134));
#46464=CARTESIAN_POINT('Ctrl Pts',(31.3898152208091,0.595521362119493,29.470508077404));
#46465=CARTESIAN_POINT('Ctrl Pts',(31.454132752542,0.414466978649508,29.4605259432583));
#46466=CARTESIAN_POINT('Ctrl Pts',(31.5126702779257,0.0306540870738048,
29.4392030048374));
#46467=CARTESIAN_POINT('Ctrl Pts',(31.5035323460368,-0.168835937693657,
29.4281202256837));
#46468=CARTESIAN_POINT('Ctrl Pts',(31.4089367798935,-0.550558804938134,
29.4069133997257));
#46469=CARTESIAN_POINT('Ctrl Pts',(31.3252882833553,-0.729258932876967,
29.3976724363492));
#46470=CARTESIAN_POINT('Ctrl Pts',(31.095809753143,-1.04226364925314,29.3779370699617));
#46471=CARTESIAN_POINT('Ctrl Pts',(30.9530486497371,-1.17422022183269,29.3674030128222));
#46472=CARTESIAN_POINT('Ctrl Pts',(30.6189939852,-1.38091973480463,29.3455891471428));
#46473=CARTESIAN_POINT('Ctrl Pts',(30.429320489981,-1.45113472826307,29.3345130603643));
#46474=CARTESIAN_POINT('Ctrl Pts',(30.1547092959792,-1.49402062264703,29.3201095482887));
#46475=CARTESIAN_POINT('Ctrl Pts',(30.0773321028638,-1.50000000000001,29.3162206425338));
#46476=CARTESIAN_POINT('Ctrl Pts',(30.,-1.50000000000001,29.3125));
#46477=CARTESIAN_POINT('Origin',(30.,-1.32966554433622E-14,16.));
#46478=CARTESIAN_POINT('',(30.0000000000001,-1.50000000000001,28.75));
#46479=CARTESIAN_POINT('',(30.,-1.50000000000001,28.8125));
#46480=CARTESIAN_POINT('',(30.,-1.50000000000001,16.));
#46481=CARTESIAN_POINT('Ctrl Pts',(30.0000000000002,-1.50000000000001,28.75));
#46482=CARTESIAN_POINT('Ctrl Pts',(30.0540853804301,-1.50000000000001,28.7526021840792));
#46483=CARTESIAN_POINT('Ctrl Pts',(30.1082259230801,-1.49707499170992,28.7552882723823));
#46484=CARTESIAN_POINT('Ctrl Pts',(30.3599293953789,-1.46969892581938,28.7681588076143));
#46485=CARTESIAN_POINT('Ctrl Pts',(30.551406195325,-1.40907643365525,28.7790551975627));
#46486=CARTESIAN_POINT('Ctrl Pts',(30.8948389562126,-1.21930777033508,28.8008499657338));
#46487=CARTESIAN_POINT('Ctrl Pts',(31.0445316684251,-1.09380802186036,28.8115381638324));
#46488=CARTESIAN_POINT('Ctrl Pts',(31.2877030940359,-0.793168713090864,
28.8315888464123));
#46489=CARTESIAN_POINT('Ctrl Pts',(31.379006293082,-0.620999590881335,28.8405000227289));
#46490=CARTESIAN_POINT('Ctrl Pts',(31.4929834420294,-0.246010850263539,
28.861332730541));
#46491=CARTESIAN_POINT('Ctrl Pts',(31.5124077516471,-0.0462064671363202,
28.872432974048));
#46492=CARTESIAN_POINT('Ctrl Pts',(31.472996504913,0.34187077296362,28.8939928207202));
#46493=CARTESIAN_POINT('Ctrl Pts',(31.4174359900152,0.526774847879437,28.9042652693267));
#46494=CARTESIAN_POINT('Ctrl Pts',(31.2357811865968,0.873408443354475,28.9235226912975));
#46495=CARTESIAN_POINT('Ctrl Pts',(31.1084372252019,1.03024288184359,28.9336214802999));
#46496=CARTESIAN_POINT('Ctrl Pts',(30.8025714917792,1.28234443647017,28.9553402732223));
#46497=CARTESIAN_POINT('Ctrl Pts',(30.6280587815183,1.37625325113107,28.9663450980946));
#46498=CARTESIAN_POINT('Ctrl Pts',(30.2588396849677,1.48965870484553,28.9872593116519));
#46499=CARTESIAN_POINT('Ctrl Pts',(30.068359262301,1.51042753130005,28.996421409812));
#46500=CARTESIAN_POINT('Ctrl Pts',(29.6808324457,1.4790834395187,29.015936971685));
#46501=CARTESIAN_POINT('Ctrl Pts',(29.4877765738488,1.42378431516532,29.0267614634377));
#46502=CARTESIAN_POINT('Ctrl Pts',(29.1387883585853,1.24336756773843,29.0485637430906));
#46503=CARTESIAN_POINT('Ctrl Pts',(28.9853282851658,1.12165139698337,29.0593280990587));
#46504=CARTESIAN_POINT('Ctrl Pts',(28.7345675292747,0.827996981331758,29.0795498986531));
#46505=CARTESIAN_POINT('Ctrl Pts',(28.6390572969471,0.659343561113025,29.0883698021604));
#46506=CARTESIAN_POINT('Ctrl Pts',(28.5145121329283,0.288224890453508,29.108987506086));
#46507=CARTESIAN_POINT('Ctrl Pts',(28.4894007489509,0.0884674237606763,
29.1200851431244));
#46508=CARTESIAN_POINT('Ctrl Pts',(28.5181714945435,-0.301617414497863,
29.1417565230277));
#46509=CARTESIAN_POINT('Ctrl Pts',(28.5688407456957,-0.488459284239858,
29.1521366269022));
#46510=CARTESIAN_POINT('Ctrl Pts',(28.7405885892344,-0.838517734954907,
29.1715843186086));
#46511=CARTESIAN_POINT('Ctrl Pts',(28.8621896492638,-0.99731625641509,29.1812936366545));
#46512=CARTESIAN_POINT('Ctrl Pts',(29.1592029920166,-1.25770358504828,29.2028166791214));
#46513=CARTESIAN_POINT('Ctrl Pts',(29.3313514615525,-1.35708034159287,29.2138596416832));
#46514=CARTESIAN_POINT('Ctrl Pts',(29.6732716198879,-1.47316539526991,29.2335348677957));
#46515=CARTESIAN_POINT('Ctrl Pts',(29.836171069295,-1.50000000000001,29.2421177768964));
#46516=CARTESIAN_POINT('Ctrl Pts',(30.0000000000001,-1.50000000000001,29.25));
#46517=CARTESIAN_POINT('Ctrl Pts',(30.,-1.50000000000001,29.3125));
#46518=CARTESIAN_POINT('Ctrl Pts',(29.8873008443269,-1.50000000000001,29.3070777593446));
#46519=CARTESIAN_POINT('Ctrl Pts',(29.7747317592542,-1.48730209620256,29.3013090571639));
#46520=CARTESIAN_POINT('Ctrl Pts',(29.4744632015876,-1.41837586794508,29.2849477619958));
#46521=CARTESIAN_POINT('Ctrl Pts',(29.294837753903,-1.33817655775596,29.2740777699983));
#46522=CARTESIAN_POINT('Ctrl Pts',(28.9731315511867,-1.11133054751215,29.2522983950411));
#46523=CARTESIAN_POINT('Ctrl Pts',(28.8350302040853,-0.965600487241644,
29.241605933651));
#46524=CARTESIAN_POINT('Ctrl Pts',(28.6283822605559,-0.636211572057215,
29.2225138877439));
#46525=CARTESIAN_POINT('Ctrl Pts',(28.5588803689078,-0.457503373167084,
29.2129168540649));
#46526=CARTESIAN_POINT('Ctrl Pts',(28.4890373687744,-0.0765943370343735,
29.1917552409464));
#46527=CARTESIAN_POINT('Ctrl Pts',(28.4920613555339,0.122462822378066,29.1806965098678));
#46528=CARTESIAN_POINT('Ctrl Pts',(28.5749385187676,0.508021327520356,29.1592765929154));
#46529=CARTESIAN_POINT('Ctrl Pts',(28.6539760022703,0.690715131611738,29.1497407450183));
#46530=CARTESIAN_POINT('Ctrl Pts',(28.8753117279029,1.01093295253508,29.1301967854836));
#46531=CARTESIAN_POINT('Ctrl Pts',(29.0138845897616,1.14650161502305,29.1197638993787));
#46532=CARTESIAN_POINT('Ctrl Pts',(29.3408853293963,1.36213850199283,29.0980411554306));
#46533=CARTESIAN_POINT('Ctrl Pts',(29.5278326261113,1.43768005817386,29.0869482728631));
#46534=CARTESIAN_POINT('Ctrl Pts',(29.9124519842907,1.50965487695232,29.0664439648431));
#46535=CARTESIAN_POINT('Ctrl Pts',(30.1057978761999,1.50848592114141,29.0576455173396));
#46536=CARTESIAN_POINT('Ctrl Pts',(30.4842893221004,1.43290905070853,29.0373359816462));
#46537=CARTESIAN_POINT('Ctrl Pts',(30.6656448486515,1.3581864320247,29.02653488151));
#46538=CARTESIAN_POINT('Ctrl Pts',(30.9934995933557,1.14126552935963,29.0047353821212));
#46539=CARTESIAN_POINT('Ctrl Pts',(31.1358790692293,0.999664672511309,28.9939517892597));
#46540=CARTESIAN_POINT('Ctrl Pts',(31.3521306759684,0.67660748989115,28.974573568351));
#46541=CARTESIAN_POINT('Ctrl Pts',(31.426848104494,0.500181082019829,28.9652878378899));
#46542=CARTESIAN_POINT('Ctrl Pts',(31.5078778462889,0.122255781263764,28.9442919878479));
#46543=CARTESIAN_POINT('Ctrl Pts',(31.5109056485428,-0.0761896933508503,
28.9332672392582));
#46544=CARTESIAN_POINT('Ctrl Pts',(31.4398008862795,-0.46541654048851,28.9116435255283));
#46545=CARTESIAN_POINT('Ctrl Pts',(31.3653977766762,-0.65214948337147,28.9017441343992));
#46546=CARTESIAN_POINT('Ctrl Pts',(31.1521444486118,-0.979425287841449,
28.8823929843003));
#46547=CARTESIAN_POINT('Ctrl Pts',(31.0177656624447,-1.1184106596764,28.8720669771632));
#46548=CARTESIAN_POINT('Ctrl Pts',(30.6979072153004,-1.34258973369453,28.8504505839492));
#46549=CARTESIAN_POINT('Ctrl Pts',(30.5137720633169,-1.42326028628083,28.8393505286358));
#46550=CARTESIAN_POINT('Ctrl Pts',(30.2141280739392,-1.48853135114915,28.8231208153399));
#46551=CARTESIAN_POINT('Ctrl Pts',(30.107104215103,-1.50000000000001,28.8176530539518));
#46552=CARTESIAN_POINT('Ctrl Pts',(30.,-1.50000000000001,28.8125));
#46553=CARTESIAN_POINT('Origin',(30.,-1.32966554433622E-14,16.));
#46554=CARTESIAN_POINT('',(30.,-1.50000000000001,28.25));
#46555=CARTESIAN_POINT('',(29.9999999999999,-1.50000000000001,28.3125));
#46556=CARTESIAN_POINT('',(30.,-1.50000000000001,16.));
#46557=CARTESIAN_POINT('Ctrl Pts',(30.,-1.50000000000001,28.25));
#46558=CARTESIAN_POINT('Ctrl Pts',(30.0829658981124,-1.50000000000001,28.2539916986341));
#46559=CARTESIAN_POINT('Ctrl Pts',(30.1659646402018,-1.49311778203419,28.258176150196));
#46560=CARTESIAN_POINT('Ctrl Pts',(30.4454386189069,-1.44623695759697,28.272924593389));
#46561=CARTESIAN_POINT('Ctrl Pts',(30.6341065114148,-1.37401296366571,28.2840081036532));
#46562=CARTESIAN_POINT('Ctrl Pts',(30.9655430066945,-1.16393488515826,28.305789851648));
#46563=CARTESIAN_POINT('Ctrl Pts',(31.1067439460802,-1.03060853555517,28.3162868947229));
#46564=CARTESIAN_POINT('Ctrl Pts',(31.3331794991128,-0.714896180931114,
28.3359510679762));
#46565=CARTESIAN_POINT('Ctrl Pts',(31.4151109522262,-0.5347128589249,28.3452937300598));
#46566=CARTESIAN_POINT('Ctrl Pts',(31.5053441166005,-0.151540941191815,
28.3665810588227));
#46567=CARTESIAN_POINT('Ctrl Pts',(31.5121960357138,0.047808853319833,28.3776560474067));
#46568=CARTESIAN_POINT('Ctrl Pts',(31.4494295470438,0.430548940590616,28.3989193855884));
#46569=CARTESIAN_POINT('Ctrl Pts',(31.3831821322801,0.610720967506089,28.4087494232854));
#46570=CARTESIAN_POINT('Ctrl Pts',(31.1825379493516,0.943999251999173,28.4276606511623));
#46571=CARTESIAN_POINT('Ctrl Pts',(31.047158086339,1.09222920702457,28.4382916166091));
#46572=CARTESIAN_POINT('Ctrl Pts',(30.7294268326579,1.32515752881874,28.4600486998403));
#46573=CARTESIAN_POINT('Ctrl Pts',(30.550958922042,1.4087432384851,28.4709570664618));
#46574=CARTESIAN_POINT('Ctrl Pts',(30.1765920486677,1.5017020595339,28.4915509905286));
#46575=CARTESIAN_POINT('Ctrl Pts',(29.9846796160604,1.51197023290498,28.5004045958464));
#46576=CARTESIAN_POINT('Ctrl Pts',(29.5971747277955,1.45876321333926,28.5205264062414));
#46577=CARTESIAN_POINT('Ctrl Pts',(29.4058997547266,1.39186434368365,28.5315874296089));
#46578=CARTESIAN_POINT('Ctrl Pts',(29.0676327101079,1.19076140439435,28.5534485031393));
#46579=CARTESIAN_POINT('Ctrl Pts',(28.9223466869136,1.06108495094317,28.5640407038963));
#46580=CARTESIAN_POINT('Ctrl Pts',(28.6879155980949,0.752518131365587,28.5838910754598));
#46581=CARTESIAN_POINT('Ctrl Pts',(28.6014862328755,0.576207606788701,28.5929884662895));
#46582=CARTESIAN_POINT('Ctrl Pts',(28.499833643426,0.196881228217823,28.6140621539879));
#46583=CARTESIAN_POINT('Ctrl Pts',(28.4869739372834,-0.00278217893022192,
28.6251545654961));
#46584=CARTESIAN_POINT('Ctrl Pts',(28.5386011115484,-0.388179803466622,
28.646565544637));
#46585=CARTESIAN_POINT('Ctrl Pts',(28.5997438056181,-0.57068109411198,28.6567045052284));
#46586=CARTESIAN_POINT('Ctrl Pts',(28.7910752661536,-0.909939730661663,
28.6755522072589));
#46587=CARTESIAN_POINT('Ctrl Pts',(28.9221594106395,-1.06198129449833,28.6859751842018));
#46588=CARTESIAN_POINT('Ctrl Pts',(29.2336502066539,-1.30423330232361,28.7076910145522));
#46589=CARTESIAN_POINT('Ctrl Pts',(29.4102115046891,-1.39300789458955,28.7186517848609));
#46590=CARTESIAN_POINT('Ctrl Pts',(29.7297304238973,-1.48169043732429,28.7364880499937));
#46591=CARTESIAN_POINT('Ctrl Pts',(29.8646679236608,-1.50000000000001,28.7434888324413));
#46592=CARTESIAN_POINT('Ctrl Pts',(30.0000000000002,-1.50000000000001,28.75));
#46593=CARTESIAN_POINT('Ctrl Pts',(30.,-1.50000000000001,28.8125));
#46594=CARTESIAN_POINT('Ctrl Pts',(29.915383015882,-1.50000000000001,28.8084288634535));
#46595=CARTESIAN_POINT('Ctrl Pts',(29.8307352254749,-1.4928411598692,28.8041573880682));
#46596=CARTESIAN_POINT('Ctrl Pts',(29.5559284168413,-1.44580747389306,28.7896292480462));
#46597=CARTESIAN_POINT('Ctrl Pts',(29.3730572440495,-1.37640415455312,28.7789029846613));
#46598=CARTESIAN_POINT('Ctrl Pts',(29.0395563050654,-1.16922544646275,28.7571024491396));
#46599=CARTESIAN_POINT('Ctrl Pts',(28.8931654598463,-1.03173520870096,28.7462400430439));
#46600=CARTESIAN_POINT('Ctrl Pts',(28.6676984257239,-0.714888535897263,
28.7265909588401));
#46601=CARTESIAN_POINT('Ctrl Pts',(28.5879546245725,-0.540586509645268,
28.7175325838691));
#46602=CARTESIAN_POINT('Ctrl Pts',(28.4963360655409,-0.165582907317607,
28.6966990504065));
#46603=CARTESIAN_POINT('Ctrl Pts',(28.4875887561367,0.032114568158461,28.6857158573245));
#46604=CARTESIAN_POINT('Ctrl Pts',(28.5470557852483,0.422500942588754,28.6640277254117));
#46605=CARTESIAN_POINT('Ctrl Pts',(28.6157998677826,0.611145026803925,28.6537877758344));
#46606=CARTESIAN_POINT('Ctrl Pts',(28.8187186237447,0.943964110383672,28.6347798680923));
#46607=CARTESIAN_POINT('Ctrl Pts',(28.9483973542157,1.08655537048085,28.6245798289275));
#46608=CARTESIAN_POINT('Ctrl Pts',(29.2601643471919,1.31985362966521,28.6030994252846));
#46609=CARTESIAN_POINT('Ctrl Pts',(29.4410566887989,1.40604402433623,28.5920020608114));
#46610=CARTESIAN_POINT('Ctrl Pts',(29.8214920682634,1.50190823479761,28.5710354603478));
#46611=CARTESIAN_POINT('Ctrl Pts',(30.0168727428654,1.5123834847247,28.5620321954671));
#46612=CARTESIAN_POINT('Ctrl Pts',(30.4002098002625,1.45848214178997,28.5420916231679));
#46613=CARTESIAN_POINT('Ctrl Pts',(30.5845472296663,1.39485738401663,28.531455330078));
#46614=CARTESIAN_POINT('Ctrl Pts',(30.9255768985555,1.19735876148644,28.5095614596354));
#46615=CARTESIAN_POINT('Ctrl Pts',(31.0774615143075,1.06275841541511,28.4985150091509));
#46616=CARTESIAN_POINT('Ctrl Pts',(31.3127681711381,0.750226996476014,28.4785123840417));
#46617=CARTESIAN_POINT('Ctrl Pts',(31.3972426471779,0.57785906771898,28.4696032815399));
#46618=CARTESIAN_POINT('Ctrl Pts',(31.4986444188222,0.205636520695856,28.4489242511497));
#46619=CARTESIAN_POINT('Ctrl Pts',(31.5126593744967,0.00877624847217685,
28.4379875693595));
#46620=CARTESIAN_POINT('Ctrl Pts',(31.4639817400215,-0.38243148199871,28.4162538065556));
#46621=CARTESIAN_POINT('Ctrl Pts',(31.4004868863224,-0.572852347631721,
28.405674869576));
#46622=CARTESIAN_POINT('Ctrl Pts',(31.2070793636249,-0.910612756316215,
28.3869104024268));
#46623=CARTESIAN_POINT('Ctrl Pts',(31.0818178721223,-1.05640050494828,28.3768711948362));
#46624=CARTESIAN_POINT('Ctrl Pts',(30.7776023551779,-1.29787423387296,28.3555270153716));
#46625=CARTESIAN_POINT('Ctrl Pts',(30.5998203088742,-1.38901510440857,28.3444417818325));
#46626=CARTESIAN_POINT('Ctrl Pts',(30.2759956104928,-1.48090471471267,28.3263092695923));
#46627=CARTESIAN_POINT('Ctrl Pts',(30.1382050521625,-1.50000000000003,28.3191493936725));
#46628=CARTESIAN_POINT('Ctrl Pts',(29.9999999999998,-1.50000000000001,28.3125));
#46629=CARTESIAN_POINT('Origin',(30.,-1.32966554433622E-14,16.));
#46630=CARTESIAN_POINT('',(30.,-1.50000000000001,27.75));
#46631=CARTESIAN_POINT('',(29.9999999999999,-1.50000000000001,27.8125));
#46632=CARTESIAN_POINT('',(30.,-1.50000000000001,16.));
#46633=CARTESIAN_POINT('Ctrl Pts',(30.,-1.50000000000001,27.75));
#46634=CARTESIAN_POINT('Ctrl Pts',(30.1124415068704,-1.50000000000002,27.7554098445216));
#46635=CARTESIAN_POINT('Ctrl Pts',(30.2247618661566,-1.48736003703784,27.7611649704098));
#46636=CARTESIAN_POINT('Ctrl Pts',(30.5287085515254,-1.41774990238772,27.7777222269793));
#46637=CARTESIAN_POINT('Ctrl Pts',(30.7117935692984,-1.3352484713228,27.7888226154224));
#46638=CARTESIAN_POINT('Ctrl Pts',(31.0290158327245,-1.10803593258209,27.810396438097));
#46639=CARTESIAN_POINT('Ctrl Pts',(31.1618575965723,-0.967846133863366,
27.8206819515156));
#46640=CARTESIAN_POINT('Ctrl Pts',(31.3721629460689,-0.6380210664967,27.8399620797878));
#46641=CARTESIAN_POINT('Ctrl Pts',(31.4448593309443,-0.449797513993593,
27.8500112492227));
#46642=CARTESIAN_POINT('Ctrl Pts',(31.5116357099559,-0.0592694964018678,
27.8717072502));
#46643=CARTESIAN_POINT('Ctrl Pts',(31.5064070816201,0.138907825669745,27.8827171014262));
#46644=CARTESIAN_POINT('Ctrl Pts',(31.4213057895144,0.515720730899333,27.9036511517167));
#46645=CARTESIAN_POINT('Ctrl Pts',(31.3446665574137,0.691326301909506,27.9128415418121));
#46646=CARTESIAN_POINT('Ctrl Pts',(31.1248857141117,1.01202109760975,27.9323239413351));
#46647=CARTESIAN_POINT('Ctrl Pts',(30.9809587395189,1.15206471718701,27.9431387316727));
#46648=CARTESIAN_POINT('Ctrl Pts',(30.6509116511972,1.36527940308072,27.964940759777));
#46649=CARTESIAN_POINT('Ctrl Pts',(30.4689587309927,1.43797198007731,27.9757142119819));
#46650=CARTESIAN_POINT('Ctrl Pts',(30.0895559298121,1.50958056680736,27.9959573651739));
#46651=CARTESIAN_POINT('Ctrl Pts',(29.8958570870542,1.50864454830606,28.0047704518936));
#46652=CARTESIAN_POINT('Ctrl Pts',(29.5119529197823,1.43233602869983,28.0253607308535));
#46653=CARTESIAN_POINT('Ctrl Pts',(29.326059536573,1.35483178794297,28.0364574259998));
#46654=CARTESIAN_POINT('Ctrl Pts',(29.0017503691465,1.13591853977073,28.058141681653));
#46655=CARTESIAN_POINT('Ctrl Pts',(28.8647633102306,0.999035130825837,28.0685347915132));
#46656=CARTESIAN_POINT('Ctrl Pts',(28.6464909172802,0.676130375169667,28.0880060034614));
#46657=CARTESIAN_POINT('Ctrl Pts',(28.5692025798653,0.491914163630282,28.097671435354));
#46658=CARTESIAN_POINT('Ctrl Pts',(28.4907708909632,0.10494838810591,28.1191695339942));
#46659=CARTESIAN_POINT('Ctrl Pts',(28.4900432259905,-0.0938982867387415,
28.1302165714856));
#46660=CARTESIAN_POINT('Ctrl Pts',(28.5641302538219,-0.473688030944453,
28.1513160017192));
#46661=CARTESIAN_POINT('Ctrl Pts',(28.6356001259049,-0.65152593371875,28.1607865563875));
#46662=CARTESIAN_POINT('Ctrl Pts',(28.845875335272,-0.978539657712538,28.1799871416705));
#46663=CARTESIAN_POINT('Ctrl Pts',(28.9856037255401,-1.12272886979256,28.1907150828729));
#46664=CARTESIAN_POINT('Ctrl Pts',(29.3096631032409,-1.34585412683097,28.2125043207586));
#46665=CARTESIAN_POINT('Ctrl Pts',(29.4899597666947,-1.42399330666579,28.2233493807965));
#46666=CARTESIAN_POINT('Ctrl Pts',(29.7854687062271,-1.48848755634025,28.2393585682142));
#46667=CARTESIAN_POINT('Ctrl Pts',(29.8926913234913,-1.50000000000001,28.2448371088943));
#46668=CARTESIAN_POINT('Ctrl Pts',(30.,-1.50000000000001,28.25));
#46669=CARTESIAN_POINT('Ctrl Pts',(29.9999999999998,-1.50000000000001,28.3125));
#46670=CARTESIAN_POINT('Ctrl Pts',(29.9436942937174,-1.50000000000001,28.3097909904434));
#46671=CARTESIAN_POINT('Ctrl Pts',(29.8873283119117,-1.49682992210333,28.3069910231599));
#46672=CARTESIAN_POINT('Ctrl Pts',(29.6396724584349,-1.46877643215582,28.2942964117443));
#46673=CARTESIAN_POINT('Ctrl Pts',(29.4541661443778,-1.41038581308707,28.2837492734071));
#46674=CARTESIAN_POINT('Ctrl Pts',(29.1087260311914,-1.22301113475657,28.2619244260365));
#46675=CARTESIAN_POINT('Ctrl Pts',(28.9535330490943,-1.09318251992373,28.250851349792));
#46676=CARTESIAN_POINT('Ctrl Pts',(28.7092889328235,-0.787692454984111,
28.2306143141317));
#46677=CARTESIAN_POINT('Ctrl Pts',(28.6196840987504,-0.61735395437333,28.2217974419096));
#46678=CARTESIAN_POINT('Ctrl Pts',(28.5078809954767,-0.248171981043882,
28.2012873322802));
#46679=CARTESIAN_POINT('Ctrl Pts',(28.4882926923279,-0.0523550997824531,
28.1904086166545));
#46680=CARTESIAN_POINT('Ctrl Pts',(28.5254878247544,0.339597077669009,28.168633495685));
#46681=CARTESIAN_POINT('Ctrl Pts',(28.5834194437059,0.531823926835376,28.1579542262869));
#46682=CARTESIAN_POINT('Ctrl Pts',(28.7667554264755,0.874769226053054,28.1389017096637));
#46683=CARTESIAN_POINT('Ctrl Pts',(28.8874031082008,1.02385470321529,28.129256101159));
#46684=CARTESIAN_POINT('Ctrl Pts',(29.1834814070674,1.27365788399194,28.1080720501192));
#46685=CARTESIAN_POINT('Ctrl Pts',(29.3578610118793,1.36987818467188,28.0970094213409));
#46686=CARTESIAN_POINT('Ctrl Pts',(29.7335617480327,1.48922788034193,28.0756182419206));
#46687=CARTESIAN_POINT('Ctrl Pts',(29.9311376367095,1.51130087803589,28.0661270552772));
#46688=CARTESIAN_POINT('Ctrl Pts',(30.3188296259211,1.47827076732948,28.0465567126743));
#46689=CARTESIAN_POINT('Ctrl Pts',(30.5053902810264,1.4253063260919,28.0361095744917));
#46690=CARTESIAN_POINT('Ctrl Pts',(30.8550820522802,1.24848731142734,28.0143733820065));
#46691=CARTESIAN_POINT('Ctrl Pts',(31.0135429189334,1.12366789185429,28.0032822239058));
#46692=CARTESIAN_POINT('Ctrl Pts',(31.2669421658592,0.825551327222966,27.9828095312695));
#46693=CARTESIAN_POINT('Ctrl Pts',(31.3618736710286,0.657250577679458,27.9740139209821));
#46694=CARTESIAN_POINT('Ctrl Pts',(31.4842407851538,0.291243414392501,27.9536801896884));
#46695=CARTESIAN_POINT('Ctrl Pts',(31.509450941646,0.0966465287303217,27.9428692515961));
#46696=CARTESIAN_POINT('Ctrl Pts',(31.4839402912682,-0.295715862316101,
27.9210713409824));
#46697=CARTESIAN_POINT('Ctrl Pts',(31.4317236332783,-0.489608696036187,
27.9102995168868));
#46698=CARTESIAN_POINT('Ctrl Pts',(31.2586786377253,-0.837725609348495,
27.8909596883695));
#46699=CARTESIAN_POINT('Ctrl Pts',(31.1426320784322,-0.99018742000189,27.8816363720611));
#46700=CARTESIAN_POINT('Ctrl Pts',(30.8547518896528,-1.24822771259633,27.8606179441152));
#46701=CARTESIAN_POINT('Ctrl Pts',(30.683921012954,-1.3494162779034,27.8495880462471));
#46702=CARTESIAN_POINT('Ctrl Pts',(30.3380948295812,-1.47125624803439,27.8295650326271));
#46703=CARTESIAN_POINT('Ctrl Pts',(30.1695563642114,-1.50000000000003,27.8206577843767));
#46704=CARTESIAN_POINT('Ctrl Pts',(29.9999999999999,-1.50000000000001,27.8125));
#46705=CARTESIAN_POINT('Origin',(30.,-1.32966554433622E-14,16.));
#46706=CARTESIAN_POINT('',(29.9999999999999,-1.50000000000001,27.25));
#46707=CARTESIAN_POINT('',(30.0000000001561,-1.50000000000001,27.312500000015));
#46708=CARTESIAN_POINT('',(30.,-1.50000000000001,16.));
#46709=CARTESIAN_POINT('Ctrl Pts',(29.9999999999998,-1.50000000000001,27.25));
#46710=CARTESIAN_POINT('Ctrl Pts',(30.1442714687728,-1.50000000000004,27.2569412642777));
#46711=CARTESIAN_POINT('Ctrl Pts',(30.2880340149987,-1.4791914741294,27.2644360576155));
#46712=CARTESIAN_POINT('Ctrl Pts',(30.6163114314673,-1.38174334274362,27.2829372047179));
#46713=CARTESIAN_POINT('Ctrl Pts',(30.7927900386128,-1.28861749288707,27.2940148648257));
#46714=CARTESIAN_POINT('Ctrl Pts',(31.0938533402203,-1.04389816914467,27.3152975386708));
#46715=CARTESIAN_POINT('Ctrl Pts',(31.2173213404585,-0.896838599044721,
27.3251756333865));
#46716=CARTESIAN_POINT('Ctrl Pts',(31.4068435879888,-0.557063752560209,
27.3440520137467));
#46717=CARTESIAN_POINT('Ctrl Pts',(31.4681965573585,-0.365925712559008,
27.3546707937468));
#46718=CARTESIAN_POINT('Ctrl Pts',(31.5124404667227,0.0256096349450533,
27.376422757497));
#46719=CARTESIAN_POINT('Ctrl Pts',(31.4962677243898,0.222085336897189,27.3873380742721));
#46720=CARTESIAN_POINT('Ctrl Pts',(31.3908461160845,0.593142920619804,27.4079523844789));
#46721=CARTESIAN_POINT('Ctrl Pts',(31.304401721973,0.764723471695272,27.4168175948822));
#46722=CARTESIAN_POINT('Ctrl Pts',(31.0656503667188,1.07455866625052,27.4369110579998));
#46723=CARTESIAN_POINT('Ctrl Pts',(30.9124772117446,1.20733392111332,27.4479688063785));
#46724=CARTESIAN_POINT('Ctrl Pts',(30.5697179509117,1.40095220523075,27.4698381046742));
#46725=CARTESIAN_POINT('Ctrl Pts',(30.3849139570494,1.46256729268532,27.4804410211816));
#46726=CARTESIAN_POINT('Ctrl Pts',(30.0007344874447,1.51254230178002,27.5003130592281));
#46727=CARTESIAN_POINT('Ctrl Pts',(29.8049569216954,1.49991645600797,27.5093863351468));
#46728=CARTESIAN_POINT('Ctrl Pts',(29.4253565109394,1.3996692288739,27.5304345136228));
#46729=CARTESIAN_POINT('Ctrl Pts',(29.245638701995,1.31157237616612,27.5415283255346));
#46730=CARTESIAN_POINT('Ctrl Pts',(28.9367683949736,1.07514318986943,27.562956332507));
#46731=CARTESIAN_POINT('Ctrl Pts',(28.8087599369318,0.93132448347984,27.5731101063824));
#46732=CARTESIAN_POINT('Ctrl Pts',(28.6094708234815,0.596592375009914,27.591996522448));
#46733=CARTESIAN_POINT('Ctrl Pts',(28.5427132787644,0.407261741609369,27.6023743476884));
#46734=CARTESIAN_POINT('Ctrl Pts',(28.4873635075659,0.0164898797776363,
27.624083895568));
#46735=CARTESIAN_POINT('Ctrl Pts',(28.4981279946982,-0.180903932406258,
27.6350502184671));
#46736=CARTESIAN_POINT('Ctrl Pts',(28.5934885065557,-0.554852956622451,
27.6558251642568));
#46737=CARTESIAN_POINT('Ctrl Pts',(28.6750314181996,-0.72841210507679,27.6648194223046));
#46738=CARTESIAN_POINT('Ctrl Pts',(28.9037835277885,-1.04301134033857,27.6845641309549));
#46739=CARTESIAN_POINT('Ctrl Pts',(29.0515807305306,-1.17900166318454,27.6954525361552));
#46740=CARTESIAN_POINT('Ctrl Pts',(29.3870321030576,-1.38265756586298,27.7172490562487));
#46741=CARTESIAN_POINT('Ctrl Pts',(29.570408592882,-1.45015060314336,27.7279465683201));
#46742=CARTESIAN_POINT('Ctrl Pts',(29.8405845073873,-1.49365112485936,27.7421537608929));
#46743=CARTESIAN_POINT('Ctrl Pts',(29.920314098353,-1.50000000000001,27.7461661102695));
#46744=CARTESIAN_POINT('Ctrl Pts',(30.,-1.50000000000001,27.75));
#46745=CARTESIAN_POINT('Ctrl Pts',(29.9999999999999,-1.50000000000001,27.8125));
#46746=CARTESIAN_POINT('Ctrl Pts',(29.9712572824709,-1.50000000000001,27.8111171153581));
#46747=CARTESIAN_POINT('Ctrl Pts',(29.9424874969812,-1.49917387170699,27.8097099804002));
#46748=CARTESIAN_POINT('Ctrl Pts',(29.7223735770152,-1.48649276547853,27.7987674915373));
#46749=CARTESIAN_POINT('Ctrl Pts',(29.5349257292356,-1.43889608772887,27.7884267728186));
#46750=CARTESIAN_POINT('Ctrl Pts',(29.1813453265204,-1.27257887490163,27.7667952051828));
#46751=CARTESIAN_POINT('Ctrl Pts',(29.0198117779222,-1.15277654761383,27.7556955762776));
#46752=CARTESIAN_POINT('Ctrl Pts',(28.7574522908629,-0.862041024530384,
27.7349968128188));
#46753=CARTESIAN_POINT('Ctrl Pts',(28.6572312223829,-0.695708343276581,
27.7261504635153));
#46754=CARTESIAN_POINT('Ctrl Pts',(28.524605736016,-0.332863036208749,27.7059923909005));
#46755=CARTESIAN_POINT('Ctrl Pts',(28.4939840388333,-0.139603136099824,
27.6952557297833));
#46756=CARTESIAN_POINT('Ctrl Pts',(28.508148989394,0.25282273238934,27.673454292645));
#46757=CARTESIAN_POINT('Ctrl Pts',(28.5547646373704,0.44816718663467,27.6626018229647));
#46758=CARTESIAN_POINT('Ctrl Pts',(28.7177569938957,0.801209312950165,27.6429883715028));
#46759=CARTESIAN_POINT('Ctrl Pts',(28.8294090431484,0.956981758536969,27.6339039237114));
#46760=CARTESIAN_POINT('Ctrl Pts',(29.1093968787388,1.22281551664853,27.6130487316321));
#46761=CARTESIAN_POINT('Ctrl Pts',(29.2767036270498,1.32864238149993,27.6020595468161));
#46762=CARTESIAN_POINT('Ctrl Pts',(29.6469534397504,1.47162694755714,27.5802741008953));
#46763=CARTESIAN_POINT('Ctrl Pts',(29.8468632228895,1.50560128622732,27.570023387908));
#46764=CARTESIAN_POINT('Ctrl Pts',(30.2385607914922,1.49319741260661,27.5508332778069));
#46765=CARTESIAN_POINT('Ctrl Pts',(30.4267058309758,1.45067195878526,27.540599882768));
#46766=CARTESIAN_POINT('Ctrl Pts',(30.7836729511717,1.29433057010809,27.5190824778378));
#46767=CARTESIAN_POINT('Ctrl Pts',(30.9479647504538,1.17932417828325,27.5079833629642));
#46768=CARTESIAN_POINT('Ctrl Pts',(31.2187102492265,0.89565657574078,27.4870774584548));
#46769=CARTESIAN_POINT('Ctrl Pts',(31.3239608540741,0.731149127851972,27.4781193959917));
#46770=CARTESIAN_POINT('Ctrl Pts',(31.4661242989034,0.37131396030254,27.4581285533501));
#46771=CARTESIAN_POINT('Ctrl Pts',(31.5017272578984,0.179429293592902,27.4474682940885));
#46772=CARTESIAN_POINT('Ctrl Pts',(31.4980926781097,-0.21275991516766,27.4256800047129));
#46773=CARTESIAN_POINT('Ctrl Pts',(31.4567210643059,-0.409304691427262,
27.4147608504762));
#46774=CARTESIAN_POINT('Ctrl Pts',(31.3031284414201,-0.766835781066652,
27.394898012163));
#46775=CARTESIAN_POINT('Ctrl Pts',(31.1955054411838,-0.925718941221814,
27.3859710339898));
#46776=CARTESIAN_POINT('Ctrl Pts',(30.9227930606553,-1.19862566676885,27.3652694110877));
#46777=CARTESIAN_POINT('Ctrl Pts',(30.75882230211,-1.30859982122977,27.354325526665));
#46778=CARTESIAN_POINT('Ctrl Pts',(30.3950972752779,-1.46060207029247,27.3326035134561));
#46779=CARTESIAN_POINT('Ctrl Pts',(30.198484714314,-1.4999999999587,27.3220496002711));
#46780=CARTESIAN_POINT('Ctrl Pts',(30.0000000003122,-1.50000000000001,27.312500000015));
#46781=CARTESIAN_POINT('Origin',(30.,-1.32966554433622E-14,16.));
#46782=CARTESIAN_POINT('',(30.,-1.50000000000001,26.75));
#46783=CARTESIAN_POINT('',(30.0000000000001,-1.50000000000001,26.8125));
#46784=CARTESIAN_POINT('',(30.,-1.50000000000001,16.));
#46785=CARTESIAN_POINT('Ctrl Pts',(29.9999999999999,-1.50000000000002,26.75));
#46786=CARTESIAN_POINT('Ctrl Pts',(30.1755630845093,-1.50000000000003,26.7584467828418));
#46787=CARTESIAN_POINT('Ctrl Pts',(30.3499584064833,-1.46918259215549,26.7676934207892));
#46788=CARTESIAN_POINT('Ctrl Pts',(30.6997034276012,-1.3412672085792,26.7880737410627));
#46789=CARTESIAN_POINT('Ctrl Pts',(30.8691431470038,-1.23821435243508,26.7990884927007));
#46790=CARTESIAN_POINT('Ctrl Pts',(31.1538803669515,-0.977054933639417,
26.8200423468827));
#46791=CARTESIAN_POINT('Ctrl Pts',(31.2681733329846,-0.823282264050392,
26.8292620964417));
#46792=CARTESIAN_POINT('Ctrl Pts',(31.4372326110993,-0.473197410553428,
26.8487112549693));
#46793=CARTESIAN_POINT('Ctrl Pts',(31.4872301101415,-0.278708237309613,
26.8595162090384));
#46794=CARTESIAN_POINT('Ctrl Pts',(31.5082331683214,0.113718878171538,26.881317715454));
#46795=CARTESIAN_POINT('Ctrl Pts',(31.4808674747884,0.307802550913579,26.8921001417175));
#46796=CARTESIAN_POINT('Ctrl Pts',(31.3544261384598,0.67256246632588,26.9123645814626));
#46797=CARTESIAN_POINT('Ctrl Pts',(31.2574072539999,0.840081862517357,26.9211719059107));
#46798=CARTESIAN_POINT('Ctrl Pts',(31.0004574791989,1.1352928844589,26.9417347138799));
#46799=CARTESIAN_POINT('Ctrl Pts',(30.8407636896231,1.25813738072432,26.9528303320317));
#46800=CARTESIAN_POINT('Ctrl Pts',(30.4894980147219,1.43081423936239,26.9745271891017));
#46801=CARTESIAN_POINT('Ctrl Pts',(30.302568408204,1.48165789304525,26.984933167702));
#46802=CARTESIAN_POINT('Ctrl Pts',(29.9140424353861,1.51051713966446,27.0044277780243));
#46803=CARTESIAN_POINT('Ctrl Pts',(29.7160053760103,1.48607476032932,27.0140505099305));
#46804=CARTESIAN_POINT('Ctrl Pts',(29.3413420123945,1.36197834203437,27.0355236321475));
#46805=CARTESIAN_POINT('Ctrl Pts',(29.1683424827117,1.26378814603618,27.0465745813446));
#46806=CARTESIAN_POINT('Ctrl Pts',(28.87548492057,1.01073104588063,27.0676940612658));
#46807=CARTESIAN_POINT('Ctrl Pts',(28.7566499301147,0.860326156686485,27.0772041024063));
#46808=CARTESIAN_POINT('Ctrl Pts',(28.5773390955292,0.515342682333064,27.0963698509815));
#46809=CARTESIAN_POINT('Ctrl Pts',(28.5216397715234,0.322442560698391,27.1070865244057));
#46810=CARTESIAN_POINT('Ctrl Pts',(28.4890218615652,-0.0697120082430973,
27.1288728893469));
#46811=CARTESIAN_POINT('Ctrl Pts',(28.510818362855,-0.265069960572926,27.1397261089208));
#46812=CARTESIAN_POINT('Ctrl Pts',(28.6267610927498,-0.633018179794785,
27.1601676766553));
#46813=CARTESIAN_POINT('Ctrl Pts',(28.7184387624141,-0.802555681667626,
27.1689674029211));
#46814=CARTESIAN_POINT('Ctrl Pts',(28.9662614123549,-1.10518359683465,27.1892971067025));
#46815=CARTESIAN_POINT('Ctrl Pts',(29.1227466839353,-1.23306866661795,27.2003783708913));
#46816=CARTESIAN_POINT('Ctrl Pts',(29.4698813680168,-1.416339226716,27.2221707450579));
#46817=CARTESIAN_POINT('Ctrl Pts',(29.6558172836666,-1.47261637710131,27.232679845148));
#46818=CARTESIAN_POINT('Ctrl Pts',(29.8981460836565,-1.49740948534734,27.2450275924248));
#46819=CARTESIAN_POINT('Ctrl Pts',(29.9491012405249,-1.5,27.247551132293));
#46820=CARTESIAN_POINT('Ctrl Pts',(29.9999999999998,-1.50000000000001,27.25));
#46821=CARTESIAN_POINT('Ctrl Pts',(30.0000000003122,-1.50000000000001,27.312500000015));
#46822=CARTESIAN_POINT('Ctrl Pts',(29.9998020603292,-1.50000000000005,27.3124904766232));
#46823=CARTESIAN_POINT('Ctrl Pts',(29.9996041185888,-1.49999996081992,27.3124809520584));
#46824=CARTESIAN_POINT('Ctrl Pts',(29.8088160951652,-1.49992443102837,27.3032995609518));
#46825=CARTESIAN_POINT('Ctrl Pts',(29.6200100906951,-1.46352575850992,27.2932045535897));
#46826=CARTESIAN_POINT('Ctrl Pts',(29.2593205849108,-1.31930644298838,27.2718447795537));
#46827=CARTESIAN_POINT('Ctrl Pts',(29.0918823606668,-1.21016636340677,27.2607572353565));
#46828=CARTESIAN_POINT('Ctrl Pts',(28.8110979291704,-0.935181294724627,
27.2396095139674));
#46829=CARTESIAN_POINT('Ctrl Pts',(28.6997118002275,-0.772848068745042,
27.2304360038192));
#46830=CARTESIAN_POINT('Ctrl Pts',(28.5461974612702,-0.416685157506792,
27.210649175417));
#46831=CARTESIAN_POINT('Ctrl Pts',(28.5047394765833,-0.226599155889903,
27.2000888419939));
#46832=CARTESIAN_POINT('Ctrl Pts',(28.4958539389935,0.166443777601294,27.1782531234666));
#46833=CARTESIAN_POINT('Ctrl Pts',(28.5315184967694,0.365700597221805,27.1671833001544));
#46834=CARTESIAN_POINT('Ctrl Pts',(28.6754701753172,0.729371435414476,27.1469793646992));
#46835=CARTESIAN_POINT('Ctrl Pts',(28.7788000491734,0.891648198610453,27.1381536711784));
#46836=CARTESIAN_POINT('Ctrl Pts',(29.0437345128306,1.17200464814443,27.1176193266989));
#46837=CARTESIAN_POINT('Ctrl Pts',(29.2040531543845,1.2862733419873,27.1067318620762));
#46838=CARTESIAN_POINT('Ctrl Pts',(29.5628324377282,1.44858368838945,27.0849614650246));
#46839=CARTESIAN_POINT('Ctrl Pts',(29.7584548095726,1.49371725552991,27.0742958690726));
#46840=CARTESIAN_POINT('Ctrl Pts',(30.1472060622831,1.50481186242553,27.055283882181));
#46841=CARTESIAN_POINT('Ctrl Pts',(30.3365600149074,1.47407427722924,27.045587089767));
#46842=CARTESIAN_POINT('Ctrl Pts',(30.7004989886168,1.34098519143669,27.0243801486806));
#46843=CARTESIAN_POINT('Ctrl Pts',(30.8706482413977,1.23730103012925,27.0133137233474));
#46844=CARTESIAN_POINT('Ctrl Pts',(31.1605713571455,0.970446090199086,26.991952153717));
#46845=CARTESIAN_POINT('Ctrl Pts',(31.2776619344983,0.810096307036669,26.9825053503909));
#46846=CARTESIAN_POINT('Ctrl Pts',(31.4414580755822,0.457344311316898,26.9629080172954));
#46847=CARTESIAN_POINT('Ctrl Pts',(31.4881418689773,0.269035150966863,26.9524463972759));
#46848=CARTESIAN_POINT('Ctrl Pts',(31.508284818313,-0.122458793694974,26.9306967336836));
#46849=CARTESIAN_POINT('Ctrl Pts',(31.478582774639,-0.322064434897177,26.9196075313946));
#46850=CARTESIAN_POINT('Ctrl Pts',(31.3455674834561,-0.689986184900448,
26.8991674341722));
#46851=CARTESIAN_POINT('Ctrl Pts',(31.246662212612,-0.855842984261559,26.8903733141072));
#46852=CARTESIAN_POINT('Ctrl Pts',(30.9897531567272,-1.14377092738595,26.8700147729728));
#46853=CARTESIAN_POINT('Ctrl Pts',(30.8332877383797,-1.26231706455743,26.8591938787678));
#46854=CARTESIAN_POINT('Ctrl Pts',(30.4799553603842,-1.43498001100993,26.8373979738484));
#46855=CARTESIAN_POINT('Ctrl Pts',(30.2857235516143,-1.48590367409306,26.8266384453951));
#46856=CARTESIAN_POINT('Ctrl Pts',(30.0581276265954,-1.49915605873645,26.8153201095514));
#46857=CARTESIAN_POINT('Ctrl Pts',(30.0290509426437,-1.50000000000001,26.8138977141296));
#46858=CARTESIAN_POINT('Ctrl Pts',(30.0000000000001,-1.50000000000001,26.8125));
#46859=CARTESIAN_POINT('Origin',(30.,-1.32966554433622E-14,16.));
#46860=CARTESIAN_POINT('',(30.,-1.50000000000001,26.25));
#46861=CARTESIAN_POINT('',(30.0000000000001,-1.50000000000001,26.3125));
#46862=CARTESIAN_POINT('',(30.,-1.50000000000001,16.));
#46863=CARTESIAN_POINT('Ctrl Pts',(30.,-1.50000000000001,26.25));
#46864=CARTESIAN_POINT('Ctrl Pts',(30.0056194401817,-1.50000000000001,26.2502703654418));
#46865=CARTESIAN_POINT('Ctrl Pts',(30.0112401600052,-1.49996842190559,26.2505416696197));
#46866=CARTESIAN_POINT('Ctrl Pts',(30.2156637559459,-1.49767029707552,26.2604408412659));
#46867=CARTESIAN_POINT('Ctrl Pts',(30.4120156853044,-1.45593401100177,26.2710471691517));
#46868=CARTESIAN_POINT('Ctrl Pts',(30.7738333695248,-1.29974623576057,26.2927936799124));
#46869=CARTESIAN_POINT('Ctrl Pts',(30.9363483004055,-1.18803068750778,26.3037158928437));
#46870=CARTESIAN_POINT('Ctrl Pts',(31.2059383925193,-0.91211987124096,26.3243507415389));
#46871=CARTESIAN_POINT('Ctrl Pts',(31.3118367658411,-0.751883140819906,
26.3332287143989));
#46872=CARTESIAN_POINT('Ctrl Pts',(31.4620725484111,-0.390717177178761,
26.3532934901568));
#46873=CARTESIAN_POINT('Ctrl Pts',(31.5011777050095,-0.191739563198423,
26.3643478020445));
#46874=CARTESIAN_POINT('Ctrl Pts',(31.4988144256802,0.202052743889533,26.3862251524383));
#46875=CARTESIAN_POINT('Ctrl Pts',(31.4603972352794,0.393097806012914,26.3968387670007));
#46876=CARTESIAN_POINT('Ctrl Pts',(31.3127984325509,0.751186708707084,26.4167325949282));
#46877=CARTESIAN_POINT('Ctrl Pts',(31.2046306350456,0.914654115967526,26.4257825736587));
#46878=CARTESIAN_POINT('Ctrl Pts',(30.929085340333,1.1942016269637,26.4468049614706));
#46879=CARTESIAN_POINT('Ctrl Pts',(30.763267624326,1.30642002708729,26.4579000478329));
#46880=CARTESIAN_POINT('Ctrl Pts',(30.4044749371868,1.4569895622401,26.479344956129));
#46881=CARTESIAN_POINT('Ctrl Pts',(30.2159899848526,1.49659297949806,26.4895135375502));
#46882=CARTESIAN_POINT('Ctrl Pts',(29.8264040657205,1.50311771775866,26.5084387415533));
#46883=CARTESIAN_POINT('Ctrl Pts',(29.6289313228251,1.46692091172634,26.5187719136178));
#46884=CARTESIAN_POINT('Ctrl Pts',(29.2622864534942,1.32066065000658,26.5404749081659));
#46885=CARTESIAN_POINT('Ctrl Pts',(29.0963152488665,1.21314636529189,26.5514467093804));
#46886=CARTESIAN_POINT('Ctrl Pts',(28.8192613253014,0.944447852152411,26.5722403200802));
#46887=CARTESIAN_POINT('Ctrl Pts',(28.7092361098565,0.787428080615722,26.5812539955214));
#46888=CARTESIAN_POINT('Ctrl Pts',(28.5500186537103,0.4325695152731,26.6009683602626));
#46889=CARTESIAN_POINT('Ctrl Pts',(28.5055087117716,0.236724815037938,26.6118486213868));
#46890=CARTESIAN_POINT('Ctrl Pts',(28.4955827399852,-0.155640049113208,
26.6336466693952));
#46891=CARTESIAN_POINT('Ctrl Pts',(28.5282144121142,-0.348361913823613,
26.6443534396569));
#46892=CARTESIAN_POINT('Ctrl Pts',(28.6646766132005,-0.710004687419899,
26.6644447048566));
#46893=CARTESIAN_POINT('Ctrl Pts',(28.7669073789545,-0.875602741749661,
26.6733284353239));
#46894=CARTESIAN_POINT('Ctrl Pts',(29.0326342692594,-1.16351957915387,26.6941109162225));
#46895=CARTESIAN_POINT('Ctrl Pts',(29.1952892767769,-1.28140768888904,26.7052113286353));
#46896=CARTESIAN_POINT('Ctrl Pts',(29.5502593863542,-1.44373597574174,26.7267989550745));
#46897=CARTESIAN_POINT('Ctrl Pts',(29.7380028348229,-1.48930167419739,26.7370974797965));
#46898=CARTESIAN_POINT('Ctrl Pts',(29.9528487018704,-1.49944465692866,26.7477160059146));
#46899=CARTESIAN_POINT('Ctrl Pts',(29.9764341399413,-1.50000000000001,26.7488661870293));
#46900=CARTESIAN_POINT('Ctrl Pts',(29.9999999999999,-1.50000000000001,26.75));
#46901=CARTESIAN_POINT('Ctrl Pts',(30.0000000000001,-1.50000000000001,26.8125));
#46902=CARTESIAN_POINT('Ctrl Pts',(29.8395800016776,-1.50000000000002,26.8047817892321));
#46903=CARTESIAN_POINT('Ctrl Pts',(29.6800130120943,-1.4742710204936,26.7963899249912));
#46904=CARTESIAN_POINT('Ctrl Pts',(29.3406580591605,-1.36160698346738,26.7769331456215));
#46905=CARTESIAN_POINT('Ctrl Pts',(29.1679496395237,-1.26348603655748,26.7658981260489));
#46906=CARTESIAN_POINT('Ctrl Pts',(28.8688888773426,-1.00499369846698,26.744329215695));
#46907=CARTESIAN_POINT('Ctrl Pts',(28.7459708502921,-0.846646295408431,
26.7345359053005));
#46908=CARTESIAN_POINT('Ctrl Pts',(28.5719299961441,-0.497373685523865,
26.7151318714181));
#46909=CARTESIAN_POINT('Ctrl Pts',(28.5201211210885,-0.310969647956289,
26.7047760915532));
#46910=CARTESIAN_POINT('Ctrl Pts',(28.4888763927518,0.078675171393689,26.6831291571448));
#46911=CARTESIAN_POINT('Ctrl Pts',(28.5126680280148,0.27845746343119,26.6720301409206));
#46912=CARTESIAN_POINT('Ctrl Pts',(28.6347687943924,0.650483449918004,26.6513620305602));
#46913=CARTESIAN_POINT('Ctrl Pts',(28.7293030467267,0.819946999855557,26.6425267967844));
#46914=CARTESIAN_POINT('Ctrl Pts',(28.9783004894773,1.11523286685495,26.62234451654));
#46915=CARTESIAN_POINT('Ctrl Pts',(29.1308905878018,1.23784103842587,26.6115972394678));
#46916=CARTESIAN_POINT('Ctrl Pts',(29.4786064716065,1.42045274911996,26.5897952036888));
#46917=CARTESIAN_POINT('Ctrl Pts',(29.671307799161,1.47699671076135,26.5789531911429));
#46918=CARTESIAN_POINT('Ctrl Pts',(30.058657983757,1.51083891985875,26.5593767353335));
#46919=CARTESIAN_POINT('Ctrl Pts',(30.2492918070221,1.49128918840572,26.5502639753537));
#46920=CARTESIAN_POINT('Ctrl Pts',(30.6191301716824,1.38027512961514,26.5293863948823));
#46921=CARTESIAN_POINT('Ctrl Pts',(30.7941362196709,1.2875659668366,26.518391157951));
#46922=CARTESIAN_POINT('Ctrl Pts',(31.1019229551517,1.03729505553015,26.4966307919773));
#46923=CARTESIAN_POINT('Ctrl Pts',(31.2305302882388,0.880892156398053,26.4864384531331));
#46924=CARTESIAN_POINT('Ctrl Pts',(31.4143329938993,0.535011347738905,26.467222852652));
#46925=CARTESIAN_POINT('Ctrl Pts',(31.4709425533457,0.350543024469619,26.4569746124704));
#46926=CARTESIAN_POINT('Ctrl Pts',(31.5126435249117,-0.0370627264893054,
26.4354409596394));
#46927=CARTESIAN_POINT('Ctrl Pts',(31.4944467514533,-0.236856679751601,
26.4243412955692));
#46928=CARTESIAN_POINT('Ctrl Pts',(31.382763240843,-0.612667143007661,26.4034629364995));
#46929=CARTESIAN_POINT('Ctrl Pts',(31.2923692914564,-0.785603738087747,
26.3945234871348));
#46930=CARTESIAN_POINT('Ctrl Pts',(31.0508333839059,-1.08773585408316,26.3745100265869));
#46931=CARTESIAN_POINT('Ctrl Pts',(30.9019600520426,-1.21403192877114,26.3638391307711));
#46932=CARTESIAN_POINT('Ctrl Pts',(30.559750929656,-1.4057831061822,26.3420481650989));
#46933=CARTESIAN_POINT('Ctrl Pts',(30.3686322762759,-1.46754077280931,26.3311374738613));
#46934=CARTESIAN_POINT('Ctrl Pts',(30.1141378164167,-1.49674664949133,26.3180818291001));
#46935=CARTESIAN_POINT('Ctrl Pts',(30.0570405412872,-1.50000000000001,26.3152443643222));
#46936=CARTESIAN_POINT('Ctrl Pts',(30.0000000000002,-1.50000000000001,26.3125));
#46937=CARTESIAN_POINT('Origin',(30.,-1.32966554433622E-14,16.));
#46938=CARTESIAN_POINT('',(30.0000000000001,-1.50000000000001,25.75));
#46939=CARTESIAN_POINT('',(30.,-1.50000000000001,25.8125));
#46940=CARTESIAN_POINT('',(30.,-1.50000000000001,16.));
#46941=CARTESIAN_POINT('Ctrl Pts',(30.0000000000002,-1.50000000000001,25.75));
#46942=CARTESIAN_POINT('Ctrl Pts',(30.0350308469701,-1.50000000000001,25.7516854224107));
#46943=CARTESIAN_POINT('Ctrl Pts',(30.0700958017757,-1.49877287551864,25.7534065726266));
#46944=CARTESIAN_POINT('Ctrl Pts',(30.3035194655511,-1.48237243734734,25.7650927416133));
#46945=CARTESIAN_POINT('Ctrl Pts',(30.4971388675202,-1.42911969045028,25.7758875024032));
#46946=CARTESIAN_POINT('Ctrl Pts',(30.848183508266,-1.2523218603483,25.7976881963921));
#46947=CARTESIAN_POINT('Ctrl Pts',(31.0030592952475,-1.13208157746957,25.8084796690252));
#46948=CARTESIAN_POINT('Ctrl Pts',(31.2567047166631,-0.841106936698577,
25.8287658189633));
#46949=CARTESIAN_POINT('Ctrl Pts',(31.3538096540821,-0.673770640691784,
25.8375682977395));
#46950=CARTESIAN_POINT('Ctrl Pts',(31.4823392304013,-0.304145984064151,
25.8581030008855));
#46951=CARTESIAN_POINT('Ctrl Pts',(31.5096068971125,-0.104447172132542,
25.8691973793261));
#46952=CARTESIAN_POINT('Ctrl Pts',(31.4848844296652,0.286323023183646,25.8909068346215));
#46953=CARTESIAN_POINT('Ctrl Pts',(31.4360830652788,0.473864860798067,25.9013258256));
#46954=CARTESIAN_POINT('Ctrl Pts',(31.2680746858178,0.825196096656156,25.9208442275921));
#46955=CARTESIAN_POINT('Ctrl Pts',(31.1486056539627,0.984726473310249,25.9304245311885));
#46956=CARTESIAN_POINT('Ctrl Pts',(30.8549287066094,1.24817526789042,25.9518720919776));
#46957=CARTESIAN_POINT('Ctrl Pts',(30.6837094772403,1.34958696185865,25.9629268724906));
#46958=CARTESIAN_POINT('Ctrl Pts',(30.3185036845909,1.47806545582453,25.9840666914365));
#46959=CARTESIAN_POINT('Ctrl Pts',(30.1289070957048,1.50647679352315,25.993618043535));
#46960=CARTESIAN_POINT('Ctrl Pts',(29.7404075656125,1.49068855536224,26.0127482980627));
#46961=CARTESIAN_POINT('Ctrl Pts',(29.545331017818,1.44318830470102,26.0234533742517));
#46962=CARTESIAN_POINT('Ctrl Pts',(29.188736991222,1.27663378618483,26.0452365267588));
#46963=CARTESIAN_POINT('Ctrl Pts',(29.0299764729631,1.16060540084053,26.056097906459));
#46964=CARTESIAN_POINT('Ctrl Pts',(28.7683079019703,0.877153943717209,26.0765610930375));
#46965=CARTESIAN_POINT('Ctrl Pts',(28.6667786145465,0.713430148276809,26.0853649917623));
#46966=CARTESIAN_POINT('Ctrl Pts',(28.5272614190292,0.348018884480366,26.1056656175288));
#46967=CARTESIAN_POINT('Ctrl Pts',(28.4940188142116,0.14859972255689,26.1167444598579));
#46968=CARTESIAN_POINT('Ctrl Pts',(28.5074840531687,-0.243852309362615,
26.1385473505201));
#46969=CARTESIAN_POINT('Ctrl Pts',(28.5510714566589,-0.433234122923729,
26.1490685623846));
#46970=CARTESIAN_POINT('Ctrl Pts',(28.7087569062828,-0.788023018123922,
26.1687790565624));
#46971=CARTESIAN_POINT('Ctrl Pts',(28.8224400778707,-0.949553940205162,
26.1780544535033));
#46972=CARTESIAN_POINT('Ctrl Pts',(29.1069273076436,-1.22127183449108,26.1992895710132));
#46973=CARTESIAN_POINT('Ctrl Pts',(29.2754819087647,-1.32821443027861,26.2103697857015));
#46974=CARTESIAN_POINT('Ctrl Pts',(29.6323103908041,-1.46593097223903,26.2313631635471));
#46975=CARTESIAN_POINT('Ctrl Pts',(29.8154198943914,-1.50000000000001,26.2411193855283));
#46976=CARTESIAN_POINT('Ctrl Pts',(30.,-1.50000000000001,26.25));
#46977=CARTESIAN_POINT('Ctrl Pts',(30.0000000000002,-1.50000000000001,26.3125));
#46978=CARTESIAN_POINT('Ctrl Pts',(29.867580258195,-1.50000000000001,26.3061289522019));
#46979=CARTESIAN_POINT('Ctrl Pts',(29.7355134428156,-1.48246999719879,26.299287940062));
#46980=CARTESIAN_POINT('Ctrl Pts',(29.4184023489971,-1.39643165750255,26.2816409715667));
#46981=CARTESIAN_POINT('Ctrl Pts',(29.2414246745114,-1.30875331188796,26.2706906196325));
#46982=CARTESIAN_POINT('Ctrl Pts',(28.9285790709285,-1.068455989113,26.2489639028796));
#46983=CARTESIAN_POINT('Ctrl Pts',(28.7965902868422,-0.917216536990246,
26.2384564742772));
#46984=CARTESIAN_POINT('Ctrl Pts',(28.6032774267936,-0.57923818308581,26.2196798990602));
#46985=CARTESIAN_POINT('Ctrl Pts',(28.5410496718181,-0.397228347537677,
26.2095682415298));
#46986=CARTESIAN_POINT('Ctrl Pts',(28.4870387262231,-0.0124011503103316,
26.1881889527949));
#46987=CARTESIAN_POINT('Ctrl Pts',(28.4986129287161,0.187210043596071,26.1770994420224));
#46988=CARTESIAN_POINT('Ctrl Pts',(28.5978341126594,0.567369358609899,26.1559794800772));
#46989=CARTESIAN_POINT('Ctrl Pts',(28.6833047820777,0.744501773375072,26.1468355900596));
#46990=CARTESIAN_POINT('Ctrl Pts',(28.9160253075989,1.05460577600707,26.1270248184819));
#46991=CARTESIAN_POINT('Ctrl Pts',(29.060441358732,1.18507685788338,26.1164524012633));
#46992=CARTESIAN_POINT('Ctrl Pts',(29.3972605323865,1.3881264388998,26.0946069150758));
#46993=CARTESIAN_POINT('Ctrl Pts',(29.5879874006837,1.45617711323181,26.0835402678372));
#46994=CARTESIAN_POINT('Ctrl Pts',(29.9751313819113,1.51185807000195,26.0633671011121));
#46995=CARTESIAN_POINT('Ctrl Pts',(30.1672228871666,1.50278877622694,26.0545319510962));
#46996=CARTESIAN_POINT('Ctrl Pts',(30.5421508905102,1.41213985662164,26.0339751935801));
#46997=CARTESIAN_POINT('Ctrl Pts',(30.7210278648892,1.32972839399854,26.0230797638426));
#46998=CARTESIAN_POINT('Ctrl Pts',(31.0401525812529,1.09890434445495,26.0013140896138));
#46999=CARTESIAN_POINT('Ctrl Pts',(31.1764827770535,0.951536572108244,25.9906613507783));
#47000=CARTESIAN_POINT('Ctrl Pts',(31.3792148041551,0.619604996410003,25.9716870800294));
#47001=CARTESIAN_POINT('Ctrl Pts',(31.4465937278795,0.439945368358781,25.9619414093531));
#47002=CARTESIAN_POINT('Ctrl Pts',(31.5118285637272,0.0578389075257285,
25.9407132726402));
#47003=CARTESIAN_POINT('Ctrl Pts',(31.5063115855957,-0.141417075009879,
25.9296434958327));
#47004=CARTESIAN_POINT('Ctrl Pts',(31.4186362556573,-0.525426994647723,
25.9083096114084));
#47005=CARTESIAN_POINT('Ctrl Pts',(31.3377111820022,-0.706481965554299,
25.8989028268757));
#47006=CARTESIAN_POINT('Ctrl Pts',(31.1130533652913,-1.0237694591265,25.8792804311414));
#47007=CARTESIAN_POINT('Ctrl Pts',(30.972766729538,-1.15788504149396,25.8688054543882));
#47008=CARTESIAN_POINT('Ctrl Pts',(30.6428698469895,-1.36991560346518,25.8470435453937));
#47009=CARTESIAN_POINT('Ctrl Pts',(30.4547968017865,-1.44330311864552,25.835956334699));
#47010=CARTESIAN_POINT('Ctrl Pts',(30.1725168697432,-1.4925627888959,25.8210068109627));
#47011=CARTESIAN_POINT('Ctrl Pts',(30.0862466800351,-1.50000000000001,25.8166495453279));
#47012=CARTESIAN_POINT('Ctrl Pts',(30.,-1.50000000000001,25.8125));
#47013=CARTESIAN_POINT('Origin',(30.,-1.32966554433622E-14,16.));
#47014=CARTESIAN_POINT('',(30.0000000000001,-1.50000000000001,25.25));
#47015=CARTESIAN_POINT('',(30.,-1.50000000000001,25.3125));
#47016=CARTESIAN_POINT('',(30.,-1.50000000000001,16.));
#47017=CARTESIAN_POINT('Ctrl Pts',(30.0000000000001,-1.50000000000001,25.25));
#47018=CARTESIAN_POINT('Ctrl Pts',(30.0627700539087,-1.50000000000001,25.2530200256268));
#47019=CARTESIAN_POINT('Ctrl Pts',(30.1255978857231,-1.49606031931736,25.2561522666689));
#47020=CARTESIAN_POINT('Ctrl Pts',(30.387395972516,-1.46296629655124,25.2696673114027));
#47021=CARTESIAN_POINT('Ctrl Pts',(30.5795743359629,-1.39800636679879,25.2807179397182));
#47022=CARTESIAN_POINT('Ctrl Pts',(30.9202426421314,-1.20018691165606,25.3026033361058));
#47023=CARTESIAN_POINT('Ctrl Pts',(31.0669765445057,-1.07185443274338,25.3132278653563));
#47024=CARTESIAN_POINT('Ctrl Pts',(31.3042648643842,-0.765865616588927,
25.3331440943071));
#47025=CARTESIAN_POINT('Ctrl Pts',(31.3922917557281,-0.59091969078094,25.3421711282901));
#47026=CARTESIAN_POINT('Ctrl Pts',(31.4979914701149,-0.212996523390812,
25.3631668598117));
#47027=CARTESIAN_POINT('Ctrl Pts',(31.5129981369395,-0.0132639168507718,
25.3742631157306));
#47028=CARTESIAN_POINT('Ctrl Pts',(31.4653583210385,0.373052959697002,25.3957251644277));
#47029=CARTESIAN_POINT('Ctrl Pts',(31.4060337226141,0.556359728684241,25.4059088738159));
#47030=CARTESIAN_POINT('Ctrl Pts',(31.2180258231604,0.89772836856045,25.4248737982534));
#47031=CARTESIAN_POINT('Ctrl Pts',(31.088460968798,1.05109657163312,25.4351618575451));
#47032=CARTESIAN_POINT('Ctrl Pts',(30.7792551558925,1.29659274113508,25.4568578671965));
#47033=CARTESIAN_POINT('Ctrl Pts',(30.6034030192283,1.3871914976091,25.4678351891908));
#47034=CARTESIAN_POINT('Ctrl Pts',(30.2324892526205,1.49400946706811,25.4886479519256));
#47035=CARTESIAN_POINT('Ctrl Pts',(30.0415773273281,1.51141487828139,25.4976825299541));
#47036=CARTESIAN_POINT('Ctrl Pts',(29.6545526771042,1.47316919187237,25.5173656422979));
#47037=CARTESIAN_POINT('Ctrl Pts',(29.4624963512885,1.41443679130397,25.5282374121534));
#47038=CARTESIAN_POINT('Ctrl Pts',(29.1170567587378,1.22797823527613,25.5500367866331));
#47039=CARTESIAN_POINT('Ctrl Pts',(28.9660123174462,1.10381260264269,25.560752961054));
#47040=CARTESIAN_POINT('Ctrl Pts',(28.7201314342041,0.805655980053721,25.5808650389699));
#47041=CARTESIAN_POINT('Ctrl Pts',(28.627324212077,0.634750626561539,25.5897360763022));
#47042=CARTESIAN_POINT('Ctrl Pts',(28.5095600205757,0.261132939276874,25.6104926144847));
#47043=CARTESIAN_POINT('Ctrl Pts',(28.4881034640454,0.0613273497745445,
25.6215929250126));
#47044=CARTESIAN_POINT('Ctrl Pts',(28.5237184917358,-0.327500650137204,
25.6431944805633));
#47045=CARTESIAN_POINT('Ctrl Pts',(28.57753700972,-0.513112472024964,25.6535062484459));
#47046=CARTESIAN_POINT('Ctrl Pts',(28.7556436240904,-0.860981573894074,
25.6728323096608));
#47047=CARTESIAN_POINT('Ctrl Pts',(28.8809148866478,-1.0185241445112,25.6827836630609));
#47048=CARTESIAN_POINT('Ctrl Pts',(29.1836083572217,-1.27362286430434,25.7044330850039));
#47049=CARTESIAN_POINT('Ctrl Pts',(29.357290902101,-1.3695025366285,25.7154527145718));
#47050=CARTESIAN_POINT('Ctrl Pts',(29.6920067607584,-1.47617903100382,25.7345199747848));
#47051=CARTESIAN_POINT('Ctrl Pts',(29.8456406050883,-1.50000000000001,25.7425733801496));
#47052=CARTESIAN_POINT('Ctrl Pts',(30.0000000000002,-1.50000000000001,25.75));
#47053=CARTESIAN_POINT('Ctrl Pts',(30.,-1.50000000000001,25.8125));
#47054=CARTESIAN_POINT('Ctrl Pts',(29.8958136711151,-1.50000000000001,25.8074873329144));
#47055=CARTESIAN_POINT('Ctrl Pts',(29.7916909834384,-1.4891476478018,25.80217627354));
#47056=CARTESIAN_POINT('Ctrl Pts',(29.4989680289332,-1.42717135574301,25.7863710701566));
#47057=CARTESIAN_POINT('Ctrl Pts',(29.3182929815531,-1.3502283271827,25.7755410315376));
#47058=CARTESIAN_POINT('Ctrl Pts',(28.9928896773701,-1.12927046795383,25.7537473394536));
#47059=CARTESIAN_POINT('Ctrl Pts',(28.8522264483536,-0.985982788210688,
25.7429994633659));
#47060=CARTESIAN_POINT('Ctrl Pts',(28.639853465626,-0.660351661724937,25.7237363544014));
#47061=CARTESIAN_POINT('Ctrl Pts',(28.5672444995779,-0.483012345456745,
25.714334019192));
#47062=CARTESIAN_POINT('Ctrl Pts',(28.4907135279836,-0.103874220197911,
25.6932707900109));
#47063=CARTESIAN_POINT('Ctrl Pts',(28.4901189594842,0.0948392876888842,
25.6822311506839));
#47064=CARTESIAN_POINT('Ctrl Pts',(28.5659791907661,0.482606924381713,25.660688504201));
#47065=CARTESIAN_POINT('Ctrl Pts',(28.6422553573453,0.667705397375409,25.6509438140946));
#47066=CARTESIAN_POINT('Ctrl Pts',(28.8587620723286,0.992152292410515,25.6315147161622));
#47067=CARTESIAN_POINT('Ctrl Pts',(28.9948328944551,1.12978254443193,25.6211449431241));
#47068=CARTESIAN_POINT('Ctrl Pts',(29.3175819275344,1.35056278988812,25.599483888434));
#47069=CARTESIAN_POINT('Ctrl Pts',(29.5028611462505,1.42918794783786,25.5883856057019));
#47070=CARTESIAN_POINT('Ctrl Pts',(29.8863465577115,1.507984767606,25.5677463546914));
#47071=CARTESIAN_POINT('Ctrl Pts',(30.0802506039983,1.51013051078303,25.5589203440921));
#47072=CARTESIAN_POINT('Ctrl Pts',(30.4601704571654,1.44079280620514,25.5387153942847));
#47073=CARTESIAN_POINT('Ctrl Pts',(30.6424548754516,1.36926262641685,25.5279582816823));
#47074=CARTESIAN_POINT('Ctrl Pts',(30.9737363815272,1.15817666999724,25.5061559940003));
#47075=CARTESIAN_POINT('Ctrl Pts',(31.118540202541,1.01903114337744,25.4953239633962));
#47076=CARTESIAN_POINT('Ctrl Pts',(31.3403349350297,0.699693252907024,25.4757823623965));
#47077=CARTESIAN_POINT('Ctrl Pts',(31.418072458882,0.524551989157358,25.4666417771753));
#47078=CARTESIAN_POINT('Ctrl Pts',(31.5054879258866,0.148377517280613,25.4457431954044));
#47079=CARTESIAN_POINT('Ctrl Pts',(31.5119666548414,-0.0496365545101339,
25.4347424136382));
#47080=CARTESIAN_POINT('Ctrl Pts',(31.4476607795272,-0.440895614279282,
25.4130057992066));
#47081=CARTESIAN_POINT('Ctrl Pts',(31.3759395541655,-0.629971074835861,
25.4028673928089));
#47082=CARTESIAN_POINT('Ctrl Pts',(31.1673112734267,-0.961240411187918,
25.383627833962));
#47083=CARTESIAN_POINT('Ctrl Pts',(31.0353453440586,-1.10210544227651,25.3733657026948));
#47084=CARTESIAN_POINT('Ctrl Pts',(30.7196295943324,-1.33102399282861,25.3518169729773));
#47085=CARTESIAN_POINT('Ctrl Pts',(30.5371475111052,-1.41455738295539,25.3407169277066));
#47086=CARTESIAN_POINT('Ctrl Pts',(30.2307882933611,-1.48667060842925,25.3239740678184));
#47087=CARTESIAN_POINT('Ctrl Pts',(30.1154677152456,-1.50000000000002,25.31805544304));
#47088=CARTESIAN_POINT('Ctrl Pts',(29.9999999999999,-1.50000000000001,25.3125));
#47089=CARTESIAN_POINT('Origin',(30.,-1.32966554433622E-14,16.));
#47090=CARTESIAN_POINT('',(30.,-1.50000000000001,24.75));
#47091=CARTESIAN_POINT('',(29.9999999999999,-1.50000000000001,24.8125));
#47092=CARTESIAN_POINT('',(30.,-1.50000000000001,16.));
#47093=CARTESIAN_POINT('Ctrl Pts',(30.,-1.50000000000001,24.75));
#47094=CARTESIAN_POINT('Ctrl Pts',(30.0924202028298,-1.50000000000002,24.7544465690819));
#47095=CARTESIAN_POINT('Ctrl Pts',(30.1848415762481,-1.49146009950343,24.759130413942));
#47096=CARTESIAN_POINT('Ctrl Pts',(30.4723479931102,-1.43762037173554,24.7744586208663));
#47097=CARTESIAN_POINT('Ctrl Pts',(30.6592834359903,-1.36205645668747,24.7855515541955));
#47098=CARTESIAN_POINT('Ctrl Pts',(30.9862537983022,-1.14638219357722,24.80727387484));
#47099=CARTESIAN_POINT('Ctrl Pts',(31.1248087259681,-1.01079850350159,24.8177063155187));
#47100=CARTESIAN_POINT('Ctrl Pts',(31.346109752526,-0.69055016576277,24.8372494532827));
#47101=CARTESIAN_POINT('Ctrl Pts',(31.4251274703691,-0.50783917665878,24.8467867124079));
#47102=CARTESIAN_POINT('Ctrl Pts',(31.5079543915197,-0.122264618516638,
24.8682075211936));
#47103=CARTESIAN_POINT('Ctrl Pts',(31.5109523526148,0.0767903025210503,
24.8792661279179));
#47104=CARTESIAN_POINT('Ctrl Pts',(31.441061251381,0.457686740875712,24.9004270411598));
#47105=CARTESIAN_POINT('Ctrl Pts',(31.3715371249325,0.636385044039808,24.9100225849775));
#47106=CARTESIAN_POINT('Ctrl Pts',(31.1648481820269,0.965747220324715,24.9291158607209));
#47107=CARTESIAN_POINT('Ctrl Pts',(31.0267283705006,1.11145999209774,24.939808730245));
#47108=CARTESIAN_POINT('Ctrl Pts',(30.7049953637051,1.33826413832451,24.9615882319247));
#47109=CARTESIAN_POINT('Ctrl Pts',(30.525362209954,1.41844022126688,24.9724579494792));
#47110=CARTESIAN_POINT('Ctrl Pts',(30.1493787440764,1.50469862427576,24.9929435291658));
#47111=CARTESIAN_POINT('Ctrl Pts',(29.9569371691124,1.5114809139774,25.00175294714));
#47112=CARTESIAN_POINT('Ctrl Pts',(29.5704977811955,1.45108059660786,25.0220233074535));
#47113=CARTESIAN_POINT('Ctrl Pts',(29.3808354910635,1.38084291684638,25.0330994853021));
#47114=CARTESIAN_POINT('Ctrl Pts',(29.0468101101847,1.17410520091496,25.0549130032641));
#47115=CARTESIAN_POINT('Ctrl Pts',(28.9040664949486,1.04213311105638,25.0654466500392));
#47116=CARTESIAN_POINT('Ctrl Pts',(28.6746221434491,0.72909790198446,25.0851812190219));
#47117=CARTESIAN_POINT('Ctrl Pts',(28.5909928953227,0.55038117737188,25.0944232679238));
#47118=CARTESIAN_POINT('Ctrl Pts',(28.496446216206,0.168641933616187,25.115631003688));
#47119=CARTESIAN_POINT('Ctrl Pts',(28.4873339658181,-0.0308466586561953,
25.1267137032587));
#47120=CARTESIAN_POINT('Ctrl Pts',(28.5459190178277,-0.414647584032544,
25.1480359768907));
#47121=CARTESIAN_POINT('Ctrl Pts',(28.6102581790788,-0.595692019972521,
25.1580163493537));
#47122=CARTESIAN_POINT('Ctrl Pts',(28.8073809961852,-0.931227827424643,
25.1768208644096));
#47123=CARTESIAN_POINT('Ctrl Pts',(28.9411488677475,-1.08089452062442,25.1874141822753));
#47124=CARTESIAN_POINT('Ctrl Pts',(29.2565034825196,-1.31734526046784,25.2091547643595));
#47125=CARTESIAN_POINT('Ctrl Pts',(29.4342658933141,-1.40290303357365,25.220083967145));
#47126=CARTESIAN_POINT('Ctrl Pts',(29.7466738861071,-1.48392560477994,25.2373653306843));
#47127=CARTESIAN_POINT('Ctrl Pts',(29.8731973879732,-1.50000000000001,25.2438992064844));
#47128=CARTESIAN_POINT('Ctrl Pts',(30.0000000000001,-1.50000000000001,25.25));
#47129=CARTESIAN_POINT('Ctrl Pts',(29.9999999999999,-1.50000000000001,25.3125));
#47130=CARTESIAN_POINT('Ctrl Pts',(29.9230963675565,-1.50000000000001,25.3087999722589));
#47131=CARTESIAN_POINT('Ctrl Pts',(29.8461434428577,-1.49408668250554,25.3049333141238));
#47132=CARTESIAN_POINT('Ctrl Pts',(29.5785997947569,-1.4525378268213,25.2909069794727));
#47133=CARTESIAN_POINT('Ctrl Pts',(29.394946779968,-1.38612426885289,25.2802261486243));
#47134=CARTESIAN_POINT('Ctrl Pts',(29.0584111434883,-1.1844646483524,25.2584329141398));
#47135=CARTESIAN_POINT('Ctrl Pts',(28.9098271705268,-1.04932739740415,25.2475303518813));
#47136=CARTESIAN_POINT('Ctrl Pts',(28.679224033866,-0.736002543967933,25.2277319851447));
#47137=CARTESIAN_POINT('Ctrl Pts',(28.5966653608253,-0.562858820299269,
25.218769934461));
#47138=CARTESIAN_POINT('Ctrl Pts',(28.4992036771274,-0.189506940379824,
25.1980281633544));
#47139=CARTESIAN_POINT('Ctrl Pts',(28.4873077258157,0.00770736323463039,
25.1870718131536));
#47140=CARTESIAN_POINT('Ctrl Pts',(28.5403428741226,0.398677937032776,25.1653512257204));
#47141=CARTESIAN_POINT('Ctrl Pts',(28.6059812891417,0.588385613614782,25.1548923783415));
#47142=CARTESIAN_POINT('Ctrl Pts',(28.8032229731553,0.924175534219124,25.1360750856002));
#47143=CARTESIAN_POINT('Ctrl Pts',(28.9302878616598,1.06867554049118,25.1259477842385));
#47144=CARTESIAN_POINT('Ctrl Pts',(29.2375170160562,1.30684882772379,25.1045502900104));
#47145=CARTESIAN_POINT('Ctrl Pts',(29.416566346389,1.39601031268743,25.0934590671725));
#47146=CARTESIAN_POINT('Ctrl Pts',(29.7956879290814,1.49872079338579,25.0723655026123));
#47147=CARTESIAN_POINT('Ctrl Pts',(29.9916913791595,1.51255777708596,25.0632485758478));
#47148=CARTESIAN_POINT('Ctrl Pts',(30.376338186137,1.46478286918679,25.0434151669436));
#47149=CARTESIAN_POINT('Ctrl Pts',(30.5613937867408,1.40429329778983,25.0328314093361));
#47150=CARTESIAN_POINT('Ctrl Pts',(30.9051019650582,1.2128519030953,25.0109769253773));
#47151=CARTESIAN_POINT('Ctrl Pts',(31.0589867932662,1.08110262857348,24.9999134360581));
#47152=CARTESIAN_POINT('Ctrl Pts',(31.2996601001576,0.7727813254929,24.9797695555402));
#47153=CARTESIAN_POINT('Ctrl Pts',(31.3872075591177,0.601637196257516,24.9709242886809));
#47154=CARTESIAN_POINT('Ctrl Pts',(31.4948659823167,0.231233394936456,24.9503462997187));
#47155=CARTESIAN_POINT('Ctrl Pts',(31.5122374051454,0.0349818838105959,
24.9394434379894));
#47156=CARTESIAN_POINT('Ctrl Pts',(31.4704629549247,-0.356714017311379,
24.9176825545938));
#47157=CARTESIAN_POINT('Ctrl Pts',(31.410306361987,-0.548240683911054,24.9070421842271));
#47158=CARTESIAN_POINT('Ctrl Pts',(31.2229499202263,-0.889130700933294,
24.8881038499482));
#47159=CARTESIAN_POINT('Ctrl Pts',(31.1004741653132,-1.03689935475768,24.8783104947773));
#47160=CARTESIAN_POINT('Ctrl Pts',(30.8011609016804,-1.28341012707365,24.8570622572132));
#47161=CARTESIAN_POINT('Ctrl Pts',(30.6254139659021,-1.37762857486559,24.8459894497178));
#47162=CARTESIAN_POINT('Ctrl Pts',(30.2947063232275,-1.4782094919839,24.8272843564766));
#47163=CARTESIAN_POINT('Ctrl Pts',(30.1476360382517,-1.50000000000004,24.8196031422022));
#47164=CARTESIAN_POINT('Ctrl Pts',(29.9999999999998,-1.50000000000001,24.8125));
#47165=CARTESIAN_POINT('Origin',(30.,-1.32966554433622E-14,16.));
#47166=CARTESIAN_POINT('',(30.,-1.50000000000001,24.25));
#47167=CARTESIAN_POINT('',(30.,-1.50000000000001,24.3125));
#47168=CARTESIAN_POINT('',(30.,-1.50000000000001,16.));
#47169=CARTESIAN_POINT('Ctrl Pts',(29.9999999999999,-1.50000000000001,24.25));
#47170=CARTESIAN_POINT('Ctrl Pts',(30.1233865336442,-1.50000000000002,24.2559364373678));
#47171=CARTESIAN_POINT('Ctrl Pts',(30.2465476489323,-1.48477988594364,24.2622848102359));
#47172=CARTESIAN_POINT('Ctrl Pts',(30.5591244259704,-1.40597165010196,24.2795127850953));
#47173=CARTESIAN_POINT('Ctrl Pts',(30.7400033595231,-1.31975922707827,24.2906101163719));
#47174=CARTESIAN_POINT('Ctrl Pts',(31.0517371878966,-1.08642473531537,24.3120899308425));
#47175=CARTESIAN_POINT('Ctrl Pts',(31.181396759577,-0.943819238764671,24.3222894436867));
#47176=CARTESIAN_POINT('Ctrl Pts',(31.3842738432636,-0.610977913754327,
24.341295964288));
#47177=CARTESIAN_POINT('Ctrl Pts',(31.4529950991553,-0.422325812949031,
24.3515374548362));
#47178=CARTESIAN_POINT('Ctrl Pts',(31.5124147536636,-0.0319347678693356,
24.3732258462295));
#47179=CARTESIAN_POINT('Ctrl Pts',(31.5036442008573,0.165759327603677,24.3842088515336));
#47180=CARTESIAN_POINT('Ctrl Pts',(31.4119825510711,0.540750850840327,24.4050417139356));
#47181=CARTESIAN_POINT('Ctrl Pts',(31.3322181025457,0.715044299742208,24.4140993016492));
#47182=CARTESIAN_POINT('Ctrl Pts',(31.106713322535,1.03186525150623,24.4337494874295));
#47183=CARTESIAN_POINT('Ctrl Pts',(30.9603062459911,1.1693383575936,24.4446121985753));
#47184=CARTESIAN_POINT('Ctrl Pts',(30.6267827077052,1.37647673516795,24.4664127011144));
#47185=CARTESIAN_POINT('Ctrl Pts',(30.4439056234701,1.4458581458551,24.47713864034));
#47186=CARTESIAN_POINT('Ctrl Pts',(30.0630400763872,1.51099956140736,24.4972725262831));
#47187=CARTESIAN_POINT('Ctrl Pts',(29.8687484810349,1.50660828894347,24.5061312780688));
#47188=CARTESIAN_POINT('Ctrl Pts',(29.4860566158504,1.4231980920111,24.526860498932));
#47189=CARTESIAN_POINT('Ctrl Pts',(29.3019333862064,1.34250650777999,24.5379605648438));
#47190=CARTESIAN_POINT('Ctrl Pts',(28.9821049580114,1.11829253966791,24.5595764830508));
#47191=CARTESIAN_POINT('Ctrl Pts',(28.8477437066725,0.979293286040407,24.5699020321484));
#47192=CARTESIAN_POINT('Ctrl Pts',(28.6345240475922,0.651988290747904,24.5892523732038));
#47193=CARTESIAN_POINT('Ctrl Pts',(28.5601403785395,0.465238374198666,24.5991534236556));
#47194=CARTESIAN_POINT('Ctrl Pts',(28.489084947481,0.0759965520384366,24.6207779693312));
#47195=CARTESIAN_POINT('Ctrl Pts',(28.4921379080883,-0.122445995567395,
24.6318025553093));
#47196=CARTESIAN_POINT('Ctrl Pts',(28.5732141775453,-0.500358663169468,
24.6527977035094));
#47197=CARTESIAN_POINT('Ctrl Pts',(28.6479534934179,-0.676775662247645,
24.662082289407));
#47198=CARTESIAN_POINT('Ctrl Pts',(28.8642453292122,-0.999806026462223,
24.6814617008812));
#47199=CARTESIAN_POINT('Ctrl Pts',(29.0066425215227,-1.1413892524153,24.6922456563782));
#47200=CARTESIAN_POINT('Ctrl Pts',(29.3345224631394,-1.35826808429126,24.7140451994209));
#47201=CARTESIAN_POINT('Ctrl Pts',(29.515884916708,-1.43296761407463,24.7248459914751));
#47202=CARTESIAN_POINT('Ctrl Pts',(29.8033393621129,-1.4903304156034,24.7402695610815));
#47203=CARTESIAN_POINT('Ctrl Pts',(29.901655948172,-1.50000000000001,24.7452684196003));
#47204=CARTESIAN_POINT('Ctrl Pts',(30.,-1.50000000000001,24.75));
#47205=CARTESIAN_POINT('Ctrl Pts',(29.9999999999998,-1.50000000000001,24.8125));
#47206=CARTESIAN_POINT('Ctrl Pts',(29.9520844763832,-1.50000000000001,24.8101946632951));
#47207=CARTESIAN_POINT('Ctrl Pts',(29.9041155058213,-1.49770423456202,24.8078229838607));
#47208=CARTESIAN_POINT('Ctrl Pts',(29.6647429412583,-1.47465918202179,24.7956660256301));
#47209=CARTESIAN_POINT('Ctrl Pts',(29.4785801635781,-1.4195491435244,24.7851784304102));
#47210=CARTESIAN_POINT('Ctrl Pts',(29.1305308217309,-1.23854895841351,24.7634051157232));
#47211=CARTESIAN_POINT('Ctrl Pts',(28.9733425780824,-1.11174127780071,24.752319957252));
#47212=CARTESIAN_POINT('Ctrl Pts',(28.7235507953419,-0.81069913235786,24.7319395626836));
#47213=CARTESIAN_POINT('Ctrl Pts',(28.6307275649839,-0.641599855569549,
24.7231444364205));
#47214=CARTESIAN_POINT('Ctrl Pts',(28.5125127288929,-0.274334472746556,
24.7027408040415));
#47215=CARTESIAN_POINT('Ctrl Pts',(28.4895069858667,-0.0792389156648355,
24.6919021619814));
#47216=CARTESIAN_POINT('Ctrl Pts',(28.5196116095794,0.313003938746328,24.6701108922919));
#47217=CARTESIAN_POINT('Ctrl Pts',(28.5740816740222,0.506262436197778,24.6593743091001));
#47218=CARTESIAN_POINT('Ctrl Pts',(28.7511791399573,0.852358280491469,24.640146762195));
#47219=CARTESIAN_POINT('Ctrl Pts',(28.8690245914396,1.00348928998653,24.630706043882));
#47220=CARTESIAN_POINT('Ctrl Pts',(29.1601188576535,1.25831795738381,24.6096221903744));
#47221=CARTESIAN_POINT('Ctrl Pts',(29.3323550489326,1.35757677634782,24.5985782833421));
#47222=CARTESIAN_POINT('Ctrl Pts',(29.7064392762191,1.4842685830248,24.577060930713));
#47223=CARTESIAN_POINT('Ctrl Pts',(29.9047304118308,1.51001063736079,24.5673617334579));
#47224=CARTESIAN_POINT('Ctrl Pts',(30.2937060245362,1.48342562743484,24.547908663068));
#47225=CARTESIAN_POINT('Ctrl Pts',(30.4808263548115,1.43373651283452,24.5375255787967));
#47226=CARTESIAN_POINT('Ctrl Pts',(30.8329282215013,1.26331849859809,24.5158512361083));
#47227=CARTESIAN_POINT('Ctrl Pts',(30.9932828024692,1.14155315563778,24.5047538020966));
#47228=CARTESIAN_POINT('Ctrl Pts',(31.2521599269974,0.847929325410954,24.4841423531291));
#47229=CARTESIAN_POINT('Ctrl Pts',(31.3503160471837,0.680833771104865,24.4753240983947));
#47230=CARTESIAN_POINT('Ctrl Pts',(31.4789636487266,0.316753550496772,24.455097419472));
#47231=CARTESIAN_POINT('Ctrl Pts',(31.5074931621648,0.122957581810777,24.4443309767673));
#47232=CARTESIAN_POINT('Ctrl Pts',(31.4889302469637,-0.269482846800126,
24.4225287307333));
#47233=CARTESIAN_POINT('Ctrl Pts',(31.4401374224707,-0.464284058469581,
24.4117064411961));
#47234=CARTESIAN_POINT('Ctrl Pts',(31.2732400969951,-0.815428064678723,
24.3921984408512));
#47235=CARTESIAN_POINT('Ctrl Pts',(31.1598920572171,-0.96991270557316,24.3830299796895));
#47236=CARTESIAN_POINT('Ctrl Pts',(30.8768520990815,-1.23274788918355,24.3621112360319));
#47237=CARTESIAN_POINT('Ctrl Pts',(30.7081704356177,-1.33679806788068,24.351105252973));
#47238=CARTESIAN_POINT('Ctrl Pts',(30.3563528915165,-1.46803396077468,24.330532982021));
#47239=CARTESIAN_POINT('Ctrl Pts',(30.1788031709794,-1.50000000000002,24.3211026715747));
#47240=CARTESIAN_POINT('Ctrl Pts',(29.9999999999999,-1.50000000000001,24.3125));
#47241=CARTESIAN_POINT('Origin',(30.,-1.32966554433622E-14,16.));
#47242=CARTESIAN_POINT('',(29.9999999999999,-1.50000000000001,23.75));
#47243=CARTESIAN_POINT('',(30.,-1.50000000000001,23.8125));
#47244=CARTESIAN_POINT('',(30.,-1.50000000000001,16.));
#47245=CARTESIAN_POINT('Ctrl Pts',(29.9999999999998,-1.50000000000001,23.75));
#47246=CARTESIAN_POINT('Ctrl Pts',(30.1539214445734,-1.50000000000004,23.7574055489549));
#47247=CARTESIAN_POINT('Ctrl Pts',(30.3071622224275,-1.47631426128188,23.7654362865035));
#47248=CARTESIAN_POINT('Ctrl Pts',(30.6423330661034,-1.36978679250727,23.7845212975935));
#47249=CARTESIAN_POINT('Ctrl Pts',(30.8166966283757,-1.27354330571266,23.7955837985834));
#47250=CARTESIAN_POINT('Ctrl Pts',(31.1127372375018,-1.02370190976136,23.8167670978074));
#47251=CARTESIAN_POINT('Ctrl Pts',(31.2333636655921,-0.874601042154043,
23.8264110532137));
#47252=CARTESIAN_POINT('Ctrl Pts',(31.4166526755054,-0.531631844802988,
23.8454648975109));
#47253=CARTESIAN_POINT('Ctrl Pts',(31.4745582697856,-0.339396978512901,
23.8561446123048));
#47254=CARTESIAN_POINT('Ctrl Pts',(31.511699941184,0.0525578729813968,23.8779198818323));
#47255=CARTESIAN_POINT('Ctrl Pts',(31.4920858025539,0.248369535334408,23.8887983075186));
#47256=CARTESIAN_POINT('Ctrl Pts',(31.3802343334373,0.617537171179423,23.909307620621));
#47257=CARTESIAN_POINT('Ctrl Pts',(31.2906053859832,0.78786629286171,23.9181242275504));
#47258=CARTESIAN_POINT('Ctrl Pts',(31.0463195284336,1.0933231170364,23.9383623481344));
#47259=CARTESIAN_POINT('Ctrl Pts',(30.8911113639651,1.22312916938911,23.9494355281055));
#47260=CARTESIAN_POINT('Ctrl Pts',(30.5456512461468,1.41045613992281,23.9712600127329));
#47261=CARTESIAN_POINT('Ctrl Pts',(30.3601397930707,1.4688221637187,23.9818067151192));
#47262=CARTESIAN_POINT('Ctrl Pts',(29.9746198000426,1.51244309002935,24.0015667468295));
#47263=CARTESIAN_POINT('Ctrl Pts',(29.7781833324316,1.4963071428617,24.0107747387592));
#47264=CARTESIAN_POINT('Ctrl Pts',(29.3999877237922,1.38893180194388,24.0319533318226));
#47265=CARTESIAN_POINT('Ctrl Pts',(29.222220687541,1.29776778429998,24.0430384861654));
#47266=CARTESIAN_POINT('Ctrl Pts',(28.9180417312452,1.05625627096343,24.0643819561719));
#47267=CARTESIAN_POINT('Ctrl Pts',(28.7928010889864,0.910453809129913,24.0744192328261));
#47268=CARTESIAN_POINT('Ctrl Pts',(28.5994385143727,0.572669994103534,24.0931850003275));
#47269=CARTESIAN_POINT('Ctrl Pts',(28.5359684061524,0.382240685005912,24.1037644063885));
#47270=CARTESIAN_POINT('Ctrl Pts',(28.4873420883061,-0.00897112678811804,
24.1254983959326));
#47271=CARTESIAN_POINT('Ctrl Pts',(28.5013820601517,-0.205827079960202,
24.1364348377755));
#47272=CARTESIAN_POINT('Ctrl Pts',(28.6028303892674,-0.578036208077185,
24.1571131226709));
#47273=CARTESIAN_POINT('Ctrl Pts',(28.6873275910153,-0.750394994115161,
24.1660216580016));
#47274=CARTESIAN_POINT('Ctrl Pts',(28.922674074919,-1.0628953635868,24.1860253368065));
#47275=CARTESIAN_POINT('Ctrl Pts',(29.0745736829203,-1.19747470970914,24.197071925274));
#47276=CARTESIAN_POINT('Ctrl Pts',(29.4156235588556,-1.39492862582615,24.2189655260838));
#47277=CARTESIAN_POINT('Ctrl Pts',(29.5999664963488,-1.45853020454807,24.2296014403193));
#47278=CARTESIAN_POINT('Ctrl Pts',(29.8606029709014,-1.49514680076604,24.2431584462207));
#47279=CARTESIAN_POINT('Ctrl Pts',(29.9303308703141,-1.50000000000001,24.2466480424351));
#47280=CARTESIAN_POINT('Ctrl Pts',(29.9999999999999,-1.50000000000001,24.25));
#47281=CARTESIAN_POINT('Ctrl Pts',(29.9999999999999,-1.50000000000001,24.3125));
#47282=CARTESIAN_POINT('Ctrl Pts',(29.9792133017942,-1.50000000000001,24.3114998995163));
#47283=CARTESIAN_POINT('Ctrl Pts',(29.9584107993835,-1.49956791710601,24.3104870363498));
#47284=CARTESIAN_POINT('Ctrl Pts',(29.7464034347025,-1.4907415866322,24.3000416514142));
#47285=CARTESIAN_POINT('Ctrl Pts',(29.5585103106211,-1.44626636462019,24.2897662164333));
#47286=CARTESIAN_POINT('Ctrl Pts',(29.2028124426411,-1.28608329400307,24.2682031650416));
#47287=CARTESIAN_POINT('Ctrl Pts',(29.0395645726164,-1.16922656097766,24.2571028778712));
#47288=CARTESIAN_POINT('Ctrl Pts',(28.7720346147835,-0.882829614311603,
24.2362758660328));
#47289=CARTESIAN_POINT('Ctrl Pts',(28.6687223598358,-0.717623891574991,
24.2273679939764));
#47290=CARTESIAN_POINT('Ctrl Pts',(28.5302095932634,-0.356628416668571,
24.2073126898149));
#47291=CARTESIAN_POINT('Ctrl Pts',(28.4965070465723,-0.164202501526158,
24.1966223611959));
#47292=CARTESIAN_POINT('Ctrl Pts',(28.504169008249,0.22811087427228,24.1748271736516));
#47293=CARTESIAN_POINT('Ctrl Pts',(28.547551398078,0.424213342298486,24.1639325920946));
#47294=CARTESIAN_POINT('Ctrl Pts',(28.7047478969298,0.780036844220854,24.1441646197656));
#47295=CARTESIAN_POINT('Ctrl Pts',(28.8139070776359,0.937725434330763,24.1351846602695));
#47296=CARTESIAN_POINT('Ctrl Pts',(29.089396967151,1.20794416549895,24.1144240709145));
#47297=CARTESIAN_POINT('Ctrl Pts',(29.2546507832928,1.31634974323744,24.10346202693));
#47298=CARTESIAN_POINT('Ctrl Pts',(29.6203184116569,1.46471395475137,24.0817476068599));
#47299=CARTESIAN_POINT('Ctrl Pts',(29.817562104219,1.50206749812624,24.0713349778568));
#47300=CARTESIAN_POINT('Ctrl Pts',(30.2070481745296,1.49784204922514,24.0524784469813));
#47301=CARTESIAN_POINT('Ctrl Pts',(30.3956551706626,1.45939464529562,24.0423361052064));
#47302=CARTESIAN_POINT('Ctrl Pts',(30.7551447714595,1.31111335433136,24.0209212289748));
#47303=CARTESIAN_POINT('Ctrl Pts',(30.9215534250012,1.20000288285394,24.0098284869129));
#47304=CARTESIAN_POINT('Ctrl Pts',(31.1989915137811,0.922095691461922,23.9887605964375));
#47305=CARTESIAN_POINT('Ctrl Pts',(31.3083178283937,0.759038041694919,23.9796687800942));
#47306=CARTESIAN_POINT('Ctrl Pts',(31.4580557742773,0.401642541393168,23.9598134745218));
#47307=CARTESIAN_POINT('Ctrl Pts',(31.4975752946798,0.210938880716583,23.9492188267065));
#47308=CARTESIAN_POINT('Ctrl Pts',(31.5023006219625,-0.182594498957542,
23.927355861169));
#47309=CARTESIAN_POINT('Ctrl Pts',(31.4644403140633,-0.381679718202,23.916295571211));
#47310=CARTESIAN_POINT('Ctrl Pts',(31.3164762945118,-0.74375638752885,23.8961802006929));
#47311=CARTESIAN_POINT('Ctrl Pts',(31.2115088567194,-0.904729197971778,
23.8873240471024));
#47312=CARTESIAN_POINT('Ctrl Pts',(30.9436055459159,-1.18225533242814,23.8667254837612));
#47313=CARTESIAN_POINT('Ctrl Pts',(30.7818828902994,-1.29490194314203,23.8558155263452));
#47314=CARTESIAN_POINT('Ctrl Pts',(30.4211554702292,-1.45331769745592,23.8340595826352));
#47315=CARTESIAN_POINT('Ctrl Pts',(30.225061216149,-1.49628795964726,23.8234313750427));
#47316=CARTESIAN_POINT('Ctrl Pts',(30.01751075903,-1.49992336974507,23.8133446154048));
#47317=CARTESIAN_POINT('Ctrl Pts',(30.0087538759465,-1.50000000000001,23.8129211710528));
#47318=CARTESIAN_POINT('Ctrl Pts',(30.,-1.50000000000001,23.8125));
#47319=CARTESIAN_POINT('Origin',(30.,-1.32966554433622E-14,16.));
#47320=CARTESIAN_POINT('',(30.,-1.50000000000001,23.25));
#47321=CARTESIAN_POINT('',(30.0000000000001,-1.50000000000001,23.3125));
#47322=CARTESIAN_POINT('',(30.,-1.50000000000001,16.));
#47323=CARTESIAN_POINT('Ctrl Pts',(30.,-1.50000000000001,23.25));
#47324=CARTESIAN_POINT('Ctrl Pts',(30.1848807806478,-1.50000000000001,23.2588950807062));
#47325=CARTESIAN_POINT('Ctrl Pts',(30.3682821495602,-1.46581977714696,23.268668433817));
#47326=CARTESIAN_POINT('Ctrl Pts',(30.7253175152828,-1.32777981441322,23.2896807492688));
#47327=CARTESIAN_POINT('Ctrl Pts',(30.8938177244611,-1.22072861570022,23.3007613637715));
#47328=CARTESIAN_POINT('Ctrl Pts',(31.17812266521,-0.948849031570725,23.3219922022812));
#47329=CARTESIAN_POINT('Ctrl Pts',(31.2916923057403,-0.787278580688064,
23.3312623010729));
#47330=CARTESIAN_POINT('Ctrl Pts',(31.4491725851422,-0.432421790169133,
23.3509765672128));
#47331=CARTESIAN_POINT('Ctrl Pts',(31.4926555401856,-0.243004803835009,
23.3614997331203));
#47332=CARTESIAN_POINT('Ctrl Pts',(31.5058959055076,0.149477495401521,23.3833043053001));
#47333=CARTESIAN_POINT('Ctrl Pts',(31.4725342594551,0.348889338242185,23.3943827410135));
#47334=CARTESIAN_POINT('Ctrl Pts',(31.3327988700423,0.714215497781599,23.4146786387656));
#47335=CARTESIAN_POINT('Ctrl Pts',(31.2311812032015,0.877867947558743,23.4234833208414));
#47336=CARTESIAN_POINT('Ctrl Pts',(30.9693523131294,1.16116792111582,23.4439500128983));
#47337=CARTESIAN_POINT('Ctrl Pts',(30.8105149834806,1.27711053175663,23.4548127055575));
#47338=CARTESIAN_POINT('Ctrl Pts',(30.4538126686857,1.44345770015622,23.4765953083576));
#47339=CARTESIAN_POINT('Ctrl Pts',(30.2587086794859,1.49084210066152,23.487298486762));
#47340=CARTESIAN_POINT('Ctrl Pts',(29.8701963712835,1.50640033026212,23.5064229669502));
#47341=CARTESIAN_POINT('Ctrl Pts',(29.6806119299331,1.47787523708767,23.5159811423084));
#47342=CARTESIAN_POINT('Ctrl Pts',(29.3158918902727,1.34932104216597,23.5370996932649));
#47343=CARTESIAN_POINT('Ctrl Pts',(29.1450773397405,1.24811033609704,23.5481294207781));
#47344=CARTESIAN_POINT('Ctrl Pts',(28.8572342555358,0.990033097118328,23.5691470898178));
#47345=CARTESIAN_POINT('Ctrl Pts',(28.741208429162,0.837555866674711,23.578469118518));
#47346=CARTESIAN_POINT('Ctrl Pts',(28.5682103547001,0.489415671302002,23.5978102404832));
#47347=CARTESIAN_POINT('Ctrl Pts',(28.5160198061383,0.295515658346084,23.6085824634252));
#47348=CARTESIAN_POINT('Ctrl Pts',(28.4905622848027,-0.0968477988030621,
23.6303804332668));
#47349=CARTESIAN_POINT('Ctrl Pts',(28.5157978904665,-0.291438773395986,
23.6411910429664));
#47350=CARTESIAN_POINT('Ctrl Pts',(28.6382130227664,-0.657431308298791,
23.6615239615721));
#47351=CARTESIAN_POINT('Ctrl Pts',(28.733169022031,-0.825722839750627,23.6703196450362));
#47352=CARTESIAN_POINT('Ctrl Pts',(28.9866100524997,-1.12380536152502,23.6907934023492));
#47353=CARTESIAN_POINT('Ctrl Pts',(29.1450855427347,-1.24860164286396,23.7018846212987));
#47354=CARTESIAN_POINT('Ctrl Pts',(29.4947960835532,-1.42537206508902,23.723620367045));
#47355=CARTESIAN_POINT('Ctrl Pts',(29.6813612118254,-1.47831159941945,23.7340670285844));
#47356=CARTESIAN_POINT('Ctrl Pts',(29.9152096611065,-1.49820471212254,23.7458706538102));
#47357=CARTESIAN_POINT('Ctrl Pts',(29.957628226374,-1.50000000000001,23.7479613870909));
#47358=CARTESIAN_POINT('Ctrl Pts',(29.9999999999998,-1.50000000000001,23.75));
#47359=CARTESIAN_POINT('Ctrl Pts',(30.,-1.50000000000001,23.8125));
#47360=CARTESIAN_POINT('Ctrl Pts',(29.8186899108673,-1.50000000000001,23.8037767142694));
#47361=CARTESIAN_POINT('Ctrl Pts',(29.6387564217711,-1.46712852254306,23.7942065636429));
#47362=CARTESIAN_POINT('Ctrl Pts',(29.284195027604,-1.33291119731626,23.7734194615783));
#47363=CARTESIAN_POINT('Ctrl Pts',(29.1150531352934,-1.22715164870581,23.762343853251));
#47364=CARTESIAN_POINT('Ctrl Pts',(28.8285848658366,-0.957196675383623,
23.7410623929517));
#47365=CARTESIAN_POINT('Ctrl Pts',(28.713664846415,-0.796095622176884,23.7317275345654));
#47366=CARTESIAN_POINT('Ctrl Pts',(28.5537507892143,-0.442046290271719,
23.7120581272374));
#47367=CARTESIAN_POINT('Ctrl Pts',(28.50903084701,-0.253050072432249,23.7015583373574));
#47368=CARTESIAN_POINT('Ctrl Pts',(28.493125704307,0.139065210502765,23.6797741549721));
#47369=CARTESIAN_POINT('Ctrl Pts',(28.5250759127101,0.338559440554235,23.6686911421915));
#47370=CARTESIAN_POINT('Ctrl Pts',(28.6622225705316,0.704891738980156,23.6483393478345));
#47371=CARTESIAN_POINT('Ctrl Pts',(28.7627930544851,0.869391639366899,23.6395420458263));
#47372=CARTESIAN_POINT('Ctrl Pts',(29.0227223626785,1.15448356589741,23.6191169709735));
#47373=CARTESIAN_POINT('Ctrl Pts',(29.1806474642266,1.27143845898823,23.6082700489523));
#47374=CARTESIAN_POINT('Ctrl Pts',(29.5360600403599,1.4402358268239,23.5864814376371));
#47375=CARTESIAN_POINT('Ctrl Pts',(29.7308346201,1.48899068833401,23.5757560395914));
#47376=CARTESIAN_POINT('Ctrl Pts',(30.1191927262396,1.50727161649964,23.5565633479378));
#47377=CARTESIAN_POINT('Ctrl Pts',(30.3089226794933,1.48009155403507,23.5470839383266));
#47378=CARTESIAN_POINT('Ctrl Pts',(30.6746275130695,1.35410584970156,23.5259893534154));
#47379=CARTESIAN_POINT('Ctrl Pts',(30.8462644331352,1.25401826984556,23.5149512576394));
#47380=CARTESIAN_POINT('Ctrl Pts',(31.1359831388577,0.997812339501797,23.4938953285128));
#47381=CARTESIAN_POINT('Ctrl Pts',(31.2530579642409,0.846112941875841,23.4845062745487));
#47382=CARTESIAN_POINT('Ctrl Pts',(31.4284239202414,0.499151075957345,23.465230615331));
#47383=CARTESIAN_POINT('Ctrl Pts',(31.4819315716114,0.305618089705,23.4544787827614));
#47384=CARTESIAN_POINT('Ctrl Pts',(31.5100720569101,-0.086682490418841,
23.4326843060879));
#47385=CARTESIAN_POINT('Ctrl Pts',(31.4861228872238,-0.281567854400411,
23.4218573414222));
#47386=CARTESIAN_POINT('Ctrl Pts',(31.3661326726942,-0.648296896097567,
23.4014835057724));
#47387=CARTESIAN_POINT('Ctrl Pts',(31.2724103712455,-0.817054396960877,
23.3926895837254));
#47388=CARTESIAN_POINT('Ctrl Pts',(31.0210775409326,-1.11685004948265,23.3722696702745));
#47389=CARTESIAN_POINT('Ctrl Pts',(30.8633432283804,-1.24281066274781,23.3611817686994));
#47390=CARTESIAN_POINT('Ctrl Pts',(30.5145869816219,-1.42202815813894,23.3394239621929));
#47391=CARTESIAN_POINT('Ctrl Pts',(30.3282514191413,-1.47622279958149,23.3289534815563));
#47392=CARTESIAN_POINT('Ctrl Pts',(30.0912045055574,-1.4979228580024,23.3169457772084));
#47393=CARTESIAN_POINT('Ctrl Pts',(30.0455768509778,-1.50000000000001,23.3146928172651));
#47394=CARTESIAN_POINT('Ctrl Pts',(30.0000000000002,-1.50000000000001,23.3125));
#47395=CARTESIAN_POINT('Origin',(30.,-1.32966554433622E-14,16.));
#47396=CARTESIAN_POINT('',(30.0000000000001,-1.50000000000001,22.75));
#47397=CARTESIAN_POINT('',(30.,-1.50000000000001,22.8125));
#47398=CARTESIAN_POINT('',(30.,-1.50000000000001,16.));
#47399=CARTESIAN_POINT('Ctrl Pts',(30.0000000000001,-1.50000000000001,22.75));
#47400=CARTESIAN_POINT('Ctrl Pts',(30.0238190927805,-1.50000000000001,22.7511459966357));
#47401=CARTESIAN_POINT('Ctrl Pts',(30.0476581179369,-1.49943265781826,22.7523087117734));
#47402=CARTESIAN_POINT('Ctrl Pts',(30.2627622738244,-1.48916810759789,22.7629430416939));
#47403=CARTESIAN_POINT('Ctrl Pts',(30.4504917710081,-1.44350305068679,22.7732436551414));
#47404=CARTESIAN_POINT('Ctrl Pts',(30.8053949324493,-1.28097942369943,22.7948334866517));
#47405=CARTESIAN_POINT('Ctrl Pts',(30.9679955997388,-1.16299746502374,22.8059338915341));
#47406=CARTESIAN_POINT('Ctrl Pts',(31.2335580340327,-0.874942371993705,
22.8267123004732));
#47407=CARTESIAN_POINT('Ctrl Pts',(31.3356903480274,-0.709308500806453,
22.8355939721774));
#47408=CARTESIAN_POINT('Ctrl Pts',(31.4719653898389,-0.347606806174152,
22.8556885107681));
#47409=CARTESIAN_POINT('Ctrl Pts',(31.5044992018676,-0.154858219876142,
22.8663967655625));
#47410=CARTESIAN_POINT('Ctrl Pts',(31.4943665307067,0.237510688978279,22.8881950382766));
#47411=CARTESIAN_POINT('Ctrl Pts',(31.4497537465181,0.433331528903234,22.899073973828));
#47412=CARTESIAN_POINT('Ctrl Pts',(31.2903519524536,0.78810181728577,22.9187834342937));
#47413=CARTESIAN_POINT('Ctrl Pts',(31.1802475750943,0.945060620681391,22.9278003293086));
#47414=CARTESIAN_POINT('Ctrl Pts',(30.9030507590494,1.21362000516214,22.948596950241));
#47415=CARTESIAN_POINT('Ctrl Pts',(30.7370141991215,1.32105257322674,22.9595696259569));
#47416=CARTESIAN_POINT('Ctrl Pts',(30.3702805499944,1.46712017353723,22.9812715402192));
#47417=CARTESIAN_POINT('Ctrl Pts',(30.1727871861063,1.50321114583692,22.991597574137));
#47418=CARTESIAN_POINT('Ctrl Pts',(29.7831928098337,1.49647610979574,23.0105290266394));
#47419=CARTESIAN_POINT('Ctrl Pts',(29.5947193673977,1.45676699750561,23.0206999902635));
#47420=CARTESIAN_POINT('Ctrl Pts',(29.2359911149794,1.30598838211349,23.0421476062271));
#47421=CARTESIAN_POINT('Ctrl Pts',(29.0702277888966,1.19366882317697,23.05324288572));
#47422=CARTESIAN_POINT('Ctrl Pts',(28.7948557226535,0.913971635465609,23.0742610967597));
#47423=CARTESIAN_POINT('Ctrl Pts',(28.686793719435,0.750466721324838,23.0833074043708));
#47424=CARTESIAN_POINT('Ctrl Pts',(28.5393908078851,0.39231449396832,23.1032047503351));
#47425=CARTESIAN_POINT('Ctrl Pts',(28.50107471408,0.201238476218244,23.1138200846545));
#47426=CARTESIAN_POINT('Ctrl Pts',(28.4989279287216,-0.192576857122968,
23.1356987142846));
#47427=CARTESIAN_POINT('Ctrl Pts',(28.5381471159066,-0.391544240809387,
23.1467524578227));
#47428=CARTESIAN_POINT('Ctrl Pts',(28.6885908974138,-0.752626531003943,
23.1668125850557));
#47429=CARTESIAN_POINT('Ctrl Pts',(28.7945746463293,-0.912795946069086,
23.1756927219105));
#47430=CARTESIAN_POINT('Ctrl Pts',(29.0643193882896,-1.1885583990927,23.1963308899987));
#47431=CARTESIAN_POINT('Ctrl Pts',(29.2269067570048,-1.30018824275338,23.2072542074138));
#47432=CARTESIAN_POINT('Ctrl Pts',(29.5888237919401,-1.45617120236401,23.228999808865));
#47433=CARTESIAN_POINT('Ctrl Pts',(29.7851989650319,-1.49779418034797,23.2396041076185));
#47434=CARTESIAN_POINT('Ctrl Pts',(29.9893352495882,-1.49997157194577,23.2494861022884));
#47435=CARTESIAN_POINT('Ctrl Pts',(29.9946682024469,-1.50000000000001,23.2497434737706));
#47436=CARTESIAN_POINT('Ctrl Pts',(30.,-1.50000000000001,23.25));
#47437=CARTESIAN_POINT('Ctrl Pts',(30.0000000000003,-1.50000000000001,23.3125));
#47438=CARTESIAN_POINT('Ctrl Pts',(29.8497176527518,-1.50000000000002,23.3052695371968));
#47439=CARTESIAN_POINT('Ctrl Pts',(29.7000480379928,-1.47742120454004,23.2974413657365));
#47440=CARTESIAN_POINT('Ctrl Pts',(29.3674490033452,-1.37435151569836,23.2785761403087));
#47441=CARTESIAN_POINT('Ctrl Pts',(29.1922818901849,-1.27927791742795,23.2675074753621));
#47442=CARTESIAN_POINT('Ctrl Pts',(28.8943459539799,-1.03136235914611,23.2462864826624));
#47443=CARTESIAN_POINT('Ctrl Pts',(28.7726494682524,-0.883034040962408,
23.2365574467202));
#47444=CARTESIAN_POINT('Ctrl Pts',(28.5870020748245,-0.541267982453404,
23.2175704434697));
#47445=CARTESIAN_POINT('Ctrl Pts',(28.5277906685824,-0.349440299767995,
23.2069133499871));
#47446=CARTESIAN_POINT('Ctrl Pts',(28.487963650694,0.0423711662580389,23.185146046319));
#47447=CARTESIAN_POINT('Ctrl Pts',(28.5062787794266,0.238440842104816,23.1742532865498));
#47448=CARTESIAN_POINT('Ctrl Pts',(28.6157002622386,0.608326552071247,23.1537040804405));
#47449=CARTESIAN_POINT('Ctrl Pts',(28.704120723826,0.779127514930934,23.1448722564411));
#47450=CARTESIAN_POINT('Ctrl Pts',(28.9463114752997,1.08624863564316,23.1246887062359));
#47451=CARTESIAN_POINT('Ctrl Pts',(29.100754465216,1.21718400346422,23.1136209708684));
#47452=CARTESIAN_POINT('Ctrl Pts',(29.4452036060534,1.40690072974557,23.0917787447896));
#47453=CARTESIAN_POINT('Ctrl Pts',(29.630453412942,1.46649956876065,23.0812103859941));
#47454=CARTESIAN_POINT('Ctrl Pts',(30.0154678344856,1.51253258675255,23.0614076760565));
#47455=CARTESIAN_POINT('Ctrl Pts',(30.2116518417758,1.49773354664468,23.052253938977));
#47456=CARTESIAN_POINT('Ctrl Pts',(30.5903886500576,1.39306917025536,23.031124612004));
#47457=CARTESIAN_POINT('Ctrl Pts',(30.7689034771477,1.3030667277533,23.0200357455338));
#47458=CARTESIAN_POINT('Ctrl Pts',(31.0748241700176,1.06351798971685,22.9986629977234));
#47459=CARTESIAN_POINT('Ctrl Pts',(31.2011381587389,0.918481956232081,22.9885569343996));
#47460=CARTESIAN_POINT('Ctrl Pts',(31.3967520547264,0.581861797904625,22.9697948964873));
#47461=CARTESIAN_POINT('Ctrl Pts',(31.4615014415134,0.391859484339943,22.9592699713522));
#47462=CARTESIAN_POINT('Ctrl Pts',(31.5127002734739,0.000740375396987882,
22.9375411319665));
#47463=CARTESIAN_POINT('Ctrl Pts',(31.4999079686113,-0.196327016676456,
22.9265929435179));
#47464=CARTESIAN_POINT('Ctrl Pts',(31.4007804390091,-0.569202940848263,
22.9058776143973));
#47465=CARTESIAN_POINT('Ctrl Pts',(31.3174135571943,-0.742018160934012,
22.8969391404085));
#47466=CARTESIAN_POINT('Ctrl Pts',(31.0853396535684,-1.05432624095891,22.8770982550692));
#47467=CARTESIAN_POINT('Ctrl Pts',(30.9361334950341,-1.18878161757634,22.8661846988469));
#47468=CARTESIAN_POINT('Ctrl Pts',(30.5987439832112,-1.38884930936682,22.8443946025078));
#47469=CARTESIAN_POINT('Ctrl Pts',(30.4148754905707,-1.45440359104526,22.8337272732621));
#47470=CARTESIAN_POINT('Ctrl Pts',(30.1494349053273,-1.49442202191131,22.8198446340705));
#47471=CARTESIAN_POINT('Ctrl Pts',(30.0746909808563,-1.50000000000001,22.816093571492));
#47472=CARTESIAN_POINT('Ctrl Pts',(30.0000000000001,-1.50000000000001,22.8125));
#47473=CARTESIAN_POINT('Origin',(30.,-1.32966554433622E-14,16.));
#47474=CARTESIAN_POINT('',(30.0000000000001,-1.50000000000001,22.25));
#47475=CARTESIAN_POINT('',(30.,-1.50000000000001,22.3125));
#47476=CARTESIAN_POINT('',(30.,-1.50000000000001,16.));
#47477=CARTESIAN_POINT('Ctrl Pts',(30.0000000000002,-1.50000000000001,22.25));
#47478=CARTESIAN_POINT('Ctrl Pts',(30.0511677444063,-1.50000000000001,22.2524618092506));
#47479=CARTESIAN_POINT('Ctrl Pts',(30.1023921263505,-1.49738203467576,22.254999064735));
#47480=CARTESIAN_POINT('Ctrl Pts',(30.3449868915282,-1.47242953219059,22.2673640358856));
#47481=CARTESIAN_POINT('Ctrl Pts',(30.5309019965201,-1.41604718249647,22.2778750569255));
#47482=CARTESIAN_POINT('Ctrl Pts',(30.8779534991821,-1.23257211766357,22.2996691097112));
#47483=CARTESIAN_POINT('Ctrl Pts',(31.0343750352224,-1.10459007945506,22.3107500009898));
#47484=CARTESIAN_POINT('Ctrl Pts',(31.2820199524192,-0.801819415517196,
22.3310751188442));
#47485=CARTESIAN_POINT('Ctrl Pts',(31.3735944009353,-0.632242273686504,
22.3398754292397));
#47486=CARTESIAN_POINT('Ctrl Pts',(31.4893318529591,-0.264232559817084,
22.3603204133435));
#47487=CARTESIAN_POINT('Ctrl Pts',(31.511019003439,-0.0688512669519718,
22.3711749296138));
#47488=CARTESIAN_POINT('Ctrl Pts',(31.4781740542578,0.32329452926424,22.3929608071814));
#47489=CARTESIAN_POINT('Ctrl Pts',(31.422363807823,0.516161881943181,22.403675660108));
#47490=CARTESIAN_POINT('Ctrl Pts',(31.2428531453717,0.861044634974944,22.4228358130542));
#47491=CARTESIAN_POINT('Ctrl Pts',(31.1239285676202,1.01138399102137,22.4323522946618));
#47492=CARTESIAN_POINT('Ctrl Pts',(30.8309115401787,1.26428053578999,22.4534749869891));
#47493=CARTESIAN_POINT('Ctrl Pts',(30.6578432463629,1.3623737449238,22.4645265505225));
#47494=CARTESIAN_POINT('Ctrl Pts',(30.2831279004866,1.48623532989505,22.4859956505893));
#47495=CARTESIAN_POINT('Ctrl Pts',(30.0851137662052,1.5105602610331,22.49561162143));
#47496=CARTESIAN_POINT('Ctrl Pts',(29.6966286981958,1.48149502237994,22.5151099857196));
#47497=CARTESIAN_POINT('Ctrl Pts',(29.5097167303907,1.43054672747056,22.5255180223776));
#47498=CARTESIAN_POINT('Ctrl Pts',(29.1585275612845,1.25766527467259,22.547216881732));
#47499=CARTESIAN_POINT('Ctrl Pts',(28.9988940242273,1.13472310971196,22.5583123140024));
#47500=CARTESIAN_POINT('Ctrl Pts',(28.7421191463059,0.839368453848379,22.5788706970727));
#47501=CARTESIAN_POINT('Ctrl Pts',(28.6452032661271,0.671810533827306,22.5876771925652));
#47502=CARTESIAN_POINT('Ctrl Pts',(28.5189623058816,0.306989072921277,22.6079450515044));
#47503=CARTESIAN_POINT('Ctrl Pts',(28.4917024287485,0.112879611784448,22.6187289104564));
#47504=CARTESIAN_POINT('Ctrl Pts',(28.5129271256702,-0.27954553838217,22.6405303076879));
#47505=CARTESIAN_POINT('Ctrl Pts',(28.5630339289139,-0.474005993650327,
22.6513336663139));
#47506=CARTESIAN_POINT('Ctrl Pts',(28.7322894218787,-0.823994430176359,
22.6707774683431));
#47507=CARTESIAN_POINT('Ctrl Pts',(28.8466683628132,-0.977702516203741,
22.680002042295));
#47508=CARTESIAN_POINT('Ctrl Pts',(29.1315598866997,-1.23870928805523,22.7009590802358));
#47509=CARTESIAN_POINT('Ctrl Pts',(29.301068288962,-1.34167114530826,22.7119746086325));
#47510=CARTESIAN_POINT('Ctrl Pts',(29.6506233621551,-1.46928601783117,22.732337442503));
#47511=CARTESIAN_POINT('Ctrl Pts',(29.8247316115896,-1.50000000000001,22.7415673957309));
#47512=CARTESIAN_POINT('Ctrl Pts',(30.0000000000001,-1.50000000000001,22.75));
#47513=CARTESIAN_POINT('Ctrl Pts',(30.0000000000001,-1.50000000000001,22.8125));
#47514=CARTESIAN_POINT('Ctrl Pts',(29.8821180181442,-1.50000000000001,22.8068284005036));
#47515=CARTESIAN_POINT('Ctrl Pts',(29.7644054408515,-1.48610745961779,22.8007790475884));
#47516=CARTESIAN_POINT('Ctrl Pts',(29.4561358619788,-1.41197523055228,22.7838881919746));
#47517=CARTESIAN_POINT('Ctrl Pts',(29.2741386603191,-1.32762177587115,22.7727886960081));
#47518=CARTESIAN_POINT('Ctrl Pts',(28.9596308471203,-1.09734948081223,22.7512604791499));
#47519=CARTESIAN_POINT('Ctrl Pts',(28.8283658665089,-0.955949757636784,
22.7410172197375));
#47520=CARTESIAN_POINT('Ctrl Pts',(28.6210784753189,-0.623528783846783,
22.7218101845402));
#47521=CARTESIAN_POINT('Ctrl Pts',(28.550139211662,-0.43377020073728,22.7115983444854));
#47522=CARTESIAN_POINT('Ctrl Pts',(28.4878128315539,-0.0419315259951405,
22.6898295292219));
#47523=CARTESIAN_POINT('Ctrl Pts',(28.4952899772074,0.155946448584049,22.678836308412));
#47524=CARTESIAN_POINT('Ctrl Pts',(28.5845546436209,0.531607574681399,22.657966245851));
#47525=CARTESIAN_POINT('Ctrl Pts',(28.6631729955745,0.706378968214403,22.6488631478995));
#47526=CARTESIAN_POINT('Ctrl Pts',(28.886581089556,1.02462509962909,22.6292742506491));
#47527=CARTESIAN_POINT('Ctrl Pts',(29.0320840520478,1.16304620087307,22.6184287055121));
#47528=CARTESIAN_POINT('Ctrl Pts',(29.3643456686259,1.37241961531272,22.5966268328521));
#47529=CARTESIAN_POINT('Ctrl Pts',(29.5468906971467,1.44301653433814,22.585883105544));
#47530=CARTESIAN_POINT('Ctrl Pts',(29.9272228832809,1.51053148619831,22.5657089493774));
#47531=CARTESIAN_POINT('Ctrl Pts',(30.1212939503538,1.50741198602448,22.5568701305933));
#47532=CARTESIAN_POINT('Ctrl Pts',(30.5044378408363,1.42661367919911,22.5361917141558));
#47533=CARTESIAN_POINT('Ctrl Pts',(30.6892182911204,1.34709011542225,22.5250924727137));
#47534=CARTESIAN_POINT('Ctrl Pts',(31.0107046879826,1.12481571216727,22.5034506622537));
#47535=CARTESIAN_POINT('Ctrl Pts',(31.1460355364563,0.986589014961116,22.4930999232927));
#47536=CARTESIAN_POINT('Ctrl Pts',(31.3611183370781,0.66090197936205,22.473704885123));
#47537=CARTESIAN_POINT('Ctrl Pts',(31.4365760335144,0.475089538086611,22.463893863227));
#47538=CARTESIAN_POINT('Ctrl Pts',(31.5103576978905,0.0866802952431828,
22.4423155719579));
#47539=CARTESIAN_POINT('Ctrl Pts',(31.5086976507443,-0.111919508747406,
22.431282249514));
#47540=CARTESIAN_POINT('Ctrl Pts',(31.4301969979147,-0.490528747223499,
22.410248402932));
#47541=CARTESIAN_POINT('Ctrl Pts',(31.3566667795852,-0.667467593155736,
22.4008985610562));
#47542=CARTESIAN_POINT('Ctrl Pts',(31.1425983489439,-0.991976419659515,
22.3815850548154));
#47543=CARTESIAN_POINT('Ctrl Pts',(31.0011829334274,-1.13452992378446,22.370821382905));
#47544=CARTESIAN_POINT('Ctrl Pts',(30.6747026750166,-1.35372782384191,22.3490247635913));
#47545=CARTESIAN_POINT('Ctrl Pts',(30.4937271061129,-1.42970164427305,22.3382071885718));
#47546=CARTESIAN_POINT('Ctrl Pts',(30.2032733713701,-1.48966742655325,22.322567010569));
#47547=CARTESIAN_POINT('Ctrl Pts',(30.1016602333963,-1.50000000000001,22.3173911302598));
#47548=CARTESIAN_POINT('Ctrl Pts',(30.,-1.50000000000001,22.3125));
#47549=CARTESIAN_POINT('Origin',(30.,-1.32966554433622E-14,16.));
#47550=CARTESIAN_POINT('',(30.,-1.50000000000001,21.75));
#47551=CARTESIAN_POINT('',(29.9999999999999,-1.50000000000001,21.8125));
#47552=CARTESIAN_POINT('',(30.,-1.50000000000001,16.));
#47553=CARTESIAN_POINT('Ctrl Pts',(30.,-1.50000000000001,21.75));
#47554=CARTESIAN_POINT('Ctrl Pts',(30.0799345840677,-1.50000000000001,21.7538458544691));
#47555=CARTESIAN_POINT('Ctrl Pts',(30.1599122998412,-1.4936114408734,21.7578712440892));
#47556=CARTESIAN_POINT('Ctrl Pts',(30.4303228176761,-1.44993500309235,21.7720946105773));
#47557=CARTESIAN_POINT('Ctrl Pts',(30.6136742893428,-1.38234553687229,21.7827935975436));
#47558=CARTESIAN_POINT('Ctrl Pts',(30.9490281775211,-1.17851150378185,21.8045903754862));
#47559=CARTESIAN_POINT('Ctrl Pts',(31.096754819913,-1.04244516916321,21.8154774972882));
#47560=CARTESIAN_POINT('Ctrl Pts',(31.3253413942278,-0.727732251316939,
21.8352173994684));
#47561=CARTESIAN_POINT('Ctrl Pts',(31.4067935410376,-0.554135842314364,
21.8442146754271));
#47562=CARTESIAN_POINT('Ctrl Pts',(31.5019658936778,-0.180133518226551,
21.8649925823208));
#47563=CARTESIAN_POINT('Ctrl Pts',(31.5126290136531,0.0172760533687308,
21.8759597807428));
#47564=CARTESIAN_POINT('Ctrl Pts',(31.457072059222,0.408029499969523,21.8976683055539));
#47565=CARTESIAN_POINT('Ctrl Pts',(31.3902144216195,0.597326073407902,21.9080390017153));
#47566=CARTESIAN_POINT('Ctrl Pts',(31.1907422817111,0.931962878929858,21.9269315763413));
#47567=CARTESIAN_POINT('Ctrl Pts',(31.0626495240423,1.07572029471252,21.9370877035676));
#47568=CARTESIAN_POINT('Ctrl Pts',(30.7536327605205,1.31199280194067,21.9585184047354));
#47569=CARTESIAN_POINT('Ctrl Pts',(30.5738554020277,1.39999410781883,21.9696124276475));
#47570=CARTESIAN_POINT('Ctrl Pts',(30.1942124641512,1.50002082255712,21.9906565268663));
#47571=CARTESIAN_POINT('Ctrl Pts',(29.9984550225415,1.51253833676667,21.9997260456303));
#47572=CARTESIAN_POINT('Ctrl Pts',(29.6143176021754,1.46236614670513,22.0196015378309));
#47573=CARTESIAN_POINT('Ctrl Pts',(29.4295365026789,1.40065016331119,22.0302061554976));
#47574=CARTESIAN_POINT('Ctrl Pts',(29.0868629977602,1.20683686352092,22.052076744962));
#47575=CARTESIAN_POINT('Ctrl Pts',(28.9337539891966,1.07396976987892,22.0631339581722));
#47576=CARTESIAN_POINT('Ctrl Pts',(28.6951751765203,0.763999003449345,22.0832228857165));
#47577=CARTESIAN_POINT('Ctrl Pts',(28.60882966791,0.592379173375639,22.0920900459236));
#47578=CARTESIAN_POINT('Ctrl Pts',(28.5036090779159,0.221263029136351,22.1127076094925));
#47579=CARTESIAN_POINT('Ctrl Pts',(28.4875441317865,0.0247675363524192,
22.1236240257582));
#47580=CARTESIAN_POINT('Ctrl Pts',(28.5320098906898,-0.36675262012417,22.1453751455625));
#47581=CARTESIAN_POINT('Ctrl Pts',(28.593470220051,-0.557855368091198,22.155991964894));
#47582=CARTESIAN_POINT('Ctrl Pts',(28.7831869687067,-0.897529793649072,
22.1748627663138));
#47583=CARTESIAN_POINT('Ctrl Pts',(28.9067443386156,-1.04452569047662,22.1847486483138));
#47584=CARTESIAN_POINT('Ctrl Pts',(29.2079650540828,-1.28908351396432,22.2060344096185));
#47585=CARTESIAN_POINT('Ctrl Pts',(29.3845091949262,-1.38211075548827,22.2171124835975));
#47586=CARTESIAN_POINT('Ctrl Pts',(29.7125665428598,-1.47927872450056,22.2355952603595));
#47587=CARTESIAN_POINT('Ctrl Pts',(29.8560312883098,-1.50000000000001,22.2430733021292));
#47588=CARTESIAN_POINT('Ctrl Pts',(30.0000000000002,-1.50000000000001,22.25));
#47589=CARTESIAN_POINT('Ctrl Pts',(30.,-1.50000000000001,22.3125));
#47590=CARTESIAN_POINT('Ctrl Pts',(29.9110895843884,-1.50000000000001,22.3082222956344));
#47591=CARTESIAN_POINT('Ctrl Pts',(29.8221645100457,-1.49209634975764,22.3037243401601));
#47592=CARTESIAN_POINT('Ctrl Pts',(29.5376207680931,-1.44087704391974,22.288611464497));
#47593=CARTESIAN_POINT('Ctrl Pts',(29.3500356587678,-1.36654835932947,22.2775215860335));
#47594=CARTESIAN_POINT('Ctrl Pts',(29.0213968226607,-1.15294073825471,22.2557763976293));
#47595=CARTESIAN_POINT('Ctrl Pts',(28.8818555948118,-1.01818896609304,22.2453196123919));
#47596=CARTESIAN_POINT('Ctrl Pts',(28.6586442869874,-0.699623440719697,
22.2257313109655));
#47597=CARTESIAN_POINT('Ctrl Pts',(28.5785399664869,-0.517856468116547,
22.2162698037842));
#47598=CARTESIAN_POINT('Ctrl Pts',(28.4929509348882,-0.133169441708886,
22.1948983023171));
#47599=CARTESIAN_POINT('Ctrl Pts',(28.4885197532221,0.0660037349236151,
22.1838331258375));
#47600=CARTESIAN_POINT('Ctrl Pts',(28.555761801385,0.44759093437612,22.1626338369791));
#47601=CARTESIAN_POINT('Ctrl Pts',(28.6240637192867,0.626835313372202,22.1529543398));
#47602=CARTESIAN_POINT('Ctrl Pts',(28.8284985352011,0.957663958533704,22.1339287805455));
#47603=CARTESIAN_POINT('Ctrl Pts',(28.9656007252824,1.10432288929781,22.1232585891618));
#47604=CARTESIAN_POINT('Ctrl Pts',(29.2858531479679,1.33342212875051,22.1014865695287));
#47605=CARTESIAN_POINT('Ctrl Pts',(29.4650586076933,1.41487321083335,22.0906020127698));
#47606=CARTESIAN_POINT('Ctrl Pts',(29.8404420905807,1.50363480947233,22.0700757665663));
#47607=CARTESIAN_POINT('Ctrl Pts',(30.0326825220108,1.51172235919918,22.0612531825154));
#47608=CARTESIAN_POINT('Ctrl Pts',(30.4195266402016,1.45401546056375,22.0410381667945));
#47609=CARTESIAN_POINT('Ctrl Pts',(30.6097995465824,1.38502427774371,22.029967235573));
#47610=CARTESIAN_POINT('Ctrl Pts',(30.9454244752463,1.18038733089544,22.0081351140291));
#47611=CARTESIAN_POINT('Ctrl Pts',(31.0891246269642,1.04926948856203,21.997579174969));
#47612=CARTESIAN_POINT('Ctrl Pts',(31.3204408508467,0.737906981306312,21.9778010094235));
#47613=CARTESIAN_POINT('Ctrl Pts',(31.4051230902783,0.560097094369773,21.9686165052427));
#47614=CARTESIAN_POINT('Ctrl Pts',(31.5023434434385,0.179258057369552,21.9474587809649));
#47615=CARTESIAN_POINT('Ctrl Pts',(31.5128623034415,-0.0203042234475934,
21.9363719875862));
#47616=CARTESIAN_POINT('Ctrl Pts',(31.4568810475112,-0.404757677376984,
21.9150134623679));
#47617=CARTESIAN_POINT('Ctrl Pts',(31.3937249627295,-0.586348141727015,
21.9049348418193));
#47618=CARTESIAN_POINT('Ctrl Pts',(31.1987850558466,-0.923274808506461,
21.8861967170992));
#47619=CARTESIAN_POINT('Ctrl Pts',(31.0660220732146,-1.07382111006007,21.8756273134093));
#47620=CARTESIAN_POINT('Ctrl Pts',(30.7521571303647,-1.31243843036869,21.8538982204082));
#47621=CARTESIAN_POINT('Ctrl Pts',(30.5748417786265,-1.39921326582906,21.8429567194739));
#47622=CARTESIAN_POINT('Ctrl Pts',(30.2597272838717,-1.48309858829145,21.8254656184301));
#47623=CARTESIAN_POINT('Ctrl Pts',(30.1300238421579,-1.50000000000003,21.8187557750226));
#47624=CARTESIAN_POINT('Ctrl Pts',(29.9999999999998,-1.50000000000001,21.8125));
#47625=CARTESIAN_POINT('Origin',(30.,-1.32966554433622E-14,16.));
#47626=CARTESIAN_POINT('',(30.,-1.50000000000001,21.25));
#47627=CARTESIAN_POINT('',(29.9999999999999,-1.50000000000001,21.3125));
#47628=CARTESIAN_POINT('',(30.,-1.50000000000001,16.));
#47629=CARTESIAN_POINT('Ctrl Pts',(30.,-1.50000000000001,21.25));
#47630=CARTESIAN_POINT('Ctrl Pts',(30.1075848726609,-1.50000000000001,21.2551761795993));
#47631=CARTESIAN_POINT('Ctrl Pts',(30.2150815962025,-1.48842822791985,21.2606695562356));
#47632=CARTESIAN_POINT('Ctrl Pts',(30.5108359622909,-1.42370950162225,21.2766967872056));
#47633=CARTESIAN_POINT('Ctrl Pts',(30.6910987866292,-1.34546461195666,21.2875431555427));
#47634=CARTESIAN_POINT('Ctrl Pts',(31.0150386063333,-1.12214805976604,21.3093319549459));
#47635=CARTESIAN_POINT('Ctrl Pts',(31.1546840327806,-0.977879417444189,
21.3200581109451));
#47636=CARTESIAN_POINT('Ctrl Pts',(31.3647735631693,-0.650743634461253,
21.3392531532717));
#47637=CARTESIAN_POINT('Ctrl Pts',(31.4361426481554,-0.472861434650035,
21.3487299202974));
#47638=CARTESIAN_POINT('Ctrl Pts',(31.5100129878737,-0.0930141634261118,
21.3698325464765));
#47639=CARTESIAN_POINT('Ctrl Pts',(31.5091680819865,0.105843895299734,21.3808802164057));
#47640=CARTESIAN_POINT('Ctrl Pts',(31.4305088048906,0.492738271362424,21.4023743484091));
#47641=CARTESIAN_POINT('Ctrl Pts',(31.3531309016418,0.676876453829759,21.4120329161916));
#47642=CARTESIAN_POINT('Ctrl Pts',(31.1347020158755,0.999644296815675,21.4315078542742));
#47643=CARTESIAN_POINT('Ctrl Pts',(30.9976338252526,1.13646112591015,21.4419030181452));
#47644=CARTESIAN_POINT('Ctrl Pts',(30.6731866853066,1.35520814296552,21.4635892944733));
#47645=CARTESIAN_POINT('Ctrl Pts',(30.4872391020676,1.43261266999426,21.474685827494));
#47646=CARTESIAN_POINT('Ctrl Pts',(30.1032980730075,1.50870030742653,21.4952717443516));
#47647=CARTESIAN_POINT('Ctrl Pts',(29.9096173130592,1.50952898426713,21.5040838450456));
#47648=CARTESIAN_POINT('Ctrl Pts',(29.5302606487566,1.43771855687004,21.5243303851611));
#47649=CARTESIAN_POINT('Ctrl Pts',(29.3483375586665,1.36492268311026,21.5351052715185));
#47650=CARTESIAN_POINT('Ctrl Pts',(29.0184009025148,1.15151905747937,21.5569072347786));
#47651=CARTESIAN_POINT('Ctrl Pts',(28.8745521744234,1.01139585435745,21.5677204711336));
#47652=CARTESIAN_POINT('Ctrl Pts',(28.6549505368779,0.690580628714703,21.5871975938919));
#47653=CARTESIAN_POINT('Ctrl Pts',(28.5784089748082,0.514933598952509,21.596392577836));
#47654=CARTESIAN_POINT('Ctrl Pts',(28.4935139297613,0.138064010695691,21.6173297771836));
#47655=CARTESIAN_POINT('Ctrl Pts',(28.4883967455728,-0.0601274794615553,
21.6283404155257));
#47656=CARTESIAN_POINT('Ctrl Pts',(28.5553929405263,-0.450590041266374,
21.6500327800704));
#47657=CARTESIAN_POINT('Ctrl Pts',(28.6281760530356,-0.63873783180513,21.6600741404618));
#47658=CARTESIAN_POINT('Ctrl Pts',(28.8386308155265,-0.968434016466414,
21.6793578772949));
#47659=CARTESIAN_POINT('Ctrl Pts',(28.9715505605447,-1.10856330761102,21.6896454618184));
#47660=CARTESIAN_POINT('Ctrl Pts',(29.2889068065357,-1.33562316156644,21.7112214894881));
#47661=CARTESIAN_POINT('Ctrl Pts',(29.4720453487169,-1.41803231498314,21.7223218898575));
#47662=CARTESIAN_POINT('Ctrl Pts',(29.7757758521236,-1.48742065117207,21.7388625842992));
#47663=CARTESIAN_POINT('Ctrl Pts',(29.8878284604463,-1.50000000000001,21.7446031442869));
#47664=CARTESIAN_POINT('Ctrl Pts',(30.,-1.50000000000001,21.75));
#47665=CARTESIAN_POINT('Ctrl Pts',(29.9999999999998,-1.50000000000001,21.8125));
#47666=CARTESIAN_POINT('Ctrl Pts',(29.9405204451645,-1.50000000000001,21.8096382885837));
#47667=CARTESIAN_POINT('Ctrl Pts',(29.8809833669271,-1.49646250510709,21.8066755458243));
#47668=CARTESIAN_POINT('Ctrl Pts',(29.6241950912386,-1.46572084178495,21.7934668790576));
#47669=CARTESIAN_POINT('Ctrl Pts',(29.4333772164259,-1.40302797833686,21.782544681346));
#47670=CARTESIAN_POINT('Ctrl Pts',(29.0921865820648,-1.20964665656295,21.760757435914));
#47671=CARTESIAN_POINT('Ctrl Pts',(28.9439925649252,-1.08269733302756,21.7501010778418));
#47672=CARTESIAN_POINT('Ctrl Pts',(28.7038088414644,-0.77933430694382,21.7301184823344));
#47673=CARTESIAN_POINT('Ctrl Pts',(28.6141674942217,-0.605760578772268,
21.7211533654873));
#47674=CARTESIAN_POINT('Ctrl Pts',(28.5043846389733,-0.22927416638246,21.7002374536878));
#47675=CARTESIAN_POINT('Ctrl Pts',(28.4872031236976,-0.0294943674923172,
21.6891385759717));
#47676=CARTESIAN_POINT('Ctrl Pts',(28.5307959749546,0.357711165892058,21.6676271574504));
#47677=CARTESIAN_POINT('Ctrl Pts',(28.588271358922,0.541814389624386,21.6573992005764));
#47678=CARTESIAN_POINT('Ctrl Pts',(28.7738533380075,0.887068805374046,21.6382183997014));
#47679=CARTESIAN_POINT('Ctrl Pts',(28.903512180976,1.043112470525,21.6279461150529));
#47680=CARTESIAN_POINT('Ctrl Pts',(29.2128905056455,1.29185751769652,21.6061515588234));
#47681=CARTESIAN_POINT('Ctrl Pts',(29.3882998946744,1.38356922217579,21.5951646233122));
#47682=CARTESIAN_POINT('Ctrl Pts',(29.7586487303438,1.49259838475184,21.5743176187989));
#47683=CARTESIAN_POINT('Ctrl Pts',(29.9494126813103,1.51113463524617,21.5652431789286));
#47684=CARTESIAN_POINT('Ctrl Pts',(30.3366113826679,1.4752126287187,21.5456162392091));
#47685=CARTESIAN_POINT('Ctrl Pts',(30.5290112502297,1.41763409463152,21.5347599925404));
#47686=CARTESIAN_POINT('Ctrl Pts',(30.8756573292315,1.23320190987312,21.512958859045));
#47687=CARTESIAN_POINT('Ctrl Pts',(31.0275193143428,1.10985575574539,21.5022261138206));
#47688=CARTESIAN_POINT('Ctrl Pts',(31.2750461098143,0.813213213668382,21.4820769047076));
#47689=CARTESIAN_POINT('Ctrl Pts',(31.3687657636095,0.643070885011216,21.4732261602783));
#47690=CARTESIAN_POINT('Ctrl Pts',(31.4888227697242,0.270291882918073,21.4525162157176));
#47691=CARTESIAN_POINT('Ctrl Pts',(31.5115128952941,0.0704953149593227,
21.4414164063865));
#47692=CARTESIAN_POINT('Ctrl Pts',(31.4782054807328,-0.318770290439176,
21.4197905394199));
#47693=CARTESIAN_POINT('Ctrl Pts',(31.4254475382382,-0.504803416717179,
21.4094553657378));
#47694=CARTESIAN_POINT('Ctrl Pts',(31.2494901966584,-0.853416070021567,
21.3900879961098));
#47695=CARTESIAN_POINT('Ctrl Pts',(31.1254658116588,-1.01138492328729,21.3802216401301));
#47696=CARTESIAN_POINT('Ctrl Pts',(30.8246930412984,-1.26828298434064,21.3586146462176));
#47697=CARTESIAN_POINT('Ctrl Pts',(30.6515224369356,-1.36534975789868,21.347586672365));
#47698=CARTESIAN_POINT('Ctrl Pts',(30.3143398429227,-1.47517879246933,21.3283131607309));
#47699=CARTESIAN_POINT('Ctrl Pts',(30.1575657374829,-1.50000000000003,21.3200808850792));
#47700=CARTESIAN_POINT('Ctrl Pts',(29.9999999999998,-1.50000000000001,21.3125));
#47701=CARTESIAN_POINT('Origin',(30.,-1.32966554433622E-14,16.));
#47702=CARTESIAN_POINT('',(29.9999999999999,-1.50000000000001,20.75));
#47703=CARTESIAN_POINT('',(30.0000000238974,-1.50000000000001,20.8125000022995));
#47704=CARTESIAN_POINT('',(30.,-1.50000000000001,16.));
#47705=CARTESIAN_POINT('Ctrl Pts',(29.9999999999998,-1.50000000000001,20.75));
#47706=CARTESIAN_POINT('Ctrl Pts',(30.1355873378723,-1.50000000000003,20.7565234488349));
#47707=CARTESIAN_POINT('Ctrl Pts',(30.2707763371628,-1.48162130053548,20.7635382520255));
#47708=CARTESIAN_POINT('Ctrl Pts',(30.5905052894202,-1.39270558594719,20.7813910993741));
#47709=CARTESIAN_POINT('Ctrl Pts',(30.767029784006,-1.30383501600373,20.7923527650226));
#47710=CARTESIAN_POINT('Ctrl Pts',(31.0784013127494,-1.06141205266722,20.8140676058879));
#47711=CARTESIAN_POINT('Ctrl Pts',(31.2094059572181,-0.909300433903993,
20.8244833092276));
#47712=CARTESIAN_POINT('Ctrl Pts',(31.4005633760122,-0.569930140644686,
20.8433372144086));
#47713=CARTESIAN_POINT('Ctrl Pts',(31.4616108021312,-0.387386085525011,
20.8534785508042));
#47714=CARTESIAN_POINT('Ctrl Pts',(31.5130288281118,-0.00193915990322278,
20.8748922688942));
#47715=CARTESIAN_POINT('Ctrl Pts',(31.5000564049022,0.197728440072968,20.8859849133374));
#47716=CARTESIAN_POINT('Ctrl Pts',(31.3981909189968,0.576981524645895,20.907054529147));
#47717=CARTESIAN_POINT('Ctrl Pts',(31.3116775745975,0.753220156722293,20.9161479987326));
#47718=CARTESIAN_POINT('Ctrl Pts',(31.0770964939546,1.06165196611475,20.9360018364982));
#47719=CARTESIAN_POINT('Ctrl Pts',(30.9317342971964,1.19125838532521,20.946595756762));
#47720=CARTESIAN_POINT('Ctrl Pts',(30.5933406580028,1.39218994814601,20.9684581606193));
#47721=CARTESIAN_POINT('Ctrl Pts',(30.4020178812766,1.458987498605,20.9795186695191));
#47722=CARTESIAN_POINT('Ctrl Pts',(30.0144815741343,1.51197726610397,20.999635956776));
#47723=CARTESIAN_POINT('Ctrl Pts',(29.8225847199203,1.50160380579917,21.0084913464817));
#47724=CARTESIAN_POINT('Ctrl Pts',(29.4482673839794,1.40844186112423,21.0290885295006));
#47725=CARTESIAN_POINT('Ctrl Pts',(29.2698358143887,1.32475295725216,21.0399980141694));
#47726=CARTESIAN_POINT('Ctrl Pts',(28.9522277915389,1.09163995424434,21.0617542984881));
#47727=CARTESIAN_POINT('Ctrl Pts',(28.8169317835683,0.943334467611102,21.0723833275575));
#47728=CARTESIAN_POINT('Ctrl Pts',(28.6164713965323,0.609937924996611,21.0912889974983));
#47729=CARTESIAN_POINT('Ctrl Pts',(28.5503235834348,0.429720618453307,21.1011266323083));
#47730=CARTESIAN_POINT('Ctrl Pts',(28.4877747716401,0.0469249157698905,
21.1223930602351));
#47731=CARTESIAN_POINT('Ctrl Pts',(28.4947443957624,-0.152432728065059,
21.1334684848926));
#47732=CARTESIAN_POINT('Ctrl Pts',(28.585202717896,-0.535530466260377,21.1547516925701));
#47733=CARTESIAN_POINT('Ctrl Pts',(28.6672227696192,-0.715637129073743,
21.1640888680802));
#47734=CARTESIAN_POINT('Ctrl Pts',(28.8938150388557,-1.03121039122832,21.1837567176656));
#47735=CARTESIAN_POINT('Ctrl Pts',(29.0350964807726,-1.16446677665445,21.1942556904709));
#47736=CARTESIAN_POINT('Ctrl Pts',(29.3666683501557,-1.37437197910307,21.2160391495426));
#47737=CARTESIAN_POINT('Ctrl Pts',(29.5553884234738,-1.44649304249621,21.2271223111757));
#47738=CARTESIAN_POINT('Ctrl Pts',(29.8346137979128,-1.49316573714005,21.2418530120072));
#47739=CARTESIAN_POINT('Ctrl Pts',(29.917323692752,-1.50000000000001,21.2460222343129));
#47740=CARTESIAN_POINT('Ctrl Pts',(30.,-1.50000000000001,21.25));
#47741=CARTESIAN_POINT('Ctrl Pts',(29.9999999999998,-1.50000000000001,21.3125));
#47742=CARTESIAN_POINT('Ctrl Pts',(29.9681380540405,-1.50000000000001,21.3109670414103));
#47743=CARTESIAN_POINT('Ctrl Pts',(29.9362464291016,-1.4989848402199,21.3094044560071));
#47744=CARTESIAN_POINT('Ctrl Pts',(29.7059061051266,-1.48427038685078,21.2979134671869));
#47745=CARTESIAN_POINT('Ctrl Pts',(29.5119585810338,-1.43225099507769,21.2871371794785));
#47746=CARTESIAN_POINT('Ctrl Pts',(29.1596955105172,-1.25764065487782,21.2653386273684));
#47747=CARTESIAN_POINT('Ctrl Pts',(29.0039750821709,-1.13829559847059,21.2545313843106));
#47748=CARTESIAN_POINT('Ctrl Pts',(28.7485987477413,-0.848934521932683,
21.2342067770101));
#47749=CARTESIAN_POINT('Ctrl Pts',(28.6505388148689,-0.682384621723858,
21.2254102567623));
#47750=CARTESIAN_POINT('Ctrl Pts',(28.5196273945211,-0.313661198442873,
21.2049256221356));
#47751=CARTESIAN_POINT('Ctrl Pts',(28.4910680085409,-0.114008266472331,
21.1938337925817));
#47752=CARTESIAN_POINT('Ctrl Pts',(28.5133617159534,0.277152561451723,21.1721026354748));
#47753=CARTESIAN_POINT('Ctrl Pts',(28.5610406223868,0.465104578293146,21.1616608567614));
#47754=CARTESIAN_POINT('Ctrl Pts',(28.7268127368948,0.817191792877632,21.1421004559512));
#47755=CARTESIAN_POINT('Ctrl Pts',(28.8450160186508,0.977157792197407,21.1325925873729));
#47756=CARTESIAN_POINT('Ctrl Pts',(29.1366994431696,1.24242044599111,21.1111905550177));
#47757=CARTESIAN_POINT('Ctrl Pts',(29.3073536529405,1.34504122266248,21.1001293733922));
#47758=CARTESIAN_POINT('Ctrl Pts',(29.6718885684984,1.47596994041667,21.0789537702634));
#47759=CARTESIAN_POINT('Ctrl Pts',(29.8613546451375,1.5056180641301,21.0693266350828));
#47760=CARTESIAN_POINT('Ctrl Pts',(30.2499905035945,1.49232790599687,21.0502592125655));
#47761=CARTESIAN_POINT('Ctrl Pts',(30.4453612619354,1.44608660162569,21.0395749518952));
#47762=CARTESIAN_POINT('Ctrl Pts',(30.8031247707546,1.28178759217525,21.017798185678));
#47763=CARTESIAN_POINT('Ctrl Pts',(30.9627170127615,1.16669332668992,21.0069227374242));
#47764=CARTESIAN_POINT('Ctrl Pts',(31.2261252563514,0.884888124749317,20.9864215801195));
#47765=CARTESIAN_POINT('Ctrl Pts',(31.3286136134484,0.721936793997485,20.9776075996665));
#47766=CARTESIAN_POINT('Ctrl Pts',(31.4704956794702,0.357450862099888,20.9573583812278));
#47767=CARTESIAN_POINT('Ctrl Pts',(31.5050292215643,0.158114714869949,20.9462841508261));
#47768=CARTESIAN_POINT('Ctrl Pts',(31.4940038450927,-0.234658795010768,
20.9244634002772));
#47769=CARTESIAN_POINT('Ctrl Pts',(31.4515503117875,-0.4244189406881,20.9139211699618));
#47770=CARTESIAN_POINT('Ctrl Pts',(31.2960889353342,-0.779942120592769,
20.8941698821893));
#47771=CARTESIAN_POINT('Ctrl Pts',(31.1836334516182,-0.941901166431575,
20.8849503363697));
#47772=CARTESIAN_POINT('Ctrl Pts',(30.9011214218994,-1.21536636315781,20.8637617145378));
#47773=CARTESIAN_POINT('Ctrl Pts',(30.7331593249481,-1.323483412269,20.8526773830162));
#47774=CARTESIAN_POINT('Ctrl Pts',(30.374104697925,-1.46471715060753,20.8314791998208));
#47775=CARTESIAN_POINT('Ctrl Pts',(30.1878361111775,-1.49999999700053,20.821537269196));
#47776=CARTESIAN_POINT('Ctrl Pts',(30.0000000239529,-1.50000000000001,20.8125000011524));
#47777=CARTESIAN_POINT('Origin',(30.,-1.32966554433622E-14,16.));
#47778=CARTESIAN_POINT('',(29.9999999999999,-1.50000000000001,20.25));
#47779=CARTESIAN_POINT('',(30.0000000000001,-1.50000000000001,20.3125));
#47780=CARTESIAN_POINT('',(30.,-1.50000000000001,16.));
#47781=CARTESIAN_POINT('Ctrl Pts',(29.9999999999999,-1.50000000000001,20.25));
#47782=CARTESIAN_POINT('Ctrl Pts',(30.1641246040904,-1.50000000000003,20.257896448696));
#47783=CARTESIAN_POINT('Ctrl Pts',(30.3273129308388,-1.47306839847894,20.2664959507697));
#47784=CARTESIAN_POINT('Ctrl Pts',(30.6694540696788,-1.35668483193177,20.2861901008358));
#47785=CARTESIAN_POINT('Ctrl Pts',(30.8415535621189,-1.25719932144175,20.2972337279289));
#47786=CARTESIAN_POINT('Ctrl Pts',(31.1383891848058,-0.996648092240175,
20.3187527726287));
#47787=CARTESIAN_POINT('Ctrl Pts',(31.2598762410215,-0.837810488997904,
20.3284549728335));
#47788=CARTESIAN_POINT('Ctrl Pts',(31.4314249865634,-0.487683998530185,
20.3479064445261));
#47789=CARTESIAN_POINT('Ctrl Pts',(31.4819950779928,-0.300804420279551,
20.3582886433178));
#47790=CARTESIAN_POINT('Ctrl Pts',(31.5105507066295,0.0893179172321859,
20.3799621065129));
#47791=CARTESIAN_POINT('Ctrl Pts',(31.4853246402279,0.289072829407564,20.3910596016338));
#47792=CARTESIAN_POINT('Ctrl Pts',(31.3605672791737,0.660112394093701,20.411672910783));
#47793=CARTESIAN_POINT('Ctrl Pts',(31.2649722312571,0.828695575895264,20.4204916500332));
#47794=CARTESIAN_POINT('Ctrl Pts',(31.0140581775355,1.12220790918685,20.4407168784407));
#47795=CARTESIAN_POINT('Ctrl Pts',(30.8605226301063,1.24384616367647,20.4514827013131));
#47796=CARTESIAN_POINT('Ctrl Pts',(30.5114243415045,1.42407146100134,20.4732849588136));
#47797=CARTESIAN_POINT('Ctrl Pts',(30.3183380047095,1.47926213924964,20.4841079039198));
#47798=CARTESIAN_POINT('Ctrl Pts',(29.9307960888716,1.51038882263748,20.5036181531332));
#47799=CARTESIAN_POINT('Ctrl Pts',(29.7403288665302,1.48951380456358,20.5127847164407));
#47800=CARTESIAN_POINT('Ctrl Pts',(29.3711639835748,1.37589985350485,20.5337021132381));
#47801=CARTESIAN_POINT('Ctrl Pts',(29.1966946677341,1.28188655628153,20.5447077525887));
#47802=CARTESIAN_POINT('Ctrl Pts',(28.8909965958092,1.02962579258236,20.5664229013678));
#47803=CARTESIAN_POINT('Ctrl Pts',(28.7637626025144,0.872753791453066,20.5765136782526));
#47804=CARTESIAN_POINT('Ctrl Pts',(28.582295287402,0.526054660802727,20.5957747410665));
#47805=CARTESIAN_POINT('Ctrl Pts',(28.5268265400693,0.341112810094873,20.6060492883281));
#47806=CARTESIAN_POINT('Ctrl Pts',(28.4876154625531,-0.0470049788678421,
20.6276113877149));
#47807=CARTESIAN_POINT('Ctrl Pts',(28.5071470207889,-0.246809925970759,
20.6387116625539));
#47808=CARTESIAN_POINT('Ctrl Pts',(28.6213243381125,-0.621726643029005,
20.6595403690571));
#47809=CARTESIAN_POINT('Ctrl Pts',(28.7127069454602,-0.793828860292424,
20.6684492190444));
#47810=CARTESIAN_POINT('Ctrl Pts',(28.9560213000323,-1.09433750409046,20.6885031487146));
#47811=CARTESIAN_POINT('Ctrl Pts',(29.1057854975977,-1.21976733917156,20.6991928441151));
#47812=CARTESIAN_POINT('Ctrl Pts',(29.4493247586543,-1.40936219023255,20.7209879081598));
#47813=CARTESIAN_POINT('Ctrl Pts',(29.6408325610402,-1.46988527163767,20.7318830283038));
#47814=CARTESIAN_POINT('Ctrl Pts',(29.8922912775479,-1.4971028845898,20.7447373862468));
#47815=CARTESIAN_POINT('Ctrl Pts',(29.9461731363168,-1.50000000000001,20.7474102538136));
#47816=CARTESIAN_POINT('Ctrl Pts',(29.9999999999998,-1.50000000000001,20.75));
#47817=CARTESIAN_POINT('Ctrl Pts',(30.0000000239529,-1.50000000000001,20.8125000011524));
#47818=CARTESIAN_POINT('Ctrl Pts',(29.9974904007656,-1.50000000004009,20.8123792568517));
#47819=CARTESIAN_POINT('Ctrl Pts',(29.994980514477,-1.49999370187214,20.8122583249421));
#47820=CARTESIAN_POINT('Ctrl Pts',(29.7936662704942,-1.49898314378545,20.8025445178046));
#47821=CARTESIAN_POINT('Ctrl Pts',(29.5970666373285,-1.45847246315053,20.7919603168594));
#47822=CARTESIAN_POINT('Ctrl Pts',(29.2341811004286,-1.30450218441903,20.7702240261379));
#47823=CARTESIAN_POINT('Ctrl Pts',(29.0708854167951,-1.19371554978206,20.7592900523783));
#47824=CARTESIAN_POINT('Ctrl Pts',(28.7996246113049,-0.919409908918738,
20.738619409654));
#47825=CARTESIAN_POINT('Ctrl Pts',(28.6928036628702,-0.759898893507146,
20.7297166051949));
#47826=CARTESIAN_POINT('Ctrl Pts',(28.540323338491,-0.399638425423168,20.7097021347457));
#47827=CARTESIAN_POINT('Ctrl Pts',(28.4999872115666,-0.200774562873281,
20.6986541423819));
#47828=CARTESIAN_POINT('Ctrl Pts',(28.5000123038317,0.193260173251348,20.6767633237083));
#47829=CARTESIAN_POINT('Ctrl Pts',(28.5373370740434,0.384636586987589,20.6661313007229));
#47830=CARTESIAN_POINT('Ctrl Pts',(28.6828216865171,0.743407395273799,20.6461995891515));
#47831=CARTESIAN_POINT('Ctrl Pts',(28.7898502936129,0.90727948583588,20.637187813622));
#47832=CARTESIAN_POINT('Ctrl Pts',(29.0635269308615,1.18843769395866,20.6162105900475));
#47833=CARTESIAN_POINT('Ctrl Pts',(29.228755223573,1.30174519776628,20.6051136094466));
#47834=CARTESIAN_POINT('Ctrl Pts',(29.5868470804747,1.45456710532649,20.5836398539607));
#47835=CARTESIAN_POINT('Ctrl Pts',(29.7752048690842,1.49530975495507,20.5734457453635));
#47836=CARTESIAN_POINT('Ctrl Pts',(30.1648759814307,1.50410182396658,20.5544534610902));
#47837=CARTESIAN_POINT('Ctrl Pts',(30.3625681263815,1.46904639647318,20.544196110566));
#47838=CARTESIAN_POINT('Ctrl Pts',(30.7301648562918,1.32486538129436,20.5225050764527));
#47839=CARTESIAN_POINT('Ctrl Pts',(30.8968384149473,1.21823387618242,20.5115240048699));
#47840=CARTESIAN_POINT('Ctrl Pts',(31.1754315899033,0.951036194862134,20.4906980266758));
#47841=CARTESIAN_POINT('Ctrl Pts',(31.2863099173977,0.794671992670377,20.4816484440372));
#47842=CARTESIAN_POINT('Ctrl Pts',(31.4475104523221,0.440765387920731,20.4619869659956));
#47843=CARTESIAN_POINT('Ctrl Pts',(31.4931266838049,0.245180433281527,20.4511211351823));
#47844=CARTESIAN_POINT('Ctrl Pts',(31.505277935416,-0.147222207316758,20.4293209884824));
#47845=CARTESIAN_POINT('Ctrl Pts',(31.4737006088925,-0.340229130529765,
20.4185983816372));
#47846=CARTESIAN_POINT('Ctrl Pts',(31.339252899941,-0.702504700740186,20.39847196107));
#47847=CARTESIAN_POINT('Ctrl Pts',(31.2380795698328,-0.868488363198902,
20.3896091209879));
#47848=CARTESIAN_POINT('Ctrl Pts',(30.9741217873874,-1.15788922779948,20.3688705333532));
#47849=CARTESIAN_POINT('Ctrl Pts',(30.8120536546578,-1.27678494801521,20.3577703677868));
#47850=CARTESIAN_POINT('Ctrl Pts',(30.4578087067642,-1.44121172280179,20.3361593393739));
#47851=CARTESIAN_POINT('Ctrl Pts',(30.2702179556352,-1.48784534045563,20.3258384968839));
#47852=CARTESIAN_POINT('Ctrl Pts',(30.052598998323,-1.49930896382792,20.3150498659359));
#47853=CARTESIAN_POINT('Ctrl Pts',(30.0262877690999,-1.50000000000001,20.3137647708805));
#47854=CARTESIAN_POINT('Ctrl Pts',(30.0000000000001,-1.50000000000001,20.3125));
#47855=CARTESIAN_POINT('Origin',(30.,-1.32966554433622E-14,16.));
#47856=CARTESIAN_POINT('',(29.9999999508795,-1.50000000000001,19.7499999952734));
#47857=CARTESIAN_POINT('',(30.0000000000001,-1.50000000000001,19.8125));
#47858=CARTESIAN_POINT('',(30.,-1.50000000000001,16.));
#47859=CARTESIAN_POINT('Ctrl Pts',(29.9999999507652,-1.50000000000001,19.7499999976312));
#47860=CARTESIAN_POINT('Ctrl Pts',(30.0036354883629,-1.50000000011934,19.7501749125187));
#47861=CARTESIAN_POINT('Ctrl Pts',(30.007271600744,-1.4999867831078,19.7503502221899));
#47862=CARTESIAN_POINT('Ctrl Pts',(30.201622915749,-1.49857339489822,19.7597402149765));
#47863=CARTESIAN_POINT('Ctrl Pts',(30.3903004853368,-1.46082693625102,19.769866481516));
#47864=CARTESIAN_POINT('Ctrl Pts',(30.7502056783764,-1.31393443624912,19.7912627754119));
#47865=CARTESIAN_POINT('Ctrl Pts',(30.9169691324023,-1.2034971179945,19.8023538891195));
#47866=CARTESIAN_POINT('Ctrl Pts',(31.1955532827852,-0.926587489668503,
19.8234492094243));
#47867=CARTESIAN_POINT('Ctrl Pts',(31.305583357368,-0.763777918932018,19.8325678933928));
#47868=CARTESIAN_POINT('Ctrl Pts',(31.4566154175894,-0.406803589900389,
19.8523998005612));
#47869=CARTESIAN_POINT('Ctrl Pts',(31.4968003232487,-0.216309448389897,
19.8629828084229));
#47870=CARTESIAN_POINT('Ctrl Pts',(31.5029527191874,0.177060648076386,19.884836702671));
#47871=CARTESIAN_POINT('Ctrl Pts',(31.4658451495388,0.376207311237188,19.8959004061799));
#47872=CARTESIAN_POINT('Ctrl Pts',(31.3192558360179,0.738832237635632,19.9160462354243));
#47873=CARTESIAN_POINT('Ctrl Pts',(31.2148503942445,0.900251242918639,19.9248907954582));
#47874=CARTESIAN_POINT('Ctrl Pts',(30.9479657510409,1.17875033469753,19.9454673747239));
#47875=CARTESIAN_POINT('Ctrl Pts',(30.7867234803792,1.29195591113542,19.9563697464337));
#47876=CARTESIAN_POINT('Ctrl Pts',(30.4266603329508,1.45171184585212,19.9781309575447));
#47877=CARTESIAN_POINT('Ctrl Pts',(30.2307253625385,1.49542562590392,19.9887721548721));
#47878=CARTESIAN_POINT('Ctrl Pts',(29.8418323593176,1.50370934578551,20.0077128815434));
#47879=CARTESIAN_POINT('Ctrl Pts',(29.6526184508184,1.47157346290215,20.0175030286082));
#47880=CARTESIAN_POINT('Ctrl Pts',(29.2894512067405,1.33570909972092,20.038749930874));
#47881=CARTESIAN_POINT('Ctrl Pts',(29.1199599079427,1.2306626568369,20.0498225415362));
#47882=CARTESIAN_POINT('Ctrl Pts',(28.8323016398048,0.961771765690436,20.0711316978356));
#47883=CARTESIAN_POINT('Ctrl Pts',(28.7166359490173,0.80092922531751,20.0805039319268));
#47884=CARTESIAN_POINT('Ctrl Pts',(28.5553841103709,0.447325657819572,20.1001485745656));
#47885=CARTESIAN_POINT('Ctrl Pts',(28.5099861175222,0.258564005548656,20.1106353330251));
#47886=CARTESIAN_POINT('Ctrl Pts',(28.4926188058233,-0.133342134639988,
20.1324078963689));
#47887=CARTESIAN_POINT('Ctrl Pts',(28.5237938243712,-0.332877530953282,
20.1434931961641));
#47888=CARTESIAN_POINT('Ctrl Pts',(28.6595170927538,-0.699759711689848,
20.1638755395383));
#47889=CARTESIAN_POINT('Ctrl Pts',(28.759513047986,-0.864726488741114,20.1726705572702));
#47890=CARTESIAN_POINT('Ctrl Pts',(29.0184002150316,-1.15079879551533,20.1930727248681));
#47891=CARTESIAN_POINT('Ctrl Pts',(29.1758229214277,-1.26830528519454,20.2039107975187));
#47892=CARTESIAN_POINT('Ctrl Pts',(29.5305217931358,-1.4384406773805,20.2257022380569));
#47893=CARTESIAN_POINT('Ctrl Pts',(29.7251117157194,-1.4879453135066,20.2364395788536));
#47894=CARTESIAN_POINT('Ctrl Pts',(29.9491466954872,-1.49935402178859,20.2475353754067));
#47895=CARTESIAN_POINT('Ctrl Pts',(29.9745837219083,-1.50000000000001,20.2487771587502));
#47896=CARTESIAN_POINT('Ctrl Pts',(29.9999999999999,-1.50000000000001,20.25));
#47897=CARTESIAN_POINT('Ctrl Pts',(30.0000000000001,-1.50000000000001,20.3125));
#47898=CARTESIAN_POINT('Ctrl Pts',(29.8275998140085,-1.50000000000001,20.3042053921841));
#47899=CARTESIAN_POINT('Ctrl Pts',(29.6562870357889,-1.47028352574469,20.2951376446808));
#47900=CARTESIAN_POINT('Ctrl Pts',(29.3085931862514,-1.34558031058123,20.2749452383464));
#47901=CARTESIAN_POINT('Ctrl Pts',(29.1384186293223,-1.24350663328035,20.2639223312337));
#47902=CARTESIAN_POINT('Ctrl Pts',(28.8520258822514,-0.983987574399218,
20.242934391019));
#47903=CARTESIAN_POINT('Ctrl Pts',(28.7368098691781,-0.830906588856551,
20.2336614771587));
#47904=CARTESIAN_POINT('Ctrl Pts',(28.5656483010559,-0.481857271883387,
20.214269848438));
#47905=CARTESIAN_POINT('Ctrl Pts',(28.5144799811963,-0.287679235979695,
20.2034821797766));
#47906=CARTESIAN_POINT('Ctrl Pts',(28.4911007681834,0.104720249591022,20.181682208356));
#47907=CARTESIAN_POINT('Ctrl Pts',(28.5173310962609,0.299077411990059,20.1708845882228));
#47908=CARTESIAN_POINT('Ctrl Pts',(28.6416246239434,0.664496311411631,20.1505835382549));
#47909=CARTESIAN_POINT('Ctrl Pts',(28.7375408574377,0.832427515421977,20.1417837739438));
#47910=CARTESIAN_POINT('Ctrl Pts',(28.9926175512114,1.12917452204563,20.1212684183864));
#47911=CARTESIAN_POINT('Ctrl Pts',(29.1516633795811,1.2530630770023,20.1101749736523));
#47912=CARTESIAN_POINT('Ctrl Pts',(29.5021040725661,1.42792836972927,20.0884570187074));
#47913=CARTESIAN_POINT('Ctrl Pts',(29.6888418601191,1.47989191267207,20.0780291609664));
#47914=CARTESIAN_POINT('Ctrl Pts',(30.0769287467939,1.5109546306831,20.0584944686474));
#47915=CARTESIAN_POINT('Ctrl Pts',(30.2747213678695,1.48776626200004,20.0489426359701));
#47916=CARTESIAN_POINT('Ctrl Pts',(30.6499367323256,1.36617967610523,20.027512673167));
#47917=CARTESIAN_POINT('Ctrl Pts',(30.8236685705517,1.26902858360925,20.0164553547449));
#47918=CARTESIAN_POINT('Ctrl Pts',(31.1182297704941,1.01768973269335,19.9953016376572));
#47919=CARTESIAN_POINT('Ctrl Pts',(31.2380227260335,0.867983838688731,19.9857213243715));
#47920=CARTESIAN_POINT('Ctrl Pts',(31.4194655172301,0.52407745893419,19.9666154143852));
#47921=CARTESIAN_POINT('Ctrl Pts',(31.4763477416476,0.331530482038543,19.9559183601132));
#47922=CARTESIAN_POINT('Ctrl Pts',(31.5113890098208,-0.0605236259430762,
19.9341375763365));
#47923=CARTESIAN_POINT('Ctrl Pts',(31.4907606610887,-0.256127601642152,
19.9232706887976));
#47924=CARTESIAN_POINT('Ctrl Pts',(31.3770092904839,-0.62473058770716,19.9027927451274));
#47925=CARTESIAN_POINT('Ctrl Pts',(31.2864311739689,-0.794691675228615,
19.8939853466257));
#47926=CARTESIAN_POINT('Ctrl Pts',(31.0405043429371,-1.09883901947073,19.8737046491109));
#47927=CARTESIAN_POINT('Ctrl Pts',(30.8847013390568,-1.22775605549742,19.8626275448131));
#47928=CARTESIAN_POINT('Ctrl Pts',(30.5384592288504,-1.41320441242881,19.8408176202706));
#47929=CARTESIAN_POINT('Ctrl Pts',(30.3527481344157,-1.47060245170435,19.8302882010938));
#47930=CARTESIAN_POINT('Ctrl Pts',(30.1075898199807,-1.49710947656403,19.8177567099449));
#47931=CARTESIAN_POINT('Ctrl Pts',(30.0537655536404,-1.50000000000001,19.8150867964056));
#47932=CARTESIAN_POINT('Ctrl Pts',(30.0000000000003,-1.50000000000001,19.8125));
#47933=CARTESIAN_POINT('Origin',(30.,-1.32966554433622E-14,16.));
#47934=CARTESIAN_POINT('',(30.0000000000001,-1.50000000000001,19.25));
#47935=CARTESIAN_POINT('',(30.,-1.50000000000001,19.3125));
#47936=CARTESIAN_POINT('',(30.,-1.50000000000001,16.));
#47937=CARTESIAN_POINT('Ctrl Pts',(30.0000000000001,-1.50000000000001,19.25));
#47938=CARTESIAN_POINT('Ctrl Pts',(30.0322695745912,-1.50000000000001,19.2515525706314));
#47939=CARTESIAN_POINT('Ctrl Pts',(30.0645714825038,-1.49895869986435,19.2531356219044));
#47940=CARTESIAN_POINT('Ctrl Pts',(30.2882590679586,-1.48448482383795,19.2642998479893));
#47941=CARTESIAN_POINT('Ctrl Pts',(30.4754930135539,-1.43550485550641,19.2746687000727));
#47942=CARTESIAN_POINT('Ctrl Pts',(30.8281012978914,-1.26647563555772,19.2963288301724));
#47943=CARTESIAN_POINT('Ctrl Pts',(30.9888581275123,-1.14537453755813,19.3074271661326));
#47944=CARTESIAN_POINT('Ctrl Pts',(31.2489169787693,-0.852727854965852,
19.328068327964));
#47945=CARTESIAN_POINT('Ctrl Pts',(31.3477723438117,-0.685891580063111,
19.3368949122188));
#47946=CARTESIAN_POINT('Ctrl Pts',(31.4777710225729,-0.322229436301838,
19.35709836465));
#47947=CARTESIAN_POINT('Ctrl Pts',(31.5070120496637,-0.128613045958812,
19.3678548307802));
#47948=CARTESIAN_POINT('Ctrl Pts',(31.4899431617665,0.263827999699887,19.3896571110945));
#47949=CARTESIAN_POINT('Ctrl Pts',(31.4418890858574,0.458816520684437,19.4004898067048));
#47950=CARTESIAN_POINT('Ctrl Pts',(31.2763170645903,0.810606892156535,19.420033716231));
#47951=CARTESIAN_POINT('Ctrl Pts',(31.1635461572557,0.965528328551652,19.4291724240899));
#47952=CARTESIAN_POINT('Ctrl Pts',(30.8815440072885,1.22938524433353,19.4500696176279));
#47953=CARTESIAN_POINT('Ctrl Pts',(30.713328176096,1.33404197013925,19.4610700368521));
#47954=CARTESIAN_POINT('Ctrl Pts',(30.3423586225268,1.47407873960012,19.4828082280827));
#47955=CARTESIAN_POINT('Ctrl Pts',(30.1427440803289,1.50655371354715,19.4929501746347));
#47956=CARTESIAN_POINT('Ctrl Pts',(29.7515262729803,1.4915957790601,19.5121881483469));
#47957=CARTESIAN_POINT('Ctrl Pts',(29.563545020268,1.44778515274356,19.522449362427));
#47958=CARTESIAN_POINT('Ctrl Pts',(29.2074099124303,1.28891068317319,19.5439971005021));
#47959=CARTESIAN_POINT('Ctrl Pts',(29.0438038910602,1.17268375630169,19.5550971246218));
#47960=CARTESIAN_POINT('Ctrl Pts',(28.7751767012687,0.88721540741588,19.5759511326745));
#47961=CARTESIAN_POINT('Ctrl Pts',(28.6712044325382,0.722248138115754,19.5848751034381));
#47962=CARTESIAN_POINT('Ctrl Pts',(28.5314450700553,0.361647735614998,19.6049084591326));
#47963=CARTESIAN_POINT('Ctrl Pts',(28.4970926988021,0.169404578017586,19.6155886345547));
#47964=CARTESIAN_POINT('Ctrl Pts',(28.5033789257342,-0.222871075081128,
19.6373817263935));
#47965=CARTESIAN_POINT('Ctrl Pts',(28.5460751647458,-0.419126971559099,
19.6482848317533));
#47966=CARTESIAN_POINT('Ctrl Pts',(28.7020419000445,-0.77553505760853,19.6680852809783));
#47967=CARTESIAN_POINT('Ctrl Pts',(28.8106757232385,-0.933630997355151,
19.6770461367592));
#47968=CARTESIAN_POINT('Ctrl Pts',(29.0852161697017,-1.20477024704427,19.697786615973));
#47969=CARTESIAN_POINT('Ctrl Pts',(29.2500326897204,-1.31371406923191,19.7087425717726));
#47970=CARTESIAN_POINT('Ctrl Pts',(29.611734771314,-1.46197087611401,19.7302632159228));
#47971=CARTESIAN_POINT('Ctrl Pts',(29.8049901134984,-1.49999999359916,19.7406175822833));
#47972=CARTESIAN_POINT('Ctrl Pts',(29.9999999507652,-1.50000000000001,19.7499999976312));
#47973=CARTESIAN_POINT('Ctrl Pts',(30.0000000000003,-1.50000000000001,19.8125));
#47974=CARTESIAN_POINT('Ctrl Pts',(29.8589500630315,-1.50000000000001,19.8057137317435));
#47975=CARTESIAN_POINT('Ctrl Pts',(29.7183576297039,-1.48011045726929,19.7983969878431));
#47976=CARTESIAN_POINT('Ctrl Pts',(29.392433533781,-1.38562863633522,19.7800914624408));
#47977=CARTESIAN_POINT('Ctrl Pts',(29.2152602016442,-1.29355450601908,19.7690095917929));
#47978=CARTESIAN_POINT('Ctrl Pts',(28.9125224323809,-1.05055621120639,19.7476941614444));
#47979=CARTESIAN_POINT('Ctrl Pts',(28.7881027470448,-0.904173072558181,
19.7377318373643));
#47980=CARTESIAN_POINT('Ctrl Pts',(28.5965141205021,-0.565467385757126,
19.7189148547643));
#47981=CARTESIAN_POINT('Ctrl Pts',(28.5340212729776,-0.374707579896709,
19.708317087772));
#47982=CARTESIAN_POINT('Ctrl Pts',(28.4874198303467,0.0166598622973653,
19.6865744520946));
#47983=CARTESIAN_POINT('Ctrl Pts',(28.5024461232084,0.213342923270549,19.6756476153738));
#47984=CARTESIAN_POINT('Ctrl Pts',(28.605730933148,0.585021358101511,19.6549988134388));
#47985=CARTESIAN_POINT('Ctrl Pts',(28.6911262279336,0.757019946925095,19.6461115535275));
#47986=CARTESIAN_POINT('Ctrl Pts',(28.9280450078188,1.06829223859541,19.6260663408692));
#47987=CARTESIAN_POINT('Ctrl Pts',(29.0805347242822,1.20204064727676,19.6150144423906));
#47988=CARTESIAN_POINT('Ctrl Pts',(29.4223784266326,1.3977266885599,19.5931317562239));
#47989=CARTESIAN_POINT('Ctrl Pts',(29.6069366918152,1.46041214264913,19.5825109299366));
#47990=CARTESIAN_POINT('Ctrl Pts',(29.9906687655378,1.51247863508202,19.562602320475));
#47991=CARTESIAN_POINT('Ctrl Pts',(30.1862339040192,1.50100007477566,19.55356759697));
#47992=CARTESIAN_POINT('Ctrl Pts',(30.5662821795392,1.40308967236277,19.5325627823883));
#47993=CARTESIAN_POINT('Ctrl Pts',(30.7466285872712,1.31600734425417,19.5214669082421));
#47994=CARTESIAN_POINT('Ctrl Pts',(31.0570470506688,1.08124306107491,19.5000106628701));
#47995=CARTESIAN_POINT('Ctrl Pts',(31.185947420448,0.938076365153711,19.4898320882731));
#47996=CARTESIAN_POINT('Ctrl Pts',(31.387173884418,0.604359282145194,19.4708806565388));
#47997=CARTESIAN_POINT('Ctrl Pts',(31.4549913450499,0.415392173173207,19.460577342954));
#47998=CARTESIAN_POINT('Ctrl Pts',(31.5125364736871,0.0248207245632997,
19.4388789291423));
#47999=CARTESIAN_POINT('Ctrl Pts',(31.5028468405333,-0.172737498474235,
19.4279034723069));
#48000=CARTESIAN_POINT('Ctrl Pts',(31.4094808313587,-0.547250043493136,
19.4070972198059));
#48001=CARTESIAN_POINT('Ctrl Pts',(31.3288984144444,-0.721204660777261,
19.3980698586427));
#48002=CARTESIAN_POINT('Ctrl Pts',(31.1018991125715,-1.03700530321776,19.3783761095713));
#48003=CARTESIAN_POINT('Ctrl Pts',(30.9548507096631,-1.17379817492847,19.3675014379958));
#48004=CARTESIAN_POINT('Ctrl Pts',(30.6204358823266,-1.37933694163779,19.3457024869274));
#48005=CARTESIAN_POINT('Ctrl Pts',(30.4373267027344,-1.44785012953098,19.3349894983086));
#48006=CARTESIAN_POINT('Ctrl Pts',(30.1646733538461,-1.49322482781476,19.3206110496582));
#48007=CARTESIAN_POINT('Ctrl Pts',(30.0823180279059,-1.50000000000001,19.3164605279642));
#48008=CARTESIAN_POINT('Ctrl Pts',(30.,-1.50000000000001,19.3125));
#48009=CARTESIAN_POINT('Origin',(30.,-1.32966554433622E-14,16.));
#48010=CARTESIAN_POINT('',(30.0000000000001,-1.50000000000001,18.75));
#48011=CARTESIAN_POINT('',(30.,-1.50000000000001,18.8125));
#48012=CARTESIAN_POINT('',(30.,-1.50000000000001,16.));
#48013=CARTESIAN_POINT('Ctrl Pts',(30.0000000000002,-1.50000000000001,18.75));
#48014=CARTESIAN_POINT('Ctrl Pts',(30.0598815861698,-1.50000000000001,18.7528810541579));
#48015=CARTESIAN_POINT('Ctrl Pts',(30.1198247627216,-1.4964145214846,18.7558646682098));
#48016=CARTESIAN_POINT('Ctrl Pts',(30.3709807388755,-1.46613984657296,18.7687893789386));
#48017=CARTESIAN_POINT('Ctrl Pts',(30.5561899070999,-1.40635296128044,18.7793610060131));
#48018=CARTESIAN_POINT('Ctrl Pts',(30.9004833554958,-1.21627199481911,18.8012058591186));
#48019=CARTESIAN_POINT('Ctrl Pts',(31.054808880873,-1.08516465668695,18.8122727199239));
#48020=CARTESIAN_POINT('Ctrl Pts',(31.2966795386424,-0.777790002612556,
18.832447912207));
#48021=CARTESIAN_POINT('Ctrl Pts',(31.3849156897549,-0.606916752329299,
18.8412824026485));
#48022=CARTESIAN_POINT('Ctrl Pts',(31.4939654845851,-0.236921615045211,
18.8618376880532));
#48023=CARTESIAN_POINT('Ctrl Pts',(31.5120817444602,-0.0408132290769898,
18.8727325983848));
#48024=CARTESIAN_POINT('Ctrl Pts',(31.4718441015158,0.350974679810523,18.8944985933229));
#48025=CARTESIAN_POINT('Ctrl Pts',(31.4124332725198,0.54273929222595,18.9051521829016));
#48026=CARTESIAN_POINT('Ctrl Pts',(31.2264254338517,0.884320880490274,18.9241289378051));
#48027=CARTESIAN_POINT('Ctrl Pts',(31.1045648671413,1.03253115218655,18.9338713522791));
#48028=CARTESIAN_POINT('Ctrl Pts',(30.8063387149155,1.2801510812434,18.9550980960807));
#48029=CARTESIAN_POINT('Ctrl Pts',(30.6310491381331,1.37504484021148,18.9661676575249));
#48030=CARTESIAN_POINT('Ctrl Pts',(30.2546711108962,1.4912245976519,18.9875033692879));
#48031=CARTESIAN_POINT('Ctrl Pts',(30.05740041095,1.51172051693628,18.9969127515258));
#48032=CARTESIAN_POINT('Ctrl Pts',(29.6702738320324,1.47589654334487,19.0165334981157));
#48033=CARTESIAN_POINT('Ctrl Pts',(29.4839742576828,1.42150925053353,19.0270075986994));
#48034=CARTESIAN_POINT('Ctrl Pts',(29.1353660189379,1.24191643228194,19.048768709802));
#48035=CARTESIAN_POINT('Ctrl Pts',(28.9777462443354,1.1157773991078,19.059856056776));
#48036=CARTESIAN_POINT('Ctrl Pts',(28.7267374929236,0.815719209989595,19.0802676706567));
#48037=CARTESIAN_POINT('Ctrl Pts',(28.6332044534767,0.64688991790973,19.0890616712273));
#48038=CARTESIAN_POINT('Ctrl Pts',(28.5135873974093,0.280047942578678,19.109441780968));
#48039=CARTESIAN_POINT('Ctrl Pts',(28.4898364137009,0.0851180238092936,
19.1202712208996));
#48040=CARTESIAN_POINT('Ctrl Pts',(28.5183897482981,-0.307171243363851,
19.1420650690759));
#48041=CARTESIAN_POINT('Ctrl Pts',(28.5720998196786,-0.500646940480604,
19.1528137189157));
#48042=CARTESIAN_POINT('Ctrl Pts',(28.747829861517,-0.847427013151625,19.1720792785085));
#48043=CARTESIAN_POINT('Ctrl Pts',(28.8650664758991,-0.999006868470888,
19.1814790094866));
#48044=CARTESIAN_POINT('Ctrl Pts',(29.1550741400796,-1.25492382568339,19.2025408141021));
#48045=CARTESIAN_POINT('Ctrl Pts',(29.3268372187205,-1.35483766663846,19.2135801535473));
#48046=CARTESIAN_POINT('Ctrl Pts',(29.6699517271029,-1.47262040644266,19.2333600008011));
#48047=CARTESIAN_POINT('Ctrl Pts',(29.8345144389513,-1.50000000000001,19.2420380722318));
#48048=CARTESIAN_POINT('Ctrl Pts',(30.0000000000001,-1.50000000000001,19.25));
#48049=CARTESIAN_POINT('Ctrl Pts',(30.,-1.50000000000001,19.3125));
#48050=CARTESIAN_POINT('Ctrl Pts',(29.8904115959066,-1.50000000000001,19.3072274254497));
#48051=CARTESIAN_POINT('Ctrl Pts',(29.7809217474217,-1.48799325955223,19.3016260720903));
#48052=CARTESIAN_POINT('Ctrl Pts',(29.479267613868,-1.42071467340943,19.2852438812078));
#48053=CARTESIAN_POINT('Ctrl Pts',(29.2956191224553,-1.33919024824593,19.2741435216794));
#48054=CARTESIAN_POINT('Ctrl Pts',(28.9769843310201,-1.11359538988626,19.2525466742853));
#48055=CARTESIAN_POINT('Ctrl Pts',(28.8433197059369,-0.97404728751911,19.2422393958357));
#48056=CARTESIAN_POINT('Ctrl Pts',(28.6314369352188,-0.64558462894177,19.2229212185382));
#48057=CARTESIAN_POINT('Ctrl Pts',(28.5578261508896,-0.458159789494097,
19.2129533216385));
#48058=CARTESIAN_POINT('Ctrl Pts',(28.4887314396478,-0.0683254796838233,
19.1912958599824));
#48059=CARTESIAN_POINT('Ctrl Pts',(28.4927829468086,0.129998312926432,19.180277871504));
#48060=CARTESIAN_POINT('Ctrl Pts',(28.5757061903925,0.507408017565263,19.1593106656908));
#48061=CARTESIAN_POINT('Ctrl Pts',(28.6513157241137,0.683452060166118,19.1500704896955));
#48062=CARTESIAN_POINT('Ctrl Pts',(28.8692063981292,1.00541452618758,19.1306438179201));
#48063=CARTESIAN_POINT('Ctrl Pts',(29.0123062748592,1.14629480240063,19.119845580885));
#48064=CARTESIAN_POINT('Ctrl Pts',(29.3411837772215,1.36149831072911,19.0980445794436));
#48065=CARTESIAN_POINT('Ctrl Pts',(29.5228193452006,1.43527924918368,19.0872561635921));
#48066=CARTESIAN_POINT('Ctrl Pts',(29.9017346505858,1.50901487689319,19.0669773805809));
#48067=CARTESIAN_POINT('Ctrl Pts',(30.095243866884,1.50920856983617,19.0581733709244));
#48068=CARTESIAN_POINT('Ctrl Pts',(30.4795337547919,1.43522535350299,19.0376291257293));
#48069=CARTESIAN_POINT('Ctrl Pts',(30.6659951148259,1.35877256279477,19.0265343107311));
#48070=CARTESIAN_POINT('Ctrl Pts',(30.9917525251624,1.14161337833726,19.0048291004505));
#48071=CARTESIAN_POINT('Ctrl Pts',(31.12959203788,1.00543319777699,18.9944145110095));
#48072=CARTESIAN_POINT('Ctrl Pts',(31.3495099297643,0.683969951441068,18.9749041718824));
#48073=CARTESIAN_POINT('Ctrl Pts',(31.4277388995994,0.500572833869038,18.9653096018815));
#48074=CARTESIAN_POINT('Ctrl Pts',(31.5085610210805,0.114360476914036,18.9438533598284));
#48075=CARTESIAN_POINT('Ctrl Pts',(31.510521839189,-0.0846024989690804,
18.9327998611683));
#48076=CARTESIAN_POINT('Ctrl Pts',(31.4387139095947,-0.464995267712227,
18.9116669295714));
#48077=CARTESIAN_POINT('Ctrl Pts',(31.3683024334794,-0.643299822803022,
18.9021297086694));
#48078=CARTESIAN_POINT('Ctrl Pts',(31.1599775839064,-0.97159308723095,18.8829874173259));
#48079=CARTESIAN_POINT('Ctrl Pts',(31.021122395481,-1.11661364586043,18.8722783951071));
#48080=CARTESIAN_POINT('Ctrl Pts',(30.6983237124874,-1.34174379218127,18.8504941210548));
#48081=CARTESIAN_POINT('Ctrl Pts',(30.5183853004494,-1.42099198981035,18.8396354913461));
#48082=CARTESIAN_POINT('Ctrl Pts',(30.220307982392,-1.48785706899676,18.8234368763837));
#48083=CARTESIAN_POINT('Ctrl Pts',(30.1102084329115,-1.50000000000001,18.8178024057007));
#48084=CARTESIAN_POINT('Ctrl Pts',(30.,-1.50000000000001,18.8125));
#48085=CARTESIAN_POINT('Origin',(30.,-1.32966554433622E-14,16.));
#48086=CARTESIAN_POINT('',(30.,-1.50000000000001,18.25));
#48087=CARTESIAN_POINT('',(29.9999999999999,-1.50000000000001,18.3125));
#48088=CARTESIAN_POINT('',(30.,-1.50000000000001,16.));
#48089=CARTESIAN_POINT('Ctrl Pts',(30.,-1.50000000000001,18.25));
#48090=CARTESIAN_POINT('Ctrl Pts',(30.0882156275205,-1.50000000000001,18.254244276358));
#48091=CARTESIAN_POINT('Ctrl Pts',(30.1764501130872,-1.49221937550789,18.2587055884823));
#48092=CARTESIAN_POINT('Ctrl Pts',(30.4546079281867,-1.44254775409159,18.2734682298626));
#48093=CARTESIAN_POINT('Ctrl Pts',(30.6370980720641,-1.37175281599007,18.2842148170619));
#48094=CARTESIAN_POINT('Ctrl Pts',(30.9691525442989,-1.16201577961996,18.3060168240942));
#48095=CARTESIAN_POINT('Ctrl Pts',(31.1145075241426,-1.02344071977941,18.3168595260404));
#48096=CARTESIAN_POINT('Ctrl Pts',(31.3375735551139,-0.704962761586156,
18.3364384054093));
#48097=CARTESIAN_POINT('Ctrl Pts',(31.4160050795816,-0.530113102524481,
18.345549272082));
#48098=CARTESIAN_POINT('Ctrl Pts',(31.5048780292219,-0.154342998497877,
18.3664253889724));
#48099=CARTESIAN_POINT('Ctrl Pts',(31.5121437205665,0.0435642244476196,
18.3774202346916));
#48100=CARTESIAN_POINT('Ctrl Pts',(31.4493976248982,0.435280459623824,18.3991822477569));
#48101=CARTESIAN_POINT('Ctrl Pts',(31.3782925123276,0.624894161678516,18.4093783750732));
#48102=CARTESIAN_POINT('Ctrl Pts',(31.1707210215853,0.957071364942045,18.428592307613));
#48103=CARTESIAN_POINT('Ctrl Pts',(31.0393074800838,1.09835818528463,18.4388395784748));
#48104=CARTESIAN_POINT('Ctrl Pts',(30.7245434883219,1.32834442072559,18.4603721746294));
#48105=CARTESIAN_POINT('Ctrl Pts',(30.5424433469957,1.41252449906513,18.4714718072734));
#48106=CARTESIAN_POINT('Ctrl Pts',(30.1611576166725,1.50380428740964,18.492351975203));
#48107=CARTESIAN_POINT('Ctrl Pts',(29.9661847612145,1.51203572283979,18.5012926108002));
#48108=CARTESIAN_POINT('Ctrl Pts',(29.583743920727,1.45401144673963,18.5213045897645));
#48109=CARTESIAN_POINT('Ctrl Pts',(29.3999206687447,1.38827539073469,18.5319747916547));
#48110=CARTESIAN_POINT('Ctrl Pts',(29.0627111089636,1.18787072518152,18.5537655904295));
#48111=CARTESIAN_POINT('Ctrl Pts',(28.9136362676481,1.05327089433686,18.5646768412665));
#48112=CARTESIAN_POINT('Ctrl Pts',(28.6818733006966,0.740747545450625,18.5845087463487));
#48113=CARTESIAN_POINT('Ctrl Pts',(28.5986773683508,0.567862991064222,18.593452056052));
#48114=CARTESIAN_POINT('Ctrl Pts',(28.4999017481138,0.194886335563048,18.6141729813576));
#48115=CARTESIAN_POINT('Ctrl Pts',(28.4872987443723,-0.0022124298529334,
18.6251229127696));
#48116=CARTESIAN_POINT('Ctrl Pts',(28.538885584329,-0.393300822235859,18.6468500456797));
#48117=CARTESIAN_POINT('Ctrl Pts',(28.6038229043615,-0.583241208522858,
18.6573608761808));
#48118=CARTESIAN_POINT('Ctrl Pts',(28.7997809979745,-0.919686600601166,
18.6761346196911));
#48119=CARTESIAN_POINT('Ctrl Pts',(28.9262538190534,-1.06460970419426,18.6862451878989));
#48120=CARTESIAN_POINT('Ctrl Pts',(29.2324514589516,-1.30386842227857,18.7076232042196));
#48121=CARTESIAN_POINT('Ctrl Pts',(29.4110795308611,-1.39369344460164,18.7187125908454));
#48122=CARTESIAN_POINT('Ctrl Pts',(29.7319270119205,-1.48199126728517,18.7366020897721));
#48123=CARTESIAN_POINT('Ctrl Pts',(29.8657845574029,-1.50000000000001,18.7435425565073));
#48124=CARTESIAN_POINT('Ctrl Pts',(30.0000000000002,-1.50000000000001,18.75));
#48125=CARTESIAN_POINT('Ctrl Pts',(30.,-1.50000000000001,18.8125));
#48126=CARTESIAN_POINT('Ctrl Pts',(29.9200694828282,-1.50000000000001,18.8086543411995));
#48127=CARTESIAN_POINT('Ctrl Pts',(29.8400989517173,-1.4936120985387,18.8046293155201));
#48128=CARTESIAN_POINT('Ctrl Pts',(29.5632380932733,-1.44889785862683,18.7900667790378));
#48129=CARTESIAN_POINT('Ctrl Pts',(29.3740258977232,-1.377754564609,18.7789871004233));
#48130=CARTESIAN_POINT('Ctrl Pts',(29.041174726881,-1.16949277461302,18.7571877412774));
#48131=CARTESIAN_POINT('Ctrl Pts',(28.8991316339595,-1.03690216726548,18.7466706173565));
#48132=CARTESIAN_POINT('Ctrl Pts',(28.6710550609186,-0.722648191218263,
18.7269680010074));
#48133=CARTESIAN_POINT('Ctrl Pts',(28.5881967902834,-0.543266122771758,
18.717681451265));
#48134=CARTESIAN_POINT('Ctrl Pts',(28.4956085723343,-0.160873384602161,
18.6964374102556));
#48135=CARTESIAN_POINT('Ctrl Pts',(28.4875239735192,0.0385552236194734,
18.6853580431322));
#48136=CARTESIAN_POINT('Ctrl Pts',(28.5480104653806,0.421875716785893,18.6640624601785));
#48137=CARTESIAN_POINT('Ctrl Pts',(28.6132160700899,0.602522755625134,18.6541515963916));
#48138=CARTESIAN_POINT('Ctrl Pts',(28.8119377533085,0.937035677616922,18.635298569339));
#48139=CARTESIAN_POINT('Ctrl Pts',(28.9464389491764,1.08605274148643,18.6246880146503));
#48140=CARTESIAN_POINT('Ctrl Pts',(29.2628767471001,1.32090830831045,18.6029396282541));
#48141=CARTESIAN_POINT('Ctrl Pts',(29.4409618987283,1.40557199772365,18.5920197332512));
#48142=CARTESIAN_POINT('Ctrl Pts',(29.814809484317,1.50065373381321,18.5713918235674));
#48143=CARTESIAN_POINT('Ctrl Pts',(30.0065604479866,1.51202122412194,18.5625182831912));
#48144=CARTESIAN_POINT('Ctrl Pts',(30.3943911928229,1.4610824148403,18.5424438008558));
#48145=CARTESIAN_POINT('Ctrl Pts',(30.58616263238,1.39524271133166,18.5313883125152));
#48146=CARTESIAN_POINT('Ctrl Pts',(30.9257469654151,1.19593240245758,18.5095136562056));
#48147=CARTESIAN_POINT('Ctrl Pts',(31.0718264769195,1.06698913560375,18.4989036450188));
#48148=CARTESIAN_POINT('Ctrl Pts',(31.3078217753803,0.759832047419874,18.4790171745892));
#48149=CARTESIAN_POINT('Ctrl Pts',(31.3951262846915,0.584269865007977,18.4699594369449));
#48150=CARTESIAN_POINT('Ctrl Pts',(31.4989966927882,0.205709858638526,18.4489283254799));
#48151=CARTESIAN_POINT('Ctrl Pts',(31.5130318328004,0.00600577899638372,
18.4378336543887));
#48152=CARTESIAN_POINT('Ctrl Pts',(31.4635867359632,-0.379900299649008,
18.4163944277973));
#48153=CARTESIAN_POINT('Ctrl Pts',(31.4034385131977,-0.562844950250642,
18.4062308360972));
#48154=CARTESIAN_POINT('Ctrl Pts',(31.213924427377,-0.903263174389702,18.387318712534));
#48155=CARTESIAN_POINT('Ctrl Pts',(31.0836707542498,-1.05603307941032,18.3769705479341));
#48156=CARTESIAN_POINT('Ctrl Pts',(30.7734274797909,-1.30006438227702,18.3552653141303));
#48157=CARTESIAN_POINT('Ctrl Pts',(30.5972523067208,-1.389838711312,18.3442953508018));
#48158=CARTESIAN_POINT('Ctrl Pts',(30.27555179434,-1.4809632576453,18.3262862902852));
#48159=CARTESIAN_POINT('Ctrl Pts',(30.1379932399681,-1.50000000000003,18.3191392028535));
#48160=CARTESIAN_POINT('Ctrl Pts',(29.9999999999998,-1.50000000000001,18.3125));
#48161=CARTESIAN_POINT('Origin',(30.,-1.32966554433622E-14,16.));
#48162=CARTESIAN_POINT('',(30.,-1.50000000000001,17.75));
#48163=CARTESIAN_POINT('',(30.,-1.50000000000001,17.8125));
#48164=CARTESIAN_POINT('',(30.,-1.50000000000001,16.));
#48165=CARTESIAN_POINT('Ctrl Pts',(30.,-1.50000000000001,17.75));
#48166=CARTESIAN_POINT('Ctrl Pts',(30.1165214576707,-1.50000000000002,17.755606141246));
#48167=CARTESIAN_POINT('Ctrl Pts',(30.2328774102524,-1.48642630258387,17.7615813667753));
#48168=CARTESIAN_POINT('Ctrl Pts',(30.5364815251301,-1.41429282343802,17.778192234317));
#48169=CARTESIAN_POINT('Ctrl Pts',(30.7156172892318,-1.33263663661631,17.7890791351975));
#48170=CARTESIAN_POINT('Ctrl Pts',(31.0356297737271,-1.1031687507031,17.8108498509785));
#48171=CARTESIAN_POINT('Ctrl Pts',(31.1725674881258,-0.956358157459637,
17.8215163418689));
#48172=CARTESIAN_POINT('Ctrl Pts',(31.376639002963,-0.625293846242278,17.8405309680715));
#48173=CARTESIAN_POINT('Ctrl Pts',(31.4447439774106,-0.445961069817197,
17.8502243850103));
#48174=CARTESIAN_POINT('Ctrl Pts',(31.5115582160321,-0.0642628969545898,
17.8714298390582));
#48175=CARTESIAN_POINT('Ctrl Pts',(31.5068955968845,0.134928419608339,17.8824960233117));
#48176=CARTESIAN_POINT('Ctrl Pts',(31.4208614242251,0.519471460613856,17.9038595255897));
#48177=CARTESIAN_POINT('Ctrl Pts',(31.3405819882652,0.701086441059189,17.9133091757132));
#48178=CARTESIAN_POINT('Ctrl Pts',(31.1170623100669,1.01937978501502,17.9329047530211));
#48179=CARTESIAN_POINT('Ctrl Pts',(30.9773620677606,1.15399638378434,17.9433654340287));
#48180=CARTESIAN_POINT('Ctrl Pts',(30.6484546459992,1.36726868066811,17.9651142302054));
#48181=CARTESIAN_POINT('Ctrl Pts',(30.4607652253454,1.44139714446346,17.9762035656613));
#48182=CARTESIAN_POINT('Ctrl Pts',(30.0756449322311,1.51026934438856,17.9966457910675));
#48183=CARTESIAN_POINT('Ctrl Pts',(29.8825476840369,1.50759466650969,18.005439964228));
#48184=CARTESIAN_POINT('Ctrl Pts',(29.5047175214704,1.42916638864856,18.025796889674));
#48185=CARTESIAN_POINT('Ctrl Pts',(29.323805468645,1.35298625851431,18.0366171395998));
#48186=CARTESIAN_POINT('Ctrl Pts',(28.9975535579724,1.13341344377778,18.0584131868245));
#48187=CARTESIAN_POINT('Ctrl Pts',(28.8562978602342,0.990703384015885,18.0691735230773));
#48188=CARTESIAN_POINT('Ctrl Pts',(28.6425900107442,0.665955504210131,18.088476321219));
#48189=CARTESIAN_POINT('Ctrl Pts',(28.5692557712623,0.488931672930093,18.0978371292817));
#48190=CARTESIAN_POINT('Ctrl Pts',(28.4911736103312,0.110209786397706,18.118877234089));
#48191=CARTESIAN_POINT('Ctrl Pts',(28.4897399259643,-0.0884146511275797,
18.1299119250627));
#48192=CARTESIAN_POINT('Ctrl Pts',(28.563963673652,-0.476687925939349,18.1514826625522));
#48193=CARTESIAN_POINT('Ctrl Pts',(28.6395954743022,-0.662348456736596,
18.1612794083161));
#48194=CARTESIAN_POINT('Ctrl Pts',(28.8549808751967,-0.987772207975308,
18.1806816918938));
#48195=CARTESIAN_POINT('Ctrl Pts',(28.9904690556508,-1.12587258901724,18.1910364917109));
#48196=CARTESIAN_POINT('Ctrl Pts',(29.3122241078786,-1.34783032180127,18.2126824314563));
#48197=CARTESIAN_POINT('Ctrl Pts',(29.4971108100191,-1.42716337813628,18.2237814930698));
#48198=CARTESIAN_POINT('Ctrl Pts',(29.7935943795659,-1.48934588454492,18.2397733573052));
#48199=CARTESIAN_POINT('Ctrl Pts',(29.8967698772032,-1.50000000000001,18.2450333384012));
#48200=CARTESIAN_POINT('Ctrl Pts',(30.,-1.50000000000001,18.25));
#48201=CARTESIAN_POINT('Ctrl Pts',(29.9999999999998,-1.50000000000001,18.3125));
#48202=CARTESIAN_POINT('Ctrl Pts',(29.9486057940186,-1.50000000000001,18.3100272951118));
#48203=CARTESIAN_POINT('Ctrl Pts',(29.8971583803719,-1.4973588143077,18.3074786639994));
#48204=CARTESIAN_POINT('Ctrl Pts',(29.6480074739756,-1.47161947014145,18.294776403644));
#48205=CARTESIAN_POINT('Ctrl Pts',(29.4562105276991,-1.41203266981329,18.2838933798658));
#48206=CARTESIAN_POINT('Ctrl Pts',(29.1116733937691,-1.22407639141983,18.2620958215476));
#48207=CARTESIAN_POINT('Ctrl Pts',(28.9612380534891,-1.09930641465076,18.2513921651757));
#48208=CARTESIAN_POINT('Ctrl Pts',(28.7165798694464,-0.800027931931824,
18.231307751621));
#48209=CARTESIAN_POINT('Ctrl Pts',(28.6244510402799,-0.628553460673264,
18.2224196367041));
#48210=CARTESIAN_POINT('Ctrl Pts',(28.5083938755392,-0.254315567480426,
18.2016286426378));
#48211=CARTESIAN_POINT('Ctrl Pts',(28.4878541874048,-0.054508044740069,
18.1905282247078));
#48212=CARTESIAN_POINT('Ctrl Pts',(28.5251827599344,0.333985841156563,18.1689452310469));
#48213=CARTESIAN_POINT('Ctrl Pts',(28.5797880070138,0.519280463308488,18.1586510853718));
#48214=CARTESIAN_POINT('Ctrl Pts',(28.7594942565881,0.866593796413574,18.1393559001993));
#48215=CARTESIAN_POINT('Ctrl Pts',(28.8856977548396,1.02381782162173,18.1293391744996));
#48216=CARTESIAN_POINT('Ctrl Pts',(29.1898211855382,1.2775694571787,18.1076583725746));
#48217=CARTESIAN_POINT('Ctrl Pts',(29.3638803222543,1.37256230066096,18.096645258358));
#48218=CARTESIAN_POINT('Ctrl Pts',(29.732534735318,1.48813273455022,18.0756980748094));
#48219=CARTESIAN_POINT('Ctrl Pts',(29.9228794435952,1.51000349618475,18.066488339394));
#48220=CARTESIAN_POINT('Ctrl Pts',(30.3105607244676,1.48091384388274,18.0470279691741));
#48221=CARTESIAN_POINT('Ctrl Pts',(30.5039294602603,1.4267400893485,18.0362196850207));
#48222=CARTESIAN_POINT('Ctrl Pts',(30.8540539626656,1.24831186951753,18.0144179726049));
#48223=CARTESIAN_POINT('Ctrl Pts',(31.0082947964679,1.12740587313612,18.0036385571291));
#48224=CARTESIAN_POINT('Ctrl Pts',(31.2606439376435,0.835225571389926,17.9833812839205));
#48225=CARTESIAN_POINT('Ctrl Pts',(31.3570327509323,0.667298431844612,17.9745721351024));
#48226=CARTESIAN_POINT('Ctrl Pts',(31.4837741625619,0.297001147228916,17.9540000637349));
#48227=CARTESIAN_POINT('Ctrl Pts',(31.5100733842477,0.0972732161684081,
17.9429040675649));
#48228=CARTESIAN_POINT('Ctrl Pts',(31.4835317838137,-0.293194316444828,
17.9212114268642));
#48229=CARTESIAN_POINT('Ctrl Pts',(31.4338905957024,-0.480424140062753,
17.9108097699965));
#48230=CARTESIAN_POINT('Ctrl Pts',(31.2642037542022,-0.83118542637216,17.8913230318682));
#48231=CARTESIAN_POINT('Ctrl Pts',(31.14378015867,-0.99038786521744,17.8816860411746));
#48232=CARTESIAN_POINT('Ctrl Pts',(30.8486060826855,-1.25246692848107,17.8602044978428));
#48233=CARTESIAN_POINT('Ctrl Pts',(30.6769673305094,-1.35296725332812,17.8491548488382));
#48234=CARTESIAN_POINT('Ctrl Pts',(30.3327732686651,-1.47215364288648,17.8292840712733));
#48235=CARTESIAN_POINT('Ctrl Pts',(30.1668871533766,-1.50000000000002,17.8205293619105));
#48236=CARTESIAN_POINT('Ctrl Pts',(29.9999999999999,-1.50000000000001,17.8125));
#48237=CARTESIAN_POINT('Origin',(30.,-1.32966554433622E-14,16.));
#48238=CARTESIAN_POINT('',(29.9999999999999,-1.50000000000001,17.25));
#48239=CARTESIAN_POINT('',(30.,-1.50000000000001,17.3125));
#48240=CARTESIAN_POINT('',(30.,-1.50000000000001,16.));
#48241=CARTESIAN_POINT('Ctrl Pts',(29.9999999999998,-1.50000000000001,17.25));
#48242=CARTESIAN_POINT('Ctrl Pts',(30.1437406795734,-1.50000000000003,17.2569157266704));
#48243=CARTESIAN_POINT('Ctrl Pts',(30.2869532673798,-1.47934432155244,17.2643798143597));
#48244=CARTESIAN_POINT('Ctrl Pts',(30.6133040117111,-1.38286217393555,17.2827614315232));
#48245=CARTESIAN_POINT('Ctrl Pts',(30.7886268831202,-1.29093521604786,17.2937501837148));
#48246=CARTESIAN_POINT('Ctrl Pts',(31.0976621700988,-1.04186059007729,17.3155373905022));
#48247=CARTESIAN_POINT('Ctrl Pts',(31.2270940102629,-0.885739363684009,
17.3257922575731));
#48248=CARTESIAN_POINT('Ctrl Pts',(31.4122925189225,-0.540349731904653,
17.3449805704497));
#48249=CARTESIAN_POINT('Ctrl Pts',(31.4695815451721,-0.356167506723217,
17.3552129162933));
#48250=CARTESIAN_POINT('Ctrl Pts',(31.5127670349393,0.0311250181831806,
17.376729167677));
#48251=CARTESIAN_POINT('Ctrl Pts',(31.4953668358477,0.230908289106308,17.3878282382838));
#48252=CARTESIAN_POINT('Ctrl Pts',(31.3851742993692,0.607249385403804,17.408736076967));
#48253=CARTESIAN_POINT('Ctrl Pts',(31.2953707932844,0.78068569360338,17.4176954906944));
#48254=CARTESIAN_POINT('Ctrl Pts',(31.054895847731,1.08378386704463,17.4376847406135));
#48255=CARTESIAN_POINT('Ctrl Pts',(30.9065553840191,1.21059289157644,17.4483442474051));
#48256=CARTESIAN_POINT('Ctrl Pts',(30.5651448786952,1.40362381134034,17.4701323379946));
#48257=CARTESIAN_POINT('Ctrl Pts',(30.3742618691092,1.46611551598061,17.4810520817598));
#48258=CARTESIAN_POINT('Ctrl Pts',(29.9878426931301,1.51196372025337,17.5009172442622));
#48259=CARTESIAN_POINT('Ctrl Pts',(29.7964276873605,1.49824842026232,17.5098430324513));
#48260=CARTESIAN_POINT('Ctrl Pts',(29.423704438961,1.39861791618851,17.5305432021031));
#48261=CARTESIAN_POINT('Ctrl Pts',(29.2464613140656,1.31164870813791,17.5414866272603));
#48262=CARTESIAN_POINT('Ctrl Pts',(28.9327465597656,1.07261781027188,17.5632199825769));
#48263=CARTESIAN_POINT('Ctrl Pts',(28.8001758891987,0.921899105215767,17.5737833830436));
#48264=CARTESIAN_POINT('Ctrl Pts',(28.6055876448106,0.584753731199478,17.5925136816001));
#48265=CARTESIAN_POINT('Ctrl Pts',(28.5426610065469,0.403064732761888,17.6026075148466));
#48266=CARTESIAN_POINT('Ctrl Pts',(28.487113056257,0.0186136653436067,17.623965907481));
#48267=CARTESIAN_POINT('Ctrl Pts',(28.4978576022209,-0.180959534499292,
17.6350533074722));
#48268=CARTESIAN_POINT('Ctrl Pts',(28.5955062015491,-0.561653522812593,
17.6562029734896));
#48269=CARTESIAN_POINT('Ctrl Pts',(28.6803571582567,-0.739318323214391,
17.6653786075964));
#48270=CARTESIAN_POINT('Ctrl Pts',(28.9119736981394,-1.05041195534416,17.6851637533487));
#48271=CARTESIAN_POINT('Ctrl Pts',(29.0558270731865,-1.1813919096406,17.6957232341464));
#48272=CARTESIAN_POINT('Ctrl Pts',(29.3917078154049,-1.38569020760041,17.7175582566121));
#48273=CARTESIAN_POINT('Ctrl Pts',(29.5820781032457,-1.45448064464283,17.7286282968298));
#48274=CARTESIAN_POINT('Ctrl Pts',(29.8532284268276,-1.49461899708891,17.7427889770903));
#48275=CARTESIAN_POINT('Ctrl Pts',(29.9266397495672,-1.50000000000001,17.7464704533054));
#48276=CARTESIAN_POINT('Ctrl Pts',(30.,-1.50000000000001,17.75));
#48277=CARTESIAN_POINT('Ctrl Pts',(29.9999999999999,-1.50000000000001,17.8125));
#48278=CARTESIAN_POINT('Ctrl Pts',(29.9772840745252,-1.50000000000001,17.811407079526));
#48279=CARTESIAN_POINT('Ctrl Pts',(29.9545509622526,-1.49948399224778,17.8102989986031));
#48280=CARTESIAN_POINT('Ctrl Pts',(29.7331702393738,-1.48941079200354,17.7993680024896));
#48281=CARTESIAN_POINT('Ctrl Pts',(29.5383211874472,-1.44096198242896,17.7886475228419));
#48282=CARTESIAN_POINT('Ctrl Pts',(29.1826189299973,-1.27271128807371,17.7668601596023));
#48283=CARTESIAN_POINT('Ctrl Pts',(29.0244894301944,-1.15598200374574,17.7560096703756));
#48284=CARTESIAN_POINT('Ctrl Pts',(28.764135320164,-0.871290254073719,17.7355752732588));
#48285=CARTESIAN_POINT('Ctrl Pts',(28.6633306533142,-0.706980266162622,
17.7267766814534));
#48286=CARTESIAN_POINT('Ctrl Pts',(28.5256044330412,-0.340872542641299,
17.70643736348));
#48287=CARTESIAN_POINT('Ctrl Pts',(28.4933384090279,-0.141395913779689,
17.6953553285433));
#48288=CARTESIAN_POINT('Ctrl Pts',(28.5086475773052,0.250803035896437,17.6735664980057));
#48289=CARTESIAN_POINT('Ctrl Pts',(28.5530910089168,0.439894111123241,17.6630614382709));
#48290=CARTESIAN_POINT('Ctrl Pts',(28.7124602775381,0.794124581104987,17.6433819677164));
#48291=CARTESIAN_POINT('Ctrl Pts',(28.8270773285161,0.955330804312479,17.6340619682235));
#48292=CARTESIAN_POINT('Ctrl Pts',(29.1130611662184,1.22571784831621,17.6127918131944));
#48293=CARTESIAN_POINT('Ctrl Pts',(29.2820600929988,1.33176716482588,17.6017150341911));
#48294=CARTESIAN_POINT('Ctrl Pts',(29.6446531268203,1.46968030941703,17.5804388480344));
#48295=CARTESIAN_POINT('Ctrl Pts',(29.8337664889299,1.50284763615596,17.5705770145346));
#48296=CARTESIAN_POINT('Ctrl Pts',(30.2227595353817,1.49663210693258,17.5516889242716));
#48297=CARTESIAN_POINT('Ctrl Pts',(30.4189176611452,1.45396403183943,17.5410660377374));
#48298=CARTESIAN_POINT('Ctrl Pts',(30.7799134803451,1.29609345193241,17.5193123244018));
#48299=CARTESIAN_POINT('Ctrl Pts',(30.9418307309724,1.18367445855365,17.5083993272327));
#48300=CARTESIAN_POINT('Ctrl Pts',(31.2101475557693,0.906543829758461,17.4877918549585));
#48301=CARTESIAN_POINT('Ctrl Pts',(31.3153431699375,0.745751786456619,17.478930654803));
#48302=CARTESIAN_POINT('Ctrl Pts',(31.463864637894,0.383898047749162,17.4588276693193));
#48303=CARTESIAN_POINT('Ctrl Pts',(31.5020303054666,0.184838532612863,17.4477688073673));
#48304=CARTESIAN_POINT('Ctrl Pts',(31.4978841524782,-0.208759642694536,
17.4259022420724));
#48305=CARTESIAN_POINT('Ctrl Pts',(31.4586348080642,-0.399547636290809,
17.4153029090948));
#48306=CARTESIAN_POINT('Ctrl Pts',(31.3094217036004,-0.757113584921528,
17.3954381341709));
#48307=CARTESIAN_POINT('Ctrl Pts',(31.200380183046,-0.920271802442848,17.3863568795276));
#48308=CARTESIAN_POINT('Ctrl Pts',(30.923406682912,-1.19858244148629,17.3653001347046));
#48309=CARTESIAN_POINT('Ctrl Pts',(30.7571425046312,-1.30996529750999,17.3542067774745));
#48310=CARTESIAN_POINT('Ctrl Pts',(30.3978227489156,-1.45880886920802,17.3327844540089));
#48311=CARTESIAN_POINT('Ctrl Pts',(30.2092450764931,-1.49754020852369,17.3226356359777));
#48312=CARTESIAN_POINT('Ctrl Pts',(30.0122952852091,-1.49996221637769,17.3130926067305));
#48313=CARTESIAN_POINT('Ctrl Pts',(30.0061468402235,-1.50000000000001,17.3127957399881));
#48314=CARTESIAN_POINT('Ctrl Pts',(30.,-1.50000000000001,17.3125));
#48315=CARTESIAN_POINT('Origin',(30.,-1.32966554433622E-14,16.));
#48316=CARTESIAN_POINT('',(30.,-1.50000000000001,16.75));
#48317=CARTESIAN_POINT('',(30.0000000000001,-1.50000000000001,16.8125));
#48318=CARTESIAN_POINT('',(30.,-1.50000000000001,16.));
#48319=CARTESIAN_POINT('Ctrl Pts',(30.,-1.50000000000001,16.75));
#48320=CARTESIAN_POINT('Ctrl Pts',(30.1733135774153,-1.50000000000002,16.7583385533812));
#48321=CARTESIAN_POINT('Ctrl Pts',(30.3454665850143,-1.46996630625128,16.767455538092));
#48322=CARTESIAN_POINT('Ctrl Pts',(30.6943533649566,-1.34416445320596,16.7877358570363));
#48323=CARTESIAN_POINT('Ctrl Pts',(30.8648984846931,-1.24131259552183,16.7987982089822));
#48324=CARTESIAN_POINT('Ctrl Pts',(31.1561999433551,-0.975703692756434,
16.8201914820235));
#48325=CARTESIAN_POINT('Ctrl Pts',(31.2741613882488,-0.815654351280513,
16.8296858693734));
#48326=CARTESIAN_POINT('Ctrl Pts',(31.4395048489934,-0.463422668720622,
16.8492542961822));
#48327=CARTESIAN_POINT('Ctrl Pts',(31.4869681438372,-0.275392752547583,
16.8597004026363));
#48328=CARTESIAN_POINT('Ctrl Pts',(31.5087956503657,0.115841301406496,16.881435627856));
#48329=CARTESIAN_POINT('Ctrl Pts',(31.4799884843839,0.315484512989904,16.8925269173884));
#48330=CARTESIAN_POINT('Ctrl Pts',(31.3486206066034,0.684034451059388,16.9130019139478));
#48331=CARTESIAN_POINT('Ctrl Pts',(31.2503774147184,0.850433854559545,16.9217976845453));
#48332=CARTESIAN_POINT('Ctrl Pts',(30.994668844219,1.13948462780369,16.9421296570253));
#48333=CARTESIAN_POINT('Ctrl Pts',(30.8387866934565,1.25865700214481,16.9529398842324));
#48334=CARTESIAN_POINT('Ctrl Pts',(30.4862910667067,1.43284604521895,16.9747379225116));
#48335=CARTESIAN_POINT('Ctrl Pts',(30.2922814189341,1.48462820882751,16.9855106094757));
#48336=CARTESIAN_POINT('Ctrl Pts',(29.904287970164,1.50893843055208,17.0048532369201));
#48337=CARTESIAN_POINT('Ctrl Pts',(29.714222422622,1.48472560659638,17.014173768808));
#48338=CARTESIAN_POINT('Ctrl Pts',(29.3467837907597,1.36454370703768,17.0351905543248));
#48339=CARTESIAN_POINT('Ctrl Pts',(29.1737126610206,1.26724866527873,17.0462200829857));
#48340=CARTESIAN_POINT('Ctrl Pts',(28.8733100927186,1.01000510192613,17.0678188628294));
#48341=CARTESIAN_POINT('Ctrl Pts',(28.7495253450837,0.851954282658887,17.0776692065189));
#48342=CARTESIAN_POINT('Ctrl Pts',(28.5739823591041,0.503198698880474,17.0970445167289));
#48343=CARTESIAN_POINT('Ctrl Pts',(28.5214293436323,0.317084997718663,17.1073841667934));
#48344=CARTESIAN_POINT('Ctrl Pts',(28.4885674976081,-0.0722634762162506,
17.1290146375676));
#48345=CARTESIAN_POINT('Ctrl Pts',(28.5114956545415,-0.272057456078969,
17.1401143031155));
#48346=CARTESIAN_POINT('Ctrl Pts',(28.6319945909535,-0.644674063533988,
17.1608152257519));
#48347=CARTESIAN_POINT('Ctrl Pts',(28.7258902835189,-0.814669507709904,
17.1696624095652));
#48348=CARTESIAN_POINT('Ctrl Pts',(28.9737348011573,-1.1110192567928,17.1898187719544));
#48349=CARTESIAN_POINT('Ctrl Pts',(29.1257542814876,-1.2342064357884,17.2005546786951));
#48350=CARTESIAN_POINT('Ctrl Pts',(29.4726321438156,-1.41824610841819,17.2223560607564));
#48351=CARTESIAN_POINT('Ctrl Pts',(29.6650975807577,-1.47560141498182,17.2332092613688));
#48352=CARTESIAN_POINT('Ctrl Pts',(29.9087297050291,-1.49791971441829,17.2455509701752));
#48353=CARTESIAN_POINT('Ctrl Pts',(29.9543886563371,-1.50000000000001,17.2478055232048));
#48354=CARTESIAN_POINT('Ctrl Pts',(29.9999999999998,-1.50000000000001,17.25));
#48355=CARTESIAN_POINT('Ctrl Pts',(30.,-1.50000000000001,17.3125));
#48356=CARTESIAN_POINT('Ctrl Pts',(29.8075276745562,-1.50000000000001,17.3032396709245));
#48357=CARTESIAN_POINT('Ctrl Pts',(29.6167265402445,-1.46295509134636,17.2930307218294));
#48358=CARTESIAN_POINT('Ctrl Pts',(29.2565239800332,-1.31741270776536,17.2716576240826));
#48359=CARTESIAN_POINT('Ctrl Pts',(29.0910935230227,-1.20922562866616,17.2606931508671));
#48360=CARTESIAN_POINT('Ctrl Pts',(28.8152192771185,-0.939380042859163,
17.2399244343056));
#48361=CARTESIAN_POINT('Ctrl Pts',(28.7058473428781,-0.781856067083356,
17.2309364481713));
#48362=CARTESIAN_POINT('Ctrl Pts',(28.5481536416827,-0.426269472803969,
17.211181637378));
#48363=CARTESIAN_POINT('Ctrl Pts',(28.5044938401357,-0.230229772369996,
17.2002905429095));
#48364=CARTESIAN_POINT('Ctrl Pts',(28.4962752409133,0.162097483734217,17.178494584237));
#48365=CARTESIAN_POINT('Ctrl Pts',(28.5297146688179,0.3545967167103,17.167800182405));
#48366=CARTESIAN_POINT('Ctrl Pts',(28.6677231734513,0.715751667501951,17.1477360184722));
#48367=CARTESIAN_POINT('Ctrl Pts',(28.7707689938353,0.881053857184024,17.1388343527704));
#48368=CARTESIAN_POINT('Ctrl Pts',(29.0378553430027,1.16782543883526,17.1180182775366));
#48369=CARTESIAN_POINT('Ctrl Pts',(29.2009578477084,1.28493633443696,17.1069179241867));
#48370=CARTESIAN_POINT('Ctrl Pts',(29.5564777297123,1.44564779283652,17.0853487587108));
#48371=CARTESIAN_POINT('Ctrl Pts',(29.7443345881639,1.49039149544099,17.0750676107666));
#48372=CARTESIAN_POINT('Ctrl Pts',(30.1352017346056,1.50720082969336,17.0557950804638));
#48373=CARTESIAN_POINT('Ctrl Pts',(30.3346031531762,1.47580805773789,17.0457293998907));
#48374=CARTESIAN_POINT('Ctrl Pts',(30.7060862860091,1.33790450333634,17.02402575504));
#48375=CARTESIAN_POINT('Ctrl Pts',(30.8749553104054,1.23409963004519,17.0130175716131));
#48376=CARTESIAN_POINT('Ctrl Pts',(31.1584137835032,0.971677105747927,16.9920901549037));
#48377=CARTESIAN_POINT('Ctrl Pts',(31.271994699923,0.817368296550736,16.9829093498084));
#48378=CARTESIAN_POINT('Ctrl Pts',(31.4394257557863,0.466485221859018,16.9634158456588));
#48379=CARTESIAN_POINT('Ctrl Pts',(31.488516036617,0.271760297088586,16.9525977942827));
#48380=CARTESIAN_POINT('Ctrl Pts',(31.5076810248584,-0.120678265071266,
16.9307956519405));
#48381=CARTESIAN_POINT('Ctrl Pts',(31.4794384691607,-0.314545865899112,
16.9200252296723));
#48382=CARTESIAN_POINT('Ctrl Pts',(31.3513352758344,-0.678794152386266,
16.8997892137563));
#48383=CARTESIAN_POINT('Ctrl Pts',(31.2534603041453,-0.845994238167287,
16.890973963719));
#48384=CARTESIAN_POINT('Ctrl Pts',(30.9950590391717,-1.14001068930543,16.8703745034186));
#48385=CARTESIAN_POINT('Ctrl Pts',(30.8348670617779,-1.26204295887652,16.8592774780469));
#48386=CARTESIAN_POINT('Ctrl Pts',(30.4829704713108,-1.43301939771413,16.8375974999208));
#48387=CARTESIAN_POINT('Ctrl Pts',(30.2958966065637,-1.48299380376918,16.8272087264607));
#48388=CARTESIAN_POINT('Ctrl Pts',(30.0696474084832,-1.49878860163674,16.8158845624575));
#48389=CARTESIAN_POINT('Ctrl Pts',(30.0348056486057,-1.50000000000001,16.8141745875493));
#48390=CARTESIAN_POINT('Ctrl Pts',(30.0000000000002,-1.50000000000001,16.8125));
#48391=CARTESIAN_POINT('Origin',(30.,-1.32966554433622E-14,16.));
#48392=CARTESIAN_POINT('',(30.0000000000023,1.33373412263454,16.1584936490537));
#48393=CARTESIAN_POINT('',(30.,1.1752404735808,16.));
#48394=CARTESIAN_POINT('',(30.,1.17524047358083,16.));
#48395=CARTESIAN_POINT('',(30.,-1.17524047358085,16.));
#48396=CARTESIAN_POINT('Ctrl Pts',(30.,-1.17524047358083,16.));
#48397=CARTESIAN_POINT('Ctrl Pts',(30.0938726776238,-1.17889502189498,16.0036545483141));
#48398=CARTESIAN_POINT('Ctrl Pts',(30.2222715669962,-1.17292308708929,16.0088746896198));
#48399=CARTESIAN_POINT('Ctrl Pts',(30.4821758748939,-1.10061359842964,16.0205734257761));
#48400=CARTESIAN_POINT('Ctrl Pts',(30.5904809486724,-1.05245648363552,16.0257840816621));
#48401=CARTESIAN_POINT('Ctrl Pts',(30.8133642274912,-0.91102859460423,16.0372929849601));
#48402=CARTESIAN_POINT('Ctrl Pts',(30.9213977318432,-0.810903247446717,
16.0434573291476));
#48403=CARTESIAN_POINT('Ctrl Pts',(31.1067869536601,-0.562636269482013,
16.0555173993883));
#48404=CARTESIAN_POINT('Ctrl Pts',(31.1779495349821,-0.411557996758087,
16.0617064115579));
#48405=CARTESIAN_POINT('Ctrl Pts',(31.2569648094213,-0.0966670523057213,
16.075198195417));
#48406=CARTESIAN_POINT('Ctrl Pts',(31.2657685184509,0.0650399419384585,
16.0820144838088));
#48407=CARTESIAN_POINT('Ctrl Pts',(31.2286447980599,0.334175553677255,16.0931820826379));
#48408=CARTESIAN_POINT('Ctrl Pts',(31.1927617340632,0.495209878479218,16.0995752755442));
#48409=CARTESIAN_POINT('Ctrl Pts',(31.0046982036223,0.825162649859306,16.1133508913014));
#48410=CARTESIAN_POINT('Ctrl Pts',(30.8901527526008,0.956864086379422,16.1201881413696));
#48411=CARTESIAN_POINT('Ctrl Pts',(30.6234294043457,1.16264469041258,16.1337830625282));
#48412=CARTESIAN_POINT('Ctrl Pts',(30.4758334589096,1.2374906559331,16.1404068749596));
#48413=CARTESIAN_POINT('Ctrl Pts',(30.2026344427889,1.31649705751482,16.1513204506313));
#48414=CARTESIAN_POINT('Ctrl Pts',(30.094862299376,1.33047991225226,16.1552394386714));
#48415=CARTESIAN_POINT('Ctrl Pts',(30.0000000000046,1.33373412263454,16.1584936490537));
#48416=CARTESIAN_POINT('Origin',(30.,-1.32966554433622E-14,16.));
#48417=CARTESIAN_POINT('Origin',(30.,-1.21864324187371E-14,15.78125));
#48418=CARTESIAN_POINT('',(30.0000000000002,-1.17524047358085,16.0625));
#48419=CARTESIAN_POINT('',(30.,-1.17524047358085,15.78125));
#48420=CARTESIAN_POINT('',(29.1765921258349,-0.838564036615843,16.));
#48421=CARTESIAN_POINT('Ctrl Pts',(30.0000000000004,-1.17524047358085,16.0625));
#48422=CARTESIAN_POINT('Ctrl Pts',(29.8936372832897,-1.17524047358089,16.0559685129868));
#48423=CARTESIAN_POINT('Ctrl Pts',(29.7875857388152,-1.16080842474563,16.0489444642731));
#48424=CARTESIAN_POINT('Ctrl Pts',(29.5893382840682,-1.10559796441283,16.034813132098));
#48425=CARTESIAN_POINT('Ctrl Pts',(29.4977179176601,-1.06709869274158,16.0278219954706));
#48426=CARTESIAN_POINT('Ctrl Pts',(29.3263212626278,-0.968061456605931,
16.0137856854629));
#48427=CARTESIAN_POINT('Ctrl Pts',(29.2472234502441,-0.90791877416947,16.0067961899552));
#48428=CARTESIAN_POINT('Ctrl Pts',(29.176592125834,-0.838564036614912,15.9999999999999));
#48429=CARTESIAN_POINT('Origin',(30.,-1.32966554433622E-14,16.));
#48430=CARTESIAN_POINT('Origin',(30.,-1.21864324187371E-14,15.78125));
#48431=CARTESIAN_POINT('',(30.0000000000002,-1.17524047358085,16.5625));
#48432=CARTESIAN_POINT('',(30.,-1.17524047358085,16.5));
#48433=CARTESIAN_POINT('',(30.,-1.17524047358085,15.78125));
#48434=CARTESIAN_POINT('Ctrl Pts',(30.0000000000004,-1.17524047358085,16.5625));
#48435=CARTESIAN_POINT('Ctrl Pts',(29.8712710011335,-1.17524047358089,16.5545950516279));
#48436=CARTESIAN_POINT('Ctrl Pts',(29.7432544697015,-1.15409887958747,16.5459843057103));
#48437=CARTESIAN_POINT('Ctrl Pts',(29.4749058017838,-1.06268366571272,16.5262646272929));
#48438=CARTESIAN_POINT('Ctrl Pts',(29.3400104190766,-0.984598569044377,
16.515212607152));
#48439=CARTESIAN_POINT('Ctrl Pts',(29.1121607207208,-0.784303734398693,
16.4941196868072));
#48440=CARTESIAN_POINT('Ctrl Pts',(29.0200231478196,-0.665589512335134,
16.4846952710458));
#48441=CARTESIAN_POINT('Ctrl Pts',(28.8817974975863,-0.393869611486594,
16.465428299239));
#48442=CARTESIAN_POINT('Ctrl Pts',(28.83947486215,-0.242215228858268,16.4546748700446));
#48443=CARTESIAN_POINT('Ctrl Pts',(28.8167032491755,0.0653802904577292,
16.4328640487538));
#48444=CARTESIAN_POINT('Ctrl Pts',(28.8351718353917,0.218291541824621,16.422021498172));
#48445=CARTESIAN_POINT('Ctrl Pts',(28.9287391651494,0.506051914833821,16.4016171370023));
#48446=CARTESIAN_POINT('Ctrl Pts',(29.0019741006921,0.638460005621421,16.3928173224174));
#48447=CARTESIAN_POINT('Ctrl Pts',(29.1986594960153,0.873851822283252,16.3723938102577));
#48448=CARTESIAN_POINT('Ctrl Pts',(29.3222166226463,0.972810188230982,16.3612980106481));
#48449=CARTESIAN_POINT('Ctrl Pts',(29.5955374213776,1.11370354874836,16.3395188200451));
#48450=CARTESIAN_POINT('Ctrl Pts',(29.7416409158841,1.1563714827732,16.3290342066007));
#48451=CARTESIAN_POINT('Ctrl Pts',(30.0452139523297,1.18442751027465,16.309397801581));
#48452=CARTESIAN_POINT('Ctrl Pts',(30.1998697024494,1.16832333055968,16.2999812279383));
#48453=CARTESIAN_POINT('Ctrl Pts',(30.4949641982123,1.07710916023858,16.2786262781941));
#48454=CARTESIAN_POINT('Ctrl Pts',(30.6323783558426,1.00262103976947,16.2675471121926));
#48455=CARTESIAN_POINT('Ctrl Pts',(30.8661146099677,0.80826573510396,16.246303290685));
#48456=CARTESIAN_POINT('Ctrl Pts',(30.9615634972897,0.691955855651338,16.2365648418493));
#48457=CARTESIAN_POINT('Ctrl Pts',(31.1071384709944,0.423965303495795,16.217562308738));
#48458=CARTESIAN_POINT('Ctrl Pts',(31.153539286677,0.273539680121433,16.2068960077584));
#48459=CARTESIAN_POINT('Ctrl Pts',(31.1846742020807,-0.0336925499575308,
16.1851109463897));
#48460=CARTESIAN_POINT('Ctrl Pts',(31.1702391074247,-0.187447361382806,
16.174208581095));
#48461=CARTESIAN_POINT('Ctrl Pts',(31.0842361864784,-0.477469105777865,
16.1536438717926));
#48462=CARTESIAN_POINT('Ctrl Pts',(31.0147909316618,-0.611342914691707,
16.1448082262658));
#48463=CARTESIAN_POINT('Ctrl Pts',(30.8246452237759,-0.851973319529638,
16.1246005735716));
#48464=CARTESIAN_POINT('Ctrl Pts',(30.7034471847234,-0.954486386541281,
16.1135236126058));
#48465=CARTESIAN_POINT('Ctrl Pts',(30.4332129266933,-1.10289061678379,16.0916676708875));
#48466=CARTESIAN_POINT('Ctrl Pts',(30.2878849143487,-1.14942616400118,16.0810935566577));
#48467=CARTESIAN_POINT('Ctrl Pts',(30.0919105154022,-1.17254804866719,16.0682394674743));
#48468=CARTESIAN_POINT('Ctrl Pts',(30.0459321343385,-1.17524047358084,16.0653205855228));
#48469=CARTESIAN_POINT('Ctrl Pts',(30.0000000000004,-1.17524047358085,16.0625));
#48470=CARTESIAN_POINT('Ctrl Pts',(29.9999999999986,-1.17524047358085,15.9999999999999));
#48471=CARTESIAN_POINT('Ctrl Pts',(30.1214028111116,-1.17524047358099,16.0074550642242));
#48472=CARTESIAN_POINT('Ctrl Pts',(30.2421537204218,-1.15643017464734,16.0155369920666));
#48473=CARTESIAN_POINT('Ctrl Pts',(30.4776301337898,-1.08113291233427,16.0326666201836));
#48474=CARTESIAN_POINT('Ctrl Pts',(30.5903997908,-1.02391620718435,16.0416200885134));
#48475=CARTESIAN_POINT('Ctrl Pts',(30.8179173133188,-0.858187726048923,
16.0614671043063));
#48476=CARTESIAN_POINT('Ctrl Pts',(30.9244135286053,-0.742266950950034,
16.0721166138301));
#48477=CARTESIAN_POINT('Ctrl Pts',(31.0824458543846,-0.481384401141323,
16.0910702726526));
#48478=CARTESIAN_POINT('Ctrl Pts',(31.1347636661213,-0.340257482296023,
16.1008732014181));
#48479=CARTESIAN_POINT('Ctrl Pts',(31.1847167047507,-0.0402726429290417,
16.1221443686182));
#48480=CARTESIAN_POINT('Ctrl Pts',(31.1797095913038,0.116033015525934,16.1332276080324));
#48481=CARTESIAN_POINT('Ctrl Pts',(31.1096057651028,0.416692954381308,16.1545466448319));
#48482=CARTESIAN_POINT('Ctrl Pts',(31.0456145958404,0.558153128413804,16.1639131875247));
#48483=CARTESIAN_POINT('Ctrl Pts',(30.868452148125,0.806074678480504,16.1835820667589));
#48484=CARTESIAN_POINT('Ctrl Pts',(30.7578944192075,0.910792535772415,16.1940837990854));
#48485=CARTESIAN_POINT('Ctrl Pts',(30.4982839285527,1.07586594639843,16.2158783446996));
#48486=CARTESIAN_POINT('Ctrl Pts',(30.350445183185,1.13268560339106,16.2269712473271));
#48487=CARTESIAN_POINT('Ctrl Pts',(30.0480054721768,1.18378716120051,16.2473551076386));
#48488=CARTESIAN_POINT('Ctrl Pts',(29.8968386090012,1.18026105605562,16.2561569026374));
#48489=CARTESIAN_POINT('Ctrl Pts',(29.6011798659176,1.11599305250821,16.276591159187));
#48490=CARTESIAN_POINT('Ctrl Pts',(29.4597499374869,1.05480717934155,16.2874453099545));
#48491=CARTESIAN_POINT('Ctrl Pts',(29.2055652972218,0.87997645163687,16.3092526000714));
#48492=CARTESIAN_POINT('Ctrl Pts',(29.0959568884663,0.766951615708884,16.3199905502909));
#48493=CARTESIAN_POINT('Ctrl Pts',(28.9310246543964,0.510549118020342,16.3392090818415));
#48494=CARTESIAN_POINT('Ctrl Pts',(28.8749728808886,0.371095429589151,16.348686560472));
#48495=CARTESIAN_POINT('Ctrl Pts',(28.8169184420094,0.0732292943615943,
16.3698074957134));
#48496=CARTESIAN_POINT('Ctrl Pts',(28.817543647408,-0.0827153411142831,
16.3808651359001));
#48497=CARTESIAN_POINT('Ctrl Pts',(28.8792006517981,-0.386085589929172,
16.4023763539327));
#48498=CARTESIAN_POINT('Ctrl Pts',(28.9398691853048,-0.530428612710414,
16.4120388426041));
#48499=CARTESIAN_POINT('Ctrl Pts',(29.1111806434797,-0.783487027051828,
16.4315305472161));
#48500=CARTESIAN_POINT('Ctrl Pts',(29.2187204550675,-0.890749010718532,
16.441937155047));
#48501=CARTESIAN_POINT('Ctrl Pts',(29.4732317621912,-1.06214794881238,16.4636428352494));
#48502=CARTESIAN_POINT('Ctrl Pts',(29.6190899112583,-1.1227476098516,16.4747481293347));
#48503=CARTESIAN_POINT('Ctrl Pts',(29.8476395120001,-1.16783357420714,16.490381294589));
#48504=CARTESIAN_POINT('Ctrl Pts',(29.9238084968367,-1.17524047358085,16.4953212570267));
#48505=CARTESIAN_POINT('Ctrl Pts',(30.,-1.17524047358085,16.5));
#48506=CARTESIAN_POINT('Origin',(30.,-1.21864324187371E-14,15.78125));
#48507=CARTESIAN_POINT('',(30.,-1.17524047358085,17.0625));
#48508=CARTESIAN_POINT('',(30.0000000000001,-1.17524047358085,17.));
#48509=CARTESIAN_POINT('',(30.,-1.17524047358085,15.78125));
#48510=CARTESIAN_POINT('Ctrl Pts',(30.,-1.17524047358085,17.0625));
#48511=CARTESIAN_POINT('Ctrl Pts',(29.8500434788821,-1.17524047358086,17.0532915188657));
#48512=CARTESIAN_POINT('Ctrl Pts',(29.7013448813168,-1.14654165820119,17.0431428036379));
#48513=CARTESIAN_POINT('Ctrl Pts',(29.4194581258723,-1.03331719487298,17.0218185633632));
#48514=CARTESIAN_POINT('Ctrl Pts',(29.2895397758247,-0.948696042884902,
17.0108404436342));
#48515=CARTESIAN_POINT('Ctrl Pts',(29.0728347660888,-0.737413048700427,
16.9900423213744));
#48516=CARTESIAN_POINT('Ctrl Pts',(28.9869014388118,-0.614031092098323,
16.9810393937031));
#48517=CARTESIAN_POINT('Ctrl Pts',(28.8628735458866,-0.335358890642938,
16.9612794518217));
#48518=CARTESIAN_POINT('Ctrl Pts',(28.82846267168,-0.181667965469806,16.9503816165397));
#48519=CARTESIAN_POINT('Ctrl Pts',(28.8217124648996,0.125982959524893,16.9285668665722));
#48520=CARTESIAN_POINT('Ctrl Pts',(28.8478169965895,0.276986540894418,16.9178595840512));
#48521=CARTESIAN_POINT('Ctrl Pts',(28.9558731518301,0.560261316962501,16.89777328523));
#48522=CARTESIAN_POINT('Ctrl Pts',(29.0365906245512,0.68988311408331,16.8888684608487));
#48523=CARTESIAN_POINT('Ctrl Pts',(29.2459337687842,0.914815990147539,16.868038474302));
#48524=CARTESIAN_POINT('Ctrl Pts',(29.3738173058995,1.00667300394252,16.8569287693601));
#48525=CARTESIAN_POINT('Ctrl Pts',(29.6525904034611,1.13269913332434,16.8353418646716));
#48526=CARTESIAN_POINT('Ctrl Pts',(29.7999172965718,1.16777128086699,16.825051424181));
#48527=CARTESIAN_POINT('Ctrl Pts',(30.1064062467105,1.18085135988937,16.8057669130232));
#48528=CARTESIAN_POINT('Ctrl Pts',(30.2627337376109,1.15617395633467,16.7956901530542));
#48529=CARTESIAN_POINT('Ctrl Pts',(30.5539694020395,1.04785975388265,16.7739659051239));
#48530=CARTESIAN_POINT('Ctrl Pts',(30.6863296582614,0.96635719030164,16.7629483992302));
#48531=CARTESIAN_POINT('Ctrl Pts',(30.9084297587183,0.760352988428474,16.7420061299136));
#48532=CARTESIAN_POINT('Ctrl Pts',(30.9973576321623,0.639251123876904,16.7328276824508));
#48533=CARTESIAN_POINT('Ctrl Pts',(31.1283061935881,0.363925745860841,16.7133050553655));
#48534=CARTESIAN_POINT('Ctrl Pts',(31.1665770325591,0.21117202309341,16.7024736747387));
#48535=CARTESIAN_POINT('Ctrl Pts',(31.1811107740607,-0.0965571386816749,
16.6806533771987));
#48536=CARTESIAN_POINT('Ctrl Pts',(31.1587010998539,-0.248535347285279,
16.6698769863224));
#48537=CARTESIAN_POINT('Ctrl Pts',(31.0576874952353,-0.534014859537023,
16.6496343552276));
#48538=CARTESIAN_POINT('Ctrl Pts',(30.9806443499075,-0.664990212129755,
16.6408093669374));
#48539=CARTESIAN_POINT('Ctrl Pts',(30.7774744062741,-0.895077677115282,
16.6201757128395));
#48540=CARTESIAN_POINT('Ctrl Pts',(30.6516599935628,-0.990433515302137,
16.6090690216144));
#48541=CARTESIAN_POINT('Ctrl Pts',(30.3754577665479,-1.12376244747141,16.5873810764564));
#48542=CARTESIAN_POINT('Ctrl Pts',(30.2286809422177,-1.16255586785604,16.5769924813814));
#48543=CARTESIAN_POINT('Ctrl Pts',(30.0523684587312,-1.17436628643519,16.5657468184328));
#48544=CARTESIAN_POINT('Ctrl Pts',(30.0261713894288,-1.17524047358084,16.5641071241452));
#48545=CARTESIAN_POINT('Ctrl Pts',(30.0000000000004,-1.17524047358085,16.5625));
#48546=CARTESIAN_POINT('Ctrl Pts',(30.,-1.17524047358085,16.5));
#48547=CARTESIAN_POINT('Ctrl Pts',(30.073608323754,-1.17524047358085,16.5045201159347));
#48548=CARTESIAN_POINT('Ctrl Pts',(30.1472072638744,-1.16832718018639,16.5092847577281));
#48549=CARTESIAN_POINT('Ctrl Pts',(30.369441082132,-1.12600740446215,16.5244320137475));
#48550=CARTESIAN_POINT('Ctrl Pts',(30.5120596783037,-1.06872004059094,16.5352209411127));
#48551=CARTESIAN_POINT('Ctrl Pts',(30.770540092832,-0.900978381413799,16.5570406907631));
#48552=CARTESIAN_POINT('Ctrl Pts',(30.8831588051698,-0.790914789141215,
16.5678585095693));
#48553=CARTESIAN_POINT('Ctrl Pts',(31.0548992370084,-0.539025681589464,
16.5873351001607));
#48554=CARTESIAN_POINT('Ctrl Pts',(31.1146464335618,-0.40117702528207,16.5965535505072));
#48555=CARTESIAN_POINT('Ctrl Pts',(31.1805926646682,-0.105443065986663,
16.6175232985392));
#48556=CARTESIAN_POINT('Ctrl Pts',(31.1842348048322,0.0500317177053629,
16.6285476227227));
#48557=CARTESIAN_POINT('Ctrl Pts',(31.1309192517252,0.355959076743607,16.650240158982));
#48558=CARTESIAN_POINT('Ctrl Pts',(31.0735350939833,0.503164977113694,16.6602491192277));
#48559=CARTESIAN_POINT('Ctrl Pts',(30.9079406905516,0.761174069707616,16.6795652728517));
#48560=CARTESIAN_POINT('Ctrl Pts',(30.8033709986449,0.870813111599809,16.6898737681392));
#48561=CARTESIAN_POINT('Ctrl Pts',(30.5539282192807,1.04817985026245,16.7114797826742));
#48562=CARTESIAN_POINT('Ctrl Pts',(30.4100715847777,1.1123704677318,16.7225894812308));
#48563=CARTESIAN_POINT('Ctrl Pts',(30.1103488398163,1.179778360742,16.7433846194973));
#48564=CARTESIAN_POINT('Ctrl Pts',(29.957856215253,1.1841771173115,16.7522711143702));
#48565=CARTESIAN_POINT('Ctrl Pts',(29.6587896018035,1.13483145500942,16.7723855875496));
#48566=CARTESIAN_POINT('Ctrl Pts',(29.5151366653971,1.08127741557342,16.7831056710399));
#48567=CARTESIAN_POINT('Ctrl Pts',(29.252747940286,0.920389087589127,16.80492244475));
#48568=CARTESIAN_POINT('Ctrl Pts',(29.137337166046,0.813224513877345,16.8158089365411));
#48569=CARTESIAN_POINT('Ctrl Pts',(28.9591466935998,0.565701034789473,16.8355268312788));
#48570=CARTESIAN_POINT('Ctrl Pts',(28.8958814901205,0.429333298679841,16.8445570602832));
#48571=CARTESIAN_POINT('Ctrl Pts',(28.8225467136217,0.135655218439199,16.8653810311245));
#48572=CARTESIAN_POINT('Ctrl Pts',(28.8149165149687,-0.0192736957647923,
16.8763666490815));
#48573=CARTESIAN_POINT('Ctrl Pts',(28.8600359901893,-0.325574492875678,
16.8980856648912));
#48574=CARTESIAN_POINT('Ctrl Pts',(28.9132427466147,-0.473736863683124,
16.908393840582));
#48575=CARTESIAN_POINT('Ctrl Pts',(29.0711075417097,-0.735375844223955,
16.9273640300312));
#48576=CARTESIAN_POINT('Ctrl Pts',(29.1722563389189,-0.847605887640186,
16.9375543168196));
#48577=CARTESIAN_POINT('Ctrl Pts',(29.4158032201734,-1.03154789820323,16.9590313959273));
#48578=CARTESIAN_POINT('Ctrl Pts',(29.5572939812199,-1.09972494823153,16.97013714563));
#48579=CARTESIAN_POINT('Ctrl Pts',(29.8035947514828,-1.1629117021743,16.9875021095456));
#48580=CARTESIAN_POINT('Ctrl Pts',(29.9016938547886,-1.17524047358087,16.9939632483014));
#48581=CARTESIAN_POINT('Ctrl Pts',(30.0000000000002,-1.17524047358085,17.));
#48582=CARTESIAN_POINT('Origin',(30.,-1.21864324187371E-14,15.78125));
#48583=CARTESIAN_POINT('',(30.,-1.17524047358085,17.5625));
#48584=CARTESIAN_POINT('',(30.0000000000003,-1.17524047358085,17.5));
#48585=CARTESIAN_POINT('',(30.,-1.17524047358085,15.78125));
#48586=CARTESIAN_POINT('Ctrl Pts',(29.9999999999999,-1.17524047358085,17.5625));
#48587=CARTESIAN_POINT('Ctrl Pts',(29.9853039952848,-1.17524047358085,17.5615975525362));
#48588=CARTESIAN_POINT('Ctrl Pts',(29.9705988101993,-1.17496482223763,17.560684768457));
#48589=CARTESIAN_POINT('Ctrl Pts',(29.8000675583885,-1.16856010727206,17.5499857698916));
#48590=CARTESIAN_POINT('Ctrl Pts',(29.6469974366404,-1.13175546252589,17.53928122759));
#48591=CARTESIAN_POINT('Ctrl Pts',(29.3669883306193,-1.00191414640604,17.51748315987));
#48592=CARTESIAN_POINT('Ctrl Pts',(29.2422159979844,-0.911212372037981,
17.5066054643129));
#48593=CARTESIAN_POINT('Ctrl Pts',(29.0365009193432,-0.689398438610156,
17.4861088470066));
#48594=CARTESIAN_POINT('Ctrl Pts',(28.9566358845376,-0.561238966410083,
17.477296037423));
#48595=CARTESIAN_POINT('Ctrl Pts',(28.8466374529962,-0.274946499836391,
17.4569957617908));
#48596=CARTESIAN_POINT('Ctrl Pts',(28.8202715815142,-0.118602529031394,
17.4459098057446));
#48597=CARTESIAN_POINT('Ctrl Pts',(28.8303001790337,0.189193535952347,17.4240847642671));
#48598=CARTESIAN_POINT('Ctrl Pts',(28.8642598713376,0.337792935402822,17.413547956213));
#48599=CARTESIAN_POINT('Ctrl Pts',(28.9875332190235,0.616132121834573,17.3938116275857));
#48600=CARTESIAN_POINT('Ctrl Pts',(29.0764632180064,0.742831294355827,17.3845427667776));
#48601=CARTESIAN_POINT('Ctrl Pts',(29.2992557500629,0.956131495581886,17.3632993064049));
#48602=CARTESIAN_POINT('Ctrl Pts',(29.431365525465,1.04013508414132,17.3522085112739));
#48603=CARTESIAN_POINT('Ctrl Pts',(29.7152659077079,1.14996876403328,17.3308808348058));
#48604=CARTESIAN_POINT('Ctrl Pts',(29.8634965281812,1.17678287245723,17.3209370444755));
#48605=CARTESIAN_POINT('Ctrl Pts',(30.1685869462377,1.17348866615416,17.3020853596773));
#48606=CARTESIAN_POINT('Ctrl Pts',(30.3225567032231,1.14080144678595,17.291471550985));
#48607=CARTESIAN_POINT('Ctrl Pts',(30.6062809135034,1.01837161133764,17.269708112041));
#48608=CARTESIAN_POINT('Ctrl Pts',(30.7337302229979,0.930754504232001,17.2587753925441));
#48609=CARTESIAN_POINT('Ctrl Pts',(30.9451039338725,0.714326579760782,17.2381222459404));
#48610=CARTESIAN_POINT('Ctrl Pts',(31.0280898505948,0.588650269560749,17.2292397036887));
#48611=CARTESIAN_POINT('Ctrl Pts',(31.1457356989614,0.305390771140385,17.209154488167));
#48612=CARTESIAN_POINT('Ctrl Pts',(31.1762844162632,0.149369866697047,17.1980914399405));
#48613=CARTESIAN_POINT('Ctrl Pts',(31.1741828829317,-0.159374372954329,
17.1761991657924));
#48614=CARTESIAN_POINT('Ctrl Pts',(31.1439148549186,-0.309160960295119,
17.1655781772438));
#48615=CARTESIAN_POINT('Ctrl Pts',(31.0278391895685,-0.589863984020037,
17.1456742348851));
#48616=CARTESIAN_POINT('Ctrl Pts',(30.9428415818715,-0.717947604052165,
17.1366104494432));
#48617=CARTESIAN_POINT('Ctrl Pts',(30.7264277284841,-0.936836489561928,
17.1155605491468));
#48618=CARTESIAN_POINT('Ctrl Pts',(30.5962729133073,-1.02460346942682,17.10445637729));
#48619=CARTESIAN_POINT('Ctrl Pts',(30.3147671476396,-1.1421454095557,17.0830024620243));
#48620=CARTESIAN_POINT('Ctrl Pts',(30.1669216238945,-1.17291749944691,17.0728326267459));
#48621=CARTESIAN_POINT('Ctrl Pts',(30.0114948569556,-1.17519832475422,17.06320736676));
#48622=CARTESIAN_POINT('Ctrl Pts',(30.0057465951805,-1.17524047358085,17.0628528850424));
#48623=CARTESIAN_POINT('Ctrl Pts',(30.,-1.17524047358085,17.0625));
#48624=CARTESIAN_POINT('Ctrl Pts',(30.0000000000002,-1.17524047358085,17.));
#48625=CARTESIAN_POINT('Ctrl Pts',(30.0532026451947,-1.17524047358084,17.0032670506819));
#48626=CARTESIAN_POINT('Ctrl Pts',(30.1064500803375,-1.17162840402792,17.0066649131742));
#48627=CARTESIAN_POINT('Ctrl Pts',(30.3094843531048,-1.14383638948677,17.0201181063427));
#48628=CARTESIAN_POINT('Ctrl Pts',(30.4541770343026,-1.0944632219883,17.0307538106078));
#48629=CARTESIAN_POINT('Ctrl Pts',(30.7220117324143,-0.94057404805184,17.0526568626846));
#48630=CARTESIAN_POINT('Ctrl Pts',(30.8414109395085,-0.835479490322757,
17.0637148850572));
#48631=CARTESIAN_POINT('Ctrl Pts',(31.0267110546809,-0.591037021798696,
17.0837601330781));
#48632=CARTESIAN_POINT('Ctrl Pts',(31.0933788874677,-0.456058910657645,
17.0926620146465));
#48633=CARTESIAN_POINT('Ctrl Pts',(31.1737387540124,-0.16438811954927,17.1133436536858));
#48634=CARTESIAN_POINT('Ctrl Pts',(31.1851490819135,-0.0100732318962758,
17.1242857325711));
#48635=CARTESIAN_POINT('Ctrl Pts',(31.1477867853133,0.296739304676255,17.1460410345334));
#48636=CARTESIAN_POINT('Ctrl Pts',(31.0983725298423,0.446176311422578,17.156637235205));
#48637=CARTESIAN_POINT('Ctrl Pts',(30.9473434585081,0.711342976495719,17.1754395336164));
#48638=CARTESIAN_POINT('Ctrl Pts',(30.8493881217234,0.825870653120103,17.1854545855523));
#48639=CARTESIAN_POINT('Ctrl Pts',(30.6112318646727,1.01569990967513,17.2068093638384));
#48640=CARTESIAN_POINT('Ctrl Pts',(30.4719800604887,1.0874234537732,17.2179033608764));
#48641=CARTESIAN_POINT('Ctrl Pts',(30.1755334231398,1.17210985582506,17.2391099087106));
#48642=CARTESIAN_POINT('Ctrl Pts',(30.0214941231326,1.18498177307235,17.2483347304275));
#48643=CARTESIAN_POINT('Ctrl Pts',(29.7191034448427,1.1511421779865,17.2681035786673));
#48644=CARTESIAN_POINT('Ctrl Pts',(29.5735822533488,1.10552321949792,17.2786570590835));
#48645=CARTESIAN_POINT('Ctrl Pts',(29.3025973986068,0.958895356196027,17.3004961143537));
#48646=CARTESIAN_POINT('Ctrl Pts',(29.1808306521913,0.85722095928387,17.3115782643265));
#48647=CARTESIAN_POINT('Ctrl Pts',(28.9891285746956,0.617827320312939,17.3318376420863));
#48648=CARTESIAN_POINT('Ctrl Pts',(28.918785924397,0.484304768960115,17.3406591721831));
#48649=CARTESIAN_POINT('Ctrl Pts',(28.8309775509286,0.194817478373176,17.361185984716));
#48650=CARTESIAN_POINT('Ctrl Pts',(28.8155773691905,0.0412543792472424,
17.3720747561758));
#48651=CARTESIAN_POINT('Ctrl Pts',(28.8447173912596,-0.266085346871024,
17.3938674398171));
#48652=CARTESIAN_POINT('Ctrl Pts',(28.8901486797617,-0.416814366578493,
17.4045552538642));
#48653=CARTESIAN_POINT('Ctrl Pts',(29.0339735284972,-0.685700945089528,
17.423621321941));
#48654=CARTESIAN_POINT('Ctrl Pts',(29.1286271803726,-0.802582950507819,
17.4332789203108));
#48655=CARTESIAN_POINT('Ctrl Pts',(29.3609543925255,-0.998368963070605,
17.45448693977));
#48656=CARTESIAN_POINT('Ctrl Pts',(29.4977729352126,-1.07372697749091,17.4655603714348));
#48657=CARTESIAN_POINT('Ctrl Pts',(29.7602131749374,-1.15682002764215,17.484622175217));
#48658=CARTESIAN_POINT('Ctrl Pts',(29.879837116137,-1.1752404735809,17.4926210768238));
#48659=CARTESIAN_POINT('Ctrl Pts',(30.0000000000005,-1.17524047358085,17.5));
#48660=CARTESIAN_POINT('Origin',(30.,-1.21864324187371E-14,15.78125));
#48661=CARTESIAN_POINT('',(29.9999999999998,-1.17524047358085,18.0625));
#48662=CARTESIAN_POINT('',(30.,-1.17524047358085,18.));
#48663=CARTESIAN_POINT('',(30.,-1.17524047358085,15.78125));
#48664=CARTESIAN_POINT('Ctrl Pts',(29.9999999999995,-1.17524047358085,18.0625));
#48665=CARTESIAN_POINT('Ctrl Pts',(29.9645254254169,-1.17524047358085,18.0603215888955));
#48666=CARTESIAN_POINT('Ctrl Pts',(29.929015100466,-1.17363438891304,18.0580840407407));
#48667=CARTESIAN_POINT('Ctrl Pts',(29.7382382629168,-1.15628718990462,18.0457538558988));
#48668=CARTESIAN_POINT('Ctrl Pts',(29.5872914572777,-1.11138228831714,18.0348925171245));
#48669=CARTESIAN_POINT('Ctrl Pts',(29.315235711072,-0.96715790012321,18.0130729130751));
#48670=CARTESIAN_POINT('Ctrl Pts',(29.1959940490486,-0.870565282945587,
18.0023259907432));
#48671=CARTESIAN_POINT('Ctrl Pts',(29.0016396885941,-0.638155310236294,
17.9821513395236));
#48672=CARTESIAN_POINT('Ctrl Pts',(28.9280461950896,-0.504858426874225,
17.9732982357813));
#48673=CARTESIAN_POINT('Ctrl Pts',(28.8336569152641,-0.212647772939916,
17.9525783164326));
#48674=CARTESIAN_POINT('Ctrl Pts',(28.8157570812338,-0.0559802507924535,
17.9414694181781));
#48675=CARTESIAN_POINT('Ctrl Pts',(28.841716723376,0.249283949869151,17.9198239048041));
#48676=CARTESIAN_POINT('Ctrl Pts',(28.8830393993721,0.395199804389445,17.9094773801424));
#48677=CARTESIAN_POINT('Ctrl Pts',(29.0209639808548,0.668562290928518,17.8900939367334));
#48678=CARTESIAN_POINT('Ctrl Pts',(29.1181759703235,0.792402282110926,17.8802238069267));
#48679=CARTESIAN_POINT('Ctrl Pts',(29.3540263292146,0.993822233016871,17.8585996950535));
#48680=CARTESIAN_POINT('Ctrl Pts',(29.4898462594122,1.06991069869815,17.8475616886318));
#48681=CARTESIAN_POINT('Ctrl Pts',(29.7781387158762,1.16368326761588,17.8265337315072));
#48682=CARTESIAN_POINT('Ctrl Pts',(29.9272121099849,1.18239624377936,17.817223433802));
#48683=CARTESIAN_POINT('Ctrl Pts',(30.231427568808,1.16273575019751,17.7978452321702));
#48684=CARTESIAN_POINT('Ctrl Pts',(30.3834744853667,1.1218012564522,17.7870571039388));
#48685=CARTESIAN_POINT('Ctrl Pts',(30.6595367886018,0.984593855649311,17.7652402449678));
#48686=CARTESIAN_POINT('Ctrl Pts',(30.78153371397,0.890859052478792,17.7544254485094));
#48687=CARTESIAN_POINT('Ctrl Pts',(30.9814968973686,0.663646825098318,17.7340906520159));
#48688=CARTESIAN_POINT('Ctrl Pts',(31.0581916579204,0.532910080900297,17.7252873077101));
#48689=CARTESIAN_POINT('Ctrl Pts',(31.1603311881744,0.243593094566313,17.7047725710215));
#48690=CARTESIAN_POINT('Ctrl Pts',(31.1824208985569,0.0870303935487086,
17.6936711053685));
#48691=CARTESIAN_POINT('Ctrl Pts',(31.1643265939555,-0.219589452433675,
17.6719294666093));
#48692=CARTESIAN_POINT('Ctrl Pts',(31.126629625228,-0.366880394031282,17.6614854379963));
#48693=CARTESIAN_POINT('Ctrl Pts',(30.9959732548856,-0.642739672382233,
17.6419249533869));
#48694=CARTESIAN_POINT('Ctrl Pts',(30.9029171297163,-0.76800751067264,17.6323839709445));
#48695=CARTESIAN_POINT('Ctrl Pts',(30.6735549835348,-0.97540763183831,17.6109462657373));
#48696=CARTESIAN_POINT('Ctrl Pts',(30.5395284406378,-1.05546393695081,17.5998777123224));
#48697=CARTESIAN_POINT('Ctrl Pts',(30.2672665806154,-1.15230702152505,17.5797252955804));
#48698=CARTESIAN_POINT('Ctrl Pts',(30.1340643685791,-1.17524047358085,17.5707325810151));
#48699=CARTESIAN_POINT('Ctrl Pts',(29.9999999999999,-1.17524047358085,17.5625));
#48700=CARTESIAN_POINT('Ctrl Pts',(30.0000000000005,-1.17524047358085,17.5));
#48701=CARTESIAN_POINT('Ctrl Pts',(30.033668671514,-1.17524047358084,17.5020675147979));
#48702=CARTESIAN_POINT('Ctrl Pts',(30.0673733741507,-1.17379373295066,17.504188534545));
#48703=CARTESIAN_POINT('Ctrl Pts',(30.2512194694897,-1.15793171152857,17.5160404635345));
#48704=CARTESIAN_POINT('Ctrl Pts',(30.3974945854731,-1.11619705184184,17.5265025277916));
#48705=CARTESIAN_POINT('Ctrl Pts',(30.6715286389123,-0.977122112696594,
17.5482610478741));
#48706=CARTESIAN_POINT('Ctrl Pts',(30.7956391457863,-0.8790277241657,17.559360198049));
#48707=CARTESIAN_POINT('Ctrl Pts',(30.9938921656194,-0.644908297614295,
17.579834863399));
#48708=CARTESIAN_POINT('Ctrl Pts',(31.0680432549382,-0.51284781086492,17.5886352571811));
#48709=CARTESIAN_POINT('Ctrl Pts',(31.1634155774875,-0.225635628704456,
17.6090007475224));
#48710=CARTESIAN_POINT('Ctrl Pts',(31.1828424433655,-0.0729412614644995,
17.6198279193986));
#48711=CARTESIAN_POINT('Ctrl Pts',(31.1620678214981,0.234707081573543,17.6416424862861));
#48712=CARTESIAN_POINT('Ctrl Pts',(31.120724241081,0.386638085314584,17.6524155299848));
#48713=CARTESIAN_POINT('Ctrl Pts',(30.9842587758127,0.659238100700609,17.6717449084903));
#48714=CARTESIAN_POINT('Ctrl Pts',(30.8929036275603,0.778529076192667,17.6811039637465));
#48715=CARTESIAN_POINT('Ctrl Pts',(30.6664518626416,0.98022024209091,17.7021605454119));
#48716=CARTESIAN_POINT('Ctrl Pts',(30.5321662358965,1.05914504613978,17.7132048926221));
#48717=CARTESIAN_POINT('Ctrl Pts',(30.2394356343315,1.16107865610412,17.7347947253164));
#48718=CARTESIAN_POINT('Ctrl Pts',(30.0837395746803,1.18253750639866,17.7445990404306));
#48719=CARTESIAN_POINT('Ctrl Pts',(29.7783085058998,1.16389753061854,17.7640157086725));
#48720=CARTESIAN_POINT('Ctrl Pts',(29.6313883618284,1.12601470121935,17.7743808208261));
#48721=CARTESIAN_POINT('Ctrl Pts',(29.3545393068819,0.994469365010162,17.7960452510406));
#48722=CARTESIAN_POINT('Ctrl Pts',(29.2282096618696,0.899966183720928,17.8071533516094));
#48723=CARTESIAN_POINT('Ctrl Pts',(29.0235241701317,0.671134004766118,17.8278355674102));
#48724=CARTESIAN_POINT('Ctrl Pts',(28.9455840780504,0.540492245953914,17.8366750601186));
#48725=CARTESIAN_POINT('Ctrl Pts',(28.8428376707835,0.255550540540784,17.8568795566889));
#48726=CARTESIAN_POINT('Ctrl Pts',(28.819515816648,0.103803872119581,17.8676395296357));
#48727=CARTESIAN_POINT('Ctrl Pts',(28.8321334408652,-0.203924479248023,
17.8894597697118));
#48728=CARTESIAN_POINT('Ctrl Pts',(28.8694569005926,-0.356918085677502,
17.9003081598831));
#48729=CARTESIAN_POINT('Ctrl Pts',(28.9987062002081,-0.633072693900888,
17.9198895855878));
#48730=CARTESIAN_POINT('Ctrl Pts',(29.0868937988439,-0.754733453808526,
17.9290197269592));
#48731=CARTESIAN_POINT('Ctrl Pts',(29.3076626510103,-0.962047131353844,
17.9499266732212));
#48732=CARTESIAN_POINT('Ctrl Pts',(29.439425880769,-1.04432722335896,17.9609350833968));
#48733=CARTESIAN_POINT('Ctrl Pts',(29.7165797609128,-1.14942800619046,17.981680673977));
#48734=CARTESIAN_POINT('Ctrl Pts',(29.857771536572,-1.17524047358086,17.9912660809114));
#48735=CARTESIAN_POINT('Ctrl Pts',(30.0000000000001,-1.17524047358085,18.));
#48736=CARTESIAN_POINT('Origin',(30.,-1.21864324187371E-14,15.78125));
#48737=CARTESIAN_POINT('',(29.9999999999999,-1.17524047358085,18.5625));
#48738=CARTESIAN_POINT('',(30.,-1.17524047358085,18.5));
#48739=CARTESIAN_POINT('',(30.,-1.17524047358085,15.78125));
#48740=CARTESIAN_POINT('Ctrl Pts',(29.9999999999998,-1.17524047358085,18.5625));
#48741=CARTESIAN_POINT('Ctrl Pts',(29.9448799883238,-1.17524047358085,18.5591152083026));
#48742=CARTESIAN_POINT('Ctrl Pts',(29.8897199177939,-1.17136342891428,18.5555905009623));
#48743=CARTESIAN_POINT('Ctrl Pts',(29.6792216999803,-1.14149919812993,18.5416054964814));
#48744=CARTESIAN_POINT('Ctrl Pts',(29.5295600411529,-1.08838822549331,18.5305321396985));
#48745=CARTESIAN_POINT('Ctrl Pts',(29.2651715824486,-0.929562358041593,
18.5086656889335));
#48746=CARTESIAN_POINT('Ctrl Pts',(29.1517563578462,-0.827380506823195,
18.4980783953365));
#48747=CARTESIAN_POINT('Ctrl Pts',(28.9690035888602,-0.584433789122884,
18.4782426038757));
#48748=CARTESIAN_POINT('Ctrl Pts',(28.9018681826973,-0.445680079983302,
18.4691020486872));
#48749=CARTESIAN_POINT('Ctrl Pts',(28.8237798560613,-0.147691887525462,
18.4479724586759));
#48750=CARTESIAN_POINT('Ctrl Pts',(28.8145788645707,0.00884554058040183,
18.4368727850612));
#48751=CARTESIAN_POINT('Ctrl Pts',(28.8567482751501,0.310649796974269,18.4154726075955));
#48752=CARTESIAN_POINT('Ctrl Pts',(28.9054833559201,0.453415390787842,18.4053494599629));
#48753=CARTESIAN_POINT('Ctrl Pts',(29.0569965845258,0.718468314308288,18.3865552266777));
#48754=CARTESIAN_POINT('Ctrl Pts',(29.1604683184012,0.83707730034545,18.3760428358642));
#48755=CARTESIAN_POINT('Ctrl Pts',(29.4058248734932,1.0255154952049,18.3542952223602));
#48756=CARTESIAN_POINT('Ctrl Pts',(29.544631443668,1.0942445155017,18.3433347331662));
#48757=CARTESIAN_POINT('Ctrl Pts',(29.8366929775619,1.17335763361873,18.3225950580774));
#48758=CARTESIAN_POINT('Ctrl Pts',(29.986714530993,1.18458952273488,18.3136472884771));
#48759=CARTESIAN_POINT('Ctrl Pts',(30.2898186404183,1.14957783224746,18.2937930749288));
#48760=CARTESIAN_POINT('Ctrl Pts',(30.4396462258347,1.10100720458506,18.2828705011767));
#48761=CARTESIAN_POINT('Ctrl Pts',(30.7078144176317,0.95036138884417,18.2610619591969));
#48762=CARTESIAN_POINT('Ctrl Pts',(30.8244348872713,0.851181456147988,18.250384268188));
#48763=CARTESIAN_POINT('Ctrl Pts',(31.0135314789776,0.613960284599869,18.2303619093383));
#48764=CARTESIAN_POINT('Ctrl Pts',(31.0842069749077,0.478217809229905,18.2214092168781));
#48765=CARTESIAN_POINT('Ctrl Pts',(31.1712537448649,0.183351777827692,18.2005010114207));
#48766=CARTESIAN_POINT('Ctrl Pts',(31.1852144107931,0.026684835425868,18.1893921542744));
#48767=CARTESIAN_POINT('Ctrl Pts',(31.151894218573,-0.277120859310672,18.1678500598715));
#48768=CARTESIAN_POINT('Ctrl Pts',(31.1071955868466,-0.421659698179358,
18.1576011759113));
#48769=CARTESIAN_POINT('Ctrl Pts',(30.9623980704004,-0.692609521716023,
18.1383888083414));
#48770=CARTESIAN_POINT('Ctrl Pts',(30.8611688824271,-0.815074867780112,
18.1281515944925));
#48771=CARTESIAN_POINT('Ctrl Pts',(30.6191698348665,-1.010677278137,18.1063561595037));
#48772=CARTESIAN_POINT('Ctrl Pts',(30.481744547401,-1.08294295672688,18.0953551039148));
#48773=CARTESIAN_POINT('Ctrl Pts',(30.2255864017037,-1.15894806928573,18.0769303627887));
#48774=CARTESIAN_POINT('Ctrl Pts',(30.1130100641695,-1.17524047358085,18.0694396851576));
#48775=CARTESIAN_POINT('Ctrl Pts',(29.9999999999995,-1.17524047358085,18.0625));
#48776=CARTESIAN_POINT('Ctrl Pts',(30.0000000000001,-1.17524047358085,18.));
#48777=CARTESIAN_POINT('Ctrl Pts',(30.0145244311397,-1.17524047358085,18.0008919115297));
#48778=CARTESIAN_POINT('Ctrl Pts',(30.0290585224951,-1.1749712210064,18.0017939622806));
#48779=CARTESIAN_POINT('Ctrl Pts',(30.1935181174434,-1.16886648233729,18.0121094792412));
#48780=CARTESIAN_POINT('Ctrl Pts',(30.3409577753235,-1.13464684718278,18.022376619604));
#48781=CARTESIAN_POINT('Ctrl Pts',(30.6202928748417,-1.01029888563142,18.0439385382044));
#48782=CARTESIAN_POINT('Ctrl Pts',(30.7486368752819,-0.919248747112441,
18.055047912384));
#48783=CARTESIAN_POINT('Ctrl Pts',(30.9593869332128,-0.695506306327382,
18.0759220888488));
#48784=CARTESIAN_POINT('Ctrl Pts',(31.0409497614259,-0.566191331080132,
18.084852802908));
#48785=CARTESIAN_POINT('Ctrl Pts',(31.1506054030915,-0.283424289026694,
18.1049030995926));
#48786=CARTESIAN_POINT('Ctrl Pts',(31.1775442736485,-0.132654402671248,
18.1155938113905));
#48787=CARTESIAN_POINT('Ctrl Pts',(31.1725598607287,0.174951078257229,18.1374053390341));
#48788=CARTESIAN_POINT('Ctrl Pts',(31.1390289434739,0.328840847644919,18.148317273857));
#48789=CARTESIAN_POINT('Ctrl Pts',(31.0165781905916,0.608264397522364,18.1681304919571));
#48790=CARTESIAN_POINT('Ctrl Pts',(30.9313199722933,0.732167484063905,18.1771012136858));
#48791=CARTESIAN_POINT('Ctrl Pts',(30.7158345492886,0.944633593585631,18.1978663898215));
#48792=CARTESIAN_POINT('Ctrl Pts',(30.5864762504196,1.02994768568734,18.208834685427));
#48793=CARTESIAN_POINT('Ctrl Pts',(30.3000115977578,1.14695518635867,18.2305741665317));
#48794=CARTESIAN_POINT('Ctrl Pts',(30.1454149851266,1.17656763909288,18.2410233510493));
#48795=CARTESIAN_POINT('Ctrl Pts',(29.8400425266379,1.17387642244061,18.2598709770579));
#48796=CARTESIAN_POINT('Ctrl Pts',(29.6921041520777,1.14400535739554,18.2700145693908));
#48797=CARTESIAN_POINT('Ctrl Pts',(29.4100579886469,1.02824734385133,18.2914384223622));
#48798=CARTESIAN_POINT('Ctrl Pts',(29.2794434337127,0.941343746808855,18.3025402156205));
#48799=CARTESIAN_POINT('Ctrl Pts',(29.061555804029,0.723734320476339,18.3236352554819));
#48800=CARTESIAN_POINT('Ctrl Pts',(28.9756558249342,0.595970538008072,18.3327412345668));
#48801=CARTESIAN_POINT('Ctrl Pts',(28.8579142725366,0.315809924655313,18.3526067159761));
#48802=CARTESIAN_POINT('Ctrl Pts',(28.8267878271973,0.166290213657428,18.3632087809973));
#48803=CARTESIAN_POINT('Ctrl Pts',(28.8228465258246,-0.142252171918218,
18.3850867421828));
#48804=CARTESIAN_POINT('Ctrl Pts',(28.8524261916584,-0.298357527348321,
18.3961557786154));
#48805=CARTESIAN_POINT('Ctrl Pts',(28.9683032793772,-0.582326286319503,
18.4162912860112));
#48806=CARTESIAN_POINT('Ctrl Pts',(29.0505638845767,-0.708574806470949,
18.4251522948912));
#48807=CARTESIAN_POINT('Ctrl Pts',(29.2606233813178,-0.926260402003281,
18.4457693278011));
#48808=CARTESIAN_POINT('Ctrl Pts',(29.3874559625716,-1.01460273580079,18.4566898874478));
#48809=CARTESIAN_POINT('Ctrl Pts',(29.670332667393,-1.13876808411125,18.4784628134696));
#48810=CARTESIAN_POINT('Ctrl Pts',(29.8241031351402,-1.17241612945781,18.4890984491449));
#48811=CARTESIAN_POINT('Ctrl Pts',(29.9866645216768,-1.17518374723239,18.4991790881359));
#48812=CARTESIAN_POINT('Ctrl Pts',(29.9933333092278,-1.17524047358085,18.4995906140276));
#48813=CARTESIAN_POINT('Ctrl Pts',(30.,-1.17524047358085,18.5));
#48814=CARTESIAN_POINT('Origin',(30.,-1.21864324187371E-14,15.78125));
#48815=CARTESIAN_POINT('',(30.,-1.17524047358085,19.0625));
#48816=CARTESIAN_POINT('',(29.9999999999998,-1.17524047358085,18.9999999999999));
#48817=CARTESIAN_POINT('',(30.,-1.17524047358085,15.78125));
#48818=CARTESIAN_POINT('Ctrl Pts',(30.,-1.17524047358085,19.0625));
#48819=CARTESIAN_POINT('Ctrl Pts',(29.9235115354988,-1.17524047358085,19.0578030213218));
#48820=CARTESIAN_POINT('Ctrl Pts',(29.84704716558,-1.16777574293408,19.0528428696387));
#48821=CARTESIAN_POINT('Ctrl Pts',(29.6182505756017,-1.12246086107485,19.0371864213689));
#48822=CARTESIAN_POINT('Ctrl Pts',(29.4724485773796,-1.06175746863862,19.0260808977107));
#48823=CARTESIAN_POINT('Ctrl Pts',(29.2180805672544,-0.890185564352666,
19.0043778847458));
#48824=CARTESIAN_POINT('Ctrl Pts',(29.1106251205818,-0.782854361416016,
18.9939740034863));
#48825=CARTESIAN_POINT('Ctrl Pts',(28.9394765622835,-0.529653947083613,
18.9744872677464));
#48826=CARTESIAN_POINT('Ctrl Pts',(28.8789010658566,-0.385229961133875,
18.9648156834562));
#48827=CARTESIAN_POINT('Ctrl Pts',(28.8174805423046,-0.0817855742350542,
18.9432992084794));
#48828=CARTESIAN_POINT('Ctrl Pts',(28.8169771571136,0.0741472763924911,
18.9322424039265));
#48829=CARTESIAN_POINT('Ctrl Pts',(28.8752567923883,0.371953492557534,18.9111257173945));
#48830=CARTESIAN_POINT('Ctrl Pts',(28.9314131886074,0.511361040736907,18.9016564371649));
#48831=CARTESIAN_POINT('Ctrl Pts',(29.0965385184593,0.767636822695621,18.8824305405978));
#48832=CARTESIAN_POINT('Ctrl Pts',(29.2062331582591,0.880579083863968,18.8716902227143));
#48833=CARTESIAN_POINT('Ctrl Pts',(29.4605419802015,1.05521085002794,18.8498823608196));
#48834=CARTESIAN_POINT('Ctrl Pts',(29.6020069692685,1.11628678080371,18.8390299549287));
#48835=CARTESIAN_POINT('Ctrl Pts',(29.8977163387384,1.18033932535056,18.8186002283572));
#48836=CARTESIAN_POINT('Ctrl Pts',(30.0489012110254,1.18375239923791,18.8097988699583));
#48837=CARTESIAN_POINT('Ctrl Pts',(30.351304458352,1.13241772416719,18.7894089839185));
#48838=CARTESIAN_POINT('Ctrl Pts',(30.4990888608278,1.07549105419273,18.7783156243515));
#48839=CARTESIAN_POINT('Ctrl Pts',(30.7585582244441,0.910237971254531,18.7565233749656));
#48840=CARTESIAN_POINT('Ctrl Pts',(30.869032001546,0.80544751578808,18.7460242240482));
#48841=CARTESIAN_POINT('Ctrl Pts',(31.0460310070461,0.557381504027199,18.7263602597134));
#48842=CARTESIAN_POINT('Ctrl Pts',(31.1099298338315,0.41584148204013,18.7169862690792));
#48843=CARTESIAN_POINT('Ctrl Pts',(31.1797989523814,0.115104609901925,18.6956617771348));
#48844=CARTESIAN_POINT('Ctrl Pts',(31.1846835245906,-0.0411926090939851,
18.6845791361414));
#48845=CARTESIAN_POINT('Ctrl Pts',(31.134503841219,-0.341119161052378,18.6633121019541));
#48846=CARTESIAN_POINT('Ctrl Pts',(31.082082323541,-0.482198917475646,18.6535190714213));
#48847=CARTESIAN_POINT('Ctrl Pts',(30.9238582069445,-0.74295817680152,18.6345580062792));
#48848=CARTESIAN_POINT('Ctrl Pts',(30.8172746962663,-0.85879990158245,18.6239059387776));
#48849=CARTESIAN_POINT('Ctrl Pts',(30.5674863902569,-1.04046451233651,18.6021263306283));
#48850=CARTESIAN_POINT('Ctrl Pts',(30.4273223446806,-1.10544579712631,18.5912153532567));
#48851=CARTESIAN_POINT('Ctrl Pts',(30.1872213612661,-1.164041447155,18.5743938756203));
#48852=CARTESIAN_POINT('Ctrl Pts',(30.0936931422672,-1.17524047358085,18.5682534779185));
#48853=CARTESIAN_POINT('Ctrl Pts',(29.9999999999998,-1.17524047358085,18.5625));
#48854=CARTESIAN_POINT('Ctrl Pts',(30.,-1.17524047358085,18.5));
#48855=CARTESIAN_POINT('Ctrl Pts',(30.1423690472132,-1.17524047358085,18.5087425520117));
#48856=CARTESIAN_POINT('Ctrl Pts',(30.2836710124158,-1.14937338085773,18.5183366621019));
#48857=CARTESIAN_POINT('Ctrl Pts',(30.561858730089,-1.04379601878612,18.5391626347549));
#48858=CARTESIAN_POINT('Ctrl Pts',(30.6944274791866,-0.96071277520592,18.550248984724));
#48859=CARTESIAN_POINT('Ctrl Pts',(30.9187624839086,-0.748784365111015,
18.5715385296331));
#48860=CARTESIAN_POINT('Ctrl Pts',(31.0086541273172,-0.622420436396325,
18.5808657390843));
#48861=CARTESIAN_POINT('Ctrl Pts',(31.1336634286392,-0.344659292163419,
18.6005610801994));
#48862=CARTESIAN_POINT('Ctrl Pts',(31.1685065373813,-0.196359387070609,
18.6110766518651));
#48863=CARTESIAN_POINT('Ctrl Pts',(31.1804379609257,0.111178530247992,18.6328833887437));
#48864=CARTESIAN_POINT('Ctrl Pts',(31.1550790566304,0.267584160665563,18.6439737169172));
#48865=CARTESIAN_POINT('Ctrl Pts',(31.0469271232095,0.554595748580105,18.6643249836272));
#48866=CARTESIAN_POINT('Ctrl Pts',(30.9678100781097,0.68335841703765,18.6731299773448));
#48867=CARTESIAN_POINT('Ctrl Pts',(30.763452167876,0.90645295543942,18.6935886563282));
#48868=CARTESIAN_POINT('Ctrl Pts',(30.6393299618342,0.997879761179756,18.7044521341951));
#48869=CARTESIAN_POINT('Ctrl Pts',(30.3602369836734,1.12947461105548,18.7262561139589));
#48870=CARTESIAN_POINT('Ctrl Pts',(30.207398548302,1.16725893034935,18.7369811620628));
#48871=CARTESIAN_POINT('Ctrl Pts',(29.9028111520737,1.18064726329168,18.7561598319717));
#48872=CARTESIAN_POINT('Ctrl Pts',(29.7540809815473,1.15884794274813,18.7656824913455));
#48873=CARTESIAN_POINT('Ctrl Pts',(29.4674235177593,1.05897426017317,18.7868263546523));
#48874=CARTESIAN_POINT('Ctrl Pts',(29.332959967187,0.979858413005439,18.7978884009434));
#48875=CARTESIAN_POINT('Ctrl Pts',(29.1020498086111,0.773870883761844,18.8193710843283));
#48876=CARTESIAN_POINT('Ctrl Pts',(29.0080096312967,0.648942084974305,18.8289851559772));
#48877=CARTESIAN_POINT('Ctrl Pts',(28.8756172989166,0.373674108747255,18.8485037128466));
#48878=CARTESIAN_POINT('Ctrl Pts',(28.8370493704244,0.226703861544607,18.85892500183));
#48879=CARTESIAN_POINT('Ctrl Pts',(28.8170693542027,-0.0796098764074361,
18.8806449352421));
#48880=CARTESIAN_POINT('Ctrl Pts',(28.838156352639,-0.236207536581086,18.8917488797605));
#48881=CARTESIAN_POINT('Ctrl Pts',(28.9384458248014,-0.526222673597261,
18.9123131205504));
#48882=CARTESIAN_POINT('Ctrl Pts',(29.0143989785152,-0.657569956199922,
18.921123179589));
#48883=CARTESIAN_POINT('Ctrl Pts',(29.2130173163762,-0.886033452067211,
18.9414197543903));
#48884=CARTESIAN_POINT('Ctrl Pts',(29.3343580168877,-0.980462303689547,
18.9522188602181));
#48885=CARTESIAN_POINT('Ctrl Pts',(29.609473809437,-1.11936682716347,18.9740377655105));
#48886=CARTESIAN_POINT('Ctrl Pts',(29.7612660994758,-1.16125829944545,18.9848441861849));
#48887=CARTESIAN_POINT('Ctrl Pts',(29.9445511530895,-1.1742603871282,18.9965602675684));
#48888=CARTESIAN_POINT('Ctrl Pts',(29.9722886221142,-1.17524047358085,18.998298308746));
#48889=CARTESIAN_POINT('Ctrl Pts',(29.9999999999996,-1.17524047358085,18.9999999999999));
#48890=CARTESIAN_POINT('Origin',(30.,-1.21864324187371E-14,15.78125));
#48891=CARTESIAN_POINT('',(30.0000000000001,-1.17524047358085,19.5625));
#48892=CARTESIAN_POINT('',(29.9999999999998,-1.17524047358085,19.4999999999999));
#48893=CARTESIAN_POINT('',(30.,-1.17524047358085,15.78125));
#48894=CARTESIAN_POINT('Ctrl Pts',(30.0000000000003,-1.17524047358085,19.5625));
#48895=CARTESIAN_POINT('Ctrl Pts',(29.9013941092948,-1.17524047358088,19.5564448416279));
#48896=CARTESIAN_POINT('Ctrl Pts',(29.8029987638489,-1.16283641906691,19.549962842264));
#48897=CARTESIAN_POINT('Ctrl Pts',(29.5564668004839,-1.09938994466242,19.5325744732568));
#48898=CARTESIAN_POINT('Ctrl Pts',(29.415037771559,-1.03111229808663,19.5214689478566));
#48899=CARTESIAN_POINT('Ctrl Pts',(29.1716434679328,-0.847005065425004,
19.4999953804452));
#48900=CARTESIAN_POINT('Ctrl Pts',(29.0705827398005,-0.734710314058229,
19.4898082076353));
#48901=CARTESIAN_POINT('Ctrl Pts',(28.9129094963582,-0.472970867922037,
19.4708462190468));
#48902=CARTESIAN_POINT('Ctrl Pts',(28.8598073237114,-0.32477237703938,19.4605287888834));
#48903=CARTESIAN_POINT('Ctrl Pts',(28.8149047814539,-0.0184511328725056,
19.4388083232246));
#48904=CARTESIAN_POINT('Ctrl Pts',(28.8226412643137,0.136461808695805,19.4278238378469));
#48905=CARTESIAN_POINT('Ctrl Pts',(28.8961732267534,0.430084241574931,19.4070038128194));
#48906=CARTESIAN_POINT('Ctrl Pts',(28.9595331463533,0.5664127336681,19.3979778677293));
#48907=CARTESIAN_POINT('Ctrl Pts',(29.137896746023,0.813817787616469,19.3782535402653));
#48908=CARTESIAN_POINT('Ctrl Pts',(29.2533816215898,0.92090330809607,19.3673653008166));
#48909=CARTESIAN_POINT('Ctrl Pts',(29.5158730245192,1.08160589182486,19.3455488072285));
#48910=CARTESIAN_POINT('Ctrl Pts',(29.6595524720356,1.13505921849913,19.3348306663965));
#48911=CARTESIAN_POINT('Ctrl Pts',(29.9586626554596,1.18420822106571,19.3147204900089));
#48912=CARTESIAN_POINT('Ctrl Pts',(30.1111738123977,1.17970362181747,19.305831310076));
#48913=CARTESIAN_POINT('Ctrl Pts',(30.4108580361143,1.11207867833533,19.2850308420592));
#48914=CARTESIAN_POINT('Ctrl Pts',(30.5546592354692,1.0477915906526,19.2739211274165));
#48915=CARTESIAN_POINT('Ctrl Pts',(30.8039627363725,0.870265103601911,19.2523180019705));
#48916=CARTESIAN_POINT('Ctrl Pts',(30.9084512058835,0.760562755820576,19.242012249931));
#48917=CARTESIAN_POINT('Ctrl Pts',(31.0738897348627,0.502419631313023,19.2227009162624));
#48918=CARTESIAN_POINT('Ctrl Pts',(31.1311837638208,0.355135076925594,19.2126817312365));
#48919=CARTESIAN_POINT('Ctrl Pts',(31.1842706831827,0.04913932312708,19.1909843452775));
#48920=CARTESIAN_POINT('Ctrl Pts',(31.1805124566442,-0.106321035688241,
19.1799610439256));
#48921=CARTESIAN_POINT('Ctrl Pts',(31.1143513914742,-0.401996025434437,
19.1589954772754));
#48922=CARTESIAN_POINT('Ctrl Pts',(31.0545027280943,-0.539801328735837,
19.1497832518808));
#48923=CARTESIAN_POINT('Ctrl Pts',(30.8825757787308,-0.791565442014421,
19.1302996391962));
#48924=CARTESIAN_POINT('Ctrl Pts',(30.7698754890686,-0.90154647307845,19.1194797380197));
#48925=CARTESIAN_POINT('Ctrl Pts',(30.5112798180774,-1.06909180183037,19.0976598713853));
#48926=CARTESIAN_POINT('Ctrl Pts',(30.3686300461772,-1.12627173763864,19.0868728383175));
#48927=CARTESIAN_POINT('Ctrl Pts',(30.146651557919,-1.16837939048486,19.071748782068));
#48928=CARTESIAN_POINT('Ctrl Pts',(30.0733297917687,-1.17524047358085,19.0670030119334));
#48929=CARTESIAN_POINT('Ctrl Pts',(30.,-1.17524047358085,19.0625));
#48930=CARTESIAN_POINT('Ctrl Pts',(29.9999999999996,-1.17524047358085,18.9999999999999));
#48931=CARTESIAN_POINT('Ctrl Pts',(30.1208018343283,-1.17524047358085,19.0074181596379));
#48932=CARTESIAN_POINT('Ctrl Pts',(30.2410273417982,-1.15662316578329,19.0154609815185));
#48933=CARTESIAN_POINT('Ctrl Pts',(30.5033214237856,-1.07312795539109,19.0345280681775));
#48934=CARTESIAN_POINT('Ctrl Pts',(30.6395388198866,-0.997960158889978,
19.0455578408927));
#48935=CARTESIAN_POINT('Ctrl Pts',(30.876878941369,-0.797935916319293,19.067223952545));
#48936=CARTESIAN_POINT('Ctrl Pts',(30.9750570407496,-0.674426741281125,
19.0771781033725));
#48937=CARTESIAN_POINT('Ctrl Pts',(31.1146479426385,-0.401644540658674,
19.0965204001729));
#48938=CARTESIAN_POINT('Ctrl Pts',(31.1567939343853,-0.256055794064216,
19.1068437304378));
#48939=CARTESIAN_POINT('Ctrl Pts',(31.1845453028865,0.0488704061743495,
19.1284652770555));
#48940=CARTESIAN_POINT('Ctrl Pts',(31.1676027188842,0.205546638234067,19.1395747929079));
#48941=CARTESIAN_POINT('Ctrl Pts',(31.0749923240704,0.498408501569657,19.1603408878703));
#48942=CARTESIAN_POINT('Ctrl Pts',(31.0021074917097,0.632295920687204,19.1692134966416));
#48943=CARTESIAN_POINT('Ctrl Pts',(30.8090318381138,0.865881565613648,19.1893513074212));
#48944=CARTESIAN_POINT('Ctrl Pts',(30.6904244547157,0.963111668252584,19.2000818814201));
#48945=CARTESIAN_POINT('Ctrl Pts',(30.419302827982,1.10891198567697,19.2218999959461));
#48946=CARTESIAN_POINT('Ctrl Pts',(30.2686205389783,1.15471361101177,19.232776883577));
#48947=CARTESIAN_POINT('Ctrl Pts',(29.9650775926592,1.18413115670169,19.2524597117397));
#48948=CARTESIAN_POINT('Ctrl Pts',(29.8154193388389,1.17018311968912,19.2615139711268));
#48949=CARTESIAN_POINT('Ctrl Pts',(29.5246945745281,1.08577187830739,19.2823593965739));
#48950=CARTESIAN_POINT('Ctrl Pts',(29.3869225275025,1.01437069769904,19.2933510961767));
#48951=CARTESIAN_POINT('Ctrl Pts',(29.1449076103833,0.821179121928182,19.3150620325829));
#48952=CARTESIAN_POINT('Ctrl Pts',(29.0436548787038,0.700625409307818,19.3253204220004));
#48953=CARTESIAN_POINT('Ctrl Pts',(28.8969987915807,0.43246305184088,19.3443351373923));
#48954=CARTESIAN_POINT('Ctrl Pts',(28.8509250755758,0.288512534702925,19.3545423049446));
#48955=CARTESIAN_POINT('Ctrl Pts',(28.8145962917767,-0.0146433580687103,
19.3760383235316));
#48956=CARTESIAN_POINT('Ctrl Pts',(28.8269416915671,-0.171282191603316,
19.3871451875491));
#48957=CARTESIAN_POINT('Ctrl Pts',(28.9109596159865,-0.467218400914038,
19.4081292766188));
#48958=CARTESIAN_POINT('Ctrl Pts',(28.9804361831083,-0.603975745967944,
19.4171374882925));
#48959=CARTESIAN_POINT('Ctrl Pts',(29.167379298401,-0.843150163563664,19.4370968570367));
#48960=CARTESIAN_POINT('Ctrl Pts',(29.2829166096857,-0.943363871775425,
19.447744685016));
#48961=CARTESIAN_POINT('Ctrl Pts',(29.5508199561077,-1.09737775425148,19.4696563740096));
#48962=CARTESIAN_POINT('Ctrl Pts',(29.7018004358378,-1.14764798506443,19.4807100016028));
#48963=CARTESIAN_POINT('Ctrl Pts',(29.9053565213586,-1.17238533019257,19.4940869386326));
#48964=CARTESIAN_POINT('Ctrl Pts',(29.9526999581129,-1.17524047358085,19.4970954144566));
#48965=CARTESIAN_POINT('Ctrl Pts',(29.9999999999997,-1.17524047358085,19.4999999999999));
#48966=CARTESIAN_POINT('Origin',(30.,-1.21864324187371E-14,15.78125));
#48967=CARTESIAN_POINT('',(30.0000000000003,-1.17524047358085,20.0625));
#48968=CARTESIAN_POINT('',(30.,-1.17524047358085,20.));
#48969=CARTESIAN_POINT('',(30.,-1.17524047358085,15.78125));
#48970=CARTESIAN_POINT('Ctrl Pts',(30.0000000000005,-1.17524047358085,20.0625));
#48971=CARTESIAN_POINT('Ctrl Pts',(29.8795085612599,-1.17524047358091,20.0551009010331));
#48972=CARTESIAN_POINT('Ctrl Pts',(29.7595622632698,-1.15671912815303,20.0470786269818));
#48973=CARTESIAN_POINT('Ctrl Pts',(29.4968909328774,-1.07331217196907,20.0279915033172));
#48974=CARTESIAN_POINT('Ctrl Pts',(29.3601452160293,-0.997848639613717,
20.0169188027128));
#48975=CARTESIAN_POINT('Ctrl Pts',(29.1279895360134,-0.801888849412877,
19.9957151555763));
#48976=CARTESIAN_POINT('Ctrl Pts',(29.0334325756294,-0.684937055319331,
19.9860671564471));
#48977=CARTESIAN_POINT('Ctrl Pts',(28.8898211655935,-0.415941538872162,
19.9669933638564));
#48978=CARTESIAN_POINT('Ctrl Pts',(28.8445081931777,-0.265175978908636,
19.956302958832));
#48979=CARTESIAN_POINT('Ctrl Pts',(28.8156113317766,0.0421759568632406,
19.934509409435));
#48980=CARTESIAN_POINT('Ctrl Pts',(28.8311290214712,0.195715280521655,19.9236223238335));
#48981=CARTESIAN_POINT('Ctrl Pts',(28.9191574051752,0.485137216573778,19.9031001454256));
#48982=CARTESIAN_POINT('Ctrl Pts',(28.9896097101006,0.618617028321211,19.8942800985803));
#48983=CARTESIAN_POINT('Ctrl Pts',(29.1815016413357,0.8578593810217,19.8740144260076));
#48984=CARTESIAN_POINT('Ctrl Pts',(29.3033374545183,0.95943115864218,19.8629316730427));
#48985=CARTESIAN_POINT('Ctrl Pts',(29.5744131919249,1.10584185120943,19.8410947363937));
#48986=CARTESIAN_POINT('Ctrl Pts',(29.7199575824398,1.1513488317962,19.8305438014147));
#48987=CARTESIAN_POINT('Ctrl Pts',(30.0223936436952,1.18496921575338,19.8107799381662));
#48988=CARTESIAN_POINT('Ctrl Pts',(30.17645595477,1.17197553997772,19.8015484961906));
#48989=CARTESIAN_POINT('Ctrl Pts',(30.4728526803367,1.08704252391974,19.7803362699347));
#48990=CARTESIAN_POINT('Ctrl Pts',(30.6120360120599,1.01521369720442,19.7692427449689));
#48991=CARTESIAN_POINT('Ctrl Pts',(30.8500255075595,0.825212607475584,19.7478921149936));
#48992=CARTESIAN_POINT('Ctrl Pts',(30.9478859340228,0.710618012755788,19.7378881282691));
#48993=CARTESIAN_POINT('Ctrl Pts',(31.0987101974267,0.445344450081356,19.7190782500187));
#48994=CARTESIAN_POINT('Ctrl Pts',(31.148011535677,0.295869142851177,19.7084793335565));
#48995=CARTESIAN_POINT('Ctrl Pts',(31.1851397417262,-0.0109614779842622,
19.6867227492848));
#48996=CARTESIAN_POINT('Ctrl Pts',(31.1736153786499,-0.165256365490512,
19.6757820885594));
#48997=CARTESIAN_POINT('Ctrl Pts',(31.093043155488,-0.456865689692268,19.6551048079831));
#48998=CARTESIAN_POINT('Ctrl Pts',(31.0262715370984,-0.591802059151614,
19.6462060198927));
#48999=CARTESIAN_POINT('Ctrl Pts',(30.8407896047275,-0.836102523209368,
19.6261546414896));
#49000=CARTESIAN_POINT('Ctrl Pts',(30.7213221432726,-0.941101033293042,
19.6150958330235));
#49001=CARTESIAN_POINT('Ctrl Pts',(30.4533957183897,-1.09478566221008,19.5931944001043));
#49002=CARTESIAN_POINT('Ctrl Pts',(30.3086782810935,-1.14405280540599,19.5825609345826));
#49003=CARTESIAN_POINT('Ctrl Pts',(30.1059062370161,-1.17166523878134,19.5691302110914));
#49004=CARTESIAN_POINT('Ctrl Pts',(30.0529306288365,-1.17524047358084,19.5657503467901));
#49005=CARTESIAN_POINT('Ctrl Pts',(30.0000000000003,-1.17524047358085,19.5625));
#49006=CARTESIAN_POINT('Ctrl Pts',(29.9999999999997,-1.17524047358085,19.4999999999999));
#49007=CARTESIAN_POINT('Ctrl Pts',(30.1013134091967,-1.17524047358085,19.5062214207844));
#49008=CARTESIAN_POINT('Ctrl Pts',(30.2023703512557,-1.16214610944681,19.5128913366607));
#49009=CARTESIAN_POINT('Ctrl Pts',(30.4489451189351,-1.0968832859302,19.530346730545));
#49010=CARTESIAN_POINT('Ctrl Pts',(30.5880725807912,-1.02901377075515,19.5412964522821));
#49011=CARTESIAN_POINT('Ctrl Pts',(30.8343712795547,-0.842194481571482,
19.5630445243813));
#49012=CARTESIAN_POINT('Ctrl Pts',(30.9385897374703,-0.724253666071193,
19.5736257801046));
#49013=CARTESIAN_POINT('Ctrl Pts',(31.0916505061583,-0.460199205120922,
19.5923866032744));
#49014=CARTESIAN_POINT('Ctrl Pts',(31.1412805360793,-0.317836464065441,
19.6024630191855));
#49015=CARTESIAN_POINT('Ctrl Pts',(31.1853286010408,-0.0163533735884271,
19.6238404235873));
#49016=CARTESIAN_POINT('Ctrl Pts',(31.1771308821554,0.140138676220234,19.6349368795415));
#49017=CARTESIAN_POINT('Ctrl Pts',(31.1009443941398,0.438772825443172,19.6561122727154));
#49018=CARTESIAN_POINT('Ctrl Pts',(31.0345585763112,0.578169376036336,19.6653017627446));
#49019=CARTESIAN_POINT('Ctrl Pts',(30.8531427469532,0.82231181712456,19.6850978487155));
#49020=CARTESIAN_POINT('Ctrl Pts',(30.7404083067898,0.925109501957493,19.6956651705268));
#49021=CARTESIAN_POINT('Ctrl Pts',(30.4771535858122,1.08544747135218,19.7175156107599));
#49022=CARTESIAN_POINT('Ctrl Pts',(30.3279214291812,1.13945389596675,19.7285943399309));
#49023=CARTESIAN_POINT('Ctrl Pts',(30.0245530133835,1.1844610145353,19.7488191591971));
#49024=CARTESIAN_POINT('Ctrl Pts',(29.8738446796079,1.17798106878653,19.7576497404222));
#49025=CARTESIAN_POINT('Ctrl Pts',(29.5795308296296,1.10805786067705,19.7782019083499));
#49026=CARTESIAN_POINT('Ctrl Pts',(29.4390520876789,1.04399036655414,19.7890998131999));
#49027=CARTESIAN_POINT('Ctrl Pts',(29.1881857877585,0.86396490371117,19.8108875045287));
#49028=CARTESIAN_POINT('Ctrl Pts',(29.0808654270878,0.748795351686304,19.8215609892382));
#49029=CARTESIAN_POINT('Ctrl Pts',(28.9210185508111,0.489082061917269,19.8405846207479));
#49030=CARTESIAN_POINT('Ctrl Pts',(28.8677194354805,0.348399842158546,19.8502958472478));
#49031=CARTESIAN_POINT('Ctrl Pts',(28.8156254684423,0.0489678765559477,
19.8715278115659));
#49032=CARTESIAN_POINT('Ctrl Pts',(28.8194748723048,-0.107254256712007,
19.88260512842));
#49033=CARTESIAN_POINT('Ctrl Pts',(28.8873579337553,-0.408638429267571,
19.9039755188019));
#49034=CARTESIAN_POINT('Ctrl Pts',(28.9504754704978,-0.550854728104584,
19.9134143320288));
#49035=CARTESIAN_POINT('Ctrl Pts',(29.1260934520651,-0.800139160205639,
19.9330366884507));
#49036=CARTESIAN_POINT('Ctrl Pts',(29.2358570179041,-0.905539531949709,
19.9435138507578));
#49037=CARTESIAN_POINT('Ctrl Pts',(29.4941308064619,-1.07230397107708,19.9652862658853));
#49038=CARTESIAN_POINT('Ctrl Pts',(29.6414537313008,-1.13013161490591,19.9763832300743));
#49039=CARTESIAN_POINT('Ctrl Pts',(29.8633704190017,-1.16928660340085,19.9913988083098));
#49040=CARTESIAN_POINT('Ctrl Pts',(29.9316910379181,-1.17524047358085,19.9958053055382));
#49041=CARTESIAN_POINT('Ctrl Pts',(30.,-1.17524047358085,20.));
#49042=CARTESIAN_POINT('Origin',(30.,-1.21864324187371E-14,15.78125));
#49043=CARTESIAN_POINT('',(30.,-1.17524047358085,20.5625));
#49044=CARTESIAN_POINT('',(30.,-1.17524047358085,20.5));
#49045=CARTESIAN_POINT('',(30.,-1.17524047358085,15.78125));
#49046=CARTESIAN_POINT('Ctrl Pts',(30.0000000000001,-1.17524047358085,20.5625));
#49047=CARTESIAN_POINT('Ctrl Pts',(29.857466677664,-1.17524047358086,20.5537473602351));
#49048=CARTESIAN_POINT('Ctrl Pts',(29.7159780885029,-1.14931710991913,20.5441397949867));
#49049=CARTESIAN_POINT('Ctrl Pts',(29.4386327044728,-1.04389937724848,20.5233712075421));
#49050=CARTESIAN_POINT('Ctrl Pts',(29.3069416102485,-0.961526015490682,
20.5123639202805));
#49051=CARTESIAN_POINT('Ctrl Pts',(29.086333053172,-0.75405497378,20.4914612382194));
#49052=CARTESIAN_POINT('Ctrl Pts',(28.998234525789,-0.632326756560098,20.4823366930552));
#49053=CARTESIAN_POINT('Ctrl Pts',(28.8691902031313,-0.356072447869899,
20.4627481978422));
#49054=CARTESIAN_POINT('Ctrl Pts',(28.8319810448841,-0.203050335093991,
20.4518977863579));
#49055=CARTESIAN_POINT('Ctrl Pts',(28.8195943462911,0.104677105391675,20.4300776108702));
#49056=CARTESIAN_POINT('Ctrl Pts',(28.8430260194231,0.256395499280261,20.419319642799));
#49057=CARTESIAN_POINT('Ctrl Pts',(28.9459812899286,0.541272174450661,20.399119757359));
#49058=CARTESIAN_POINT('Ctrl Pts',(29.0240298052411,0.671873753047622,20.3902782906932));
#49059=CARTESIAN_POINT('Ctrl Pts',(29.2288981247322,0.900554058537053,20.3695902323474));
#49060=CARTESIAN_POINT('Ctrl Pts',(29.3552896087803,0.99495410007641,20.3584819910769));
#49061=CARTESIAN_POINT('Ctrl Pts',(29.6322160097862,1.12628386030684,20.3368204541948));
#49062=CARTESIAN_POINT('Ctrl Pts',(29.7791530812878,1.16405670631925,20.3264582018892));
#49063=CARTESIAN_POINT('Ctrl Pts',(30.0846260087116,1.18247957174534,20.3070466605788));
#49064=CARTESIAN_POINT('Ctrl Pts',(30.2403465146444,1.16089584876694,20.297232309072));
#49065=CARTESIAN_POINT('Ctrl Pts',(30.5330201521523,1.05871377596515,20.2756371654718));
#49066=CARTESIAN_POINT('Ctrl Pts',(30.6672316693715,0.979687699230499,20.2645937786601));
#49067=CARTESIAN_POINT('Ctrl Pts',(30.8935142020877,0.777827856358351,20.2435416089216));
#49068=CARTESIAN_POINT('Ctrl Pts',(30.9847747247484,0.658466900361099,20.2341902246224));
#49069=CARTESIAN_POINT('Ctrl Pts',(31.1210267097183,0.385760488516485,20.2148533018128));
#49070=CARTESIAN_POINT('Ctrl Pts',(31.1622514979646,0.233796400148884,20.2040779121667));
#49071=CARTESIAN_POINT('Ctrl Pts',(31.1827840987885,-0.0738574566284658,
20.1822629543138));
#49072=CARTESIAN_POINT('Ctrl Pts',(31.1632412224874,-0.226525134572718,
20.1714376749082));
#49073=CARTESIAN_POINT('Ctrl Pts',(31.0676501608268,-0.513670659031922,
20.1510769110961));
#49074=CARTESIAN_POINT('Ctrl Pts',(30.9933877261944,-0.645689071009633,
20.1422762056128));
#49075=CARTESIAN_POINT('Ctrl Pts',(30.7949445520148,-0.879653706050947,
20.1217953512642));
#49076=CARTESIAN_POINT('Ctrl Pts',(30.670767244765,-0.977642983856647,20.1106958256016));
#49077=CARTESIAN_POINT('Ctrl Pts',(30.3966473841018,-1.11649688166864,20.0889398730384));
#49078=CARTESIAN_POINT('Ctrl Pts',(30.2503518300705,-1.15811817698529,20.0784805729189));
#49079=CARTESIAN_POINT('Ctrl Pts',(30.0667947188483,-1.17381847353791,20.0666521235228));
#49080=CARTESIAN_POINT('Ctrl Pts',(30.0333795266192,-1.17524047358084,20.0645497590825));
#49081=CARTESIAN_POINT('Ctrl Pts',(30.0000000000005,-1.17524047358085,20.0625));
#49082=CARTESIAN_POINT('Ctrl Pts',(30.,-1.17524047358085,20.));
#49083=CARTESIAN_POINT('Ctrl Pts',(30.0810461612404,-1.17524047358085,20.0049768562329));
#49084=CARTESIAN_POINT('Ctrl Pts',(30.1620390634994,-1.16685998246121,20.0102475616837));
#49085=CARTESIAN_POINT('Ctrl Pts',(30.3910188268312,-1.11873616439623,20.0260148454886));
#49086=CARTESIAN_POINT('Ctrl Pts',(30.5327757448135,-1.05858684074315,20.0368523263699));
#49087=CARTESIAN_POINT('Ctrl Pts',(30.7881241531233,-0.885634167315425,
20.0586644967329));
#49088=CARTESIAN_POINT('Ctrl Pts',(30.8985424642913,-0.773390023616368,
20.0694245027186));
#49089=CARTESIAN_POINT('Ctrl Pts',(31.0652926267422,-0.518183463935382,
20.0887122685505));
#49090=CARTESIAN_POINT('Ctrl Pts',(31.1223297618129,-0.379162720763723,
20.0981145292327));
#49091=CARTESIAN_POINT('Ctrl Pts',(31.182501138976,-0.0818619977066759,
20.1191953725253));
#49092=CARTESIAN_POINT('Ctrl Pts',(31.1830210318339,0.0739680814447177,
20.1302448898124));
#49093=CARTESIAN_POINT('Ctrl Pts',(31.1235906320717,0.378032609170699,20.1518053374088));
#49094=CARTESIAN_POINT('Ctrl Pts',(31.0637982215859,0.523138441463073,20.1615551718639));
#49095=CARTESIAN_POINT('Ctrl Pts',(30.8940186419568,0.777530022608243,20.1810000731231));
#49096=CARTESIAN_POINT('Ctrl Pts',(30.7872728375238,0.885439479392022,20.1913808781633));
#49097=CARTESIAN_POINT('Ctrl Pts',(30.5341117586616,1.05845819784869,20.2130610712561));
#49098=CARTESIAN_POINT('Ctrl Pts',(30.3887837233288,1.12003007025227,20.2241682808161));
#49099=CARTESIAN_POINT('Ctrl Pts',(30.0880464072922,1.18158358213937,20.2448181618436));
#49100=CARTESIAN_POINT('Ctrl Pts',(29.9360438868879,1.18313176496437,20.2536476203627));
#49101=CARTESIAN_POINT('Ctrl Pts',(29.6381705506099,1.1284628410545,20.2738775466838));
#49102=CARTESIAN_POINT('Ctrl Pts',(29.4952627894061,1.07218329111658,20.2846485002308));
#49103=CARTESIAN_POINT('Ctrl Pts',(29.2357076507194,0.906285518142771,20.3064688735353));
#49104=CARTESIAN_POINT('Ctrl Pts',(29.1223265216238,0.796998466553187,20.3173059793119));
#49105=CARTESIAN_POINT('Ctrl Pts',(28.94883850375,0.546283376626024,20.3368482617845));
#49106=CARTESIAN_POINT('Ctrl Pts',(28.8881400415123,0.408839661433748,20.3460102123335));
#49107=CARTESIAN_POINT('Ctrl Pts',(28.8201837019616,0.113659356458156,20.3669407021362));
#49108=CARTESIAN_POINT('Ctrl Pts',(28.8154556440784,-0.0416770716817043,
20.377955215877));
#49109=CARTESIAN_POINT('Ctrl Pts',(28.8666287496698,-0.348241759389233,
20.3996929435023));
#49110=CARTESIAN_POINT('Ctrl Pts',(28.923168044506,-0.496185032937023,20.4097992015263));
#49111=CARTESIAN_POINT('Ctrl Pts',(29.0873034963183,-0.755446668555585,
20.4290701716561));
#49112=CARTESIAN_POINT('Ctrl Pts',(29.1911125253156,-0.865675121623956,
20.4393528532326));
#49113=CARTESIAN_POINT('Ctrl Pts',(29.4392495659902,-1.04453090441881,20.4609314775711));
#49114=CARTESIAN_POINT('Ctrl Pts',(29.5825856119781,-1.10962145963742,20.4720411141544));
#49115=CARTESIAN_POINT('Ctrl Pts',(29.8217321396476,-1.16509155071327,20.4886931681386));
#49116=CARTESIAN_POINT('Ctrl Pts',(29.9108091908387,-1.17524047358086,20.4945229998842));
#49117=CARTESIAN_POINT('Ctrl Pts',(30.0000000000001,-1.17524047358085,20.5));
#49118=CARTESIAN_POINT('Origin',(30.,-1.21864324187371E-14,15.78125));
#49119=CARTESIAN_POINT('',(30.,-1.17524047358085,21.0625));
#49120=CARTESIAN_POINT('',(30.0000000000003,-1.17524047358085,21.));
#49121=CARTESIAN_POINT('',(30.,-1.17524047358085,15.78125));
#49122=CARTESIAN_POINT('Ctrl Pts',(30.,-1.17524047358085,21.0625));
#49123=CARTESIAN_POINT('Ctrl Pts',(29.9930425354756,-1.17524047358085,21.062072758288));
#49124=CARTESIAN_POINT('Ctrl Pts',(29.9860827950433,-1.17517869098314,21.0616431863938));
#49125=CARTESIAN_POINT('Ctrl Pts',(29.8232316065342,-1.17228514735699,21.0515402867957));
#49126=CARTESIAN_POINT('Ctrl Pts',(29.6694853244495,-1.13852257202281,21.0409020757897));
#49127=CARTESIAN_POINT('Ctrl Pts',(29.3867104280309,-1.01415059452875,21.0191280758083));
#49128=CARTESIAN_POINT('Ctrl Pts',(29.2599516823908,-0.925722033008617,
21.0082089931399));
#49129=CARTESIAN_POINT('Ctrl Pts',(29.0500490851207,-0.707886564567504,
20.9875962815068));
#49130=CARTESIAN_POINT('Ctrl Pts',(28.9678750474644,-0.58156955059427,20.9787376277926));
#49131=CARTESIAN_POINT('Ctrl Pts',(28.852209421352,-0.297516308143681,20.9585961298867));
#49132=CARTESIAN_POINT('Ctrl Pts',(28.8227455494544,-0.141401249035421,
20.9475264053908));
#49133=CARTESIAN_POINT('Ctrl Pts',(28.8269065561122,0.16711629798966,20.9256502054441));
#49134=CARTESIAN_POINT('Ctrl Pts',(28.8581354481118,0.316603790040456,20.915050424987));
#49135=CARTESIAN_POINT('Ctrl Pts',(28.9760761175465,0.596699382404322,20.8951895540518));
#49136=CARTESIAN_POINT('Ctrl Pts',(29.0620842641545,0.724424918144287,20.8860783197069));
#49137=CARTESIAN_POINT('Ctrl Pts',(29.2801481558297,0.941880855388224,20.8649778977684));
#49138=CARTESIAN_POINT('Ctrl Pts',(29.4108173740059,1.02868094436595,20.8538764175153));
#49139=CARTESIAN_POINT('Ctrl Pts',(29.6929274853784,1.14422525088517,20.8324562143623));
#49140=CARTESIAN_POINT('Ctrl Pts',(29.8408766090356,1.17398844910975,20.8223157862342));
#49141=CARTESIAN_POINT('Ctrl Pts',(30.146238089068,1.17646530253954,20.8034764343644));
#49142=CARTESIAN_POINT('Ctrl Pts',(30.3008127704194,1.14674523024735,20.7930175246536));
#49143=CARTESIAN_POINT('Ctrl Pts',(30.5871854304481,1.02954198948055,20.7712767528846));
#49144=CARTESIAN_POINT('Ctrl Pts',(30.7164764357369,0.944145175747713,20.7603096568304));
#49145=CARTESIAN_POINT('Ctrl Pts',(30.9318157386174,0.731537563311469,20.7395484367846));
#49146=CARTESIAN_POINT('Ctrl Pts',(31.0169931096024,0.607571893797524,20.7305813882675));
#49147=CARTESIAN_POINT('Ctrl Pts',(31.1392545858023,0.328058458126713,20.7107617965928));
#49148=CARTESIAN_POINT('Ctrl Pts',(31.1726798971535,0.174145191638854,20.6998481956499));
#49149=CARTESIAN_POINT('Ctrl Pts',(31.177452605602,-0.133454152417299,20.6780371031564));
#49150=CARTESIAN_POINT('Ctrl Pts',(31.1504138008343,-0.284195707834949,
20.6673484002337));
#49151=CARTESIAN_POINT('Ctrl Pts',(31.0405663350578,-0.566901684154618,
20.647302433566));
#49152=CARTESIAN_POINT('Ctrl Pts',(30.9589018497076,-0.696179869646961,
20.6383684206626));
#49153=CARTESIAN_POINT('Ctrl Pts',(30.7479829469593,-0.919779045347213,
20.6174889551129));
#49154=CARTESIAN_POINT('Ctrl Pts',(30.6195839675717,-1.0107321163549,20.6063796462101));
#49155=CARTESIAN_POINT('Ctrl Pts',(30.3401820261614,-1.13487834149049,20.5848207753144));
#49156=CARTESIAN_POINT('Ctrl Pts',(30.1927291526794,-1.16899555973842,20.5745564544744));
#49157=CARTESIAN_POINT('Ctrl Pts',(30.02853673898,-1.17498080122699,20.5642615811144));
#49158=CARTESIAN_POINT('Ctrl Pts',(30.0142636931895,-1.17524047358085,20.5633759002187));
#49159=CARTESIAN_POINT('Ctrl Pts',(30.0000000000001,-1.17524047358085,20.5625));
#49160=CARTESIAN_POINT('Ctrl Pts',(30.0000000000001,-1.17524047358085,20.5));
#49161=CARTESIAN_POINT('Ctrl Pts',(30.0615320920417,-1.17524047358085,20.5037785426368));
#49162=CARTESIAN_POINT('Ctrl Pts',(30.1230970944725,-1.17040913175211,20.5077303953467));
#49163=CARTESIAN_POINT('Ctrl Pts',(30.3340845761439,-1.13693724894346,20.5218733491291));
#49164=CARTESIAN_POINT('Ctrl Pts',(30.4779822284686,-1.08432359797014,20.5325751197693));
#49165=CARTESIAN_POINT('Ctrl Pts',(30.7413240882277,-0.925171378815601,
20.5543888717152));
#49166=CARTESIAN_POINT('Ctrl Pts',(30.8574242886598,-0.818746672756081,
20.5652914684918));
#49167=CARTESIAN_POINT('Ctrl Pts',(31.0372296037246,-0.572330389441825,
20.5850692727305));
#49168=CARTESIAN_POINT('Ctrl Pts',(31.1013789298939,-0.436327710632643,
20.5940611041994));
#49169=CARTESIAN_POINT('Ctrl Pts',(31.1765507195451,-0.143169609179877,
20.6148482046583));
#49170=CARTESIAN_POINT('Ctrl Pts',(31.1851707108535,0.0116076749541518,
20.6258230709101));
#49171=CARTESIAN_POINT('Ctrl Pts',(31.1420730921553,0.318093458162843,20.6475552036167));
#49172=CARTESIAN_POINT('Ctrl Pts',(31.0898417933348,0.466589648702242,20.6579510306787));
#49173=CARTESIAN_POINT('Ctrl Pts',(30.9337645237733,0.729159361106415,20.6768444502657));
#49174=CARTESIAN_POINT('Ctrl Pts',(30.8334379992983,0.84198975683026,20.6870055279311));
#49175=CARTESIAN_POINT('Ctrl Pts',(30.591317195237,1.02746666327729,20.7084494527507));
#49176=CARTESIAN_POINT('Ctrl Pts',(30.4504043784541,1.09657907803444,20.7195528744157));
#49177=CARTESIAN_POINT('Ctrl Pts',(30.1527579068286,1.17519666342875,20.7406179390521));
#49178=CARTESIAN_POINT('Ctrl Pts',(29.9992772327099,1.18508027808452,20.7496955256169));
#49179=CARTESIAN_POINT('Ctrl Pts',(29.6980213394833,1.14582802600215,20.7695865882633));
#49180=CARTESIAN_POINT('Ctrl Pts',(29.5531012936116,1.09744171629364,20.7802012666676));
#49181=CARTESIAN_POINT('Ctrl Pts',(29.2844190436536,0.945457598499347,20.8020888235724));
#49182=CARTESIAN_POINT('Ctrl Pts',(29.1643876737344,0.84125826030012,20.8131539267157));
#49183=CARTESIAN_POINT('Ctrl Pts',(28.9773975743441,0.59813879267389,20.8332560474103));
#49184=CARTESIAN_POINT('Ctrl Pts',(28.9097638018428,0.463547729800393,20.8421310013978));
#49185=CARTESIAN_POINT('Ctrl Pts',(28.8274319674294,0.172449502758382,20.8627720413655));
#49186=CARTESIAN_POINT('Ctrl Pts',(28.8149632933605,0.0183235810432114,
20.8737007211534));
#49187=CARTESIAN_POINT('Ctrl Pts',(28.850150967155,-0.288650006351519,20.8954674428227));
#49188=CARTESIAN_POINT('Ctrl Pts',(28.898515176706,-0.438439388541448,20.906088629547));
#49189=CARTESIAN_POINT('Ctrl Pts',(29.047641063206,-0.704596833168998,20.9249611816339));
#49190=CARTESIAN_POINT('Ctrl Pts',(29.1447168471359,-0.819746341645053,
20.9348754556746));
#49191=CARTESIAN_POINT('Ctrl Pts',(29.381325819526,-1.01116668011756,20.9561916286088));
#49192=CARTESIAN_POINT('Ctrl Pts',(29.5199396968772,-1.08386414625954,20.96728098122));
#49193=CARTESIAN_POINT('Ctrl Pts',(29.7764916553148,-1.15925176815251,20.9857080131187));
#49194=CARTESIAN_POINT('Ctrl Pts',(29.8880479255875,-1.1752404735809,20.9931252835322));
#49195=CARTESIAN_POINT('Ctrl Pts',(30.0000000000005,-1.17524047358085,21.));
#49196=CARTESIAN_POINT('Origin',(30.,-1.21864324187371E-14,15.78125));
#49197=CARTESIAN_POINT('',(29.9999999999998,-1.17524047358085,21.5625));
#49198=CARTESIAN_POINT('',(30.0000000000001,-1.17524047358085,21.5));
#49199=CARTESIAN_POINT('',(30.,-1.17524047358085,15.78125));
#49200=CARTESIAN_POINT('Ctrl Pts',(29.9999999999996,-1.17524047358085,21.5625));
#49201=CARTESIAN_POINT('Ctrl Pts',(29.9719988088573,-1.17524047358085,21.5607805119881));
#49202=CARTESIAN_POINT('Ctrl Pts',(29.9439711363572,-1.17423978092491,21.5590239195234));
#49203=CARTESIAN_POINT('Ctrl Pts',(29.7604047377572,-1.16108096387714,21.547285004757));
#49204=CARTESIAN_POINT('Ctrl Pts',(29.6086428973266,-1.11907669828182,21.5364764549777));
#49205=CARTESIAN_POINT('Ctrl Pts',(29.3336394628651,-0.979972388454951,
21.5146573661612));
#49206=CARTESIAN_POINT('Ctrl Pts',(29.2123764352237,-0.885461951955829,
21.503860137555));
#49207=CARTESIAN_POINT('Ctrl Pts',(29.0139169118187,-0.656850944948416,
21.4835680853588));
#49208=CARTESIAN_POINT('Ctrl Pts',(28.9380513713638,-0.525431379870783,
21.4747570119112));
#49209=CARTESIAN_POINT('Ctrl Pts',(28.8379806985326,-0.235334014126339,
21.4541869404899));
#49210=CARTESIAN_POINT('Ctrl Pts',(28.81701218115,-0.0787326333033737,21.4430827321496));
#49211=CARTESIAN_POINT('Ctrl Pts',(28.8372148732154,0.227544173701852,21.4213654174177));
#49212=CARTESIAN_POINT('Ctrl Pts',(28.8758855793473,0.374476178993786,21.4109468400715));
#49213=CARTESIAN_POINT('Ctrl Pts',(29.008483168462,0.64967403277934,21.3914332554072));
#49214=CARTESIAN_POINT('Ctrl Pts',(29.1026400510551,0.774562668949264,21.3818103125428));
#49215=CARTESIAN_POINT('Ctrl Pts',(29.3337333173752,0.980382528955385,21.3603223294383));
#49216=CARTESIAN_POINT('Ctrl Pts',(29.4682481852686,1.05938687455618,21.3492610850172));
#49217=CARTESIAN_POINT('Ctrl Pts',(29.7549668128984,1.15903498567807,21.3281214631321));
#49218=CARTESIAN_POINT('Ctrl Pts',(29.9037091563498,1.1807204220266,21.3186072813687));
#49219=CARTESIAN_POINT('Ctrl Pts',(30.2082836909242,1.16710140483065,21.2994212226452));
#49220=CARTESIAN_POINT('Ctrl Pts',(30.3610942123922,1.12920096767185,21.2886937718569));
#49221=CARTESIAN_POINT('Ctrl Pts',(30.6400777787282,0.99739853025376,21.2668891510646));
#49222=CARTESIAN_POINT('Ctrl Pts',(30.7641225887122,0.905886016702667,21.2560273872475));
#49223=CARTESIAN_POINT('Ctrl Pts',(30.9683193471767,0.682639701404097,21.2355732231612));
#49224=CARTESIAN_POINT('Ctrl Pts',(31.0473475790777,0.553805208866279,21.2267689284532));
#49225=CARTESIAN_POINT('Ctrl Pts',(31.1552799375254,0.266708452111841,21.2064116226359));
#49226=CARTESIAN_POINT('Ctrl Pts',(31.1805191858716,0.110295910456217,21.195320804404));
#49227=CARTESIAN_POINT('Ctrl Pts',(31.1683617956532,-0.197210560675315,
21.173516297295));
#49228=CARTESIAN_POINT('Ctrl Pts',(31.1334138492448,-0.345474524238407,
21.1630032741523));
#49229=CARTESIAN_POINT('Ctrl Pts',(31.0081981695942,-0.623166742222595,
21.1433128204234));
#49230=CARTESIAN_POINT('Ctrl Pts',(30.9181918552343,-0.749490769431124,
21.1339784439808));
#49231=CARTESIAN_POINT('Ctrl Pts',(30.6936733778382,-0.961255467276285,
21.1126834366527));
#49232=CARTESIAN_POINT('Ctrl Pts',(30.5610503971428,-1.04422897430134,21.1015976470182));
#49233=CARTESIAN_POINT('Ctrl Pts',(30.283074075588,-1.14948332004627,21.080796107845));
#49234=CARTESIAN_POINT('Ctrl Pts',(30.1420666819575,-1.17524047358085,21.0712239844648));
#49235=CARTESIAN_POINT('Ctrl Pts',(30.,-1.17524047358085,21.0625));
#49236=CARTESIAN_POINT('Ctrl Pts',(30.0000000000005,-1.17524047358085,21.));
#49237=CARTESIAN_POINT('Ctrl Pts',(30.0409368563611,-1.17524047358083,21.0025138371222));
#49238=CARTESIAN_POINT('Ctrl Pts',(30.0819173014533,-1.17310176285816,21.0051061762144));
#49239=CARTESIAN_POINT('Ctrl Pts',(30.2729829235624,-1.15303120950392,21.0175506477331));
#49240=CARTESIAN_POINT('Ctrl Pts',(30.4187156327833,-1.10844931428969,21.0280803491923));
#49241=CARTESIAN_POINT('Ctrl Pts',(30.6905353954506,-0.963834030798816,
21.0498993207407));
#49242=CARTESIAN_POINT('Ctrl Pts',(30.8129383742835,-0.863111359129209,
21.0609867980498));
#49243=CARTESIAN_POINT('Ctrl Pts',(31.0063964161767,-0.625120486728277,
21.0813042721815));
#49244=CARTESIAN_POINT('Ctrl Pts',(31.0777548462909,-0.49199236060375,21.0901140644785));
#49245=CARTESIAN_POINT('Ctrl Pts',(31.1675962416571,-0.203110857145286,
21.1105979221763));
#49246=CARTESIAN_POINT('Ctrl Pts',(31.1840814343856,-0.0497708726068158,
21.1214708731443));
#49247=CARTESIAN_POINT('Ctrl Pts',(31.1571888276141,0.257674311285982,21.14327103453));
#49248=CARTESIAN_POINT('Ctrl Pts',(31.1128522255693,0.408737402730974,21.1539825367601));
#49249=CARTESIAN_POINT('Ctrl Pts',(30.9710010878299,0.678628541040232,21.1731198356347));
#49250=CARTESIAN_POINT('Ctrl Pts',(30.8772391714915,0.796156039182743,21.1826908232652));
#49251=CARTESIAN_POINT('Ctrl Pts',(30.6464955823919,0.993543206250726,21.2038583630273));
#49252=CARTESIAN_POINT('Ctrl Pts',(30.5103519798164,1.06987223749504,21.214924774365));
#49253=CARTESIAN_POINT('Ctrl Pts',(30.2162079552513,1.16549604568273,21.2363776960251));
#49254=CARTESIAN_POINT('Ctrl Pts',(30.061127965963,1.18379547472913,21.2459429670447));
#49255=CARTESIAN_POINT('Ctrl Pts',(29.7567781749822,1.15962478754955,21.2654893209196));
#49256=CARTESIAN_POINT('Ctrl Pts',(29.6103180879013,1.11893466526318,21.2759257110673));
#49257=CARTESIAN_POINT('Ctrl Pts',(29.3355002124366,0.981897695520532,21.2976601102058));
#49258=CARTESIAN_POINT('Ctrl Pts',(29.2107776319456,0.884773136393355,21.3087624623211));
#49259=CARTESIAN_POINT('Ctrl Pts',(29.0107746609087,0.652081932742376,21.3292939522647));
#49260=CARTESIAN_POINT('Ctrl Pts',(28.9355970901093,0.52040794626517,21.3380991870768));
#49261=CARTESIAN_POINT('Ctrl Pts',(28.8382134265824,0.233810524699486,21.3584210862971));
#49262=CARTESIAN_POINT('Ctrl Pts',(28.8177208295725,0.0813648692728661,
21.3692306226469));
#49263=CARTESIAN_POINT('Ctrl Pts',(28.8362699803681,-0.22632694032349,21.3910482716382));
#49264=CARTESIAN_POINT('Ctrl Pts',(28.8765201026755,-0.378558584509325,
21.4018426329915));
#49265=CARTESIAN_POINT('Ctrl Pts',(29.0110211856253,-0.652134791815677,
21.4212412308003));
#49266=CARTESIAN_POINT('Ctrl Pts',(29.1015077791443,-0.772069972681635,
21.4305317818752));
#49267=CARTESIAN_POINT('Ctrl Pts',(29.3264048767426,-0.975307798634206,
21.4515477299157));
#49268=CARTESIAN_POINT('Ctrl Pts',(29.4600073333855,-1.05515984377402,21.4625829994009));
#49269=CARTESIAN_POINT('Ctrl Pts',(29.7321091399909,-1.15220558787994,21.4827327726726));
#49270=CARTESIAN_POINT('Ctrl Pts',(29.8656344449969,-1.17524047358088,21.4917489238272));
#49271=CARTESIAN_POINT('Ctrl Pts',(30.0000000000003,-1.17524047358085,21.5));
#49272=CARTESIAN_POINT('Origin',(30.,-1.21864324187371E-14,15.78125));
#49273=CARTESIAN_POINT('',(29.9999999999998,-1.17524047358085,22.0625));
#49274=CARTESIAN_POINT('',(30.000000003784,-1.17524047358085,22.0000000004647));
#49275=CARTESIAN_POINT('',(30.,-1.17524047358085,15.78125));
#49276=CARTESIAN_POINT('Ctrl Pts',(29.9999999999997,-1.17524047358085,22.0625));
#49277=CARTESIAN_POINT('Ctrl Pts',(29.9524010211782,-1.17524047358085,22.0595770574349));
#49278=CARTESIAN_POINT('Ctrl Pts',(29.9047586284152,-1.17234913259513,22.0565489400777));
#49279=CARTESIAN_POINT('Ctrl Pts',(29.7009349924679,-1.1474210952591,22.0431488126472));
#49280=CARTESIAN_POINT('Ctrl Pts',(29.5500039838267,-1.09704169086814,22.0320943523472));
#49281=CARTESIAN_POINT('Ctrl Pts',(29.2822334508411,-0.942842462410207,
22.01018424791));
#49282=CARTESIAN_POINT('Ctrl Pts',(29.1667766500969,-0.842552714869588,
21.9995386680174));
#49283=CARTESIAN_POINT('Ctrl Pts',(28.9799931885339,-0.603233884932394,
21.9795839832802));
#49284=CARTESIAN_POINT('Ctrl Pts',(28.910605612196,-0.466400997640195,21.9705713166174));
#49285=CARTESIAN_POINT('Ctrl Pts',(28.8268127379948,-0.170385863417145,
21.9495816311816));
#49286=CARTESIAN_POINT('Ctrl Pts',(28.8145871174915,-0.0137497615287427,
21.9384749608582));
#49287=CARTESIAN_POINT('Ctrl Pts',(28.85113877829,0.289356743861303,21.9169824442057));
#49288=CARTESIAN_POINT('Ctrl Pts',(28.8973142483913,0.433263084581444,21.9067784090915));
#49289=CARTESIAN_POINT('Ctrl Pts',(29.0441562961032,0.701308793511537,21.8877719649526));
#49290=CARTESIAN_POINT('Ctrl Pts',(29.145494108998,0.821789237943167,21.8775043861745));
#49291=CARTESIAN_POINT('Ctrl Pts',(29.3876377187977,1.01480099788269,21.8557919221934));
#49292=CARTESIAN_POINT('Ctrl Pts',(29.5254500415353,1.08610079854932,21.8448013436507));
#49293=CARTESIAN_POINT('Ctrl Pts',(29.8162261597603,1.17031056565349,21.8239599076952));
#49294=CARTESIAN_POINT('Ctrl Pts',(29.965897796871,1.18415559330363,21.814910211276));
#49295=CARTESIAN_POINT('Ctrl Pts',(30.2694248477664,1.15452627142302,21.7952208509568));
#49296=CARTESIAN_POINT('Ctrl Pts',(30.4200757340443,1.10861951539323,21.7843421644183));
#49297=CARTESIAN_POINT('Ctrl Pts',(30.6910871340011,0.962634653497324,21.762524275871));
#49298=CARTESIAN_POINT('Ctrl Pts',(30.8096198631452,0.865330005993902,21.7517956433222));
#49299=CARTESIAN_POINT('Ctrl Pts',(31.0025452942337,0.631606479581076,21.7316621689435));
#49300=CARTESIAN_POINT('Ctrl Pts',(31.075346835895,0.497649504779323,21.7227870693252));
#49301=CARTESIAN_POINT('Ctrl Pts',(31.1677479593254,0.204711362167963,21.7020155655921));
#49302=CARTESIAN_POINT('Ctrl Pts',(31.1845780485819,0.0480344792828584,
21.6909060035913));
#49303=CARTESIAN_POINT('Ctrl Pts',(31.1566162472742,-0.256851307753155,
21.6692873225717));
#49304=CARTESIAN_POINT('Ctrl Pts',(31.1143736239456,-0.402401296420415,
21.6589667405334));
#49305=CARTESIAN_POINT('Ctrl Pts',(30.9745867433069,-0.675115053903835,
21.6396292968631));
#49306=CARTESIAN_POINT('Ctrl Pts',(30.8762946890393,-0.798585224220405,
21.6296650545771));
#49307=CARTESIAN_POINT('Ctrl Pts',(30.6387793080734,-0.998444700485959,
21.6079940222289));
#49308=CARTESIAN_POINT('Ctrl Pts',(30.5025155082578,-1.07350395293815,21.5969652482617));
#49309=CARTESIAN_POINT('Ctrl Pts',(30.2404480736925,-1.15671325182863,21.5779222161248));
#49310=CARTESIAN_POINT('Ctrl Pts',(30.1205093503255,-1.17524047358085,21.5699001988757));
#49311=CARTESIAN_POINT('Ctrl Pts',(29.9999999999996,-1.17524047358085,21.5625));
#49312=CARTESIAN_POINT('Ctrl Pts',(30.0000000000003,-1.17524047358085,21.5));
#49313=CARTESIAN_POINT('Ctrl Pts',(30.0212839202784,-1.17524047358085,21.5013069960338));
#49314=CARTESIAN_POINT('Ctrl Pts',(30.0425864419315,-1.17466229796956,21.5026356328208));
#49315=CARTESIAN_POINT('Ctrl Pts',(30.2139454930837,-1.16533366693515,21.5134891283695));
#49316=CARTESIAN_POINT('Ctrl Pts',(30.3610177391346,-1.12845915530085,21.523827832119));
#49317=CARTESIAN_POINT('Ctrl Pts',(30.6385696146112,-0.998891400827412,
21.5454653082446));
#49318=CARTESIAN_POINT('Ctrl Pts',(30.7654630357173,-0.905335035089088,
21.5565744608423));
#49319=CARTESIAN_POINT('Ctrl Pts',(30.9718229035628,-0.677897335355307,
21.5773100566854));
#49320=CARTESIAN_POINT('Ctrl Pts',(31.0507577571561,-0.547623084998762,
21.5861694304673));
#49321=CARTESIAN_POINT('Ctrl Pts',(31.1570604439752,-0.258809326298121,
21.6066484845527));
#49322=CARTESIAN_POINT('Ctrl Pts',(31.1812214838473,-0.102338491331391,
21.6177434360859));
#49323=CARTESIAN_POINT('Ctrl Pts',(31.1670292938221,0.204877234262332,21.6395273271632));
#49324=CARTESIAN_POINT('Ctrl Pts',(31.1311379778152,0.352813947812694,21.6500171458341));
#49325=CARTESIAN_POINT('Ctrl Pts',(31.0040616369159,0.629882761963365,21.6696633955718));
#49326=CARTESIAN_POINT('Ctrl Pts',(30.9130181373807,0.755846555951633,21.6790645983814));
#49327=CARTESIAN_POINT('Ctrl Pts',(30.6868446220844,0.966129203413541,21.7004086935125));
#49328=CARTESIAN_POINT('Ctrl Pts',(30.553735937256,1.0481102897547,21.711489124086));
#49329=CARTESIAN_POINT('Ctrl Pts',(30.2686762405413,1.15380487275931,21.7327412449065));
#49330=CARTESIAN_POINT('Ctrl Pts',(30.1202468756007,1.17853792824007,21.7424990119962));
#49331=CARTESIAN_POINT('Ctrl Pts',(29.8153503696085,1.17107054155024,21.7614867439455));
#49332=CARTESIAN_POINT('Ctrl Pts',(29.661826921183,1.13627251461424,21.7721479818837));
#49333=CARTESIAN_POINT('Ctrl Pts',(29.3799800833098,1.01003478165367,21.7939311399523));
#49334=CARTESIAN_POINT('Ctrl Pts',(29.253891997555,0.920828765085568,21.8048366026441));
#49335=CARTESIAN_POINT('Ctrl Pts',(29.0454103417907,0.701638656512355,21.8254100846196));
#49336=CARTESIAN_POINT('Ctrl Pts',(28.9640200854668,0.5746995746724,21.8342495048467));
#49337=CARTESIAN_POINT('Ctrl Pts',(28.8502724171258,0.289883112959693,21.8544451207025));
#49338=CARTESIAN_POINT('Ctrl Pts',(28.8218581810328,0.133683866085342,21.8655208147403));
#49339=CARTESIAN_POINT('Ctrl Pts',(28.8280094580603,-0.174601530686287,
21.8873805534988));
#49340=CARTESIAN_POINT('Ctrl Pts',(28.8601657562679,-0.323793761637004,
21.8979593977371));
#49341=CARTESIAN_POINT('Ctrl Pts',(28.9799119697649,-0.603297917389521,
21.9177783313962));
#49342=CARTESIAN_POINT('Ctrl Pts',(29.0669039974813,-0.730676428244075,
21.9269392883002));
#49343=CARTESIAN_POINT('Ctrl Pts',(29.2865672059309,-0.946735069741176,
21.9480883812055));
#49344=CARTESIAN_POINT('Ctrl Pts',(29.4177292577255,-1.03259356038437,21.9591867420451));
#49345=CARTESIAN_POINT('Ctrl Pts',(29.7004129009365,-1.14619538664958,21.98057329627));
#49346=CARTESIAN_POINT('Ctrl Pts',(29.8484560704769,-1.17497884076058,21.9906847639469));
#49347=CARTESIAN_POINT('Ctrl Pts',(29.9986381885534,-1.17523988185415,21.9999163533479));
#49348=CARTESIAN_POINT('Ctrl Pts',(29.9993191103818,-1.17524047358524,21.9999581881525));
#49349=CARTESIAN_POINT('Ctrl Pts',(30.0000000075681,-1.17524047358085,22.0000000004647));
#49350=CARTESIAN_POINT('Origin',(30.,-1.21864324187371E-14,15.78125));
#49351=CARTESIAN_POINT('',(30.,-1.17524047358085,22.5625));
#49352=CARTESIAN_POINT('',(29.9999999999999,-1.17524047358085,22.4999999999999));
#49353=CARTESIAN_POINT('',(30.,-1.17524047358085,15.78125));
#49354=CARTESIAN_POINT('Ctrl Pts',(30.,-1.17524047358085,22.5625));
#49355=CARTESIAN_POINT('Ctrl Pts',(29.9313687068489,-1.17524047358085,22.5582855119371));
#49356=CARTESIAN_POINT('Ctrl Pts',(29.8627268799626,-1.16923029327301,22.55385729367));
#49357=CARTESIAN_POINT('Ctrl Pts',(29.6405360439417,-1.12983827415446,22.5388164770024));
#49358=CARTESIAN_POINT('Ctrl Pts',(29.4932720438495,-1.07189657475161,22.5277190875488));
#49359=CARTESIAN_POINT('Ctrl Pts',(29.2351505504649,-0.904940984815958,
22.505949247503));
#49360=CARTESIAN_POINT('Ctrl Pts',(29.125477326134,-0.799463570556349,22.4954749014128));
#49361=CARTESIAN_POINT('Ctrl Pts',(28.9500348086396,-0.550024618450246,
22.4758578415198));
#49362=CARTESIAN_POINT('Ctrl Pts',(28.8870166724079,-0.407722193677489,
22.4664105508506));
#49363=CARTESIAN_POINT('Ctrl Pts',(28.8193863135494,-0.106256134735224,
22.4450343541119));
#49364=CARTESIAN_POINT('Ctrl Pts',(28.8156683957017,0.0499559751614321,
22.4339577479897));
#49365=CARTESIAN_POINT('Ctrl Pts',(28.8680054797788,0.349324836623415,22.4127302582268));
#49366=CARTESIAN_POINT('Ctrl Pts',(28.9214162690158,0.489956671932254,22.4030291896045));
#49367=CARTESIAN_POINT('Ctrl Pts',(29.0814696037689,0.749536525817022,22.3839976107609));
#49368=CARTESIAN_POINT('Ctrl Pts',(29.1888834831425,0.864620134172483,22.3733214303097));
#49369=CARTESIAN_POINT('Ctrl Pts',(29.4398862783311,1.04443640573476,22.3515327737366));
#49370=CARTESIAN_POINT('Ctrl Pts',(29.5804046735503,1.10838743829029,22.3406365628695));
#49371=CARTESIAN_POINT('Ctrl Pts',(29.874773559948,1.17808176091705,22.320089130129));
#49372=CARTESIAN_POINT('Ctrl Pts',(30.0254999210416,1.18444262102585,22.3112603596819));
#49373=CARTESIAN_POINT('Ctrl Pts',(30.3288317944626,1.13918974891494,22.2910290715165));
#49374=CARTESIAN_POINT('Ctrl Pts',(30.4780087858284,1.08506931516396,22.2799496878662));
#49375=CARTESIAN_POINT('Ctrl Pts',(30.7411182596149,0.924538989516088,22.2581013471772));
#49376=CARTESIAN_POINT('Ctrl Pts',(30.8537656083098,0.82166305580017,22.2475365992352));
#49377=CARTESIAN_POINT('Ctrl Pts',(31.0350106463268,0.577368135111118,22.2277455951917));
#49378=CARTESIAN_POINT('Ctrl Pts',(31.1013006049905,0.437889260334813,22.2185496213456));
#49379=CARTESIAN_POINT('Ctrl Pts',(31.1772437890897,0.139172903087767,22.1973683990083));
#49380=CARTESIAN_POINT('Ctrl Pts',(31.185313349087,-0.0173128950364053,
22.1862723863453));
#49381=CARTESIAN_POINT('Ctrl Pts',(31.1410279217834,-0.318736522964712,
22.1648991982826));
#49382=CARTESIAN_POINT('Ctrl Pts',(31.0912903592309,-0.461049327500964,
22.1548343474741));
#49383=CARTESIAN_POINT('Ctrl Pts',(30.9380306919572,-0.724977765907907,
22.136065778375));
#49384=CARTESIAN_POINT('Ctrl Pts',(30.8337205687989,-0.842838844072579,
22.1254817206889));
#49385=CARTESIAN_POINT('Ctrl Pts',(30.5872857957992,-1.02946130111843,22.1037322710222));
#49386=CARTESIAN_POINT('Ctrl Pts',(30.4481174203718,-1.09722011431045,22.0927839616769));
#49387=CARTESIAN_POINT('Ctrl Pts',(30.2017882631029,-1.16222172164091,22.0753529112466));
#49388=CARTESIAN_POINT('Ctrl Pts',(30.1010204315162,-1.17524047358085,22.0687034297066));
#49389=CARTESIAN_POINT('Ctrl Pts',(29.9999999999997,-1.17524047358085,22.0625));
#49390=CARTESIAN_POINT('Ctrl Pts',(30.0000000075681,-1.17524047358085,22.0000000004647));
#49391=CARTESIAN_POINT('Ctrl Pts',(30.1550617076756,-1.17524047258231,22.0095219788006));
#49392=CARTESIAN_POINT('Ctrl Pts',(30.3087125624576,-1.14455036320512,22.020045399438));
#49393=CARTESIAN_POINT('Ctrl Pts',(30.5936146237504,-1.02583437646268,22.0417494976575));
#49394=CARTESIAN_POINT('Ctrl Pts',(30.7222919834293,-0.9396884903777,22.0527054685765));
#49395=CARTESIAN_POINT('Ctrl Pts',(30.9363028934711,-0.725796874489648,
22.0734306378289));
#49396=CARTESIAN_POINT('Ctrl Pts',(31.0207456221836,-0.60126080890756,22.0823661148205));
#49397=CARTESIAN_POINT('Ctrl Pts',(31.1412832329984,-0.320931550152795,
22.1022435544492));
#49398=CARTESIAN_POINT('Ctrl Pts',(31.1737467539974,-0.166807893544759,
22.1131720736242));
#49399=CARTESIAN_POINT('Ctrl Pts',(31.1765934878998,0.140728845238564,22.1349787269359));
#49400=CARTESIAN_POINT('Ctrl Pts',(31.148646481366,0.291209583454888,22.1456489359696));
#49401=CARTESIAN_POINT('Ctrl Pts',(31.0370532707971,0.573358102978206,22.165655374784));
#49402=CARTESIAN_POINT('Ctrl Pts',(30.9544609034821,0.702301510156061,22.1746213225474));
#49403=CARTESIAN_POINT('Ctrl Pts',(30.7420042686145,0.924591934894812,22.1955488165371));
#49404=CARTESIAN_POINT('Ctrl Pts',(30.6131073712558,1.01465868002552,22.2066572778597));
#49405=CARTESIAN_POINT('Ctrl Pts',(30.3331026676289,1.1369643062698,22.228187906872));
#49406=CARTESIAN_POINT('Ctrl Pts',(30.1855325771707,1.17014774287538,22.2384263196851));
#49407=CARTESIAN_POINT('Ctrl Pts',(29.8783465649041,1.17947691083341,22.2576206519922));
#49408=CARTESIAN_POINT('Ctrl Pts',(29.7215875906434,1.15260328305267,22.2678992314176));
#49409=CARTESIAN_POINT('Ctrl Pts',(29.4314038660401,1.03996407151785,22.2897122199048));
#49410=CARTESIAN_POINT('Ctrl Pts',(29.3003745517226,0.9567417174806,22.3007089687507));
#49411=CARTESIAN_POINT('Ctrl Pts',(29.0812311411824,0.747835374300097,22.3215725663721));
#49412=CARTESIAN_POINT('Ctrl Pts',(28.9939461402353,0.625488946274541,22.3306481587999));
#49413=CARTESIAN_POINT('Ctrl Pts',(28.866779072646,0.34832483100282,22.3503011660994));
#49414=CARTESIAN_POINT('Ctrl Pts',(28.8306169080572,0.195045951299282,22.3611697842779));
#49415=CARTESIAN_POINT('Ctrl Pts',(28.8203429359976,-0.112665031360941,
22.3829887927828));
#49416=CARTESIAN_POINT('Ctrl Pts',(28.844778193878,-0.264121048518041,22.3937281563827));
#49417=CARTESIAN_POINT('Ctrl Pts',(28.9496447173484,-0.548400594969454,
22.4138857009336));
#49418=CARTESIAN_POINT('Ctrl Pts',(29.0286885091485,-0.678634752036216,
22.4227474921567));
#49419=CARTESIAN_POINT('Ctrl Pts',(29.2352313232766,-0.905919594975383,
22.4434889029608));
#49420=CARTESIAN_POINT('Ctrl Pts',(29.3621859947411,-0.999372204838993,
22.454598138267));
#49421=CARTESIAN_POINT('Ctrl Pts',(29.6398139077013,-1.12872343697434,22.4762326071516));
#49422=CARTESIAN_POINT('Ctrl Pts',(29.7869023742936,-1.1654876328242,22.4865683958599));
#49423=CARTESIAN_POINT('Ctrl Pts',(29.9579757834663,-1.17467745886044,22.4973994296432));
#49424=CARTESIAN_POINT('Ctrl Pts',(29.9789969929607,-1.17524047358085,22.4987102541947));
#49425=CARTESIAN_POINT('Ctrl Pts',(29.9999999999997,-1.17524047358085,22.4999999999999));
#49426=CARTESIAN_POINT('Origin',(30.,-1.21864324187371E-14,15.78125));
#49427=CARTESIAN_POINT('',(30.,-1.17524047358085,23.0625));
#49428=CARTESIAN_POINT('',(29.9999999999997,-1.17524047358085,22.9999999999999));
#49429=CARTESIAN_POINT('',(30.,-1.17524047358085,15.78125));
#49430=CARTESIAN_POINT('Ctrl Pts',(30.0000000000001,-1.17524047358085,23.0625));
#49431=CARTESIAN_POINT('Ctrl Pts',(29.9105144759955,-1.17524047358086,23.0570049021313));
#49432=CARTESIAN_POINT('Ctrl Pts',(29.8211453329131,-1.16502438899623,23.0511547525684));
#49433=CARTESIAN_POINT('Ctrl Pts',(29.5817638222111,-1.10931034878277,23.0344796199141));
#49434=CARTESIAN_POINT('Ctrl Pts',(29.4384864599594,-1.04411918186912,23.0233700199021));
#49435=CARTESIAN_POINT('Ctrl Pts',(29.1904963016638,-0.865097093142698,
23.001794519102));
#49436=CARTESIAN_POINT('Ctrl Pts',(29.0867727283959,-0.754802905276228,
22.9915147546188));
#49437=CARTESIAN_POINT('Ctrl Pts',(28.9228010666229,-0.495400927229172,
22.9722488667908));
#49438=CARTESIAN_POINT('Ctrl Pts',(28.8663568012591,-0.347374707529959,
22.9621314630453));
#49439=CARTESIAN_POINT('Ctrl Pts',(28.8154245654916,-0.0407388679671123,
22.9403886902216));
#49440=CARTESIAN_POINT('Ctrl Pts',(28.820274444704,0.114581560721945,22.9293753109615));
#49441=CARTESIAN_POINT('Ctrl Pts',(28.8884563534747,0.409699470717337,22.9084492454292));
#49442=CARTESIAN_POINT('Ctrl Pts',(28.9492618301764,0.547097841052301,22.8992933904858));
#49443=CARTESIAN_POINT('Ctrl Pts',(29.1229462954904,0.797680554149997,22.8797437378863));
#49444=CARTESIAN_POINT('Ctrl Pts',(29.2364128570735,0.906879897838648,22.8689044954722));
#49445=CARTESIAN_POINT('Ctrl Pts',(29.4960880788397,1.07256979024568,22.8470841182882));
#49446=CARTESIAN_POINT('Ctrl Pts',(29.6390279331417,1.12873587584898,22.8363152167134));
#49447=CARTESIAN_POINT('Ctrl Pts',(29.9369514995214,1.18318311725145,22.8160900653519));
#49448=CARTESIAN_POINT('Ctrl Pts',(30.0889739777062,1.18151676550276,22.8072588330028));
#49449=CARTESIAN_POINT('Ctrl Pts',(30.3896701123462,1.11972025811827,22.7866028657307));
#49450=CARTESIAN_POINT('Ctrl Pts',(30.5349379950004,1.05803905954289,22.7754954739854));
#49451=CARTESIAN_POINT('Ctrl Pts',(30.7879462278465,0.88483838172195,22.7538182156715));
#49452=CARTESIAN_POINT('Ctrl Pts',(30.894602280459,0.776856295524231,22.7434403470977));
#49453=CARTESIAN_POINT('Ctrl Pts',(31.0642088755634,0.522314474535101,22.7240007418519));
#49454=CARTESIAN_POINT('Ctrl Pts',(31.1239021773863,0.377122301428262,22.7142407897863));
#49455=CARTESIAN_POINT('Ctrl Pts',(31.1830807507881,0.07297978420699,22.6926748121518));
#49456=CARTESIAN_POINT('Ctrl Pts',(31.1824316194307,-0.0828368341019099,
22.681626249339));
#49457=CARTESIAN_POINT('Ctrl Pts',(31.1220212984731,-0.380073436416841,
22.6605499526862));
#49458=CARTESIAN_POINT('Ctrl Pts',(31.0648726782981,-0.5190454232441,22.6511559208149));
#49459=CARTESIAN_POINT('Ctrl Pts',(30.897916936256,-0.774116322820778,22.6318603404761));
#49460=CARTESIAN_POINT('Ctrl Pts',(30.7874073117601,-0.886271721025917,
22.6210978735108));
#49461=CARTESIAN_POINT('Ctrl Pts',(30.5319280571356,-1.05901132752472,22.5992852221989));
#49462=CARTESIAN_POINT('Ctrl Pts',(30.390134598554,-1.11904322637321,22.5884496605924));
#49463=CARTESIAN_POINT('Ctrl Pts',(30.1614293865023,-1.16692310230727,22.5727078850032));
#49464=CARTESIAN_POINT('Ctrl Pts',(30.0807402688424,-1.17524047358085,22.5674580720923));
#49465=CARTESIAN_POINT('Ctrl Pts',(30.,-1.17524047358085,22.5625));
#49466=CARTESIAN_POINT('Ctrl Pts',(29.9999999999997,-1.17524047358085,22.4999999999999));
#49467=CARTESIAN_POINT('Ctrl Pts',(30.1346907701741,-1.17524047358085,22.5082710468799));
#49468=CARTESIAN_POINT('Ctrl Pts',(30.2685335864829,-1.15209385827977,22.5173106568969));
#49469=CARTESIAN_POINT('Ctrl Pts',(30.5408486178537,-1.05471955701661,22.5374851723845));
#49470=CARTESIAN_POINT('Ctrl Pts',(30.6743758210798,-0.974766233245233,
22.5485194114384));
#49471=CARTESIAN_POINT('Ctrl Pts',(30.8991023951896,-0.771359157149707,
22.5695308885782));
#49472=CARTESIAN_POINT('Ctrl Pts',(30.9894938192057,-0.651353133995038,
22.5788141945814));
#49473=CARTESIAN_POINT('Ctrl Pts',(31.1237789969096,-0.377670022359416,
22.598220372706));
#49474=CARTESIAN_POINT('Ctrl Pts',(31.1639088895479,-0.225405854113982,
22.6090170402582));
#49475=CARTESIAN_POINT('Ctrl Pts',(31.1822136536976,0.0822897394418652,
22.6308349575606));
#49476=CARTESIAN_POINT('Ctrl Pts',(31.1616041653703,0.234707632570292,22.6416425253559));
#49477=CARTESIAN_POINT('Ctrl Pts',(31.0639996311159,0.521237294982461,22.6619596199458));
#49478=CARTESIAN_POINT('Ctrl Pts',(30.9887089758802,0.652868889710107,22.6707656569643));
#49479=CARTESIAN_POINT('Ctrl Pts',(30.7885136410845,0.885402585167096,22.6913033752648));
#49480=CARTESIAN_POINT('Ctrl Pts',(30.6637241461389,0.982420191755087,22.7024060445739));
#49481=CARTESIAN_POINT('Ctrl Pts',(30.38882091141,1.11923262290395,22.724137724694));
#49482=CARTESIAN_POINT('Ctrl Pts',(30.2423409189137,1.15980775171446,22.7345712602384));
#49483=CARTESIAN_POINT('Ctrl Pts',(29.9379463484727,1.1837522744206,22.75411234554));
#49484=CARTESIAN_POINT('Ctrl Pts',(29.7828414350779,1.1653244529442,22.7636867623073));
#49485=CARTESIAN_POINT('Ctrl Pts',(29.4887538037787,1.06944336967731,22.7851453423512));
#49486=CARTESIAN_POINT('Ctrl Pts',(29.3526850446683,0.993007607592932,22.7962109417328));
#49487=CARTESIAN_POINT('Ctrl Pts',(29.1221162292212,0.795444169323972,22.8173739985243));
#49488=CARTESIAN_POINT('Ctrl Pts',(29.0284526004007,0.677845266859518,22.8269357043589));
#49489=CARTESIAN_POINT('Ctrl Pts',(28.8868197290406,0.407843425299078,22.8460808529214));
#49490=CARTESIAN_POINT('Ctrl Pts',(28.8426042638403,0.256743916657897,22.8567949374029));
#49491=CARTESIAN_POINT('Ctrl Pts',(28.8159600292804,-0.0507119050410385,
22.8785958530886));
#49492=CARTESIAN_POINT('Ctrl Pts',(28.8325649861531,-0.204026768591548,
22.8894670227908));
#49493=CARTESIAN_POINT('Ctrl Pts',(28.9226310063267,-0.492841082076786,
22.9099461162173));
#49494=CARTESIAN_POINT('Ctrl Pts',(28.994102015515,-0.625925698199416,22.918754883105));
#49495=CARTESIAN_POINT('Ctrl Pts',(29.1877542901984,-0.863760919482141,
22.9390787662067));
#49496=CARTESIAN_POINT('Ctrl Pts',(29.3102272892874,-0.964377961033194,
22.9501667983144));
#49497=CARTESIAN_POINT('Ctrl Pts',(29.5821386201159,-1.10877008329771,22.9719834809511));
#49498=CARTESIAN_POINT('Ctrl Pts',(29.7278943046296,-1.1532370774207,22.9825105195965));
#49499=CARTESIAN_POINT('Ctrl Pts',(29.9186700556686,-1.17313232338821,22.9949309755051));
#49500=CARTESIAN_POINT('Ctrl Pts',(29.9593567068785,-1.17524047358085,22.9975041899134));
#49501=CARTESIAN_POINT('Ctrl Pts',(29.9999999999995,-1.17524047358085,22.9999999999999));
#49502=CARTESIAN_POINT('Origin',(30.,-1.21864324187371E-14,15.78125));
#49503=CARTESIAN_POINT('',(30.0000000000003,-1.17524047358085,23.5625));
#49504=CARTESIAN_POINT('',(30.,-1.17524047358085,23.5));
#49505=CARTESIAN_POINT('',(30.,-1.17524047358085,15.78125));
#49506=CARTESIAN_POINT('Ctrl Pts',(30.0000000000005,-1.17524047358085,23.5625));
#49507=CARTESIAN_POINT('Ctrl Pts',(29.8877180837681,-1.1752404735809,23.5556050287134));
#49508=CARTESIAN_POINT('Ctrl Pts',(29.7758372881673,-1.15915740880452,23.548164484563));
#49509=CARTESIAN_POINT('Ctrl Pts',(29.5190446425994,-1.08346545175016,23.5297118828087));
#49510=CARTESIAN_POINT('Ctrl Pts',(29.3805019669677,-1.01066023747548,23.5186230824555));
#49511=CARTESIAN_POINT('Ctrl Pts',(29.1440648218203,-0.81906365611398,23.4973112125635));
#49512=CARTESIAN_POINT('Ctrl Pts',(29.0470865676084,-0.703844960553528,
23.4874078682461));
#49513=CARTESIAN_POINT('Ctrl Pts',(28.8981724330839,-0.43757763652763,23.4685275248886));
#49514=CARTESIAN_POINT('Ctrl Pts',(28.8499251562346,-0.287749538271772,
23.4579035929059));
#49515=CARTESIAN_POINT('Ctrl Pts',(28.8149793372208,0.0192409990811535,
23.4361356693579));
#49516=CARTESIAN_POINT('Ctrl Pts',(28.8275655785823,0.173345465604893,23.4252085109033));
#49517=CARTESIAN_POINT('Ctrl Pts',(28.9101166290744,0.46437979734691,23.4045720015899));
#49518=CARTESIAN_POINT('Ctrl Pts',(28.9778580847147,0.598927911512345,23.3956997913279));
#49519=CARTESIAN_POINT('Ctrl Pts',(29.1650362747697,0.841899704480849,23.3755913560416));
#49520=CARTESIAN_POINT('Ctrl Pts',(29.2851376881026,0.945999066866448,23.3645254962114));
#49521=CARTESIAN_POINT('Ctrl Pts',(29.5539135664443,1.09777062977422,23.3426397256705));
#49522=CARTESIAN_POINT('Ctrl Pts',(29.6988585362439,1.14604691671332,23.3320274174642));
#49523=CARTESIAN_POINT('Ctrl Pts',(30.0001600354305,1.18508412542801,23.3121411783529));
#49524=CARTESIAN_POINT('Ctrl Pts',(30.1536625413848,1.17508243739145,23.3030583378086));
#49525=CARTESIAN_POINT('Ctrl Pts',(30.4512625228178,1.09622449574564,23.2819876064994));
#49526=CARTESIAN_POINT('Ctrl Pts',(30.592110439614,1.02700793469459,23.2708844778163));
#49527=CARTESIAN_POINT('Ctrl Pts',(30.8340714315268,0.841360319080231,23.2494443144111));
#49528=CARTESIAN_POINT('Ctrl Pts',(30.9343059293982,0.728463261371192,23.2392865244689));
#49529=CARTESIAN_POINT('Ctrl Pts',(31.0901832738534,0.465790392750319,23.2204017245443));
#49530=CARTESIAN_POINT('Ctrl Pts',(31.1423055420081,0.317257314781848,23.2099959148018));
#49531=CARTESIAN_POINT('Ctrl Pts',(31.1851773743111,0.010751647338072,23.1882623721543));
#49532=CARTESIAN_POINT('Ctrl Pts',(31.1764469607209,-0.144008319910697,
23.1772887337992));
#49533=CARTESIAN_POINT('Ctrl Pts',(31.1010701340243,-0.437108167734962,
23.1565057639579));
#49534=CARTESIAN_POINT('Ctrl Pts',(31.0368218842674,-0.573070176242618,
23.1475180074206));
#49535=CARTESIAN_POINT('Ctrl Pts',(30.8568360573785,-0.819362332337596,
23.1277335191445));
#49536=CARTESIAN_POINT('Ctrl Pts',(30.7406590361852,-0.925703986430565,
23.1168291494862));
#49537=CARTESIAN_POINT('Ctrl Pts',(30.477211273408,-1.08466164141258,23.0950157923094));
#49538=CARTESIAN_POINT('Ctrl Pts',(30.3332866239118,-1.13717003604433,23.0843160955662));
#49539=CARTESIAN_POINT('Ctrl Pts',(30.1225555529996,-1.17045159552602,23.0701956350453));
#49540=CARTESIAN_POINT('Ctrl Pts',(30.0612610274847,-1.17524047358085,23.066261897193));
#49541=CARTESIAN_POINT('Ctrl Pts',(30.0000000000001,-1.17524047358085,23.0625));
#49542=CARTESIAN_POINT('Ctrl Pts',(29.9999999999995,-1.17524047358085,22.9999999999999));
#49543=CARTESIAN_POINT('Ctrl Pts',(30.1122819160637,-1.17524047358085,23.0068949712763));
#49544=CARTESIAN_POINT('Ctrl Pts',(30.2241627114991,-1.15915740885253,23.0143355154149));
#49545=CARTESIAN_POINT('Ctrl Pts',(30.4809553569443,-1.08346545195345,23.0327881171562));
#49546=CARTESIAN_POINT('Ctrl Pts',(30.6194980326123,-1.01066023773368,23.0438769175097));
#49547=CARTESIAN_POINT('Ctrl Pts',(30.8559351778473,-0.819063656461988,
23.0651887874038));
#49548=CARTESIAN_POINT('Ctrl Pts',(30.952913432109,-0.703844960936813,23.0750921317269));
#49549=CARTESIAN_POINT('Ctrl Pts',(31.1018275667414,-0.437577636966923,
23.0939724750804));
#49550=CARTESIAN_POINT('Ctrl Pts',(31.1500748436503,-0.287749538730812,
23.1045964070617));
#49551=CARTESIAN_POINT('Ctrl Pts',(31.1850206627874,0.0192409986134863,
23.126364330609));
#49552=CARTESIAN_POINT('Ctrl Pts',(31.1724344214858,0.173345465148191,23.1372914890643));
#49553=CARTESIAN_POINT('Ctrl Pts',(31.0898833711054,0.464379796922714,23.15792799838));
#49554=CARTESIAN_POINT('Ctrl Pts',(31.0221419155201,0.598927911110121,23.1668002086434));
#49555=CARTESIAN_POINT('Ctrl Pts',(30.8349637255609,0.841899704153978,23.1869086439265));
#49556=CARTESIAN_POINT('Ctrl Pts',(30.7148623122637,0.945999066590532,23.1979745037564));
#49557=CARTESIAN_POINT('Ctrl Pts',(30.4460864339697,1.09777062960664,23.2198602742982));
#49558=CARTESIAN_POINT('Ctrl Pts',(30.3011414641827,1.1460469166018,23.2304725825058));
#49559=CARTESIAN_POINT('Ctrl Pts',(29.9998399650194,1.18508412542607,23.2503588216195));
#49560=CARTESIAN_POINT('Ctrl Pts',(29.8463374590763,1.17508243744973,23.2594416621611));
#49561=CARTESIAN_POINT('Ctrl Pts',(29.5487374776195,1.09622449592641,23.2805123934674));
#49562=CARTESIAN_POINT('Ctrl Pts',(29.4078895607902,1.02700793492841,23.2916155221506));
#49563=CARTESIAN_POINT('Ctrl Pts',(29.1659285687959,0.841360319401014,23.3130556855578));
#49564=CARTESIAN_POINT('Ctrl Pts',(29.0656940708777,0.72846326172594,23.3232134755017));
#49565=CARTESIAN_POINT('Ctrl Pts',(28.9098167263205,0.465790393157422,23.3420982754308));
#49566=CARTESIAN_POINT('Ctrl Pts',(28.8576944581104,0.317257315207477,23.3525040851682));
#49567=CARTESIAN_POINT('Ctrl Pts',(28.8148226256923,0.0107516477743395,
23.3742376278149));
#49568=CARTESIAN_POINT('Ctrl Pts',(28.8235530392262,-0.144008319483296,
23.3852112661707));
#49569=CARTESIAN_POINT('Ctrl Pts',(28.8989298658185,-0.437108167337535,
23.4059942360141));
#49570=CARTESIAN_POINT('Ctrl Pts',(28.9631781155251,-0.573070175865714,
23.4149819925535));
#49571=CARTESIAN_POINT('Ctrl Pts',(29.1431639423218,-0.819362332023802,
23.4347664808262));
#49572=CARTESIAN_POINT('Ctrl Pts',(29.2593409634759,-0.925703986159073,
23.4456708504836));
#49573=CARTESIAN_POINT('Ctrl Pts',(29.5227887261992,-1.08466164124026,23.4674842076606));
#49574=CARTESIAN_POINT('Ctrl Pts',(29.6667133756817,-1.13717003592563,23.4781839044047));
#49575=CARTESIAN_POINT('Ctrl Pts',(29.8774444467245,-1.17045159550418,23.4923043649371));
#49576=CARTESIAN_POINT('Ctrl Pts',(29.9387389723772,-1.17524047358085,23.4962381027985));
#49577=CARTESIAN_POINT('Ctrl Pts',(29.9999999999999,-1.17524047358085,23.5));
#49578=CARTESIAN_POINT('Origin',(30.,-1.21864324187371E-14,15.78125));
#49579=CARTESIAN_POINT('',(30.0000000000001,-1.17524047358085,24.0625));
#49580=CARTESIAN_POINT('',(30.,-1.17524047358085,24.));
#49581=CARTESIAN_POINT('',(30.,-1.17524047358085,15.78125));
#49582=CARTESIAN_POINT('Ctrl Pts',(30.0000000000002,-1.17524047358085,24.0625));
#49583=CARTESIAN_POINT('Ctrl Pts',(29.8653092296601,-1.17524047358088,24.0542289531099));
#49584=CARTESIAN_POINT('Ctrl Pts',(29.7314664131893,-1.15209385822287,24.045189343081));
#49585=CARTESIAN_POINT('Ctrl Pts',(29.4591513817099,-1.05471955679206,24.0250148275808));
#49586=CARTESIAN_POINT('Ctrl Pts',(29.3256241785221,-0.974766232969058,
24.0139805885274));
#49587=CARTESIAN_POINT('Ctrl Pts',(29.1008976044993,-0.771359156787199,
23.99296911139));
#49588=CARTESIAN_POINT('Ctrl Pts',(29.0105061805318,-0.651353133596405,
23.9836858053905));
#49589=CARTESIAN_POINT('Ctrl Pts',(28.876221002938,-0.377670021906335,23.9642796272619));
#49590=CARTESIAN_POINT('Ctrl Pts',(28.8360911103609,-0.225405853644338,
23.9534829597086));
#49591=CARTESIAN_POINT('Ctrl Pts',(28.8177863463358,0.0822897399134218,
23.931665042406));
#49592=CARTESIAN_POINT('Ctrl Pts',(28.8383958347227,0.234707633027682,23.9208574746117));
#49593=CARTESIAN_POINT('Ctrl Pts',(28.9360003690899,0.521237295405437,23.9005403800242));
#49594=CARTESIAN_POINT('Ctrl Pts',(29.0112910243832,0.652868890111379,23.8917343430053));
#49595=CARTESIAN_POINT('Ctrl Pts',(29.211486359277,0.885402585487968,23.8711966247017));
#49596=CARTESIAN_POINT('Ctrl Pts',(29.3362758542566,0.98242019202142,23.8600939553924));
#49597=CARTESIAN_POINT('Ctrl Pts',(29.611179089029,1.11923262305578,23.8383622752737));
#49598=CARTESIAN_POINT('Ctrl Pts',(29.7576590815354,1.15980775180767,23.8279287397307));
#49599=CARTESIAN_POINT('Ctrl Pts',(30.0620536519992,1.1837522743985,23.8083876544318));
#49600=CARTESIAN_POINT('Ctrl Pts',(30.2171585654068,1.16532445285658,23.7988132376599));
#49601=CARTESIAN_POINT('Ctrl Pts',(30.5112461966771,1.06944336945855,23.7773546576131));
#49602=CARTESIAN_POINT('Ctrl Pts',(30.6473149557494,0.993007607319778,23.7662890582319));
#49603=CARTESIAN_POINT('Ctrl Pts',(30.8778837711073,0.795444168961031,23.7451260014428));
#49604=CARTESIAN_POINT('Ctrl Pts',(30.9715473998777,0.67784526646015,23.735564295613));
#49605=CARTESIAN_POINT('Ctrl Pts',(31.1131802711266,0.407843424843195,23.7164191470464));
#49606=CARTESIAN_POINT('Ctrl Pts',(31.1573957362652,0.25674391618342,23.7057050625635));
#49607=CARTESIAN_POINT('Ctrl Pts',(31.1840399706984,-0.0507119055208601,
23.6839041468775));
#49608=CARTESIAN_POINT('Ctrl Pts',(31.1674350137646,-0.204026769058537,
23.6730329771762));
#49609=CARTESIAN_POINT('Ctrl Pts',(31.0773689934766,-0.492841082509219,
23.6525538837521));
#49610=CARTESIAN_POINT('Ctrl Pts',(31.0058979842309,-0.625925698609867,
23.643745116865));
#49611=CARTESIAN_POINT('Ctrl Pts',(30.8122457094484,-0.863760919813326,
23.62342123376));
#49612=CARTESIAN_POINT('Ctrl Pts',(30.6897727103237,-0.964377961310509,
23.612333201652));
#49613=CARTESIAN_POINT('Ctrl Pts',(30.4178613794486,-1.10877008346121,23.5905165190165));
#49614=CARTESIAN_POINT('Ctrl Pts',(30.2721056949232,-1.15323707752562,23.5799894803724));
#49615=CARTESIAN_POINT('Ctrl Pts',(30.081329944032,-1.17313232340388,23.5675690244761));
#49616=CARTESIAN_POINT('Ctrl Pts',(30.0406432929718,-1.17524047358083,23.5649958100773));
#49617=CARTESIAN_POINT('Ctrl Pts',(30.0000000000005,-1.17524047358085,23.5625));
#49618=CARTESIAN_POINT('Ctrl Pts',(29.9999999999999,-1.17524047358085,23.5));
#49619=CARTESIAN_POINT('Ctrl Pts',(30.0894855238544,-1.17524047358085,23.5054950978594));
#49620=CARTESIAN_POINT('Ctrl Pts',(30.178854666788,-1.16502438903023,23.5113452474122));
#49621=CARTESIAN_POINT('Ctrl Pts',(30.4182361773703,-1.10931034894115,23.5280203800546));
#49622=CARTESIAN_POINT('Ctrl Pts',(30.5615135396518,-1.04411918207875,23.5391299800668));
#49623=CARTESIAN_POINT('Ctrl Pts',(30.8095036980223,-0.865097093436967,
23.5607054808684));
#49624=CARTESIAN_POINT('Ctrl Pts',(30.9132272713337,-0.75480290560396,23.5709852453531));
#49625=CARTESIAN_POINT('Ctrl Pts',(31.0771989331901,-0.495400927628404,
23.5902511331837));
#49626=CARTESIAN_POINT('Ctrl Pts',(31.1336431986023,-0.347374707971562,
23.6003685369235));
#49627=CARTESIAN_POINT('Ctrl Pts',(31.1845754344926,-0.0407388684447008,
23.6221113097446));
#49628=CARTESIAN_POINT('Ctrl Pts',(31.1797255553422,0.114581560252514,23.6331246890053));
#49629=CARTESIAN_POINT('Ctrl Pts',(31.1115436466863,0.409699470279596,23.6540507545398));
#49630=CARTESIAN_POINT('Ctrl Pts',(31.0507381700391,0.547097840637693,23.6632066094863));
#49631=CARTESIAN_POINT('Ctrl Pts',(30.877053704825,0.797680553802843,23.6827562620821));
#49632=CARTESIAN_POINT('Ctrl Pts',(30.7635871432854,0.906879897536129,23.6935955044951));
#49633=CARTESIAN_POINT('Ctrl Pts',(30.5039119215803,1.07256979004896,23.7154158816792));
#49634=CARTESIAN_POINT('Ctrl Pts',(30.3609720672946,1.12873587571,23.726184783255));
#49635=CARTESIAN_POINT('Ctrl Pts',(30.0630485009405,1.18318311722529,23.7464099346189));
#49636=CARTESIAN_POINT('Ctrl Pts',(29.9110260227659,1.18151676553675,23.755241166967));
#49637=CARTESIAN_POINT('Ctrl Pts',(29.6103298881048,1.1197202582759,23.7758971342361));
#49638=CARTESIAN_POINT('Ctrl Pts',(29.46506200542,1.05803905975613,23.7870045259814));
#49639=CARTESIAN_POINT('Ctrl Pts',(29.2120537724961,0.884838382027716,23.8086817842968));
#49640=CARTESIAN_POINT('Ctrl Pts',(29.1053977198379,0.776856295866943,23.8190596528721));
#49641=CARTESIAN_POINT('Ctrl Pts',(28.9357911246459,0.52231447495466,23.8384992581206));
#49642=CARTESIAN_POINT('Ctrl Pts',(28.8760978227722,0.377122301892393,23.8482592101808));
#49643=CARTESIAN_POINT('Ctrl Pts',(28.816919249242,0.0729797847098555,23.8698251878126));
#49644=CARTESIAN_POINT('Ctrl Pts',(28.8175683805337,-0.0828368336059415,
23.8808737506258));
#49645=CARTESIAN_POINT('Ctrl Pts',(28.8779787013698,-0.380073435953635,
23.9019500472809));
#49646=CARTESIAN_POINT('Ctrl Pts',(28.9351273214881,-0.519045422805617,
23.9113440791565));
#49647=CARTESIAN_POINT('Ctrl Pts',(29.1020830634255,-0.774116322451291,
23.9306396594913));
#49648=CARTESIAN_POINT('Ctrl Pts',(29.212592687875,-0.88627172070161,23.9414021264554));
#49649=CARTESIAN_POINT('Ctrl Pts',(29.4680719424329,-1.05901132730886,23.963214777767));
#49650=CARTESIAN_POINT('Ctrl Pts',(29.609865400996,-1.11904322621712,23.9740503393744));
#49651=CARTESIAN_POINT('Ctrl Pts',(29.8385706131875,-1.1669231022752,23.9897921149766));
#49652=CARTESIAN_POINT('Ctrl Pts',(29.9192597310019,-1.17524047358085,23.9950419278981));
#49653=CARTESIAN_POINT('Ctrl Pts',(30.,-1.17524047358085,24.));
#49654=CARTESIAN_POINT('Origin',(30.,-1.21864324187371E-14,15.78125));
#49655=CARTESIAN_POINT('',(29.9999999962159,-1.17524047358085,24.5624999995353));
#49656=CARTESIAN_POINT('',(30.0000000000002,-1.17524047358085,24.5));
#49657=CARTESIAN_POINT('',(30.,-1.17524047358085,15.78125));
#49658=CARTESIAN_POINT('Ctrl Pts',(29.9999999924319,-1.17524047358085,24.5624999995353));
#49659=CARTESIAN_POINT('Ctrl Pts',(29.8449382921852,-1.17524047258231,24.5529780211908));
#49660=CARTESIAN_POINT('Ctrl Pts',(29.6912874372683,-1.14455036315003,24.5424546005433));
#49661=CARTESIAN_POINT('Ctrl Pts',(29.4063853758944,-1.0258343762565,24.5207505023134));
#49662=CARTESIAN_POINT('Ctrl Pts',(29.2777080162496,-0.939688490130196,
24.5097945313951));
#49663=CARTESIAN_POINT('Ctrl Pts',(29.0636971062813,-0.72579687417109,24.4890693621447));
#49664=CARTESIAN_POINT('Ctrl Pts',(28.9792543776096,-0.601260808557374,
24.4801338851547));
#49665=CARTESIAN_POINT('Ctrl Pts',(28.8587167668904,-0.3209315497576,24.4602564455228));
#49666=CARTESIAN_POINT('Ctrl Pts',(28.8262532459446,-0.166807893138082,
24.449327926347));
#49667=CARTESIAN_POINT('Ctrl Pts',(28.823406512149,0.140728845641508,24.4275212730356));
#49668=CARTESIAN_POINT('Ctrl Pts',(28.851353518733,0.291209583843224,24.4168510640028));
#49669=CARTESIAN_POINT('Ctrl Pts',(28.9629467293987,0.573358103335639,24.3968446251906));
#49670=CARTESIAN_POINT('Ctrl Pts',(29.0455390967654,0.702301510494977,24.3878786774254));
#49671=CARTESIAN_POINT('Ctrl Pts',(29.2579957317181,0.924591935160839,24.3669511834331));
#49672=CARTESIAN_POINT('Ctrl Pts',(29.3868926291043,1.01465868024229,24.3558427221105));
#49673=CARTESIAN_POINT('Ctrl Pts',(29.6668973327643,1.13696430638437,24.3343120930999));
#49674=CARTESIAN_POINT('Ctrl Pts',(29.8144674232288,1.17014774293813,24.3240736802882));
#49675=CARTESIAN_POINT('Ctrl Pts',(30.1216534355145,1.17947691079308,24.3048793479835));
#49676=CARTESIAN_POINT('Ctrl Pts',(30.2784124097871,1.15260328295164,24.2946007685524));
#49677=CARTESIAN_POINT('Ctrl Pts',(30.5685961343608,1.03996407129779,24.2727877800628));
#49678=CARTESIAN_POINT('Ctrl Pts',(30.6996254486415,0.956741717213513,24.2617910312175));
#49679=CARTESIAN_POINT('Ctrl Pts',(30.9187688591,0.747835373953449,24.2409274335984));
#49680=CARTESIAN_POINT('Ctrl Pts',(31.006053860002,0.625488945893405,24.2318518411732));
#49681=CARTESIAN_POINT('Ctrl Pts',(31.1332209274868,0.348324830571042,24.2121988338701));
#49682=CARTESIAN_POINT('Ctrl Pts',(31.1693830920172,0.195045950853365,24.2013302156905));
#49683=CARTESIAN_POINT('Ctrl Pts',(31.1796570639592,-0.112665031805443,
24.1795112071857));
#49684=CARTESIAN_POINT('Ctrl Pts',(31.1552218060231,-0.264121048947789,
24.1687718435869));
#49685=CARTESIAN_POINT('Ctrl Pts',(31.0503552824464,-0.548400595365726,
24.1486142990383));
#49686=CARTESIAN_POINT('Ctrl Pts',(30.9713114905908,-0.678634752411996,
24.1397525078141));
#49687=CARTESIAN_POINT('Ctrl Pts',(30.7647686763693,-0.905919595273436,
24.119011097007));
#49688=CARTESIAN_POINT('Ctrl Pts',(30.6378140048735,-0.999372205084128,
24.1079018617007));
#49689=CARTESIAN_POINT('Ctrl Pts',(30.3601860918747,-1.12872343710904,24.0862673928177));
#49690=CARTESIAN_POINT('Ctrl Pts',(30.2130976252741,-1.16548763290266,24.0759316041108));
#49691=CARTESIAN_POINT('Ctrl Pts',(30.042024216247,-1.17467745886824,24.065100570339));
#49692=CARTESIAN_POINT('Ctrl Pts',(30.021003006896,-1.17524047358085,24.0637897457965));
#49693=CARTESIAN_POINT('Ctrl Pts',(30.0000000000002,-1.17524047358085,24.0625));
#49694=CARTESIAN_POINT('Ctrl Pts',(30.,-1.17524047358085,24.));
#49695=CARTESIAN_POINT('Ctrl Pts',(30.068631292987,-1.17524047358085,24.0042144880528));
#49696=CARTESIAN_POINT('Ctrl Pts',(30.1372731197099,-1.16923029330172,24.0086427063088));
#49697=CARTESIAN_POINT('Ctrl Pts',(30.3594639555913,-1.12983827430394,24.0236835229636));
#49698=CARTESIAN_POINT('Ctrl Pts',(30.5067279557135,-1.07189657495913,24.034780912417));
#49699=CARTESIAN_POINT('Ctrl Pts',(30.7648494491756,-0.904940985120749,
24.0565507524641));
#49700=CARTESIAN_POINT('Ctrl Pts',(30.8745226735525,-0.799463570900332,
24.0670250985558));
#49701=CARTESIAN_POINT('Ctrl Pts',(31.0499651911362,-0.550024618872908,
24.0866421584515));
#49702=CARTESIAN_POINT('Ctrl Pts',(31.1129833274185,-0.407722194144101,
24.0960894491163));
#49703=CARTESIAN_POINT('Ctrl Pts',(31.1806136864057,-0.106256135243321,
24.117465645852));
#49704=CARTESIAN_POINT('Ctrl Pts',(31.1843316043204,0.0499559746584703,
24.1285422519746));
#49705=CARTESIAN_POINT('Ctrl Pts',(31.131994520367,0.349324836152535,24.1497697417397));
#49706=CARTESIAN_POINT('Ctrl Pts',(31.0785837311869,0.489956671487056,24.1594708103671));
#49707=CARTESIAN_POINT('Ctrl Pts',(30.9185303965388,0.749536525439823,24.1785023892068));
#49708=CARTESIAN_POINT('Ctrl Pts',(30.8111165172128,0.864620133839068,24.1891785696567));
#49709=CARTESIAN_POINT('Ctrl Pts',(30.5601137220937,1.04443640550787,24.2109672262292));
#49710=CARTESIAN_POINT('Ctrl Pts',(30.4195953268947,1.10838743812269,24.2218634370972));
#49711=CARTESIAN_POINT('Ctrl Pts',(30.125226440525,1.17808176086598,24.2424108698401));
#49712=CARTESIAN_POINT('Ctrl Pts',(29.9745000794406,1.18444262103543,24.2512396402881));
#49713=CARTESIAN_POINT('Ctrl Pts',(29.671168206001,1.13918974904968,24.2714709284502));
#49714=CARTESIAN_POINT('Ctrl Pts',(29.5219912146071,1.08506931535676,24.2825503121002));
#49715=CARTESIAN_POINT('Ctrl Pts',(29.2588817407465,0.924538989806815,24.3043986527903));
#49716=CARTESIAN_POINT('Ctrl Pts',(29.1462343920073,0.821663056130735,24.3149634007337));
#49717=CARTESIAN_POINT('Ctrl Pts',(28.9649893539032,0.577368135519195,24.3347544047798));
#49718=CARTESIAN_POINT('Ctrl Pts',(28.8986993951907,0.437889260784583,24.3439503786226));
#49719=CARTESIAN_POINT('Ctrl Pts',(28.8227562109677,0.139172903579825,24.3651316009568));
#49720=CARTESIAN_POINT('Ctrl Pts',(28.814686650905,-0.0173128945475468,
24.3762276136201));
#49721=CARTESIAN_POINT('Ctrl Pts',(28.8589720780878,-0.318736522506238,
24.3976008016849));
#49722=CARTESIAN_POINT('Ctrl Pts',(28.9087096405855,-0.46104932706788,24.4076656524993));
#49723=CARTESIAN_POINT('Ctrl Pts',(29.0619693077579,-0.724977765539007,
24.4264342215945));
#49724=CARTESIAN_POINT('Ctrl Pts',(29.1662794308695,-0.84283884374432,24.4370182792792));
#49725=CARTESIAN_POINT('Ctrl Pts',(29.4127142037999,-1.0294613008905,24.4587677289451));
#49726=CARTESIAN_POINT('Ctrl Pts',(29.5518825792064,-1.09722011413893,24.4697160382912));
#49727=CARTESIAN_POINT('Ctrl Pts',(29.7982117366005,-1.1622217216024,24.4871470887339));
#49728=CARTESIAN_POINT('Ctrl Pts',(29.8989795683345,-1.17524047358088,24.4937965702842));
#49729=CARTESIAN_POINT('Ctrl Pts',(30.0000000000003,-1.17524047358085,24.5));
#49730=CARTESIAN_POINT('Origin',(30.,-1.21864324187371E-14,15.78125));
#49731=CARTESIAN_POINT('',(29.9999999999999,-1.17524047358085,25.0625));
#49732=CARTESIAN_POINT('',(30.0000000000002,-1.17524047358085,25.));
#49733=CARTESIAN_POINT('',(30.,-1.17524047358085,15.78125));
#49734=CARTESIAN_POINT('Ctrl Pts',(29.9999999999998,-1.17524047358085,25.0625));
#49735=CARTESIAN_POINT('Ctrl Pts',(29.9787160795735,-1.17524047358085,25.0611930039571));
#49736=CARTESIAN_POINT('Ctrl Pts',(29.9574135577721,-1.17466229796152,25.0598643671606));
#49737=CARTESIAN_POINT('Ctrl Pts',(29.7860545064693,-1.16533366685381,25.0490108716001));
#49738=CARTESIAN_POINT('Ctrl Pts',(29.638982260427,-1.12845915516134,25.0386721678491));
#49739=CARTESIAN_POINT('Ctrl Pts',(29.3614303849904,-0.998891400573746,
25.0170346917219));
#49740=CARTESIAN_POINT('Ctrl Pts',(29.2345369639167,-0.905335034780717,
25.0059255391243));
#49741=CARTESIAN_POINT('Ctrl Pts',(29.0281770961676,-0.677897334966365,
24.9851899432843));
#49742=CARTESIAN_POINT('Ctrl Pts',(28.9492422426318,-0.547623084588669,
24.9763305695037));
#49743=CARTESIAN_POINT('Ctrl Pts',(28.8429395559285,-0.25880932586385,24.9558515154165));
#49744=CARTESIAN_POINT('Ctrl Pts',(28.8187785161156,-0.102338490894112,
24.9447565638831));
#49745=CARTESIAN_POINT('Ctrl Pts',(28.8329707062525,0.20487723468326,24.9229726728069));
#49746=CARTESIAN_POINT('Ctrl Pts',(28.8688620223111,0.352813948215486,24.9124828541373));
#49747=CARTESIAN_POINT('Ctrl Pts',(28.9959383633127,0.629882762331914,24.8928366044019));
#49748=CARTESIAN_POINT('Ctrl Pts',(29.0869818629053,0.755846556300386,24.8834354015886));
#49749=CARTESIAN_POINT('Ctrl Pts',(29.3131553782924,0.966129203680405,24.8620913064548));
#49750=CARTESIAN_POINT('Ctrl Pts',(29.4462640631474,1.04811028996687,24.8510108758816));
#49751=CARTESIAN_POINT('Ctrl Pts',(29.731323759893,1.1538048728599,24.8297587550632));
#49752=CARTESIAN_POINT('Ctrl Pts',(29.8797531248391,1.17853792828451,24.8200009879783));
#49753=CARTESIAN_POINT('Ctrl Pts',(30.1846496308258,1.17107054148177,24.8010132560253));
#49754=CARTESIAN_POINT('Ctrl Pts',(30.3381730792388,1.13627251448872,24.7903520180859));
#49755=CARTESIAN_POINT('Ctrl Pts',(30.6200199170605,1.01003478142549,24.7685688600169));
#49756=CARTESIAN_POINT('Ctrl Pts',(30.7461080027782,0.920828764814659,24.7576633973259));
#49757=CARTESIAN_POINT('Ctrl Pts',(30.954589658464,0.701638656166971,24.7370899153526));
#49758=CARTESIAN_POINT('Ctrl Pts',(31.0359799147447,0.574699574292555,24.7282504951265));
#49759=CARTESIAN_POINT('Ctrl Pts',(31.1497275829798,0.289883112537678,24.7080548792676));
#49760=CARTESIAN_POINT('Ctrl Pts',(31.1781418190148,0.133683865658838,24.6969791852295));
#49761=CARTESIAN_POINT('Ctrl Pts',(31.1719905418774,-0.174601531099527,
24.6751194464719));
#49762=CARTESIAN_POINT('Ctrl Pts',(31.1398342436188,-0.323793762033814,
24.6645406022347));
#49763=CARTESIAN_POINT('Ctrl Pts',(31.020088030022,-0.603297917753395,24.644721668578));
#49764=CARTESIAN_POINT('Ctrl Pts',(30.9330960022514,-0.730676428588708,
24.6355607116713));
#49765=CARTESIAN_POINT('Ctrl Pts',(30.7134327937131,-0.946735070008641,
24.6144116187632));
#49766=CARTESIAN_POINT('Ctrl Pts',(30.5822707418913,-1.03259356059966,24.6033132579239));
#49767=CARTESIAN_POINT('Ctrl Pts',(30.299587098649,-1.14619538675731,24.5819267037008));
#49768=CARTESIAN_POINT('Ctrl Pts',(30.1515439291036,-1.17497884081411,24.5718152360255));
#49769=CARTESIAN_POINT('Ctrl Pts',(30.0013618111703,-1.17523988185447,24.5625836466351));
#49770=CARTESIAN_POINT('Ctrl Pts',(30.0006808894801,-1.17524047358524,24.5625418118389));
#49771=CARTESIAN_POINT('Ctrl Pts',(29.9999999924319,-1.17524047358085,24.5624999995353));
#49772=CARTESIAN_POINT('Ctrl Pts',(30.0000000000003,-1.17524047358085,24.5));
#49773=CARTESIAN_POINT('Ctrl Pts',(30.0475989786694,-1.17524047358084,24.5029229425557));
#49774=CARTESIAN_POINT('Ctrl Pts',(30.0952413712801,-1.17234913261358,24.5059510599029));
#49775=CARTESIAN_POINT('Ctrl Pts',(30.2990650070911,-1.14742109537484,24.5193511873216));
#49776=CARTESIAN_POINT('Ctrl Pts',(30.4499960157575,-1.0970416910395,24.5304056476212));
#49777=CARTESIAN_POINT('Ctrl Pts',(30.7177665488108,-0.942842462676014,
24.5523157520592));
#49778=CARTESIAN_POINT('Ctrl Pts',(30.833223349596,-0.842552715174129,24.5629613319529));
#49779=CARTESIAN_POINT('Ctrl Pts',(31.0200068112404,-0.603233885310555,
24.5829160166926));
#49780=CARTESIAN_POINT('Ctrl Pts',(31.0893943876237,-0.466400998056969,
24.591928683353));
#49781=CARTESIAN_POINT('Ctrl Pts',(31.1731872619397,-0.170385863873932,
24.612918368786));
#49782=CARTESIAN_POINT('Ctrl Pts',(31.185412882504,-0.0137497619841131,
24.6240250391094));
#49783=CARTESIAN_POINT('Ctrl Pts',(31.1488612218191,0.289356743431089,24.6455175557638));
#49784=CARTESIAN_POINT('Ctrl Pts',(31.1026857517696,0.433263084173784,24.6557215908795));
#49785=CARTESIAN_POINT('Ctrl Pts',(30.9558437041525,0.701308793163264,24.6747280350226));
#49786=CARTESIAN_POINT('Ctrl Pts',(30.8545058913013,0.821789237632239,24.6849956137961));
#49787=CARTESIAN_POINT('Ctrl Pts',(30.6123622815668,1.01480099766359,24.7067080777764));
#49788=CARTESIAN_POINT('Ctrl Pts',(30.4745499588497,1.08610079838188,24.7176986563197));
#49789=CARTESIAN_POINT('Ctrl Pts',(30.1837738406509,1.17031056558872,24.7385400922772));
#49790=CARTESIAN_POINT('Ctrl Pts',(30.0341022035471,1.18415559329136,24.7475897886987));
#49791=CARTESIAN_POINT('Ctrl Pts',(29.7305751526436,1.15452627151871,24.7672791490145));
#49792=CARTESIAN_POINT('Ctrl Pts',(29.5799242663497,1.10861951554252,24.7781578355522));
#49793=CARTESIAN_POINT('Ctrl Pts',(29.3089128663366,0.962634653740643,24.7999757240996));
#49794=CARTESIAN_POINT('Ctrl Pts',(29.1903801371545,0.865330006275208,24.8107043566494));
#49795=CARTESIAN_POINT('Ctrl Pts',(28.9974547059893,0.631606479932577,24.8308378310304));
#49796=CARTESIAN_POINT('Ctrl Pts',(28.9246531642855,0.497649505166107,24.8397129306474));
#49797=CARTESIAN_POINT('Ctrl Pts',(28.8322520407485,0.204711362593916,24.8604844343777));
#49798=CARTESIAN_POINT('Ctrl Pts',(28.8154219514347,0.0480344797090969,
24.8715939963785));
#49799=CARTESIAN_POINT('Ctrl Pts',(28.8433837526351,-0.256851307347509,
24.8932126773996));
#49800=CARTESIAN_POINT('Ctrl Pts',(28.8856263759144,-0.402401296034548,
24.9035332594392));
#49801=CARTESIAN_POINT('Ctrl Pts',(29.0254132564532,-0.675115053553108,
24.9228707031121));
#49802=CARTESIAN_POINT('Ctrl Pts',(29.1237053106631,-0.798585223889617,
24.932834945393));
#49803=CARTESIAN_POINT('Ctrl Pts',(29.3612206915393,-0.998444700238917,
24.9545059777387));
#49804=CARTESIAN_POINT('Ctrl Pts',(29.4974844913312,-1.07350395274647,24.9655347517064));
#49805=CARTESIAN_POINT('Ctrl Pts',(29.7595519260122,-1.15671325178265,24.9845777838555));
#49806=CARTESIAN_POINT('Ctrl Pts',(29.8794906495254,-1.17524047358089,24.9925998011151));
#49807=CARTESIAN_POINT('Ctrl Pts',(30.0000000000004,-1.17524047358085,25.));
#49808=CARTESIAN_POINT('Origin',(30.,-1.21864324187371E-14,15.78125));
#49809=CARTESIAN_POINT('',(29.9999999999997,-1.17524047358085,25.5625));
#49810=CARTESIAN_POINT('',(30.,-1.17524047358085,25.5));
#49811=CARTESIAN_POINT('',(30.,-1.17524047358085,15.78125));
#49812=CARTESIAN_POINT('Ctrl Pts',(29.9999999999995,-1.17524047358085,25.5625));
#49813=CARTESIAN_POINT('Ctrl Pts',(29.9590631434842,-1.17524047358085,25.5599861628683));
#49814=CARTESIAN_POINT('Ctrl Pts',(29.9180826982373,-1.17310176284205,25.557393823766));
#49815=CARTESIAN_POINT('Ctrl Pts',(29.7270170759755,-1.15303120939534,25.5449493522346));
#49816=CARTESIAN_POINT('Ctrl Pts',(29.5812843667667,-1.10844931412058,25.534419650774));
#49817=CARTESIAN_POINT('Ctrl Pts',(29.3094646041477,-0.963834030512161,
25.5126006792245));
#49818=CARTESIAN_POINT('Ctrl Pts',(29.1870616253517,-0.863111358786919,
25.5015132019157));
#49819=CARTESIAN_POINT('Ctrl Pts',(28.9936035835609,-0.625120486304078,
25.4811957277874));
#49820=CARTESIAN_POINT('Ctrl Pts',(28.922245153506,-0.491992360156719,25.4723859354899));
#49821=CARTESIAN_POINT('Ctrl Pts',(28.8324037582581,-0.203110856662721,
25.4519020777895));
#49822=CARTESIAN_POINT('Ctrl Pts',(28.8159185655927,-0.0497708721110285,
25.4410291268206));
#49823=CARTESIAN_POINT('Ctrl Pts',(28.8428111724951,0.257674311776114,25.4192289654353));
#49824=CARTESIAN_POINT('Ctrl Pts',(28.8871477746036,0.408737403201897,25.4085174632064));
#49825=CARTESIAN_POINT('Ctrl Pts',(29.028998912458,0.678628541452795,25.389380164336));
#49826=CARTESIAN_POINT('Ctrl Pts',(29.1227608288482,0.796156039557689,25.3798091767006));
#49827=CARTESIAN_POINT('Ctrl Pts',(29.3535044180399,0.99354320653279,25.3586416369362));
#49828=CARTESIAN_POINT('Ctrl Pts',(29.4896480206548,1.06987223772086,25.3475752255981));
#49829=CARTESIAN_POINT('Ctrl Pts',(29.7837920452496,1.16549604577304,25.326122303941));
#49830=CARTESIAN_POINT('Ctrl Pts',(29.9388720345248,1.18379547475176,25.3165570329261));
#49831=CARTESIAN_POINT('Ctrl Pts',(30.243221825482,1.15962478745302,25.2970106790485));
#49832=CARTESIAN_POINT('Ctrl Pts',(30.3896819125524,1.11893466510606,25.2865742888993));
#49833=CARTESIAN_POINT('Ctrl Pts',(30.664499787972,0.981897695245122,25.2648398897594));
#49834=CARTESIAN_POINT('Ctrl Pts',(30.7892223684277,0.884773136061606,25.2537375376443));
#49835=CARTESIAN_POINT('Ctrl Pts',(30.9892253393634,0.652081932327525,25.233206047704));
#49836=CARTESIAN_POINT('Ctrl Pts',(31.0644029101032,0.520407945827758,25.2244008128923));
#49837=CARTESIAN_POINT('Ctrl Pts',(31.1617865735135,0.233810524226684,25.2040789136694));
#49838=CARTESIAN_POINT('Ctrl Pts',(31.1822791704619,0.0813648687854731,
25.1932693773186));
#49839=CARTESIAN_POINT('Ctrl Pts',(31.1637300195375,-0.226326940808914,
25.1714517283273));
#49840=CARTESIAN_POINT('Ctrl Pts',(31.1234798971667,-0.378558584977568,
25.1606573669753));
#49841=CARTESIAN_POINT('Ctrl Pts',(30.9889788141031,-0.652134792227603,
25.1412587691706));
#49842=CARTESIAN_POINT('Ctrl Pts',(30.8984922205339,-0.772069973056249,
25.1319682180917));
#49843=CARTESIAN_POINT('Ctrl Pts',(30.6735951228457,-0.975307798919531,
25.1109522700489));
#49844=CARTESIAN_POINT('Ctrl Pts',(30.5399926661631,-1.05515984400593,25.0999170005632));
#49845=CARTESIAN_POINT('Ctrl Pts',(30.2678908596704,-1.15220558793873,25.0797672273045));
#49846=CARTESIAN_POINT('Ctrl Pts',(30.1343655548317,-1.17524047358085,25.0707510761622));
#49847=CARTESIAN_POINT('Ctrl Pts',(29.9999999999998,-1.17524047358085,25.0625));
#49848=CARTESIAN_POINT('Ctrl Pts',(30.0000000000004,-1.17524047358085,25.));
#49849=CARTESIAN_POINT('Ctrl Pts',(30.0280011909949,-1.17524047358084,25.0017194880028));
#49850=CARTESIAN_POINT('Ctrl Pts',(30.056028863347,-1.17423978093536,25.0034760804581));
#49851=CARTESIAN_POINT('Ctrl Pts',(30.2395952618035,-1.16108096396762,25.0152149952129));
#49852=CARTESIAN_POINT('Ctrl Pts',(30.3913571022497,-1.11907669842983,25.0260235449911));
#49853=CARTESIAN_POINT('Ctrl Pts',(30.6663605367685,-0.979972388704826,
25.0478426338075));
#49854=CARTESIAN_POINT('Ctrl Pts',(30.7876235644496,-0.885461952247295,
25.0586398624147));
#49855=CARTESIAN_POINT('Ctrl Pts',(30.9860830879355,-0.656850945315206,
25.0789319146131));
#49856=CARTESIAN_POINT('Ctrl Pts',(31.0619486284351,-0.525431380274417,
25.0877429880603));
#49857=CARTESIAN_POINT('Ctrl Pts',(31.162019301378,-0.235334014571736,25.1083130594786));
#49858=CARTESIAN_POINT('Ctrl Pts',(31.182987818821,-0.0787326337506094,
25.1194172678187));
#49859=CARTESIAN_POINT('Ctrl Pts',(31.162785126869,0.227544173273347,25.1411345825519));
#49860=CARTESIAN_POINT('Ctrl Pts',(31.1241144207896,0.374476178584838,25.1515531598995));
#49861=CARTESIAN_POINT('Ctrl Pts',(30.9915168317796,0.649674032406111,25.1710667445663));
#49862=CARTESIAN_POINT('Ctrl Pts',(30.8973599492461,0.774562668596496,25.1806896874262));
#49863=CARTESIAN_POINT('Ctrl Pts',(30.6662666830193,0.980382528688255,25.202177670528));
#49864=CARTESIAN_POINT('Ctrl Pts',(30.531751815152,1.05938687434591,25.2132389149495));
#49865=CARTESIAN_POINT('Ctrl Pts',(30.2450331875533,1.15903498558282,25.2343785368368));
#49866=CARTESIAN_POINT('Ctrl Pts',(30.0962908441082,1.18072042198942,25.2438927186044));
#49867=CARTESIAN_POINT('Ctrl Pts',(29.7917163095273,1.16710140491111,25.2630787773242));
#49868=CARTESIAN_POINT('Ctrl Pts',(29.638905788045,1.12920096781154,25.2738062281113));
#49869=CARTESIAN_POINT('Ctrl Pts',(29.3599222216531,0.997398530499289,25.2956108489033));
#49870=CARTESIAN_POINT('Ctrl Pts',(29.2358774116296,0.905886016991888,25.3064726127214));
#49871=CARTESIAN_POINT('Ctrl Pts',(29.0316806530828,0.682639701770527,25.32692677681));
#49872=CARTESIAN_POINT('Ctrl Pts',(28.9526524211366,0.553805209269406,25.3357310715183));
#49873=CARTESIAN_POINT('Ctrl Pts',(28.844720062577,0.266708452558536,25.3560883773325));
#49874=CARTESIAN_POINT('Ctrl Pts',(28.8194808141697,0.110295910906438,25.3671791955642));
#49875=CARTESIAN_POINT('Ctrl Pts',(28.8316382042729,-0.197210560241239,
25.3889837026743));
#49876=CARTESIAN_POINT('Ctrl Pts',(28.8665861506279,-0.345474523822663,
25.3994967258182));
#49877=CARTESIAN_POINT('Ctrl Pts',(28.9918018301732,-0.623166741842213,
25.4191871795497));
#49878=CARTESIAN_POINT('Ctrl Pts',(29.081808144475,-0.749490769071139,25.4285215559887));
#49879=CARTESIAN_POINT('Ctrl Pts',(29.3063266217772,-0.961255466999539,
25.449816563314));
#49880=CARTESIAN_POINT('Ctrl Pts',(29.438949602445,-1.04422897408056,25.4609023529488));
#49881=CARTESIAN_POINT('Ctrl Pts',(29.7169259241077,-1.14948331999011,25.4817038921344));
#49882=CARTESIAN_POINT('Ctrl Pts',(29.8579333178884,-1.17524047358086,25.4912760155257));
#49883=CARTESIAN_POINT('Ctrl Pts',(30.,-1.17524047358085,25.5));
#49884=CARTESIAN_POINT('Origin',(30.,-1.21864324187371E-14,15.78125));
#49885=CARTESIAN_POINT('',(30.,-1.17524047358085,26.0625));
#49886=CARTESIAN_POINT('',(30.,-1.17524047358085,26.));
#49887=CARTESIAN_POINT('',(30.,-1.17524047358085,15.78125));
#49888=CARTESIAN_POINT('Ctrl Pts',(29.9999999999999,-1.17524047358085,26.0625));
#49889=CARTESIAN_POINT('Ctrl Pts',(29.9384679078155,-1.17524047358085,26.0587214573544));
#49890=CARTESIAN_POINT('Ctrl Pts',(29.8769029052424,-1.17040913172972,26.054769604635));
#49891=CARTESIAN_POINT('Ctrl Pts',(29.6659154234359,-1.13693724882076,26.0406266508408));
#49892=CARTESIAN_POINT('Ctrl Pts',(29.5220177711255,-1.084323597792,26.0299248801994));
#49893=CARTESIAN_POINT('Ctrl Pts',(29.2586759114222,-0.925171378535031,
26.0081111282534));
#49894=CARTESIAN_POINT('Ctrl Pts',(29.1425757110306,-0.818746672431791,
25.9972085314777));
#49895=CARTESIAN_POINT('Ctrl Pts',(28.9627703960609,-0.572330389052239,
25.9774307272425));
#49896=CARTESIAN_POINT('Ctrl Pts',(28.8986210699436,-0.436327710221708,
25.9684388957715));
#49897=CARTESIAN_POINT('Ctrl Pts',(28.8234492804003,-0.143169608738148,
25.9476517953103));
#49898=CARTESIAN_POINT('Ctrl Pts',(28.8148292891501,0.0116076754049962,
25.936676929058));
#49899=CARTESIAN_POINT('Ctrl Pts',(28.8579269079672,0.318093458602922,25.9149447963521));
#49900=CARTESIAN_POINT('Ctrl Pts',(28.910158206845,0.466589649123026,25.9045489692953));
#49901=CARTESIAN_POINT('Ctrl Pts',(29.0662354765119,0.729159361472922,25.8856555497038));
#49902=CARTESIAN_POINT('Ctrl Pts',(29.1665620010353,0.841989757161643,25.8754944720367));
#49903=CARTESIAN_POINT('Ctrl Pts',(29.4086828051808,1.02746666351878,25.8540505472151));
#49904=CARTESIAN_POINT('Ctrl Pts',(29.5495956219979,1.09657907822105,25.84294712555));
#49905=CARTESIAN_POINT('Ctrl Pts',(29.8472420936479,1.17519666348882,25.8218820609165));
#49906=CARTESIAN_POINT('Ctrl Pts',(30.000722767755,1.18508027808238,25.8128044743545));
#49907=CARTESIAN_POINT('Ctrl Pts',(30.3019786609575,1.14582802588677,25.7929134117055));
#49908=CARTESIAN_POINT('Ctrl Pts',(30.4468987068161,1.09744171612032,25.7822987333));
#49909=CARTESIAN_POINT('Ctrl Pts',(30.7155809567247,0.94545759821414,25.7604111763944));
#49910=CARTESIAN_POINT('Ctrl Pts',(30.835612326607,0.841258259962285,25.7493460732515));
#49911=CARTESIAN_POINT('Ctrl Pts',(31.0226024258984,0.598138792258194,25.7292439525602));
#49912=CARTESIAN_POINT('Ctrl Pts',(31.0902361983429,0.463547729361891,25.7203689985712));
#49913=CARTESIAN_POINT('Ctrl Pts',(31.1725680326408,0.172449502286477,25.6997279586011));
#49914=CARTESIAN_POINT('Ctrl Pts',(31.1850367066478,0.0183235805600113,
25.6887992788123));
#49915=CARTESIAN_POINT('Ctrl Pts',(31.149849032726,-0.288650006825612,25.6670325571437));
#49916=CARTESIAN_POINT('Ctrl Pts',(31.1014848231134,-0.438439388995189,
25.6564113704209));
#49917=CARTESIAN_POINT('Ctrl Pts',(30.9523589365019,-0.704596833564904,
25.637538818338));
#49918=CARTESIAN_POINT('Ctrl Pts',(30.8552831525205,-0.819746342004528,
25.6276245442916));
#49919=CARTESIAN_POINT('Ctrl Pts',(30.6186741800399,-1.01116668038418,25.6063083713552));
#49920=CARTESIAN_POINT('Ctrl Pts',(30.4800603026513,-1.08386414646939,25.5952190187437));
#49921=CARTESIAN_POINT('Ctrl Pts',(30.2235083443405,-1.15925176820215,25.5767919868584));
#49922=CARTESIAN_POINT('Ctrl Pts',(30.1119520742388,-1.17524047358085,25.5693747164571));
#49923=CARTESIAN_POINT('Ctrl Pts',(29.9999999999995,-1.17524047358085,25.5625));
#49924=CARTESIAN_POINT('Ctrl Pts',(30.,-1.17524047358085,25.5));
#49925=CARTESIAN_POINT('Ctrl Pts',(30.0069574643761,-1.17524047358085,25.5004272417029));
#49926=CARTESIAN_POINT('Ctrl Pts',(30.01391720466,-1.17517869098561,25.5008568135879));
#49927=CARTESIAN_POINT('Ctrl Pts',(30.1767683930213,-1.17228514742378,25.5109597131747));
#49928=CARTESIAN_POINT('Ctrl Pts',(30.3305146751184,-1.13852257214804,25.5215979241794));
#49929=CARTESIAN_POINT('Ctrl Pts',(30.613289571589,-1.01415059475931,25.5433719241602));
#49930=CARTESIAN_POINT('Ctrl Pts',(30.7400483172667,-0.925722033283128,
25.5542910068295));
#49931=CARTESIAN_POINT('Ctrl Pts',(30.9499509146168,-0.707886564918499,
25.5749037184647));
#49932=CARTESIAN_POINT('Ctrl Pts',(31.0321249523172,-0.581569550980178,
25.5837623721801));
#49933=CARTESIAN_POINT('Ctrl Pts',(31.1477905785375,-0.297516308572578,
25.6039038700829));
#49934=CARTESIAN_POINT('Ctrl Pts',(31.1772544504942,-0.141401249469257,
25.6149735945785));
#49935=CARTESIAN_POINT('Ctrl Pts',(31.1730934439483,0.167116297568546,25.636849794526));
#49936=CARTESIAN_POINT('Ctrl Pts',(31.1418645520009,0.316603789635784,25.6474495749843));
#49937=CARTESIAN_POINT('Ctrl Pts',(31.0239238826678,0.596699382032703,25.6673104459219));
#49938=CARTESIAN_POINT('Ctrl Pts',(30.9379157361151,0.724424917792123,25.6764216802641));
#49939=CARTESIAN_POINT('Ctrl Pts',(30.7198518445296,0.941880855114492,25.6975221021999));
#49940=CARTESIAN_POINT('Ctrl Pts',(30.5891826263813,1.02868094414498,25.7086235824532));
#49941=CARTESIAN_POINT('Ctrl Pts',(30.3070725150413,1.14422525077315,25.730043785608));
#49942=CARTESIAN_POINT('Ctrl Pts',(30.1591233913896,1.1739884490527,25.7401842137377));
#49943=CARTESIAN_POINT('Ctrl Pts',(29.8537619113516,1.17646530259176,25.7590235656117));
#49944=CARTESIAN_POINT('Ctrl Pts',(29.6991872299891,1.1467452303545,25.7694824753175));
#49945=CARTESIAN_POINT('Ctrl Pts',(29.4128145699134,1.02954198968741,25.7912232470859));
#49946=CARTESIAN_POINT('Ctrl Pts',(29.2835235645903,0.944145175996724,25.8021903431407));
#49947=CARTESIAN_POINT('Ctrl Pts',(29.0681842616351,0.731537563632497,25.8229515631887));
#49948=CARTESIAN_POINT('Ctrl Pts',(28.9830068906091,0.607571894150497,25.8319186117076));
#49949=CARTESIAN_POINT('Ctrl Pts',(28.8607454143127,0.328058458525624,25.851738203379));
#49950=CARTESIAN_POINT('Ctrl Pts',(28.8273201029076,0.174145192049772,25.8626518043211));
#49951=CARTESIAN_POINT('Ctrl Pts',(28.8225473943512,-0.133454152009573,
25.8844628968148));
#49952=CARTESIAN_POINT('Ctrl Pts',(28.849586199068,-0.284195707441678,25.8951515997385));
#49953=CARTESIAN_POINT('Ctrl Pts',(28.9594336647467,-0.566901683792667,
25.9151975664084));
#49954=CARTESIAN_POINT('Ctrl Pts',(29.0410981500453,-0.696179869303813,
25.9241315793102));
#49955=CARTESIAN_POINT('Ctrl Pts',(29.2520170527073,-0.919779045076863,
25.9450110448572));
#49956=CARTESIAN_POINT('Ctrl Pts',(29.3804160320669,-1.01073211613404,25.95612035376));
#49957=CARTESIAN_POINT('Ctrl Pts',(29.6598179734432,-1.13487834137248,25.9776792246572));
#49958=CARTESIAN_POINT('Ctrl Pts',(29.8072708469184,-1.1689955596726,25.9879435454987));
#49959=CARTESIAN_POINT('Ctrl Pts',(29.9714632607541,-1.17498080122199,25.9982384188692));
#49960=CARTESIAN_POINT('Ctrl Pts',(29.9857363066776,-1.17524047358085,25.9991240997731));
#49961=CARTESIAN_POINT('Ctrl Pts',(29.9999999999999,-1.17524047358085,26.));
#49962=CARTESIAN_POINT('Origin',(30.,-1.21864324187371E-14,15.78125));
#49963=CARTESIAN_POINT('',(30.,-1.17524047358085,26.5625));
#49964=CARTESIAN_POINT('',(29.9999999999997,-1.17524047358085,26.4999999999999));
#49965=CARTESIAN_POINT('',(30.,-1.17524047358085,15.78125));
#49966=CARTESIAN_POINT('Ctrl Pts',(30.,-1.17524047358085,26.5625));
#49967=CARTESIAN_POINT('Ctrl Pts',(29.9189538385986,-1.17524047358085,26.5575231437572));
#49968=CARTESIAN_POINT('Ctrl Pts',(29.8379609361797,-1.16685998242801,26.5522524382954));
#49969=CARTESIAN_POINT('Ctrl Pts',(29.6089811727034,-1.1187361642345,26.5364851544771));
#49970=CARTESIAN_POINT('Ctrl Pts',(29.4672242547403,-1.05858684051961,26.5256476735947));
#49971=CARTESIAN_POINT('Ctrl Pts',(29.2118758464994,-0.885634166979752,
26.5038355032321));
#49972=CARTESIAN_POINT('Ctrl Pts',(29.1014575353795,-0.773390023233997,
26.4930754972477));
#49973=CARTESIAN_POINT('Ctrl Pts',(28.9347073730369,-0.518183463481665,
26.4737877314199));
#49974=CARTESIAN_POINT('Ctrl Pts',(28.8776702380248,-0.379162720284378,
26.4643854707334));
#49975=CARTESIAN_POINT('Ctrl Pts',(28.8174988609875,-0.0818619971934983,
26.4433046274383));
#49976=CARTESIAN_POINT('Ctrl Pts',(28.8169789681977,0.0739680819649894,
26.4322551101507));
#49977=CARTESIAN_POINT('Ctrl Pts',(28.8764093680924,0.378032609649621,26.4106946625572));
#49978=CARTESIAN_POINT('Ctrl Pts',(28.9362017786302,0.523138441896699,26.4009448281074));
#49979=CARTESIAN_POINT('Ctrl Pts',(29.1059813583505,0.777530022962841,26.3814999268455));
#49980=CARTESIAN_POINT('Ctrl Pts',(29.2127271628307,0.885439479708375,26.3711191218038));
#49981=CARTESIAN_POINT('Ctrl Pts',(29.4658882417733,1.05845819806925,26.3494389287095));
#49982=CARTESIAN_POINT('Ctrl Pts',(29.6112162771377,1.12003007041528,26.3383317191495));
#49983=CARTESIAN_POINT('Ctrl Pts',(29.9119535931961,1.18158358217449,26.3176818381253));
#49984=CARTESIAN_POINT('Ctrl Pts',(30.0639561135899,1.18313176493728,26.308852379607));
#49985=CARTESIAN_POINT('Ctrl Pts',(30.3618294498414,1.12846284091072,26.2886224532834));
#49986=CARTESIAN_POINT('Ctrl Pts',(30.5047372110283,1.07218329091309,26.2778514997354));
#49987=CARTESIAN_POINT('Ctrl Pts',(30.7642923496518,0.906285517829887,26.2560311264309));
#49988=CARTESIAN_POINT('Ctrl Pts',(30.8776734787023,0.796998466194141,26.2451940206555));
#49989=CARTESIAN_POINT('Ctrl Pts',(31.0511614964728,0.546283376197254,26.2256517381869));
#49990=CARTESIAN_POINT('Ctrl Pts',(31.1118599586541,0.408839660981002,26.2164897876345));
#49991=CARTESIAN_POINT('Ctrl Pts',(31.179816298086,0.113659355972694,26.1955592978295));
#49992=CARTESIAN_POINT('Ctrl Pts',(31.1845443559052,-0.0416770721755796,
26.1845447840881));
#49993=CARTESIAN_POINT('Ctrl Pts',(31.1333712501869,-0.348241759846019,
26.1628070564654));
#49994=CARTESIAN_POINT('Ctrl Pts',(31.0768319553006,-0.496185033349922,
26.1527007984472));
#49995=CARTESIAN_POINT('Ctrl Pts',(30.9126965034022,-0.755446668894444,
26.1334298283147));
#49996=CARTESIAN_POINT('Ctrl Pts',(30.8088874743598,-0.865675121928193,
26.1231471467367));
#49997=CARTESIAN_POINT('Ctrl Pts',(30.5607504336079,-1.04453090463544,26.1015685223966));
#49998=CARTESIAN_POINT('Ctrl Pts',(30.4174143875892,-1.10962145980108,26.0904588858133));
#49999=CARTESIAN_POINT('Ctrl Pts',(30.1782678600435,-1.16509155074858,26.0738068318412));
#50000=CARTESIAN_POINT('Ctrl Pts',(30.0891908090061,-1.17524047358085,26.0679770001062));
#50001=CARTESIAN_POINT('Ctrl Pts',(29.9999999999999,-1.17524047358085,26.0625));
#50002=CARTESIAN_POINT('Ctrl Pts',(29.9999999999999,-1.17524047358085,26.));
#50003=CARTESIAN_POINT('Ctrl Pts',(30.1425333221801,-1.17524047358085,26.0087526397553));
#50004=CARTESIAN_POINT('Ctrl Pts',(30.2840219111895,-1.14931710997616,26.0183602049923));
#50005=CARTESIAN_POINT('Ctrl Pts',(30.561367295123,-1.04389937746679,26.0391287924253));
#50006=CARTESIAN_POINT('Ctrl Pts',(30.6930583893841,-0.961526015756511,
26.0501360796874));
#50007=CARTESIAN_POINT('Ctrl Pts',(30.9136669465422,-0.754054974126117,
26.0710387617507));
#50008=CARTESIAN_POINT('Ctrl Pts',(31.0017654739708,-0.632326756940585,
26.0801633069178));
#50009=CARTESIAN_POINT('Ctrl Pts',(31.130809796733,-0.356072448301099,26.0997518021271));
#50010=CARTESIAN_POINT('Ctrl Pts',(31.1680189550385,-0.20305033553964,26.1106022136104));
#50011=CARTESIAN_POINT('Ctrl Pts',(31.1804056537492,0.10467710494643,26.1324223890981));
#50012=CARTESIAN_POINT('Ctrl Pts',(31.1569739806732,0.256395498849484,26.1431803571703));
#50013=CARTESIAN_POINT('Ctrl Pts',(31.0540187102742,0.541272174052999,26.1633802426127));
#50014=CARTESIAN_POINT('Ctrl Pts',(30.9759701950171,0.671873752670431,26.1722217092774));
#50015=CARTESIAN_POINT('Ctrl Pts',(30.7711018756191,0.900554058237447,26.1929097676203));
#50016=CARTESIAN_POINT('Ctrl Pts',(30.6447103916025,0.994954099829424,26.2040180088908));
#50017=CARTESIAN_POINT('Ctrl Pts',(30.3677839906361,1.12628386016982,26.2256795457743));
#50018=CARTESIAN_POINT('Ctrl Pts',(30.2208469191431,1.16405670623833,26.2360417980814));
#50019=CARTESIAN_POINT('Ctrl Pts',(29.9153739917407,1.18247957177519,26.2554533393943));
#50020=CARTESIAN_POINT('Ctrl Pts',(29.7596534858204,1.16089584886057,26.265267690896));
#50021=CARTESIAN_POINT('Ctrl Pts',(29.4669798482834,1.05871377618554,26.2868628344935));
#50022=CARTESIAN_POINT('Ctrl Pts',(29.3327683310263,0.97968769950255,26.2979062213058));
#50023=CARTESIAN_POINT('Ctrl Pts',(29.1064857982236,0.777827856716442,26.3189583910466));
#50024=CARTESIAN_POINT('Ctrl Pts',(29.0152252755147,0.658466900754918,26.3283097753497));
#50025=CARTESIAN_POINT('Ctrl Pts',(28.8789732904358,0.385760488964649,26.3476466981555));
#50026=CARTESIAN_POINT('Ctrl Pts',(28.8377485021289,0.233796400613908,26.3584220878003));
#50027=CARTESIAN_POINT('Ctrl Pts',(28.8172159011814,-0.0738574561607104,
26.3802370456529));
#50028=CARTESIAN_POINT('Ctrl Pts',(28.8367587774233,-0.226525134118623,
26.3910623250595));
#50029=CARTESIAN_POINT('Ctrl Pts',(28.9323498389723,-0.513670658612161,
26.411423088874));
#50030=CARTESIAN_POINT('Ctrl Pts',(29.0066122735479,-0.645689070611162,
26.4202237943573));
#50031=CARTESIAN_POINT('Ctrl Pts',(29.2050554476303,-0.879653705731429,
26.4407046487027));
#50032=CARTESIAN_POINT('Ctrl Pts',(29.329232754846,-0.977642983590833,26.4518041743651));
#50033=CARTESIAN_POINT('Ctrl Pts',(29.6033526154654,-1.11649688151574,26.4735601269295));
#50034=CARTESIAN_POINT('Ctrl Pts',(29.7496481694863,-1.15811817689029,26.4840194270505));
#50035=CARTESIAN_POINT('Ctrl Pts',(29.9332052808561,-1.1738184735254,26.4958478764586));
#50036=CARTESIAN_POINT('Ctrl Pts',(29.9666204732331,-1.17524047358085,26.4979502409084));
#50037=CARTESIAN_POINT('Ctrl Pts',(29.9999999999995,-1.17524047358085,26.4999999999999));
#50038=CARTESIAN_POINT('Origin',(30.,-1.21864324187371E-14,15.78125));
#50039=CARTESIAN_POINT('',(30.0000000000002,-1.17524047358085,27.0625));
#50040=CARTESIAN_POINT('',(29.9999999999999,-1.17524047358085,26.9999999999999));
#50041=CARTESIAN_POINT('',(30.,-1.17524047358085,15.78125));
#50042=CARTESIAN_POINT('Ctrl Pts',(30.0000000000003,-1.17524047358085,27.0625));
#50043=CARTESIAN_POINT('Ctrl Pts',(29.898686590649,-1.17524047358088,27.0562785792061));
#50044=CARTESIAN_POINT('Ctrl Pts',(29.7976296484377,-1.16214610940709,27.0496086633191));
#50045=CARTESIAN_POINT('Ctrl Pts',(29.5510548806291,-1.0968832857528,27.032153269422));
#50046=CARTESIAN_POINT('Ctrl Pts',(29.4119274187945,-1.02901377051944,27.0212035476842));
#50047=CARTESIAN_POINT('Ctrl Pts',(29.1656287201027,-0.842194481232163,
26.9994554755857));
#50048=CARTESIAN_POINT('Ctrl Pts',(29.0614102622354,-0.72425366568988,26.9888742198639));
#50049=CARTESIAN_POINT('Ctrl Pts',(28.9083494936521,-0.460199204673261,
26.9701133966982));
#50050=CARTESIAN_POINT('Ctrl Pts',(28.8587194637877,-0.317836463591476,
26.960036980781));
#50051=CARTESIAN_POINT('Ctrl Pts',(28.8146713989512,-0.0163533730831442,
26.9386595763769));
#50052=CARTESIAN_POINT('Ctrl Pts',(28.8228691179041,0.140138676728786,26.9275631204225));
#50053=CARTESIAN_POINT('Ctrl Pts',(28.8990556060477,0.438772825908234,26.9063877272517));
#50054=CARTESIAN_POINT('Ctrl Pts',(28.9654414239268,0.578169376458166,26.8971982372258));
#50055=CARTESIAN_POINT('Ctrl Pts',(29.1468572533747,0.822311817466142,26.8774021512523));
#50056=CARTESIAN_POINT('Ctrl Pts',(29.259591693584,0.925109502257862,26.8668348294397));
#50057=CARTESIAN_POINT('Ctrl Pts',(29.522846414638,1.08544747155122,26.8449843892055));
#50058=CARTESIAN_POINT('Ctrl Pts',(29.672078571298,1.13945389610578,26.8339056600349));
#50059=CARTESIAN_POINT('Ctrl Pts',(29.9754469871149,1.18446101454497,26.813680840772));
#50060=CARTESIAN_POINT('Ctrl Pts',(30.1261553208811,1.17798106873351,26.804850259546));
#50061=CARTESIAN_POINT('Ctrl Pts',(30.4204691708303,1.10805786050355,26.7842980916158));
#50062=CARTESIAN_POINT('Ctrl Pts',(30.5609479127602,1.04399036631935,26.7734001867649));
#50063=CARTESIAN_POINT('Ctrl Pts',(30.8118142126087,0.8639649033663,26.7516124954367));
#50064=CARTESIAN_POINT('Ctrl Pts',(30.9191345732301,0.748795351296203,26.7409390107287));
#50065=CARTESIAN_POINT('Ctrl Pts',(31.0789814493982,0.489082061456906,26.7219153792232));
#50066=CARTESIAN_POINT('Ctrl Pts',(31.13228056467,0.348399841671576,26.7122041527178));
#50067=CARTESIAN_POINT('Ctrl Pts',(31.1843745315803,0.0489678760358684,
26.6909721883974));
#50068=CARTESIAN_POINT('Ctrl Pts',(31.1805251276485,-0.10725425723734,26.6798948715428));
#50069=CARTESIAN_POINT('Ctrl Pts',(31.112642066065,-0.408638429750164,26.658524481164));
#50070=CARTESIAN_POINT('Ctrl Pts',(31.04952452927,-0.550854728541633,26.6490856679416));
#50071=CARTESIAN_POINT('Ctrl Pts',(30.8739065476105,-0.80013916056119,26.6294633115169));
#50072=CARTESIAN_POINT('Ctrl Pts',(30.7641429817239,-0.90553953226469,26.6189861492083));
#50073=CARTESIAN_POINT('Ctrl Pts',(30.5058691930861,-1.0723039712914,26.5972137340794));
#50074=CARTESIAN_POINT('Ctrl Pts',(30.3585462682162,-1.13013161506019,26.5861167698907));
#50075=CARTESIAN_POINT('Ctrl Pts',(30.1366295806596,-1.1692866034305,26.5711011916684));
#50076=CARTESIAN_POINT('Ctrl Pts',(30.0683089619122,-1.17524047358085,26.5666946944513));
#50077=CARTESIAN_POINT('Ctrl Pts',(30.,-1.17524047358085,26.5625));
#50078=CARTESIAN_POINT('Ctrl Pts',(29.9999999999995,-1.17524047358085,26.4999999999999));
#50079=CARTESIAN_POINT('Ctrl Pts',(30.1204914385722,-1.17524047358085,26.5073990989566));
#50080=CARTESIAN_POINT('Ctrl Pts',(30.2404377363977,-1.1567191282047,26.5154213729959));
#50081=CARTESIAN_POINT('Ctrl Pts',(30.503109066672,-1.07331217218126,26.5345084966475));
#50082=CARTESIAN_POINT('Ctrl Pts',(30.6398547835573,-0.997848639879795,
26.5455811972524));
#50083=CARTESIAN_POINT('Ctrl Pts',(30.8720104636609,-0.801888849767787,
26.566784844391));
#50084=CARTESIAN_POINT('Ctrl Pts',(30.9665674240944,-0.684937055709897,
26.5764328435252));
#50085=CARTESIAN_POINT('Ctrl Pts',(31.1101788342394,-0.415941539318355,
26.595506636112));
#50086=CARTESIAN_POINT('Ctrl Pts',(31.1554918067157,-0.265175979373474,
26.606197041135));
#50087=CARTESIAN_POINT('Ctrl Pts',(31.184388668241,0.0421759563922281,26.6279905905315));
#50088=CARTESIAN_POINT('Ctrl Pts',(31.1688709786064,0.195715280062819,26.6388776761339));
#50089=CARTESIAN_POINT('Ctrl Pts',(31.080842595015,0.4851372161482,26.6593998545441));
#50090=CARTESIAN_POINT('Ctrl Pts',(31.0103902901456,0.618617027917578,26.6682199013902));
#50091=CARTESIAN_POINT('Ctrl Pts',(30.8184983590075,0.857859380695496,26.6884855739597));
#50092=CARTESIAN_POINT('Ctrl Pts',(30.6966625458602,0.959431158368461,26.6995683269243));
#50093=CARTESIAN_POINT('Ctrl Pts',(30.4255868085001,1.10584185104675,26.7214052635744));
#50094=CARTESIAN_POINT('Ctrl Pts',(30.280042417997,1.15134883169079,26.7319561985547));
#50095=CARTESIAN_POINT('Ctrl Pts',(29.9776063567648,1.18496921576007,26.7517200618056));
#50096=CARTESIAN_POINT('Ctrl Pts',(29.8235440457018,1.17197554004672,26.7609515037779));
#50097=CARTESIAN_POINT('Ctrl Pts',(29.5271473201095,1.08704252411486,26.7821637300309));
#50098=CARTESIAN_POINT('Ctrl Pts',(29.3879639883513,1.01521369745337,26.7932572549969));
#50099=CARTESIAN_POINT('Ctrl Pts',(29.1499744927664,0.825212607812385,26.8146078849744));
#50100=CARTESIAN_POINT('Ctrl Pts',(29.0521140662545,0.710618013126823,26.8246118717047));
#50101=CARTESIAN_POINT('Ctrl Pts',(28.9012898027458,0.445344450507133,26.8434217499511));
#50102=CARTESIAN_POINT('Ctrl Pts',(28.8519884644377,0.295869143296566,26.8540206664119));
#50103=CARTESIAN_POINT('Ctrl Pts',(28.8148602582687,-0.0109614775297701,
26.8757772506829));
#50104=CARTESIAN_POINT('Ctrl Pts',(28.8263846212866,-0.165256365046284,
26.886717911409));
#50105=CARTESIAN_POINT('Ctrl Pts',(28.90695684434,-0.456865689279699,26.9073951919876));
#50106=CARTESIAN_POINT('Ctrl Pts',(28.9737284626765,-0.591802058760263,
26.9162939800796));
#50107=CARTESIAN_POINT('Ctrl Pts',(29.1592103949543,-0.836102522890621,
26.9363453584795));
#50108=CARTESIAN_POINT('Ctrl Pts',(29.2786778563743,-0.94110103302348,26.9474041669452));
#50109=CARTESIAN_POINT('Ctrl Pts',(29.5466042812102,-1.09478566204523,26.9693055998652));
#50110=CARTESIAN_POINT('Ctrl Pts',(29.6913217184938,-1.14405280529544,26.9799390653881));
#50111=CARTESIAN_POINT('Ctrl Pts',(29.8940937627055,-1.17166523876262,26.9933697888908));
#50112=CARTESIAN_POINT('Ctrl Pts',(29.9470693710243,-1.17524047358085,26.9967496532013));
#50113=CARTESIAN_POINT('Ctrl Pts',(29.9999999999997,-1.17524047358085,26.9999999999999));
#50114=CARTESIAN_POINT('Origin',(30.,-1.21864324187371E-14,15.78125));
#50115=CARTESIAN_POINT('',(30.0000000000002,-1.17524047358085,27.5625));
#50116=CARTESIAN_POINT('',(30.,-1.17524047358085,27.5));
#50117=CARTESIAN_POINT('',(30.,-1.17524047358085,15.78125));
#50118=CARTESIAN_POINT('Ctrl Pts',(30.0000000000004,-1.17524047358085,27.5625));
#50119=CARTESIAN_POINT('Ctrl Pts',(29.8791981655177,-1.17524047358089,27.5550818403526));
#50120=CARTESIAN_POINT('Ctrl Pts',(29.7589726578968,-1.15662316573575,27.547039018461));
#50121=CARTESIAN_POINT('Ctrl Pts',(29.4966785757901,-1.0731279551929,27.5279719317893));
#50122=CARTESIAN_POINT('Ctrl Pts',(29.3604611797136,-0.99796015863462,27.5169421590736));
#50123=CARTESIAN_POINT('Ctrl Pts',(29.1231210583237,-0.797935915977368,
27.495276047424));
#50124=CARTESIAN_POINT('Ctrl Pts',(29.0249429590029,-0.674426740918645,
27.4853218966019));
#50125=CARTESIAN_POINT('Ctrl Pts',(28.8853520572172,-0.401644540260052,
27.4659795997989));
#50126=CARTESIAN_POINT('Ctrl Pts',(28.8432060655213,-0.256055793645229,
27.4556562695324));
#50127=CARTESIAN_POINT('Ctrl Pts',(28.8154546971309,0.0488704066146756,
27.4340347229132));
#50128=CARTESIAN_POINT('Ctrl Pts',(28.8323972811925,0.205546638674019,27.4229252070608));
#50129=CARTESIAN_POINT('Ctrl Pts',(28.9250076761164,0.498408501969224,27.4021591121013));
#50130=CARTESIAN_POINT('Ctrl Pts',(28.997892508521,0.632295921050251,27.3932865033313));
#50131=CARTESIAN_POINT('Ctrl Pts',(29.1909681621961,0.865881565904131,27.3731486925495));
#50132=CARTESIAN_POINT('Ctrl Pts',(29.3095755456334,0.963111668503783,27.3624181185496));
#50133=CARTESIAN_POINT('Ctrl Pts',(29.5806971724252,1.10891198583092,27.3406000040234));
#50134=CARTESIAN_POINT('Ctrl Pts',(29.7313794614454,1.15471361111034,27.3297231163935));
#50135=CARTESIAN_POINT('Ctrl Pts',(30.0349224077729,1.1841311566887,27.3100402882342));
#50136=CARTESIAN_POINT('Ctrl Pts',(30.1845806615862,1.17018311962186,27.3009860288447));
#50137=CARTESIAN_POINT('Ctrl Pts',(30.4753054258698,1.08577187813399,27.2801406033955));
#50138=CARTESIAN_POINT('Ctrl Pts',(30.6130774728742,1.01437069747224,27.2691489037921));
#50139=CARTESIAN_POINT('Ctrl Pts',(30.8550923899249,0.82117912160722,27.2474379673869));
#50140=CARTESIAN_POINT('Ctrl Pts',(30.9563451215602,0.700625408948211,27.2371795779744));
#50141=CARTESIAN_POINT('Ctrl Pts',(31.1030012085855,0.43246305141941,27.218164862578));
#50142=CARTESIAN_POINT('Ctrl Pts',(31.1490749245368,0.288512534258167,27.207957695024));
#50143=CARTESIAN_POINT('Ctrl Pts',(31.1854037082186,-0.0146433585393976,
27.1864616764351));
#50144=CARTESIAN_POINT('Ctrl Pts',(31.173058308365,-0.171282192075426,27.1753548124176));
#50145=CARTESIAN_POINT('Ctrl Pts',(31.089040383827,-0.467218401344852,27.1543707233508));
#50146=CARTESIAN_POINT('Ctrl Pts',(31.0195638166583,-0.603975746358807,
27.1453625116794));
#50147=CARTESIAN_POINT('Ctrl Pts',(30.8326207012815,-0.843150163878356,
27.1254031429327));
#50148=CARTESIAN_POINT('Ctrl Pts',(30.7170833899544,-0.943363872050058,
27.1147553149523));
#50149=CARTESIAN_POINT('Ctrl Pts',(30.4491800434626,-1.09737775442843,27.0928436259578));
#50150=CARTESIAN_POINT('Ctrl Pts',(30.2981995637065,-1.14764798518389,27.0817899983651));
#50151=CARTESIAN_POINT('Ctrl Pts',(30.0946434783266,-1.17238533021172,27.0684130613475));
#50152=CARTESIAN_POINT('Ctrl Pts',(30.0473000417297,-1.17524047358084,27.0654045855337));
#50153=CARTESIAN_POINT('Ctrl Pts',(30.0000000000003,-1.17524047358085,27.0625));
#50154=CARTESIAN_POINT('Ctrl Pts',(29.9999999999997,-1.17524047358085,26.9999999999999));
#50155=CARTESIAN_POINT('Ctrl Pts',(30.0986058905517,-1.17524047358085,27.0060551583626));
#50156=CARTESIAN_POINT('Ctrl Pts',(30.197001235846,-1.16283641910558,27.0125371577158));
#50157=CARTESIAN_POINT('Ctrl Pts',(30.4435331990926,-1.0993899448342,27.029925526711));
#50158=CARTESIAN_POINT('Ctrl Pts',(30.5849622280491,-1.0311122983099,27.0410310521114));
#50159=CARTESIAN_POINT('Ctrl Pts',(30.8283565317534,-0.84700506573289,27.0625046195245));
#50160=CARTESIAN_POINT('Ctrl Pts',(30.9294172599309,-0.734710314399227,
27.0726917923361));
#50161=CARTESIAN_POINT('Ctrl Pts',(31.0870905034712,-0.472970868314495,
27.0916537809288));
#50162=CARTESIAN_POINT('Ctrl Pts',(31.1401926761717,-0.324772377450416,
27.1019712110874));
#50163=CARTESIAN_POINT('Ctrl Pts',(31.1850952185403,-0.0184511332937437,
27.1236916767454));
#50164=CARTESIAN_POINT('Ctrl Pts',(31.1773587357349,0.136461808282747,27.1346761621237));
#50165=CARTESIAN_POINT('Ctrl Pts',(31.1038267733963,0.430084241190232,27.1554961871532));
#50166=CARTESIAN_POINT('Ctrl Pts',(31.0404668538449,0.566412733303589,27.1645221322455));
#50167=CARTESIAN_POINT('Ctrl Pts',(30.8621032542639,0.813817787312719,27.1842464597062));
#50168=CARTESIAN_POINT('Ctrl Pts',(30.746618378735,0.920903307832853,27.195134699154));
#50169=CARTESIAN_POINT('Ctrl Pts',(30.4841269758582,1.08160589165682,27.2169511927423));
#50170=CARTESIAN_POINT('Ctrl Pts',(30.3404475283553,1.13505921838268,27.2276693335753));
#50171=CARTESIAN_POINT('Ctrl Pts',(30.0413373449537,1.18420822105003,27.2477795099651));
#50172=CARTESIAN_POINT('Ctrl Pts',(29.8888261880251,1.17970362185606,27.2566686898965));
#50173=CARTESIAN_POINT('Ctrl Pts',(29.5891419642887,1.11207867848515,27.2774691579106));
#50174=CARTESIAN_POINT('Ctrl Pts',(29.4453407649054,1.04779159085184,27.2885788725534));
#50175=CARTESIAN_POINT('Ctrl Pts',(29.1960372639306,0.870265103883027,27.3101819980009));
#50176=CARTESIAN_POINT('Ctrl Pts',(29.091548794378,0.760562756134129,27.3204877500418));
#50177=CARTESIAN_POINT('Ctrl Pts',(28.9261102653187,0.502419631695097,27.3397990837129));
#50178=CARTESIAN_POINT('Ctrl Pts',(28.8688162363146,0.355135077347701,27.3498182687336));
#50179=CARTESIAN_POINT('Ctrl Pts',(28.8157293168355,0.0491393235848099,
27.3715156546901));
#50180=CARTESIAN_POINT('Ctrl Pts',(28.8194875433144,-0.106321035237959,
27.3825389560425));
#50181=CARTESIAN_POINT('Ctrl Pts',(28.8856486083743,-0.401996025014571,
27.4035045226948));
#50182=CARTESIAN_POINT('Ctrl Pts',(28.9454972717022,-0.539801328338099,
27.4127167480926));
#50183=CARTESIAN_POINT('Ctrl Pts',(29.11742422097,-0.791565441680741,27.4322003607736));
#50184=CARTESIAN_POINT('Ctrl Pts',(29.2301245105903,-0.901546472787143,
27.4430202619491));
#50185=CARTESIAN_POINT('Ctrl Pts',(29.4887201815225,-1.06909180163981,27.4648401285834));
#50186=CARTESIAN_POINT('Ctrl Pts',(29.6313699534066,-1.1262717375032,27.4756271616522));
#50187=CARTESIAN_POINT('Ctrl Pts',(29.853348441796,-1.16837939045814,27.4907512179135));
#50188=CARTESIAN_POINT('Ctrl Pts',(29.9266702080884,-1.17524047358085,27.4954969880578));
#50189=CARTESIAN_POINT('Ctrl Pts',(30.,-1.17524047358085,27.5));
#50190=CARTESIAN_POINT('Origin',(30.,-1.21864324187371E-14,15.78125));
#50191=CARTESIAN_POINT('',(30.,-1.17524047358085,28.0625));
#50192=CARTESIAN_POINT('',(30.0000000000001,-1.17524047358085,28.));
#50193=CARTESIAN_POINT('',(30.,-1.17524047358085,15.78125));
#50194=CARTESIAN_POINT('Ctrl Pts',(30.,-1.17524047358085,28.0625));
#50195=CARTESIAN_POINT('Ctrl Pts',(29.8576309526277,-1.17524047358085,28.0537574479785));
#50196=CARTESIAN_POINT('Ctrl Pts',(29.7163289872701,-1.14937338079985,28.0441633378768));
#50197=CARTESIAN_POINT('Ctrl Pts',(29.4381412694858,-1.0437960185582,28.0233373652109));
#50198=CARTESIAN_POINT('Ctrl Pts',(29.3055725204167,-0.960712774920266,
28.0122510152415));
#50199=CARTESIAN_POINT('Ctrl Pts',(29.0812375157914,-0.748784364739409,
27.9909614703353));
#50200=CARTESIAN_POINT('Ctrl Pts',(28.991345872443,-0.622420436003701,27.9816342608879));
#50201=CARTESIAN_POINT('Ctrl Pts',(28.8663365712296,-0.344659291734443,
27.9619389197703));
#50202=CARTESIAN_POINT('Ctrl Pts',(28.8314934625426,-0.196359386622749,
27.9514233481032));
#50203=CARTESIAN_POINT('Ctrl Pts',(28.8195620391171,0.111178530712451,27.9296166112233));
#50204=CARTESIAN_POINT('Ctrl Pts',(28.8449209434754,0.267584161126331,27.9185262830501));
#50205=CARTESIAN_POINT('Ctrl Pts',(28.9530728770119,0.554595748995939,27.8981750163432));
#50206=CARTESIAN_POINT('Ctrl Pts',(29.0321899221582,0.683358417415679,27.8893700226253));
#50207=CARTESIAN_POINT('Ctrl Pts',(29.2365478324768,0.90645295573766,27.8689113436395));
#50208=CARTESIAN_POINT('Ctrl Pts',(29.3606700385593,0.997879761432882,27.8580478657718));
#50209=CARTESIAN_POINT('Ctrl Pts',(29.6397630167776,1.12947461119937,27.8362438860083));
#50210=CARTESIAN_POINT('Ctrl Pts',(29.7926014521638,1.16725893043214,27.8255188379057));
#50211=CARTESIAN_POINT('Ctrl Pts',(30.0971888483988,1.18064726325309,27.8063401680006));
#50212=CARTESIAN_POINT('Ctrl Pts',(30.2459190189188,1.15884794264961,27.7968175086224));
#50213=CARTESIAN_POINT('Ctrl Pts',(30.5325764826745,1.05897425995597,27.7756736453134));
#50214=CARTESIAN_POINT('Ctrl Pts',(30.6670400332198,0.979858412729581,27.7646115990219));
#50215=CARTESIAN_POINT('Ctrl Pts',(30.8979501916997,0.773870883397489,27.7431289156398));
#50216=CARTESIAN_POINT('Ctrl Pts',(30.9919903689524,0.648942084588862,27.7335148439956));
#50217=CARTESIAN_POINT('Ctrl Pts',(31.1243827012244,0.373674108325156,27.7139962871235));
#50218=CARTESIAN_POINT('Ctrl Pts',(31.1629506296625,0.226703861102418,27.7035749981386));
#50219=CARTESIAN_POINT('Ctrl Pts',(31.182930645767,-0.0796098768690557,
27.6818550647252));
#50220=CARTESIAN_POINT('Ctrl Pts',(31.1618436472684,-0.236207537040712,
27.6707511202069));
#50221=CARTESIAN_POINT('Ctrl Pts',(31.0615541749908,-0.526222674013738,
27.6501868794201));
#50222=CARTESIAN_POINT('Ctrl Pts',(30.9856010212307,-0.657569956578418,
27.641376820382));
#50223=CARTESIAN_POINT('Ctrl Pts',(30.7869826832863,-0.886033452367878,
27.6210802455783));
#50224=CARTESIAN_POINT('Ctrl Pts',(30.6656419827339,-0.980462303947253,
27.6102811397496));
#50225=CARTESIAN_POINT('Ctrl Pts',(30.3905261901255,-1.11936682731598,27.5884622344572));
#50226=CARTESIAN_POINT('Ctrl Pts',(30.2387339000707,-1.16125829953858,27.5776558137839));
#50227=CARTESIAN_POINT('Ctrl Pts',(30.0554488466051,-1.17426038713893,27.5659397324124));
#50228=CARTESIAN_POINT('Ctrl Pts',(30.0277113777332,-1.17524047358084,27.5642016912446));
#50229=CARTESIAN_POINT('Ctrl Pts',(30.0000000000004,-1.17524047358085,27.5625));
#50230=CARTESIAN_POINT('Ctrl Pts',(30.,-1.17524047358085,27.5));
#50231=CARTESIAN_POINT('Ctrl Pts',(30.0764884643488,-1.17524047358085,27.5046969786688));
#50232=CARTESIAN_POINT('Ctrl Pts',(30.1529528341161,-1.16777574296381,27.5096571303415));
#50233=CARTESIAN_POINT('Ctrl Pts',(30.3817494239676,-1.12246086122216,27.5253135785994));
#50234=CARTESIAN_POINT('Ctrl Pts',(30.5275514222186,-1.06175746883915,27.5364191022575));
#50235=CARTESIAN_POINT('Ctrl Pts',(30.7819194324173,-0.890185564641921,
27.5581221152238));
#50236=CARTESIAN_POINT('Ctrl Pts',(30.8893748791333,-0.782854361740771,
27.5685259964847));
#50237=CARTESIAN_POINT('Ctrl Pts',(31.0605234375151,-0.529653947481304,
27.5880127322271));
#50238=CARTESIAN_POINT('Ctrl Pts',(31.1210989339899,-0.385229961573254,
27.5976843165126));
#50239=CARTESIAN_POINT('Ctrl Pts',(31.1825194576632,-0.0817855747122669,
27.6192007914867));
#50240=CARTESIAN_POINT('Ctrl Pts',(31.1830228429167,0.0741472759213479,
27.63025759604));
#50241=CARTESIAN_POINT('Ctrl Pts',(31.1247432077576,0.371953492117145,27.6513742825742));
#50242=CARTESIAN_POINT('Ctrl Pts',(31.0685868115923,0.511361040320207,27.6608435628079));
#50243=CARTESIAN_POINT('Ctrl Pts',(30.9034614818395,0.767636822344003,27.6800694593713));
#50244=CARTESIAN_POINT('Ctrl Pts',(30.7937668420839,0.880579083554765,27.6908097772536));
#50245=CARTESIAN_POINT('Ctrl Pts',(30.5394580202052,1.05521084982092,27.712617639148));
#50246=CARTESIAN_POINT('Ctrl Pts',(30.3979930311562,1.11628678065312,27.7234700450399));
#50247=CARTESIAN_POINT('Ctrl Pts',(30.102283661711,1.18033932531086,27.7438997716137));
#50248=CARTESIAN_POINT('Ctrl Pts',(29.9510987894339,1.18375239925559,27.752701130013));
#50249=CARTESIAN_POINT('Ctrl Pts',(29.6486955420892,1.13241772430468,27.7730910160496));
#50250=CARTESIAN_POINT('Ctrl Pts',(29.5009111395855,1.07549105438516,27.7841843756164));
#50251=CARTESIAN_POINT('Ctrl Pts',(29.2414417758967,0.910237971539166,27.8059766250036));
#50252=CARTESIAN_POINT('Ctrl Pts',(29.1309679987517,0.805447516109976,27.8164757759223));
#50253=CARTESIAN_POINT('Ctrl Pts',(28.9539689931679,0.557381504423619,27.8361397402596));
#50254=CARTESIAN_POINT('Ctrl Pts',(28.8900701663349,0.415841482478183,27.8455137308899));
#50255=CARTESIAN_POINT('Ctrl Pts',(28.8202010476643,0.115104610378523,27.8668382228314));
#50256=CARTESIAN_POINT('Ctrl Pts',(28.8153164753922,-0.0411926086217122,
27.8779208638252));
#50257=CARTESIAN_POINT('Ctrl Pts',(28.8654961586475,-0.341119160610214,
27.8991878980145));
#50258=CARTESIAN_POINT('Ctrl Pts',(28.9179176762722,-0.482198917057609,
27.9089809285524));
#50259=CARTESIAN_POINT('Ctrl Pts',(29.0761417927703,-0.742958176446737,
27.9279419936907));
#50260=CARTESIAN_POINT('Ctrl Pts',(29.1827253034037,-0.858799901268264,
27.938594061191));
#50261=CARTESIAN_POINT('Ctrl Pts',(29.4325136093474,-1.04046451212148,27.9603736693398));
#50262=CARTESIAN_POINT('Ctrl Pts',(29.5726776549044,-1.10544579696665,27.9712846467122));
#50263=CARTESIAN_POINT('Ctrl Pts',(29.8127786384444,-1.16404144712018,27.9881061243607));
#50264=CARTESIAN_POINT('Ctrl Pts',(29.9063068575872,-1.17524047358087,27.9942465220726));
#50265=CARTESIAN_POINT('Ctrl Pts',(30.0000000000002,-1.17524047358085,28.));
#50266=CARTESIAN_POINT('Origin',(30.,-1.21864324187371E-14,15.78125));
#50267=CARTESIAN_POINT('',(30.,-1.17524047358085,28.5625));
#50268=CARTESIAN_POINT('',(30.0000000000002,-1.17524047358085,28.5));
#50269=CARTESIAN_POINT('',(30.,-1.17524047358085,15.78125));
#50270=CARTESIAN_POINT('Ctrl Pts',(29.9999999999999,-1.17524047358085,28.5625));
#50271=CARTESIAN_POINT('Ctrl Pts',(29.9854755687231,-1.17524047358085,28.5616080884619));
#50272=CARTESIAN_POINT('Ctrl Pts',(29.9709414772303,-1.17497122100143,28.5607060377023));
#50273=CARTESIAN_POINT('Ctrl Pts',(29.8064818821414,-1.16886648226933,28.5503905207309));
#50274=CARTESIAN_POINT('Ctrl Pts',(29.6590422242683,-1.13464684706092,28.5401233803667));
#50275=CARTESIAN_POINT('Ctrl Pts',(29.3797071247853,-1.01029888540339,28.5185614617647));
#50276=CARTESIAN_POINT('Ctrl Pts',(29.251363124374,-0.919248746833339,28.507452087585));
#50277=CARTESIAN_POINT('Ctrl Pts',(29.0406130665321,-0.695506305973089,
28.486577911123));
#50278=CARTESIAN_POINT('Ctrl Pts',(28.9590502383724,-0.56619133070644,28.4776471970656));
#50279=CARTESIAN_POINT('Ctrl Pts',(28.8493945968077,-0.283424288620792,
28.4575969003786));
#50280=CARTESIAN_POINT('Ctrl Pts',(28.8224557263032,-0.132654402250458,
28.4469061885797));
#50281=CARTESIAN_POINT('Ctrl Pts',(28.8274401393345,0.174951078681269,28.4250946609358));
#50282=CARTESIAN_POINT('Ctrl Pts',(28.8609710566448,0.328840848056597,28.4141827261138));
#50283=CARTESIAN_POINT('Ctrl Pts',(28.9834218096268,0.608264397886715,28.394369508017));
#50284=CARTESIAN_POINT('Ctrl Pts',(29.0686800279675,0.732167484395331,28.3853987862865));
#50285=CARTESIAN_POINT('Ctrl Pts',(29.2841654510491,0.944633593842617,28.3646336101487));
#50286=CARTESIAN_POINT('Ctrl Pts',(29.4135237499535,1.0299476859008,28.3536653145426));
#50287=CARTESIAN_POINT('Ctrl Pts',(29.6999884026637,1.14695518646917,28.3319258334386));
#50288=CARTESIAN_POINT('Ctrl Pts',(29.8545850153065,1.1765676391467,28.321476648926));
#50289=CARTESIAN_POINT('Ctrl Pts',(30.1599574738008,1.17387642238167,28.3026290229131));
#50290=CARTESIAN_POINT('Ctrl Pts',(30.3078958483554,1.14400535727984,28.2924854305785));
#50291=CARTESIAN_POINT('Ctrl Pts',(30.5899420117525,1.02824734362325,28.2710615776053));
#50292=CARTESIAN_POINT('Ctrl Pts',(30.7205565666579,0.941343746526345,28.2599597843468));
#50293=CARTESIAN_POINT('Ctrl Pts',(30.9384441962492,0.723734320112842,28.2388647444883));
#50294=CARTESIAN_POINT('Ctrl Pts',(31.0243441752868,0.5959705376245,28.2297587654061));
#50295=CARTESIAN_POINT('Ctrl Pts',(31.1420857275796,0.315809924237744,28.2098932839944));
#50296=CARTESIAN_POINT('Ctrl Pts',(31.1732121728651,0.166290213222924,28.1992912189719));
#50297=CARTESIAN_POINT('Ctrl Pts',(31.1771534741222,-0.14225217236566,28.1774132577855));
#50298=CARTESIAN_POINT('Ctrl Pts',(31.1475738082276,-0.298357527790664,
28.1663442213532));
#50299=CARTESIAN_POINT('Ctrl Pts',(31.0316967203975,-0.582326286717529,
28.1462087139606));
#50300=CARTESIAN_POINT('Ctrl Pts',(30.9494361151523,-0.708574806833004,
28.1373477050794));
#50301=CARTESIAN_POINT('Ctrl Pts',(30.7393766183288,-0.926260402286338,
28.1167306721673));
#50302=CARTESIAN_POINT('Ctrl Pts',(30.6125440370362,-1.01460273603848,28.1058101125197));
#50303=CARTESIAN_POINT('Ctrl Pts',(30.3296673321613,-1.13876808424026,28.0840371864985));
#50304=CARTESIAN_POINT('Ctrl Pts',(30.1758968644013,-1.17241612952657,28.0734015508245));
#50305=CARTESIAN_POINT('Ctrl Pts',(30.0133354780172,-1.17518374723503,28.0633209118452));
#50306=CARTESIAN_POINT('Ctrl Pts',(30.0066666906193,-1.17524047358085,28.0629093859629));
#50307=CARTESIAN_POINT('Ctrl Pts',(30.,-1.17524047358085,28.0625));
#50308=CARTESIAN_POINT('Ctrl Pts',(30.0000000000002,-1.17524047358085,28.));
#50309=CARTESIAN_POINT('Ctrl Pts',(30.055120011526,-1.17524047358084,28.0033847916881));
#50310=CARTESIAN_POINT('Ctrl Pts',(30.1102800819057,-1.17136342893539,28.0069094990185));
#50311=CARTESIAN_POINT('Ctrl Pts',(30.320778299587,-1.14149919825233,28.0208945034877));
#50312=CARTESIAN_POINT('Ctrl Pts',(30.4704399584402,-1.08838822567003,28.0319678602702));
#50313=CARTESIAN_POINT('Ctrl Pts',(30.7348284172129,-0.929562358310031,
28.0538343110362));
#50314=CARTESIAN_POINT('Ctrl Pts',(30.8482436418564,-0.827380507129033,
28.0644216046344));
#50315=CARTESIAN_POINT('Ctrl Pts',(31.0309964109232,-0.58443378950115,28.0842573960977));
#50316=CARTESIAN_POINT('Ctrl Pts',(31.0981318171314,-0.445680080400429,
28.0933979512832));
#50317=CARTESIAN_POINT('Ctrl Pts',(31.1762201438822,-0.147691887981632,
28.1145275412917));
#50318=CARTESIAN_POINT('Ctrl Pts',(31.1854211354334,0.00884554012676132,
28.1256272149066));
#50319=CARTESIAN_POINT('Ctrl Pts',(31.1432517249665,0.310649796547867,28.1470273923742));
#50320=CARTESIAN_POINT('Ctrl Pts',(31.0945166442476,0.453415390384783,28.1571505400084));
#50321=CARTESIAN_POINT('Ctrl Pts',(30.9430034157352,0.718468313966014,28.1759447732979));
#50322=CARTESIAN_POINT('Ctrl Pts',(30.8395316819024,0.837077300041102,28.1864571641064));
#50323=CARTESIAN_POINT('Ctrl Pts',(30.594175126874,1.02551549499305,28.2082047776097));
#50324=CARTESIAN_POINT('Ctrl Pts',(30.4553685567187,1.0942445153416,28.2191652668043));
#50325=CARTESIAN_POINT('Ctrl Pts',(30.1633070228503,1.17335763356101,28.2399049418951));
#50326=CARTESIAN_POINT('Ctrl Pts',(30.0132854694265,1.18458952272981,28.2488527114972));
#50327=CARTESIAN_POINT('Ctrl Pts',(29.7101813599922,1.14957783235101,28.2687069250423));
#50328=CARTESIAN_POINT('Ctrl Pts',(29.5603537745588,1.10100720474222,28.2796294987935));
#50329=CARTESIAN_POINT('Ctrl Pts',(29.2921855827035,0.950361389094781,28.3014380407736));
#50330=CARTESIAN_POINT('Ctrl Pts',(29.1755651130251,0.851181456436058,28.3121157317836));
#50331=CARTESIAN_POINT('Ctrl Pts',(28.9864685212412,0.613960284958293,28.3321380906356));
#50332=CARTESIAN_POINT('Ctrl Pts',(28.9157930252681,0.478217809624506,28.341090783094));
#50333=CARTESIAN_POINT('Ctrl Pts',(28.8287462552022,0.18335177826131,28.3619989885486));
#50334=CARTESIAN_POINT('Ctrl Pts',(28.8147855892159,0.0266848358587583,
28.3731078456949));
#50335=CARTESIAN_POINT('Ctrl Pts',(28.8481057813277,-0.277120858900621,
28.3946499400995));
#50336=CARTESIAN_POINT('Ctrl Pts',(28.8928044130046,-0.421659697790202,
28.4048988240612));
#50337=CARTESIAN_POINT('Ctrl Pts',(29.0376019293491,-0.692609521363159,
28.4241111916336));
#50338=CARTESIAN_POINT('Ctrl Pts',(29.1388311172626,-0.815074867447836,
28.4343484054768));
#50339=CARTESIAN_POINT('Ctrl Pts',(29.3808301647318,-1.01067727789171,28.456143840463));
#50340=CARTESIAN_POINT('Ctrl Pts',(29.5182554521743,-1.08294295653866,28.4671448960526));
#50341=CARTESIAN_POINT('Ctrl Pts',(29.7744135979937,-1.15894806924162,28.4855696371912));
#50342=CARTESIAN_POINT('Ctrl Pts',(29.8869899356779,-1.1752404735809,28.493060314833));
#50343=CARTESIAN_POINT('Ctrl Pts',(30.0000000000005,-1.17524047358085,28.5));
#50344=CARTESIAN_POINT('Origin',(30.,-1.21864324187371E-14,15.78125));
#50345=CARTESIAN_POINT('',(29.9999999999997,-1.17524047358085,29.0625));
#50346=CARTESIAN_POINT('',(30.,-1.17524047358085,29.));
#50347=CARTESIAN_POINT('',(30.,-1.17524047358085,15.78125));
#50348=CARTESIAN_POINT('Ctrl Pts',(29.9999999999995,-1.17524047358085,29.0625));
#50349=CARTESIAN_POINT('Ctrl Pts',(29.9663313283337,-1.17524047358085,29.0604324851927));
#50350=CARTESIAN_POINT('Ctrl Pts',(29.9326266255446,-1.17379373293774,29.0583114654359));
#50351=CARTESIAN_POINT('Ctrl Pts',(29.7487805300534,-1.15793171143038,29.046459536434));
#50352=CARTESIAN_POINT('Ctrl Pts',(29.6025054140808,-1.11619705168394,29.0359974721754));
#50353=CARTESIAN_POINT('Ctrl Pts',(29.3284713606868,-0.977122112422326,
29.0142389520917));
#50354=CARTESIAN_POINT('Ctrl Pts',(29.204360853848,-0.879027723836093,29.003139801917));
#50355=CARTESIAN_POINT('Ctrl Pts',(29.0061078341151,-0.644908297203287,
28.9826651365702));
#50356=CARTESIAN_POINT('Ctrl Pts',(28.9319567448549,-0.512847810431858,
28.9738647427883));
#50357=CARTESIAN_POINT('Ctrl Pts',(28.8365844224207,-0.225635628236165,
28.9534992524445));
#50358=CARTESIAN_POINT('Ctrl Pts',(28.8171575566038,-0.0729412609821712,
28.9426720805673));
#50359=CARTESIAN_POINT('Ctrl Pts',(28.8379321785986,0.234707082052963,28.92085751368));
#50360=CARTESIAN_POINT('Ctrl Pts',(28.8792757590782,0.386638085776581,28.9100844699825));
#50361=CARTESIAN_POINT('Ctrl Pts',(29.0157412244589,0.659238101106546,28.8907550914809));
#50362=CARTESIAN_POINT('Ctrl Pts',(29.107096372761,0.778529076561771,28.8813960362208));
#50363=CARTESIAN_POINT('Ctrl Pts',(29.3335481377689,0.980220242371224,28.8603394545531));
#50364=CARTESIAN_POINT('Ctrl Pts',(29.4678337645529,1.05914504636678,28.8492951073424));
#50365=CARTESIAN_POINT('Ctrl Pts',(29.760564366148,1.1610786562004,28.8277052746509));
#50366=CARTESIAN_POINT('Ctrl Pts',(29.9162604257863,1.18253750642917,28.8179009595418));
#50367=CARTESIAN_POINT('Ctrl Pts',(30.2216914945448,1.16389753053477,28.7984842912973));
#50368=CARTESIAN_POINT('Ctrl Pts',(30.3686116386073,1.12601470107769,28.7881191791422));
#50369=CARTESIAN_POINT('Ctrl Pts',(30.645460693513,0.994469364755083,28.7664547489262));
#50370=CARTESIAN_POINT('Ctrl Pts',(30.7717903384927,0.899966183411579,28.7553466483575));
#50371=CARTESIAN_POINT('Ctrl Pts',(30.9764758301347,0.671134004376585,28.7346644325598));
#50372=CARTESIAN_POINT('Ctrl Pts',(31.0544159221586,0.540492245543279,28.7258249398524));
#50373=CARTESIAN_POINT('Ctrl Pts',(31.1571623293156,0.255550540096121,28.7056204432797));
#50374=CARTESIAN_POINT('Ctrl Pts',(31.1804841833933,0.103803871660056,28.6948604703318));
#50375=CARTESIAN_POINT('Ctrl Pts',(31.1678665590545,-0.203924479708025,
28.6730402302557));
#50376=CARTESIAN_POINT('Ctrl Pts',(31.130543099267,-0.356918086122505,28.6621918400855));
#50377=CARTESIAN_POINT('Ctrl Pts',(31.0012937995436,-0.633072694293491,
28.6426104143845));
#50378=CARTESIAN_POINT('Ctrl Pts',(30.9131062008608,-0.754733454165662,
28.6334802730101));
#50379=CARTESIAN_POINT('Ctrl Pts',(30.6923373486102,-0.962047131628042,
28.6125733267459));
#50380=CARTESIAN_POINT('Ctrl Pts',(30.5605741188135,-1.04432722358406,28.6015649165697));
#50381=CARTESIAN_POINT('Ctrl Pts',(30.2834202387706,-1.14942800624881,28.5808193260016));
#50382=CARTESIAN_POINT('Ctrl Pts',(30.1422284632676,-1.17524047358085,28.5712339190787));
#50383=CARTESIAN_POINT('Ctrl Pts',(29.9999999999999,-1.17524047358085,28.5625));
#50384=CARTESIAN_POINT('Ctrl Pts',(30.0000000000005,-1.17524047358085,28.5));
#50385=CARTESIAN_POINT('Ctrl Pts',(30.0354745744302,-1.17524047358084,28.5021784110951));
#50386=CARTESIAN_POINT('Ctrl Pts',(30.070984899228,-1.17363438892678,28.50441595924));
#50387=CARTESIAN_POINT('Ctrl Pts',(30.2617617366305,-1.15628719000694,28.5167461440698));
#50388=CARTESIAN_POINT('Ctrl Pts',(30.4127085422869,-1.11138228847866,28.527607482843));
#50389=CARTESIAN_POINT('Ctrl Pts',(30.6847642885538,-0.967157900388871,
28.5494270868925));
#50390=CARTESIAN_POINT('Ctrl Pts',(30.804005950619,-0.870565283253422,28.5601740092255));
#50391=CARTESIAN_POINT('Ctrl Pts',(30.9983603111577,-0.638155310621775,
28.5803486604476));
#50392=CARTESIAN_POINT('Ctrl Pts',(31.0719538047089,-0.504858427298666,
28.5892017641887));
#50393=CARTESIAN_POINT('Ctrl Pts',(31.1663430846515,-0.212647773407092,
28.6099216835343));
#50394=CARTESIAN_POINT('Ctrl Pts',(31.1842429187448,-0.0559802512603478,
28.6210305817888));
#50395=CARTESIAN_POINT('Ctrl Pts',(31.1582832767207,0.249283949423046,28.6426760951642));
#50396=CARTESIAN_POINT('Ctrl Pts',(31.1169606007789,0.395199803964739,28.6530226198275));
#50397=CARTESIAN_POINT('Ctrl Pts',(30.9790360194058,0.668562290541804,28.6724060632391));
#50398=CARTESIAN_POINT('Ctrl Pts',(30.8818240300007,0.792402281745908,28.6822761930404));
#50399=CARTESIAN_POINT('Ctrl Pts',(30.6459736712074,0.993822232743541,28.7039003049109));
#50400=CARTESIAN_POINT('Ctrl Pts',(30.5101537410361,1.06991069848525,28.7149383113331));
#50401=CARTESIAN_POINT('Ctrl Pts',(30.2218612846042,1.16368326752433,28.7359662684601));
#50402=CARTESIAN_POINT('Ctrl Pts',(30.0727878905027,1.18239624374933,28.7452765661691));
#50403=CARTESIAN_POINT('Ctrl Pts',(29.7685724316717,1.16273575029291,28.764654767797));
#50404=CARTESIAN_POINT('Ctrl Pts',(29.6165255150965,1.12180125661046,28.7754428960271));
#50405=CARTESIAN_POINT('Ctrl Pts',(29.3404632117996,0.984593855919108,28.797259754998));
#50406=CARTESIAN_POINT('Ctrl Pts',(29.2184662863885,0.890859052794272,28.8080745514575));
#50407=CARTESIAN_POINT('Ctrl Pts',(29.0185031029016,0.663646825495766,28.8284093479536));
#50408=CARTESIAN_POINT('Ctrl Pts',(28.9418083423014,0.532910081337728,28.8372126922591));
#50409=CARTESIAN_POINT('Ctrl Pts',(28.8396688119263,0.243593095049782,28.8577274289443));
#50410=CARTESIAN_POINT('Ctrl Pts',(28.8175791014781,0.0870303940346913,
28.8688288945971));
#50411=CARTESIAN_POINT('Ctrl Pts',(28.8356734059559,-0.219589451967425,
28.8905705333577));
#50412=CARTESIAN_POINT('Ctrl Pts',(28.8733703746263,-0.366880393585839,
28.9010145619721));
#50413=CARTESIAN_POINT('Ctrl Pts',(29.0040267448551,-0.642739671975603,
28.9205750465844));
#50414=CARTESIAN_POINT('Ctrl Pts',(29.0970828699605,-0.768007510288218,
28.9301160290222));
#50415=CARTESIAN_POINT('Ctrl Pts',(29.3264450160403,-0.975407631545752,
28.9515537342264));
#50416=CARTESIAN_POINT('Ctrl Pts',(29.4604715589085,-1.05546393671967,28.9626222876417));
#50417=CARTESIAN_POINT('Ctrl Pts',(29.7327334190531,-1.15230702146743,28.9827747043974));
#50418=CARTESIAN_POINT('Ctrl Pts',(29.8659356312532,-1.17524047358086,28.9917674189746));
#50419=CARTESIAN_POINT('Ctrl Pts',(30.0000000000001,-1.17524047358085,29.));
#50420=CARTESIAN_POINT('Origin',(30.,-1.21864324187371E-14,15.78125));
#50421=CARTESIAN_POINT('',(29.9999999999999,-1.17524047358085,29.5625));
#50422=CARTESIAN_POINT('',(30.,-1.17524047358085,29.5));
#50423=CARTESIAN_POINT('',(30.,-1.17524047358085,15.78125));
#50424=CARTESIAN_POINT('Ctrl Pts',(29.9999999999998,-1.17524047358085,29.5625));
#50425=CARTESIAN_POINT('Ctrl Pts',(29.9467973546619,-1.17524047358085,29.5592329493093));
#50426=CARTESIAN_POINT('Ctrl Pts',(29.8935499193759,-1.17162840400865,29.5558350868076));
#50427=CARTESIAN_POINT('Ctrl Pts',(29.6905156464705,-1.14383638937277,29.5423818936273));
#50428=CARTESIAN_POINT('Ctrl Pts',(29.5458229652857,-1.09446322181842,29.531746189361));
#50429=CARTESIAN_POINT('Ctrl Pts',(29.2779882672223,-0.940574047774209,
29.5098431372833));
#50430=CARTESIAN_POINT('Ctrl Pts',(29.1585890601641,-0.835479489994527,
29.4987851149112));
#50431=CARTESIAN_POINT('Ctrl Pts',(28.9732889450876,-0.591037021395749,
29.4787398668936));
#50432=CARTESIAN_POINT('Ctrl Pts',(28.9066211123554,-0.456058910232785,
29.4698379853235));
#50433=CARTESIAN_POINT('Ctrl Pts',(28.8262612459225,-0.164388119091858,
29.4491563462818));
#50434=CARTESIAN_POINT('Ctrl Pts',(28.8148509180816,-0.0100732314283097,
29.4382142673958));
#50435=CARTESIAN_POINT('Ctrl Pts',(28.852213214805,0.296739305134607,29.4164589654342));
#50436=CARTESIAN_POINT('Ctrl Pts',(28.9016274703356,0.446176311860775,29.405862764764));
#50437=CARTESIAN_POINT('Ctrl Pts',(29.0526565417776,0.711342976877612,29.3870604663565));
#50438=CARTESIAN_POINT('Ctrl Pts',(29.1506118786123,0.825870653466757,29.3770454144149));
#50439=CARTESIAN_POINT('Ctrl Pts',(29.3887681357508,1.01569990993121,29.3556906361267));
#50440=CARTESIAN_POINT('Ctrl Pts',(29.5280199399709,1.08742345397384,29.3445966390884));
#50441=CARTESIAN_POINT('Ctrl Pts',(29.8244665773462,1.17210985589585,29.3233900912571));
#50442=CARTESIAN_POINT('Ctrl Pts',(29.9785058773413,1.18498177307898,29.3141652695437));
#50443=CARTESIAN_POINT('Ctrl Pts',(30.2808965556073,1.15114217787766,29.2943964213012));
#50444=CARTESIAN_POINT('Ctrl Pts',(30.4264177470889,1.1055232193301,29.2838429408837));
#50445=CARTESIAN_POINT('Ctrl Pts',(30.697402601783,0.95889535591386,29.2620038856125));
#50446=CARTESIAN_POINT('Ctrl Pts',(30.819169348162,0.85722095894767,29.2509217356401));
#50447=CARTESIAN_POINT('Ctrl Pts',(31.0108714255578,0.617827319896978,29.2306623578836));
#50448=CARTESIAN_POINT('Ctrl Pts',(31.0812140757987,0.48430476852144,29.221840827786));
#50449=CARTESIAN_POINT('Ctrl Pts',(31.1690224491511,0.194817477900372,29.2013140152506));
#50450=CARTESIAN_POINT('Ctrl Pts',(31.1844226308274,0.0412543787619307,
29.1904252437899));
#50451=CARTESIAN_POINT('Ctrl Pts',(31.1552826086302,-0.266085347349785,
29.1686325601491));
#50452=CARTESIAN_POINT('Ctrl Pts',(31.1098513200658,-0.416814367038074,
29.1579447461033));
#50453=CARTESIAN_POINT('Ctrl Pts',(30.9660264712179,-0.685700945491834,
29.1388786780306));
#50454=CARTESIAN_POINT('Ctrl Pts',(30.8713728192914,-0.802582950873403,
29.1292210796557));
#50455=CARTESIAN_POINT('Ctrl Pts',(30.6390456070483,-0.99836896334456,29.1080130601942));
#50456=CARTESIAN_POINT('Ctrl Pts',(30.5022270643229,-1.07372697770931,29.0969396285291));
#50457=CARTESIAN_POINT('Ctrl Pts',(30.2397868247199,-1.15682002769535,29.0778778247601));
#50458=CARTESIAN_POINT('Ctrl Pts',(30.1201628836901,-1.17524047358085,29.0698789231656));
#50459=CARTESIAN_POINT('Ctrl Pts',(29.9999999999995,-1.17524047358085,29.0625));
#50460=CARTESIAN_POINT('Ctrl Pts',(30.0000000000001,-1.17524047358085,29.));
#50461=CARTESIAN_POINT('Ctrl Pts',(30.0146960045521,-1.17524047358085,29.0009024474538));
#50462=CARTESIAN_POINT('Ctrl Pts',(30.0294011894743,-1.17496482224357,29.0018152315228));
#50463=CARTESIAN_POINT('Ctrl Pts',(30.199932441124,-1.16856010735523,29.0125142300756));
#50464=CARTESIAN_POINT('Ctrl Pts',(30.353002562887,-1.13175546267305,29.0232187723758));
#50465=CARTESIAN_POINT('Ctrl Pts',(30.6330116689674,-1.00191414666784,29.0450168400954));
#50466=CARTESIAN_POINT('Ctrl Pts',(30.7577840016447,-0.911212372347243,
29.0558945356534));
#50467=CARTESIAN_POINT('Ctrl Pts',(30.9634990803743,-0.689398439003151,
29.0763911529622));
#50468=CARTESIAN_POINT('Ctrl Pts',(31.0433641152287,-0.561238966842274,
29.0852039625465));
#50469=CARTESIAN_POINT('Ctrl Pts',(31.1533625468904,-0.274946500315461,
29.1055042381753));
#50470=CARTESIAN_POINT('Ctrl Pts',(31.1797284184379,-0.118602529514694,
29.1165901942211));
#50471=CARTESIAN_POINT('Ctrl Pts',(31.1696998210424,0.189193535485508,29.1384152356998));
#50472=CARTESIAN_POINT('Ctrl Pts',(31.1357401287962,0.337792934955289,29.1489520437553));
#50473=CARTESIAN_POINT('Ctrl Pts',(31.0124667812232,0.616132121424454,29.1686883723852));
#50474=CARTESIAN_POINT('Ctrl Pts',(30.9235367823029,0.742831293967475,29.1779572331897));
#50475=CARTESIAN_POINT('Ctrl Pts',(30.7007442503466,0.956131495282673,29.1992006935594));
#50476=CARTESIAN_POINT('Ctrl Pts',(30.5686344749746,1.04013508390185,29.2102914886907));
#50477=CARTESIAN_POINT('Ctrl Pts',(30.2847340927663,1.14996876391647,29.231619165161));
#50478=CARTESIAN_POINT('Ctrl Pts',(30.1365034722987,1.17678287240203,29.241562955497));
#50479=CARTESIAN_POINT('Ctrl Pts',(29.8314130542368,1.17348866622216,29.2604146402912));
#50480=CARTESIAN_POINT('Ctrl Pts',(29.6774432972388,1.14080144691636,29.271028448982));
#50481=CARTESIAN_POINT('Ctrl Pts',(29.3937190869037,1.01837161158084,29.2927918879254));
#50482=CARTESIAN_POINT('Ctrl Pts',(29.2662697773694,0.930754504522398,29.3037246074232));
#50483=CARTESIAN_POINT('Ctrl Pts',(29.0548960664095,0.714326580132712,29.3243777540292));
#50484=CARTESIAN_POINT('Ctrl Pts',(28.9719101496403,0.588650269969742,29.3332602962825));
#50485=CARTESIAN_POINT('Ctrl Pts',(28.8542643011592,0.305390771595589,29.3533455118009));
#50486=CARTESIAN_POINT('Ctrl Pts',(28.8237155837947,0.14936986715794,29.3644085600269));
#50487=CARTESIAN_POINT('Ctrl Pts',(28.8258171170069,-0.159374372506235,
29.386300834176));
#50488=CARTESIAN_POINT('Ctrl Pts',(28.8560851449643,-0.309160959864127,
29.3969218227258));
#50489=CARTESIAN_POINT('Ctrl Pts',(28.9721608102066,-0.589863983624277,
29.416825765087));
#50490=CARTESIAN_POINT('Ctrl Pts',(29.0571584178456,-0.717947603677171,
29.4258895505263));
#50491=CARTESIAN_POINT('Ctrl Pts',(29.2735722711375,-0.936836489269234,
29.4469394508198));
#50492=CARTESIAN_POINT('Ctrl Pts',(29.4037270862843,-1.02460346918986,29.4580436226767));
#50493=CARTESIAN_POINT('Ctrl Pts',(29.6852328519168,-1.14214540943397,29.4794975379443));
#50494=CARTESIAN_POINT('Ctrl Pts',(29.8330783756557,-1.1729174993834,29.4896673732243));
#50495=CARTESIAN_POINT('Ctrl Pts',(29.9885051427478,-1.17519832475183,29.4992926332218));
#50496=CARTESIAN_POINT('Ctrl Pts',(29.9942534046712,-1.17524047358085,29.4996471149485));
#50497=CARTESIAN_POINT('Ctrl Pts',(30.,-1.17524047358085,29.5));
#50498=CARTESIAN_POINT('Origin',(30.,-1.21864324187371E-14,15.78125));
#50499=CARTESIAN_POINT('',(30.,-1.17524047358085,30.0625));
#50500=CARTESIAN_POINT('',(29.9999999999998,-1.17524047358085,29.9999999999999));
#50501=CARTESIAN_POINT('',(30.,-1.17524047358085,15.78125));
#50502=CARTESIAN_POINT('Ctrl Pts',(30.,-1.17524047358085,30.0625));
#50503=CARTESIAN_POINT('Ctrl Pts',(29.9263916760993,-1.17524047358085,30.0579798840563));
#50504=CARTESIAN_POINT('Ctrl Pts',(29.8527927358329,-1.1683271801588,30.0532152422529));
#50505=CARTESIAN_POINT('Ctrl Pts',(29.6305589174408,-1.12600740432272,30.0380679862212));
#50506=CARTESIAN_POINT('Ctrl Pts',(29.4879403212856,-1.06872004039491,30.0272790588551));
#50507=CARTESIAN_POINT('Ctrl Pts',(29.229459906818,-0.900978381114361,30.0054593092048));
#50508=CARTESIAN_POINT('Ctrl Pts',(29.1168411945232,-0.790914788798306,
29.9946414903997));
#50509=CARTESIAN_POINT('Ctrl Pts',(28.9451007627829,-0.539025681180781,
29.975164899812));
#50510=CARTESIAN_POINT('Ctrl Pts',(28.885353566283,-0.401177024850609,29.9659464494622));
#50511=CARTESIAN_POINT('Ctrl Pts',(28.8194073352897,-0.10544306552401,29.944976701428));
#50512=CARTESIAN_POINT('Ctrl Pts',(28.8157651951869,0.0500317181756064,
29.9339523772439));
#50513=CARTESIAN_POINT('Ctrl Pts',(28.8690807484143,0.355959077177534,29.9122598409872));
#50514=CARTESIAN_POINT('Ctrl Pts',(28.9264649062036,0.503164977506288,29.9022508807468));
#50515=CARTESIAN_POINT('Ctrl Pts',(29.0920593097175,0.761174070029624,29.8829347271204));
#50516=CARTESIAN_POINT('Ctrl Pts',(29.1966290016669,0.870813111888444,29.8726262318314));
#50517=CARTESIAN_POINT('Ctrl Pts',(29.4460717811045,1.04817985046692,29.851020217295));
#50518=CARTESIAN_POINT('Ctrl Pts',(29.5899284156368,1.11237046788542,29.8399105187383));
#50519=CARTESIAN_POINT('Ctrl Pts',(29.8896511606184,1.17977836078127,29.8191153804746));
#50520=CARTESIAN_POINT('Ctrl Pts',(30.042143785172,1.18417711729498,29.810228885603));
#50521=CARTESIAN_POINT('Ctrl Pts',(30.3412103985985,1.13483145488925,29.7901144124214));
#50522=CARTESIAN_POINT('Ctrl Pts',(30.484863334991,1.08127741540018,29.7793943289302));
#50523=CARTESIAN_POINT('Ctrl Pts',(30.7472520600478,0.920389087318013,29.7575775552199));
#50524=CARTESIAN_POINT('Ctrl Pts',(30.8626628342488,0.813224513564577,29.7466910634298));
#50525=CARTESIAN_POINT('Ctrl Pts',(31.0408533066038,0.565701034414209,29.7269731686955));
#50526=CARTESIAN_POINT('Ctrl Pts',(31.1041185100332,0.42933329828376,29.7179429396888));
#50527=CARTESIAN_POINT('Ctrl Pts',(31.1774532864279,0.13565521801398,29.6971189688454));
#50528=CARTESIAN_POINT('Ctrl Pts',(31.185083485025,-0.0192736961984122,
29.6861333508878));
#50529=CARTESIAN_POINT('Ctrl Pts',(31.1399640096901,-0.325574493297471,
29.6644143350789));
#50530=CARTESIAN_POINT('Ctrl Pts',(31.0867572532099,-0.473736864086508,
29.654106159393));
#50531=CARTESIAN_POINT('Ctrl Pts',(30.9288924580137,-0.735375844574816,
29.6351359699395));
#50532=CARTESIAN_POINT('Ctrl Pts',(30.827743660758,-0.847605887956935,29.6249456831495));
#50533=CARTESIAN_POINT('Ctrl Pts',(30.5841967794232,-1.03154789843284,29.6034686040399));
#50534=CARTESIAN_POINT('Ctrl Pts',(30.4427060183441,-1.0997249484081,29.5923628543371));
#50535=CARTESIAN_POINT('Ctrl Pts',(30.1964052482032,-1.16291170221409,29.5749978904338));
#50536=CARTESIAN_POINT('Ctrl Pts',(30.0983061450535,-1.17524047358085,29.5685367516888));
#50537=CARTESIAN_POINT('Ctrl Pts',(29.9999999999998,-1.17524047358085,29.5625));
#50538=CARTESIAN_POINT('Ctrl Pts',(30.,-1.17524047358085,29.5));
#50539=CARTESIAN_POINT('Ctrl Pts',(30.1499565209686,-1.17524047358085,29.5092084811251));
#50540=CARTESIAN_POINT('Ctrl Pts',(30.2986551183888,-1.14654165825818,29.5193571963421));
#50541=CARTESIAN_POINT('Ctrl Pts',(30.5805418737435,-1.03331719508937,29.5406814366056));
#50542=CARTESIAN_POINT('Ctrl Pts',(30.7104602238272,-0.948696043146186,
29.5516595563353));
#50543=CARTESIAN_POINT('Ctrl Pts',(30.9271652336418,-0.73741304903825,29.5724576785973));
#50544=CARTESIAN_POINT('Ctrl Pts',(31.0130985609625,-0.614031092469691,
29.5814606062707));
#50545=CARTESIAN_POINT('Ctrl Pts',(31.1371264539894,-0.335358891062759,
29.6012205481486));
#50546=CARTESIAN_POINT('Ctrl Pts',(31.1715373282526,-0.181667965902616,
29.6121183834297));
#50547=CARTESIAN_POINT('Ctrl Pts',(31.1782875351469,0.125982959094587,29.6339331333974));
#50548=CARTESIAN_POINT('Ctrl Pts',(31.1521830035108,0.27698654047903,29.6446404159195));
#50549=CARTESIAN_POINT('Ctrl Pts',(31.0441268483734,0.560261316579686,29.6647267147429));
#50550=CARTESIAN_POINT('Ctrl Pts',(30.9634093757068,0.689883113720223,29.6736315391227));
#50551=CARTESIAN_POINT('Ctrl Pts',(30.7540662315648,0.914815989860588,29.6944615256665));
#50552=CARTESIAN_POINT('Ctrl Pts',(30.6261826944801,1.0066730037076,29.7055712306082));
#50553=CARTESIAN_POINT('Ctrl Pts',(30.3474095969538,1.1326991331979,29.7271581352984));
#50554=CARTESIAN_POINT('Ctrl Pts',(30.2000827038505,1.16777128079541,29.7374485757904));
#50555=CARTESIAN_POINT('Ctrl Pts',(29.8935937537322,1.18085135992657,29.7567330869508));
#50556=CARTESIAN_POINT('Ctrl Pts',(29.7372662628443,1.15617395643532,29.7668098469142));
#50557=CARTESIAN_POINT('Ctrl Pts',(29.4460305983855,1.04785975410839,29.7885340948419));
#50558=CARTESIAN_POINT('Ctrl Pts',(29.3136703421255,0.966357190577468,29.7995516007362));
#50559=CARTESIAN_POINT('Ctrl Pts',(29.091570241583,0.760352988788506,29.8204938700552));
#50560=CARTESIAN_POINT('Ctrl Pts',(29.0026423680915,0.639251124272773,29.8296723175212));
#50561=CARTESIAN_POINT('Ctrl Pts',(28.8716938065568,0.363925746310141,29.8491949446027));
#50562=CARTESIAN_POINT('Ctrl Pts',(28.8334229675251,0.211172023558316,29.8600263252283));
#50563=CARTESIAN_POINT('Ctrl Pts',(28.8188892259004,-0.0965571382164996,
29.8818466227683));
#50564=CARTESIAN_POINT('Ctrl Pts',(28.8412989000486,-0.248535346834791,
29.8926230136456));
#50565=CARTESIAN_POINT('Ctrl Pts',(28.942312504556,-0.5340148591211,29.9128656447428));
#50566=CARTESIAN_POINT('Ctrl Pts',(29.0193556498266,-0.664990211735325,
29.9216906330323));
#50567=CARTESIAN_POINT('Ctrl Pts',(29.2225255933627,-0.895077676800941,
29.9423242871271));
#50568=CARTESIAN_POINT('Ctrl Pts',(29.3483400060408,-0.990433515042349,
29.9534309783521));
#50569=CARTESIAN_POINT('Ctrl Pts',(29.6245422330139,-1.1237624473258,29.9751189235115));
#50570=CARTESIAN_POINT('Ctrl Pts',(29.7713190573348,-1.16255586776877,29.985507518588));
#50571=CARTESIAN_POINT('Ctrl Pts',(29.9476315409713,-1.1743662864253,29.9967531815485));
#50572=CARTESIAN_POINT('Ctrl Pts',(29.9738286104226,-1.17524047358085,29.9983928758457));
#50573=CARTESIAN_POINT('Ctrl Pts',(29.9999999999996,-1.17524047358085,29.9999999999999));
#50574=CARTESIAN_POINT('Origin',(30.,-1.21864324187371E-14,15.78125));
#50575=CARTESIAN_POINT('',(30.,-1.17524047358085,30.5625));
#50576=CARTESIAN_POINT('',(29.9999999999998,-1.17524047358085,30.4999999999999));
#50577=CARTESIAN_POINT('',(30.,-1.17524047358085,15.78125));
#50578=CARTESIAN_POINT('Ctrl Pts',(29.9999999999999,-1.17524047358085,30.5625));
#50579=CARTESIAN_POINT('Ctrl Pts',(29.87859718881,-1.17524047358085,30.555044935771));
#50580=CARTESIAN_POINT('Ctrl Pts',(29.7578462794256,-1.15643017462348,30.5469630079231));
#50581=CARTESIAN_POINT('Ctrl Pts',(29.5223698659242,-1.08113291221706,30.5298333797947));
#50582=CARTESIAN_POINT('Ctrl Pts',(29.4096002088597,-1.02391620699781,30.5208799114591));
#50583=CARTESIAN_POINT('Ctrl Pts',(29.1820826863431,-0.858187725726655,
30.5010328956616));
#50584=CARTESIAN_POINT('Ctrl Pts',(29.0755864711026,-0.74226695058618,30.4903833861391));
#50585=CARTESIAN_POINT('Ctrl Pts',(28.9175541454242,-0.481384400712606,
30.4714297273205));
#50586=CARTESIAN_POINT('Ctrl Pts',(28.8652363337421,-0.340257481842474,
30.4616267985498));
#50587=CARTESIAN_POINT('Ctrl Pts',(28.815283295232,-0.0402726424447981,
30.4403556313474));
#50588=CARTESIAN_POINT('Ctrl Pts',(28.8202904087434,0.116033016014593,30.4292723919329));
#50589=CARTESIAN_POINT('Ctrl Pts',(28.8903942350679,0.41669295482916,30.4079533551363));
#50590=CARTESIAN_POINT('Ctrl Pts',(28.9543854043788,0.558153128819785,30.3985868124474));
#50591=CARTESIAN_POINT('Ctrl Pts',(29.1315478521803,0.806074678810529,30.3789179332106));
#50592=CARTESIAN_POINT('Ctrl Pts',(29.2421055811419,0.910792536064214,30.3684162008828));
#50593=CARTESIAN_POINT('Ctrl Pts',(29.5017160718709,1.07586594659562,30.3466216552675));
#50594=CARTESIAN_POINT('Ctrl Pts',(29.6495548172672,1.13268560353193,30.3355287526402));
#50595=CARTESIAN_POINT('Ctrl Pts',(29.9519945282947,1.1837871612187,30.3151448923318));
#50596=CARTESIAN_POINT('Ctrl Pts',(30.1031613914609,1.18026105601431,30.3063430973327));
#50597=CARTESIAN_POINT('Ctrl Pts',(30.3988201345177,1.11599305235349,30.2859088407808));
#50598=CARTESIAN_POINT('Ctrl Pts',(30.5402500629299,1.05480717912897,30.2750546900124));
#50599=CARTESIAN_POINT('Ctrl Pts',(30.7944347031296,0.879976451319597,30.2532473998958));
#50600=CARTESIAN_POINT('Ctrl Pts',(30.9040431118398,0.766951615348157,30.2425094496776));
#50601=CARTESIAN_POINT('Ctrl Pts',(31.0689753458081,0.510549117592882,30.223290918131));
#50602=CARTESIAN_POINT('Ctrl Pts',(31.1250271192607,0.371095429137332,30.2138134394961));
#50603=CARTESIAN_POINT('Ctrl Pts',(31.1830815580213,0.0732292938782705,
30.1926925042524));
#50604=CARTESIAN_POINT('Ctrl Pts',(31.1824563525586,-0.0827153416037653,
30.1816348640652));
#50605=CARTESIAN_POINT('Ctrl Pts',(31.1207993480439,-0.386085590380016,
30.1601236460354));
#50606=CARTESIAN_POINT('Ctrl Pts',(31.0601308144882,-0.530428613118422,
30.1504611573687));
#50607=CARTESIAN_POINT('Ctrl Pts',(30.8888193562276,-0.783487027384905,
30.1309694527541));
#50608=CARTESIAN_POINT('Ctrl Pts',(30.7812795445953,-0.890749011015136,
30.1205628449218));
#50609=CARTESIAN_POINT('Ctrl Pts',(30.5267682373962,-1.06214794901788,30.0988571647179));
#50610=CARTESIAN_POINT('Ctrl Pts',(30.3809100882996,-1.12274761000244,30.0877518706328));
#50611=CARTESIAN_POINT('Ctrl Pts',(30.1523604876879,-1.16783357423751,30.0721187053907));
#50612=CARTESIAN_POINT('Ctrl Pts',(30.0761915030069,-1.17524047358085,30.0671787429637));
#50613=CARTESIAN_POINT('Ctrl Pts',(30.,-1.17524047358085,30.0625));
#50614=CARTESIAN_POINT('Ctrl Pts',(29.9999999999996,-1.17524047358085,29.9999999999999));
#50615=CARTESIAN_POINT('Ctrl Pts',(30.1287289986958,-1.17524047358085,30.0079049483617));
#50616=CARTESIAN_POINT('Ctrl Pts',(30.2567455299606,-1.1540988796436,30.0165156942669));
#50617=CARTESIAN_POINT('Ctrl Pts',(30.5250941977629,-1.06268366593765,30.0362353726713));
#50618=CARTESIAN_POINT('Ctrl Pts',(30.659989580509,-0.984598569323181,30.0472873928126));
#50619=CARTESIAN_POINT('Ctrl Pts',(30.8878392789542,-0.78430373476697,30.0683803131598));
#50620=CARTESIAN_POINT('Ctrl Pts',(30.9799768519055,-0.665589512740196,
30.0778047289255));
#50621=CARTESIAN_POINT('Ctrl Pts',(31.1182025022512,-0.393869611947964,
30.0970717007283));
#50622=CARTESIAN_POINT('Ctrl Pts',(31.16052513775,-0.242215229337512,30.1078251299214));
#50623=CARTESIAN_POINT('Ctrl Pts',(31.183296750852,0.0653802899747305,30.1296359512119));
#50624=CARTESIAN_POINT('Ctrl Pts',(31.1648281646971,0.218291541355271,30.1404785017947));
#50625=CARTESIAN_POINT('Ctrl Pts',(31.0712608350547,0.506051914399227,30.1608828629668));
#50626=CARTESIAN_POINT('Ctrl Pts',(30.9980258995704,0.638460005209143,30.1696826775517));
#50627=CARTESIAN_POINT('Ctrl Pts',(30.8013405043472,0.873851821952036,30.1901061897083));
#50628=CARTESIAN_POINT('Ctrl Pts',(30.6777833777517,0.972810187954768,30.2012019893176));
#50629=CARTESIAN_POINT('Ctrl Pts',(30.4044625790663,1.11370354858798,30.222981179922));
#50630=CARTESIAN_POINT('Ctrl Pts',(30.2583590845709,1.15637148267232,30.2334657933678));
#50631=CARTESIAN_POINT('Ctrl Pts',(29.9547860481489,1.18442751029054,30.2531021983901));
#50632=CARTESIAN_POINT('Ctrl Pts',(29.8001302980418,1.16832333064129,30.2625187720286));
#50633=CARTESIAN_POINT('Ctrl Pts',(29.5050358022508,1.07710916045235,30.2838737217699));
#50634=CARTESIAN_POINT('Ctrl Pts',(29.3676216445827,1.00262104003874,30.2949528877718));
#50635=CARTESIAN_POINT('Ctrl Pts',(29.133885390368,0.808265735464436,30.3161967092816));
#50636=CARTESIAN_POINT('Ctrl Pts',(29.0384365029953,0.691955856048158,30.3259351581227));
#50637=CARTESIAN_POINT('Ctrl Pts',(28.8928615291795,0.423965303949737,30.3449376912299));
#50638=CARTESIAN_POINT('Ctrl Pts',(28.8464607134353,0.273539680594875,30.3556039922081));
#50639=CARTESIAN_POINT('Ctrl Pts',(28.8153257979048,-0.0336925494769084,
30.3773890535762));
#50640=CARTESIAN_POINT('Ctrl Pts',(28.8297608924994,-0.187447360914171,
30.3882914188718));
#50641=CARTESIAN_POINT('Ctrl Pts',(28.915763813331,-0.477469105343294,30.4088561281766));
#50642=CARTESIAN_POINT('Ctrl Pts',(28.9852090680907,-0.611342914279369,
30.4176917737044));
#50643=CARTESIAN_POINT('Ctrl Pts',(29.1753547758778,-0.851973319195576,
30.4378994263954));
#50644=CARTESIAN_POINT('Ctrl Pts',(29.296552814894,-0.954486386260336,30.4489763873607));
#50645=CARTESIAN_POINT('Ctrl Pts',(29.5667870728762,-1.10289061661543,30.4708323290802));
#50646=CARTESIAN_POINT('Ctrl Pts',(29.7121150852083,-1.14942616389095,30.4814064433112));
#50647=CARTESIAN_POINT('Ctrl Pts',(29.9080894843003,-1.17254804864973,30.4942605325068));
#50648=CARTESIAN_POINT('Ctrl Pts',(29.9540678655128,-1.17524047358085,30.497179414468));
#50649=CARTESIAN_POINT('Ctrl Pts',(29.9999999999996,-1.17524047358085,30.4999999999999));
#50650=CARTESIAN_POINT('Origin',(30.,-1.21864324187371E-14,15.78125));
#50651=CARTESIAN_POINT('',(30.8234078741651,-0.838564036615812,30.5625));
#50652=CARTESIAN_POINT('Ctrl Pts',(29.9999999999996,-1.17524047358085,30.4999999999999));
#50653=CARTESIAN_POINT('Ctrl Pts',(30.1063627165445,-1.17524047358085,30.506531487003));
#50654=CARTESIAN_POINT('Ctrl Pts',(30.2124142608556,-1.16080842479057,30.5135555357051));
#50655=CARTESIAN_POINT('Ctrl Pts',(30.4106617155444,-1.10559796456395,30.5276868678729));
#50656=CARTESIAN_POINT('Ctrl Pts',(30.5022820820407,-1.06709869288998,30.5346780045058));
#50657=CARTESIAN_POINT('Ctrl Pts',(30.673678737238,-0.968061456707972,30.5487143145253));
#50658=CARTESIAN_POINT('Ctrl Pts',(30.7527765496958,-0.90791877422844,30.555703810039));
#50659=CARTESIAN_POINT('Ctrl Pts',(30.823407874166,-0.83856403661491,30.5625000000001));
#50660=CARTESIAN_POINT('Origin',(30.,-1.56558793706907E-14,30.5625000000001));
#50661=CARTESIAN_POINT('Origin',(30.,-1.32966554433622E-14,16.));
#50662=CARTESIAN_POINT('Origin',(30.,-1.32966554433622E-14,16.));
#50663=CARTESIAN_POINT('',(31.2041934952953,-0.894381364904537,16.3247595264192));
#50664=CARTESIAN_POINT('Ctrl Pts',(29.1765921258349,-0.838564036615844,
16.));
#50665=CARTESIAN_POINT('Ctrl Pts',(29.2487520159976,-0.936812680701164,
16.0195455809545));
#50666=CARTESIAN_POINT('Ctrl Pts',(29.3353435467743,-1.0235639347367,16.039234228078));
#50667=CARTESIAN_POINT('Ctrl Pts',(29.5376779891223,-1.17276771461038,16.0788670880384));
#50668=CARTESIAN_POINT('Ctrl Pts',(29.6536089107031,-1.23245734148137,16.0985110228563));
#50669=CARTESIAN_POINT('Ctrl Pts',(29.9561347058367,-1.33132329595442,16.1436679915754));
#50670=CARTESIAN_POINT('Ctrl Pts',(30.1342881765676,-1.34356937043143,16.1651272257976));
#50671=CARTESIAN_POINT('Ctrl Pts',(30.4639364648848,-1.31596498262617,16.2103767681647));
#50672=CARTESIAN_POINT('Ctrl Pts',(30.6256204275016,-1.27296147517128,16.233574208582));
#50673=CARTESIAN_POINT('Ctrl Pts',(30.9367837613818,-1.12785658919505,16.2803666131763));
#50674=CARTESIAN_POINT('Ctrl Pts',(31.0819753809162,-1.0232586553723,16.3034869854933));
#50675=CARTESIAN_POINT('Ctrl Pts',(31.2041934952953,-0.894381364904556,
16.3247595264192));
#50676=CARTESIAN_POINT('',(30.2433378840047,-1.48013062741372,16.3247595264192));
#50677=CARTESIAN_POINT('Origin',(30.,-1.32966554433622E-14,16.3247595264192));
#50678=CARTESIAN_POINT('Ctrl Pts',(30.0000000000046,1.33373412263454,16.1584936490537));
#50679=CARTESIAN_POINT('Ctrl Pts',(29.9229566197526,1.33637706265986,16.161136589079));
#50680=CARTESIAN_POINT('Ctrl Pts',(29.8544450638259,1.33215454753135,16.163603109717));
#50681=CARTESIAN_POINT('Ctrl Pts',(29.6282514683273,1.30599264999734,16.1719556820851));
#50682=CARTESIAN_POINT('Ctrl Pts',(29.4645017898244,1.25493599443995,16.1785525854589));
#50683=CARTESIAN_POINT('Ctrl Pts',(29.1556314965168,1.0904442613039,16.1921322573206));
#50684=CARTESIAN_POINT('Ctrl Pts',(29.0151927695643,0.975180135374777,16.1989814826418));
#50685=CARTESIAN_POINT('Ctrl Pts',(28.7777605589636,0.68493937081347,16.2122079855113));
#50686=CARTESIAN_POINT('Ctrl Pts',(28.6970848553023,0.520026749838233,16.218047438772));
#50687=CARTESIAN_POINT('Ctrl Pts',(28.5955913245901,0.191124499754384,16.2305887595464));
#50688=CARTESIAN_POINT('Ctrl Pts',(28.5759298114947,0.010043627653028,16.2373963058958));
#50689=CARTESIAN_POINT('Ctrl Pts',(28.6063542045486,-0.355647637044131,
16.2509482038391));
#50690=CARTESIAN_POINT('Ctrl Pts',(28.6584675525716,-0.536586390481523,
16.2575508938686));
#50691=CARTESIAN_POINT('Ctrl Pts',(28.804769485922,-0.819110586341092,16.2677424893791));
#50692=CARTESIAN_POINT('Ctrl Pts',(28.9031317119719,-0.969713974958467,
16.273653025791));
#50693=CARTESIAN_POINT('Ctrl Pts',(29.199410976174,-1.23941646392093,16.2879449223019));
#50694=CARTESIAN_POINT('Ctrl Pts',(29.3637987944395,-1.33889148571261,16.2948596529243));
#50695=CARTESIAN_POINT('Ctrl Pts',(29.6508112528307,-1.44362228182862,16.3055460935814));
#50696=CARTESIAN_POINT('Ctrl Pts',(29.7632922636866,-1.47020844863719,16.3094443635539));
#50697=CARTESIAN_POINT('Ctrl Pts',(29.9994132050485,-1.49732183809384,16.3170683877131));
#50698=CARTESIAN_POINT('Ctrl Pts',(30.1229027402064,-1.49587628373705,16.3207589898335));
#50699=CARTESIAN_POINT('Ctrl Pts',(30.2433378840021,-1.48013062741405,16.3247595264191));
#50700=CARTESIAN_POINT('Origin',(30.,-1.32966554433622E-14,16.));
#50701=CARTESIAN_POINT('Ctrl Pts',(30.0000000000002,-1.50000000000001,16.8125));
#50702=CARTESIAN_POINT('Ctrl Pts',(29.8374309170617,-1.50000000000001,16.8046783913503));
#50703=CARTESIAN_POINT('Ctrl Pts',(29.6757197620765,-1.47357729444258,16.7961640957352));
#50704=CARTESIAN_POINT('Ctrl Pts',(29.3345753610171,-1.35867108066285,16.7765589388149));
#50705=CARTESIAN_POINT('Ctrl Pts',(29.1621497524653,-1.25967607222118,16.7655132465099));
#50706=CARTESIAN_POINT('Ctrl Pts',(28.8706191056789,-1.00528518925076,16.7444205583108));
#50707=CARTESIAN_POINT('Ctrl Pts',(28.7525289442937,-0.85433413605806,16.7349630075588));
#50708=CARTESIAN_POINT('Ctrl Pts',(28.5748830688675,-0.508513347476126,
16.7157507415264));
#50709=CARTESIAN_POINT('Ctrl Pts',(28.5201083225798,-0.315342861227666,
16.705019047846));
#50710=CARTESIAN_POINT('Ctrl Pts',(28.4893812381258,0.0768796360488758,
16.6832289091084));
#50711=CARTESIAN_POINT('Ctrl Pts',(28.5120877046559,0.272040866827356,16.6723866185096));
#50712=CARTESIAN_POINT('Ctrl Pts',(28.6297398561329,0.63947572665909,16.6519735707412));
#50713=CARTESIAN_POINT('Ctrl Pts',(28.7222788636186,0.808683440996407,16.6431776245867));
#50714=CARTESIAN_POINT('Ctrl Pts',(28.9715826684579,1.11011928821307,16.6228097717056));
#50715=CARTESIAN_POINT('Ctrl Pts',(29.1285972489479,1.2371944826493,16.6117255376675));
#50716=CARTESIAN_POINT('Ctrl Pts',(29.4764211128784,1.41875808710319,16.5899474207545));
#50717=CARTESIAN_POINT('Ctrl Pts',(29.6625283053455,1.47415762233606,16.5794544583034));
#50718=CARTESIAN_POINT('Ctrl Pts',(30.0492497355351,1.51196727264003,16.5597980467542));
#50719=CARTESIAN_POINT('Ctrl Pts',(30.2463054645629,1.49258742024928,16.5504437178179));
#50720=CARTESIAN_POINT('Ctrl Pts',(30.6231564270347,1.37865583779414,16.529147701253));
#50721=CARTESIAN_POINT('Ctrl Pts',(30.7990856424485,1.28470816478719,16.5180736453463));
#50722=CARTESIAN_POINT('Ctrl Pts',(31.0988336211311,1.03864170876325,16.4968168346638));
#50723=CARTESIAN_POINT('Ctrl Pts',(31.2215556301223,0.891049402060874,16.4870027445589));
#50724=CARTESIAN_POINT('Ctrl Pts',(31.4094506590971,0.550436181771672,16.4680797878762));
#50725=CARTESIAN_POINT('Ctrl Pts',(31.4699049158396,0.359005410515039,16.4574447450286));
#50726=CARTESIAN_POINT('Ctrl Pts',(31.5122933091642,-0.0326520383467692,
16.4356859978696));
#50727=CARTESIAN_POINT('Ctrl Pts',(31.4952196858866,-0.228959953862231,
16.4247800025632));
#50728=CARTESIAN_POINT('Ctrl Pts',(31.3881172406464,-0.599526626811694,
16.4041929651771));
#50729=CARTESIAN_POINT('Ctrl Pts',(31.300844426577,-0.770779121647004,16.3953430421646));
#50730=CARTESIAN_POINT('Ctrl Pts',(31.0690211851343,-1.06871793972269,16.3759133629805));
#50731=CARTESIAN_POINT('Ctrl Pts',(30.9276174608134,-1.1935139431374,16.3656435174717));
#50732=CARTESIAN_POINT('Ctrl Pts',(30.6058972740411,-1.3849221656676,16.3448478526983));
#50733=CARTESIAN_POINT('Ctrl Pts',(30.4282952255496,-1.44972308953241,16.3345029444933));
#50734=CARTESIAN_POINT('Ctrl Pts',(30.2433378840032,-1.48013062741398,16.3247595264191));
#50735=CARTESIAN_POINT('Ctrl Pts',(31.2041934952953,-0.894381364904531,
16.3247595264192));
#50736=CARTESIAN_POINT('Ctrl Pts',(31.2978308567217,-0.768308186313297,
16.33276668881));
#50737=CARTESIAN_POINT('Ctrl Pts',(31.3710758402094,-0.628345765505124,
16.3400919019164));
#50738=CARTESIAN_POINT('Ctrl Pts',(31.4735871865681,-0.324510524004584,
16.3569716375553));
#50739=CARTESIAN_POINT('Ctrl Pts',(31.5001727925959,-0.161986730686535,
16.3660007371841));
#50740=CARTESIAN_POINT('Ctrl Pts',(31.4997859079869,0.202485940247452,16.3862492189027));
#50741=CARTESIAN_POINT('Ctrl Pts',(31.4592164909323,0.401327421311596,16.3972959678507));
#50742=CARTESIAN_POINT('Ctrl Pts',(31.3063109849155,0.761415726638002,16.4173008737022));
#50743=CARTESIAN_POINT('Ctrl Pts',(31.1993149527403,0.920789441682028,16.4262087502572));
#50744=CARTESIAN_POINT('Ctrl Pts',(30.927737201713,1.19478997630558,16.4468861668575));
#50745=CARTESIAN_POINT('Ctrl Pts',(30.7642938567671,1.30539963746525,16.4578223290454));
#50746=CARTESIAN_POINT('Ctrl Pts',(30.4012071029328,1.45894804482998,16.4795565821721));
#50747=CARTESIAN_POINT('Ctrl Pts',(30.2045613271838,1.49922584611532,16.4901365342825));
#50748=CARTESIAN_POINT('Ctrl Pts',(29.8153532439137,1.50071981302521,16.5089038160006));
#50749=CARTESIAN_POINT('Ctrl Pts',(29.6264615866043,1.46518905889,16.5189388458803));
#50750=CARTESIAN_POINT('Ctrl Pts',(29.2652001883276,1.32257698188105,16.5402814895924));
#50751=CARTESIAN_POINT('Ctrl Pts',(29.0973517156097,1.21423683760981,16.5513665514533));
#50752=CARTESIAN_POINT('Ctrl Pts',(28.8152158635768,0.940440031832944,16.5725462857904));
#50753=CARTESIAN_POINT('Ctrl Pts',(28.7029935775965,0.778399491568193,16.5817555838018));
#50754=CARTESIAN_POINT('Ctrl Pts',(28.5479560175053,0.422736814401416,16.6015146214222));
#50755=CARTESIAN_POINT('Ctrl Pts',(28.5057189580682,0.232905312381588,16.6120608159788));
#50756=CARTESIAN_POINT('Ctrl Pts',(28.4951590610144,-0.159927799856357,
16.6338848777698));
#50757=CARTESIAN_POINT('Ctrl Pts',(28.5299387266544,-0.359247208886169,
16.6449581782715));
#50758=CARTESIAN_POINT('Ctrl Pts',(28.6722713443677,-0.723556115441905,
16.665197561969));
#50759=CARTESIAN_POINT('Ctrl Pts',(28.7749427214916,-0.886360478602884,
16.6740138619457));
#50760=CARTESIAN_POINT('Ctrl Pts',(29.0386829229376,-1.16785093047933,16.6945222475229));
#50761=CARTESIAN_POINT('Ctrl Pts',(29.1984334219549,-1.28276611305493,16.7054003353954));
#50762=CARTESIAN_POINT('Ctrl Pts',(29.5564186818177,-1.44663336596446,16.7271757773774));
#50763=CARTESIAN_POINT('Ctrl Pts',(29.7518446854206,-1.49263399091841,16.7378560104973));
#50764=CARTESIAN_POINT('Ctrl Pts',(29.9670564156215,-1.49972884223086,16.7484074688974));
#50765=CARTESIAN_POINT('Ctrl Pts',(29.9835330897433,-1.50000000000001,16.7492077354109));
#50766=CARTESIAN_POINT('Ctrl Pts',(30.,-1.50000000000001,16.75));
#50767=CARTESIAN_POINT('Origin',(27.4975425688509,1.03655180724329,15.7235432561772));
#50768=CARTESIAN_POINT('',(27.507537153458,1.0459948352816,31.5905494329235));
#50769=CARTESIAN_POINT('',(27.4979325782409,1.02280733953167,31.5905494329235));
#50770=CARTESIAN_POINT('Origin',(27.4975191258909,1.03656151763528,31.5962151370756));
#50771=CARTESIAN_POINT('',(27.4979325782409,1.02280733953167,33.8969505670765));
#50772=CARTESIAN_POINT('',(27.4979325782409,1.02280733953167,15.7235432561772));
#50773=CARTESIAN_POINT('',(27.507537153458,1.0459948352816,33.8969505670765));
#50774=CARTESIAN_POINT('Origin',(27.4975191258914,1.03656151763504,33.891284862925));
#50775=CARTESIAN_POINT('',(27.507537153458,1.0459948352816,15.7235432561772));
#50776=CARTESIAN_POINT('Origin',(27.4239298924869,0.837015916807854,15.7235432561772));
#50777=CARTESIAN_POINT('',(27.4331527756843,0.847214001212616,31.5905494329235));
#50778=CARTESIAN_POINT('',(27.4253970781159,0.823344418487269,31.5905494329235));
#50779=CARTESIAN_POINT('Origin',(27.4239057599253,0.837023757952457,31.5962151370753));
#50780=CARTESIAN_POINT('',(27.4253970781159,0.823344418487269,33.8969505670765));
#50781=CARTESIAN_POINT('',(27.4253970781159,0.823344418487269,15.7235432561772));
#50782=CARTESIAN_POINT('',(27.4331527756843,0.847214001212616,33.8969505670765));
#50783=CARTESIAN_POINT('Origin',(27.4239057599256,0.837023757952334,33.8912848629251));
#50784=CARTESIAN_POINT('',(27.4331527756843,0.847214001212616,15.7235432561772));
#50785=CARTESIAN_POINT('Origin',(27.3661995449658,0.632319544909263,15.7235432561772));
#50786=CARTESIAN_POINT('',(27.3745938646118,0.643209811098917,31.5905494329235));
#50787=CARTESIAN_POINT('',(27.3687348611468,0.618805305313091,31.5905494329235));
#50788=CARTESIAN_POINT('Origin',(27.3661748715877,0.632325468463276,31.5962151370755));
#50789=CARTESIAN_POINT('',(27.3687348611468,0.618805305313091,33.8969505670765));
#50790=CARTESIAN_POINT('',(27.3687348611468,0.618805305313091,15.7235432561772));
#50791=CARTESIAN_POINT('',(27.3745938646118,0.643209811098917,33.8969505670765));
#50792=CARTESIAN_POINT('Origin',(27.3661748715881,0.632325468463155,33.891284862925));
#50793=CARTESIAN_POINT('',(27.3745938646118,0.643209811098917,15.7235432561772));
#50794=CARTESIAN_POINT('Origin',(27.3247074530776,0.423724712748722,15.7235432561772));
#50795=CARTESIAN_POINT('',(27.3322214554001,0.435240018610828,31.5905494329235));
#50796=CARTESIAN_POINT('',(27.328295268743,0.410451051658016,31.5905494329235));
#50797=CARTESIAN_POINT('Origin',(27.3246823910025,0.423728682191457,31.5962151370754));
#50798=CARTESIAN_POINT('',(27.328295268743,0.410451051658016,33.8969505670765));
#50799=CARTESIAN_POINT('',(27.328295268743,0.410451051658016,15.7235432561772));
#50800=CARTESIAN_POINT('',(27.3322214554001,0.435240018610828,33.8969505670765));
#50801=CARTESIAN_POINT('Origin',(27.3246823910029,0.423728682191396,33.891284862925));
#50802=CARTESIAN_POINT('',(27.3322214554001,0.435240018610828,15.7235432561772));
#50803=CARTESIAN_POINT('Origin',(27.2997094293662,0.212517476831317,15.7235432561772));
#50804=CARTESIAN_POINT('',(27.3062967880422,0.224586826676008,31.5905494329235));
#50805=CARTESIAN_POINT('',(27.3043276244395,0.199566230780642,31.5905494329235));
#50806=CARTESIAN_POINT('Origin',(27.2996841331102,0.212519467689854,31.5962151370755));
#50807=CARTESIAN_POINT('',(27.3043276244395,0.199566230780642,33.8969505670765));
#50808=CARTESIAN_POINT('',(27.3043276244395,0.199566230780642,15.7235432561772));
#50809=CARTESIAN_POINT('',(27.3062967880422,0.224586826676008,33.8969505670765));
#50810=CARTESIAN_POINT('Origin',(27.2996841331108,0.212519467689809,33.8912848629251));
#50811=CARTESIAN_POINT('',(27.3062967880422,0.224586826676008,15.7235432561772));
#50812=CARTESIAN_POINT('Origin',(27.2913595949605,1.54398896472578E-14,
15.7235432561772));
#50813=CARTESIAN_POINT('',(27.2969796967333,0.0125489822720319,31.5905494329235));
#50814=CARTESIAN_POINT('',(27.2969796967333,-0.0125489822720016,31.5905494329235));
#50815=CARTESIAN_POINT('Origin',(27.2913342204835,1.66533453693773E-14,
31.5962151370755));
#50816=CARTESIAN_POINT('',(27.2969796967333,-0.0125489822720016,33.8969505670765));
#50817=CARTESIAN_POINT('',(27.2969796967333,-0.0125489822720016,15.7235432561772));
#50818=CARTESIAN_POINT('',(27.2969796967333,0.0125489822720319,33.8969505670765));
#50819=CARTESIAN_POINT('Origin',(27.2913342204839,1.44047100636424E-14,
33.891284862925));
#50820=CARTESIAN_POINT('',(27.2969796967333,0.0125489822720319,15.7235432561772));
#50821=CARTESIAN_POINT('Origin',(27.5865837274296,1.22969701109861,15.7235432561772));
#50822=CARTESIAN_POINT('',(27.5972883935087,1.23832676336248,31.5905494329235));
#50823=CARTESIAN_POINT('',(27.5858941560429,1.2159643132099,31.5905494329235));
#50824=CARTESIAN_POINT('Origin',(27.586561118605,1.22970853087013,31.5962151370754));
#50825=CARTESIAN_POINT('',(27.5858941560429,1.2159643132099,33.8969505670765));
#50826=CARTESIAN_POINT('',(27.5858941560429,1.2159643132099,15.7235432561772));
#50827=CARTESIAN_POINT('',(27.5972883935087,1.23832676336248,33.8969505670765));
#50828=CARTESIAN_POINT('Origin',(27.5865611186055,1.22970853086989,33.891284862925));
#50829=CARTESIAN_POINT('',(27.5972883935087,1.23832676336248,15.7235432561772));
#50830=CARTESIAN_POINT('Origin',(27.690504399871,1.41526072396476,15.7235432561772));
#50831=CARTESIAN_POINT('',(27.701853149596,1.42302399516181,31.5905494329235));
#50832=CARTESIAN_POINT('',(27.6887394991445,1.40162446254803,31.5905494329235));
#50833=CARTESIAN_POINT('Origin',(27.6904827645727,1.41527398209261,31.5962151370755));
#50834=CARTESIAN_POINT('',(27.6887394991445,1.40162446254803,33.8969505670765));
#50835=CARTESIAN_POINT('',(27.6887394991445,1.40162446254803,15.7235432561772));
#50836=CARTESIAN_POINT('',(27.701853149596,1.42302399516181,33.8969505670765));
#50837=CARTESIAN_POINT('Origin',(27.6904827645732,1.41527398209234,33.891284862925));
#50838=CARTESIAN_POINT('',(27.701853149596,1.42302399516181,15.7235432561772));
#50839=CARTESIAN_POINT('Origin',(27.8086638806724,1.59209888384573,15.7235432561772));
#50840=CARTESIAN_POINT('',(27.8205867452275,1.59894781082746,31.5905494329235));
#50841=CARTESIAN_POINT('',(27.805834531806,1.57864313098712,31.5905494329235));
#50842=CARTESIAN_POINT('Origin',(27.8086433522893,1.59211379858911,31.5962151370755));
#50843=CARTESIAN_POINT('',(27.805834531806,1.57864313098712,33.8969505670765));
#50844=CARTESIAN_POINT('',(27.805834531806,1.57864313098712,15.7235432561772));
#50845=CARTESIAN_POINT('',(27.8205867452275,1.59894781082746,33.8969505670765));
#50846=CARTESIAN_POINT('Origin',(27.8086433522896,1.59211379858882,33.8912848629251));
#50847=CARTESIAN_POINT('',(27.8205867452275,1.59894781082746,15.7235432561772));
#50848=CARTESIAN_POINT('Origin',(27.9403336773427,1.75912122468118,15.7235432561772));
#50849=CARTESIAN_POINT('',(27.9527571483031,1.76501358153527,31.5905494329235));
#50850=CARTESIAN_POINT('',(27.9364573242129,1.74592893957157,31.5905494329235));
#50851=CARTESIAN_POINT('Origin',(27.9403143824389,1.75913770408581,31.5962151370755));
#50852=CARTESIAN_POINT('',(27.9364573242129,1.74592893957157,33.8969505670765));
#50853=CARTESIAN_POINT('',(27.9364573242129,1.74592893957157,15.7235432561772));
#50854=CARTESIAN_POINT('',(27.9527571483031,1.76501358153527,33.8969505670765));
#50855=CARTESIAN_POINT('Origin',(27.9403143824393,1.75913770408551,33.891284862925));
#50856=CARTESIAN_POINT('',(27.9527571483031,1.76501358153527,15.7235432561772));
#50857=CARTESIAN_POINT('Origin',(28.0847020018007,1.9152979981993,15.7235432561772));
#50858=CARTESIAN_POINT('',(28.0975494843367,1.92019745658633,31.5905494329235));
#50859=CARTESIAN_POINT('',(28.0798025434137,1.90245051566326,31.5905494329235));
#50860=CARTESIAN_POINT('Origin',(28.0846840593359,1.9153159406641,31.5962151370755));
#50861=CARTESIAN_POINT('',(28.0798025434137,1.90245051566326,33.8969505670765));
#50862=CARTESIAN_POINT('',(28.0798025434137,1.90245051566326,15.7235432561772));
#50863=CARTESIAN_POINT('',(28.0975494843367,1.92019745658633,33.8969505670765));
#50864=CARTESIAN_POINT('Origin',(28.0846840593363,1.91531594066375,33.891284862925));
#50865=CARTESIAN_POINT('',(28.0975494843367,1.92019745658633,15.7235432561772));
#50866=CARTESIAN_POINT('Origin',(28.2408787753188,2.05966632265731,15.7235432561772));
#50867=CARTESIAN_POINT('',(28.2540710604285,2.06354267578708,31.5905494329235));
#50868=CARTESIAN_POINT('',(28.2349864184648,2.0472428516969,31.5905494329235));
#50869=CARTESIAN_POINT('Origin',(28.2408622959143,2.05968561756092,31.5962151370754));
#50870=CARTESIAN_POINT('',(28.2349864184648,2.0472428516969,33.8969505670765));
#50871=CARTESIAN_POINT('',(28.2349864184648,2.0472428516969,15.7235432561772));
#50872=CARTESIAN_POINT('',(28.2540710604285,2.06354267578708,33.8969505670765));
#50873=CARTESIAN_POINT('Origin',(28.2408622959145,2.05968561756065,33.891284862925));
#50874=CARTESIAN_POINT('',(28.2540710604285,2.06354267578708,15.7235432561772));
#50875=CARTESIAN_POINT('Origin',(28.4079011161543,2.19133611932758,15.7235432561772));
#50876=CARTESIAN_POINT('',(28.4213568690129,2.19416546819404,31.5905494329235));
#50877=CARTESIAN_POINT('',(28.4010521891726,2.1794132547725,31.5905494329235));
#50878=CARTESIAN_POINT('Origin',(28.407886201411,2.19135664771063,31.5962151370753));
#50879=CARTESIAN_POINT('',(28.4010521891726,2.1794132547725,33.8969505670765));
#50880=CARTESIAN_POINT('',(28.4010521891726,2.1794132547725,15.7235432561772));
#50881=CARTESIAN_POINT('',(28.4213568690129,2.19416546819404,33.8969505670765));
#50882=CARTESIAN_POINT('Origin',(28.4078862014112,2.19135664771024,33.8912848629252));
#50883=CARTESIAN_POINT('',(28.4213568690129,2.19416546819404,15.7235432561772));
#50884=CARTESIAN_POINT('Origin',(28.5847392760353,2.309495600129,15.7235432561772));
#50885=CARTESIAN_POINT('',(28.598375537452,2.31126050085552,31.5905494329235));
#50886=CARTESIAN_POINT('',(28.5769760048382,2.29814685040398,31.5905494329235));
#50887=CARTESIAN_POINT('Origin',(28.5847260179075,2.30951723542729,31.5962151370754));
#50888=CARTESIAN_POINT('',(28.5769760048382,2.29814685040398,33.8969505670765));
#50889=CARTESIAN_POINT('',(28.5769760048382,2.29814685040398,15.7235432561772));
#50890=CARTESIAN_POINT('',(28.598375537452,2.31126050085552,33.8969505670765));
#50891=CARTESIAN_POINT('Origin',(28.5847260179077,2.30951723542689,33.891284862925));
#50892=CARTESIAN_POINT('',(28.598375537452,2.31126050085552,15.7235432561772));
#50893=CARTESIAN_POINT('Origin',(28.7703029889014,2.4134162725704,15.7235432561772));
#50894=CARTESIAN_POINT('',(28.7840356867901,2.41410584395713,31.5905494329235));
#50895=CARTESIAN_POINT('',(28.7616732366375,2.40271160649133,31.5905494329235));
#50896=CARTESIAN_POINT('Origin',(28.7702914691299,2.41343888139489,31.5962151370753));
#50897=CARTESIAN_POINT('',(28.7616732366375,2.40271160649133,33.8969505670765));
#50898=CARTESIAN_POINT('',(28.7616732366375,2.40271160649133,15.7235432561772));
#50899=CARTESIAN_POINT('',(28.7840356867901,2.41410584395713,33.8969505670765));
#50900=CARTESIAN_POINT('Origin',(28.7702914691301,2.41343888139455,33.8912848629251));
#50901=CARTESIAN_POINT('',(28.7840356867901,2.41410584395713,15.7235432561772));
#50902=CARTESIAN_POINT('Origin',(30.,-1.32966554433622E-14,34.));
#50903=CARTESIAN_POINT('',(28.75,0.721687836487017,33.8917468245269));
#50904=CARTESIAN_POINT('',(28.75,-1.44824191072421E-14,33.6983711515529));
#50905=CARTESIAN_POINT('Ctrl Pts',(28.75,0.72168783648698,33.8917468245269));
#50906=CARTESIAN_POINT('Ctrl Pts',(28.75,0.334936490538873,33.6983711515529));
#50907=CARTESIAN_POINT('Ctrl Pts',(28.75,-1.55145598201422E-14,33.6983711515529));
#50908=CARTESIAN_POINT('',(30.,1.44337567297405,33.8917468245269));
#50909=CARTESIAN_POINT('Ctrl Pts',(30.,1.44337567297404,33.8917468245269));
#50910=CARTESIAN_POINT('Ctrl Pts',(29.375,1.08253175473053,33.5309029062834));
#50911=CARTESIAN_POINT('Ctrl Pts',(28.75,0.721687836487025,33.8917468245269));
#50912=CARTESIAN_POINT('',(31.25,0.721687836487017,33.891746824527));
#50913=CARTESIAN_POINT('Ctrl Pts',(31.25,0.721687836487027,33.8917468245269));
#50914=CARTESIAN_POINT('Ctrl Pts',(30.625,1.08253175473053,33.5309029062834));
#50915=CARTESIAN_POINT('Ctrl Pts',(30.,1.44337567297404,33.8917468245269));
#50916=CARTESIAN_POINT('',(31.25,-0.72168783648704,33.8917468245269));
#50917=CARTESIAN_POINT('Ctrl Pts',(31.25,-0.721687836487026,33.8917468245269));
#50918=CARTESIAN_POINT('Ctrl Pts',(31.25,-1.26287869051112E-14,33.5309029062834));
#50919=CARTESIAN_POINT('Ctrl Pts',(31.25,0.721687836487001,33.8917468245269));
#50920=CARTESIAN_POINT('',(30.,-1.44337567297407,33.8917468245269));
#50921=CARTESIAN_POINT('Ctrl Pts',(30.,-1.44337567297406,33.8917468245269));
#50922=CARTESIAN_POINT('Ctrl Pts',(30.625,-1.08253175473056,33.5309029062834));
#50923=CARTESIAN_POINT('Ctrl Pts',(31.25,-0.721687836487049,33.8917468245269));
#50924=CARTESIAN_POINT('',(28.75,-0.721687836487044,33.8917468245269));
#50925=CARTESIAN_POINT('Ctrl Pts',(28.75,-0.721687836487053,33.8917468245269));
#50926=CARTESIAN_POINT('Ctrl Pts',(29.375,-1.08253175473056,33.5309029062834));
#50927=CARTESIAN_POINT('Ctrl Pts',(30.,-1.44337567297406,33.8917468245269));
#50928=CARTESIAN_POINT('Ctrl Pts',(28.75,-1.55145598201422E-14,33.6983711515529));
#50929=CARTESIAN_POINT('Ctrl Pts',(28.75,-0.334936490538901,33.6983711515529));
#50930=CARTESIAN_POINT('Ctrl Pts',(28.75,-0.721687836487005,33.8917468245269));
#50931=CARTESIAN_POINT('',(28.4483711515529,-1.34873480853811E-14,34.));
#50932=CARTESIAN_POINT('',(28.4483711515529,-1.34873480853811E-14,34.));
#50933=CARTESIAN_POINT('Origin',(30.,-1.32966554433622E-14,34.));
#50934=CARTESIAN_POINT('Origin',(30.,-1.32966554433622E-14,33.953125));
#50935=CARTESIAN_POINT('',(30.,-2.6137293696319,33.9862706303681));
#50936=CARTESIAN_POINT('Origin',(30.,-1.32966554433622E-14,33.9862706303681));
#50937=CARTESIAN_POINT('',(30.,-2.58058373926378,34.));
#50938=CARTESIAN_POINT('Origin',(30.,-2.58058373926378,33.953125));
#50939=CARTESIAN_POINT('Origin',(30.,-1.32966554433622E-14,34.));
#50940=CARTESIAN_POINT('Origin',(30.,-1.32966554433622E-14,33.8637293696319));
#50941=CARTESIAN_POINT('',(30.012548982272,-2.70302030326669,33.8969505670765));
#50942=CARTESIAN_POINT('',(30.,-2.69489040503949,33.9051095949605));
#50943=CARTESIAN_POINT('Ctrl Pts',(30.012548982272,-2.70302030326672,33.8969505670765));
#50944=CARTESIAN_POINT('Ctrl Pts',(30.0117595027242,-2.70125749446881,33.8987170220581));
#50945=CARTESIAN_POINT('Ctrl Pts',(30.0105608813139,-2.69960157002983,33.9003782103613));
#50946=CARTESIAN_POINT('Ctrl Pts',(30.0079476416933,-2.69733049287042,33.9026580100842));
#50947=CARTESIAN_POINT('Ctrl Pts',(30.0065751610721,-2.69644647069985,33.9035459832655));
#50948=CARTESIAN_POINT('Ctrl Pts',(30.0034509360646,-2.69522714758869,33.9047710768107));
#50949=CARTESIAN_POINT('Ctrl Pts',(30.0017003028408,-2.69489040503949,33.9051095949605));
#50950=CARTESIAN_POINT('Ctrl Pts',(30.,-2.69489040503949,33.9051095949605));
#50951=CARTESIAN_POINT('',(30.027378900953,-2.73613365141358,33.8637293696319));
#50952=CARTESIAN_POINT('Ctrl Pts',(30.0273789009518,-2.73613365141079,33.8637293696347));
#50953=CARTESIAN_POINT('Ctrl Pts',(30.019918653996,-2.71947585577342,33.8804609779984));
#50954=CARTESIAN_POINT('Ctrl Pts',(30.0125489822686,-2.70302030325915,33.8969505670841));
#50955=CARTESIAN_POINT('',(30.1873800711417,-2.72984718831552,33.8637293696319));
#50956=CARTESIAN_POINT('Origin',(30.,-1.32966554433622E-14,33.8637293696319));
#50957=CARTESIAN_POINT('',(30.1995662307806,-2.69567237556051,33.8969505670765));
#50958=CARTESIAN_POINT('Ctrl Pts',(30.1995662307834,-2.69567237555272,33.8969505670841));
#50959=CARTESIAN_POINT('Ctrl Pts',(30.1935103650644,-2.71265541886991,33.8804609779983));
#50960=CARTESIAN_POINT('Ctrl Pts',(30.1873800711428,-2.72984718831265,33.8637293696347));
#50961=CARTESIAN_POINT('',(30.224586826676,-2.69370321195777,33.8969505670765));
#50962=CARTESIAN_POINT('Origin',(30.2125187883694,-2.70030745889015,33.8912937927563));
#50963=CARTESIAN_POINT('',(30.241969073019,-2.72555094069392,33.8637293696319));
#50964=CARTESIAN_POINT('Ctrl Pts',(30.2419690730176,-2.72555094069121,33.8637293696347));
#50965=CARTESIAN_POINT('Ctrl Pts',(30.233224867931,-2.70952981970859,33.8804609779984));
#50966=CARTESIAN_POINT('Ctrl Pts',(30.2245868266721,-2.69370321195052,33.8969505670841));
#50967=CARTESIAN_POINT('',(30.4009837827878,-2.70673030953518,33.8637293696319));
#50968=CARTESIAN_POINT('Origin',(30.,-1.32966554433622E-14,33.8637293696319));
#50969=CARTESIAN_POINT('',(30.410451051658,-2.67170473125697,33.8969505670765));
#50970=CARTESIAN_POINT('Ctrl Pts',(30.4104510516601,-2.67170473124899,33.8969505670841));
#50971=CARTESIAN_POINT('Ctrl Pts',(30.4057463283755,-2.68911055925959,33.8804609779983));
#50972=CARTESIAN_POINT('Ctrl Pts',(30.4009837827886,-2.70673030953223,33.8637293696347));
#50973=CARTESIAN_POINT('',(30.4352400186108,-2.66777854459992,33.8969505670765));
#50974=CARTESIAN_POINT('Origin',(30.4237273077484,-2.67530902338216,33.8912940899387));
#50975=CARTESIAN_POINT('',(30.455067425287,-2.69816430208722,33.8637293696319));
#50976=CARTESIAN_POINT('Ctrl Pts',(30.4550674252854,-2.69816430208464,33.8637293696347));
#50977=CARTESIAN_POINT('Ctrl Pts',(30.445093173,-2.68287863129519,33.8804609779983));
#50978=CARTESIAN_POINT('Ctrl Pts',(30.4352400186063,-2.667778544593,33.8969505670841));
#50979=CARTESIAN_POINT('',(30.6121152960723,-2.66692553831739,33.8637293696319));
#50980=CARTESIAN_POINT('Origin',(30.,-1.32966554433622E-14,33.8637293696319));
#50981=CARTESIAN_POINT('',(30.618805305313,-2.63126513885325,33.8969505670765));
#50982=CARTESIAN_POINT('Ctrl Pts',(30.6188053053145,-2.63126513884514,33.8969505670841));
#50983=CARTESIAN_POINT('Ctrl Pts',(30.6154807306477,-2.64898643883144,33.8804609779984));
#50984=CARTESIAN_POINT('Ctrl Pts',(30.6121152960728,-2.66692553831439,33.8637293696347));
#50985=CARTESIAN_POINT('',(30.6432098110989,-2.62540613538822,33.8969505670765));
#50986=CARTESIAN_POINT('Origin',(30.6323233823986,-2.63381649164655,33.8912943077151));
#50987=CARTESIAN_POINT('',(30.6653601355529,-2.65414258332748,33.8637293696319));
#50988=CARTESIAN_POINT('Ctrl Pts',(30.665360135551,-2.65414258332505,33.8637293696347));
#50989=CARTESIAN_POINT('Ctrl Pts',(30.6542173306489,-2.63968660397218,33.8804609779983));
#50990=CARTESIAN_POINT('Ctrl Pts',(30.6432098110939,-2.62540613538168,33.8969505670841));
#50991=CARTESIAN_POINT('',(30.8194729150075,-2.61067828431314,33.8637293696319));
#50992=CARTESIAN_POINT('Origin',(30.,-1.32966554433622E-14,33.8637293696319));
#50993=CARTESIAN_POINT('',(30.8233444184872,-2.57460292188405,33.8969505670765));
#50994=CARTESIAN_POINT('Ctrl Pts',(30.8233444184881,-2.57460292187584,33.8969505670841));
#50995=CARTESIAN_POINT('Ctrl Pts',(30.8214204895475,-2.59253043613051,33.8804609779984));
#50996=CARTESIAN_POINT('Ctrl Pts',(30.8194729150079,-2.61067828431011,33.8637293696347));
#50997=CARTESIAN_POINT('',(30.8472140012126,-2.56684722431573,33.8969505670765));
#50998=CARTESIAN_POINT('Origin',(30.837020957759,-2.57608565616367,33.891294472568));
#50999=CARTESIAN_POINT('',(30.8715506793283,-2.59375719294955,33.8637293696319));
#51000=CARTESIAN_POINT('Ctrl Pts',(30.8715506793263,-2.59375719294726,33.8637293696347));
#51001=CARTESIAN_POINT('Ctrl Pts',(30.8593080209051,-2.58022003095079,33.8804609779983));
#51002=CARTESIAN_POINT('Ctrl Pts',(30.8472140012071,-2.5668472243096,33.8969505670841));
#51003=CARTESIAN_POINT('',(31.0217782109194,-2.53833533054748,33.8637293696319));
#51004=CARTESIAN_POINT('Origin',(30.,-1.32966554433622E-14,33.8637293696319));
#51005=CARTESIAN_POINT('',(31.0228073395316,-2.5020674217591,33.8969505670765));
#51006=CARTESIAN_POINT('Ctrl Pts',(31.0228073395319,-2.50206742175084,33.8969505670841));
#51007=CARTESIAN_POINT('Ctrl Pts',(31.0222959179792,-2.52009062118698,33.8804609779983));
#51008=CARTESIAN_POINT('Ctrl Pts',(31.0217782109195,-2.53833533054442,33.8637293696347));
#51009=CARTESIAN_POINT('',(31.0459948352815,-2.49246284654201,33.8969505670765));
#51010=CARTESIAN_POINT('Origin',(31.0365580110689,-2.50247243285094,33.8912946002427));
#51011=CARTESIAN_POINT('',(31.0723678233457,-2.51738042696529,33.8637293696319));
#51012=CARTESIAN_POINT('Ctrl Pts',(31.0723678233435,-2.51738042696321,33.8637293696347));
#51013=CARTESIAN_POINT('Ctrl Pts',(31.0591007914634,-2.5048455434284,33.8804609779984));
#51014=CARTESIAN_POINT('Ctrl Pts',(31.0459948352755,-2.49246284653634,33.8969505670841));
#51015=CARTESIAN_POINT('',(31.2177839043851,-2.45034269538684,33.8637293696319));
#51016=CARTESIAN_POINT('Origin',(30.,-1.32966554433622E-14,33.8637293696319));
#51017=CARTESIAN_POINT('',(31.2159643132098,-2.41410584395714,33.8969505670765));
#51018=CARTESIAN_POINT('Ctrl Pts',(31.2159643132094,-2.4141058439489,33.8969505670841));
#51019=CARTESIAN_POINT('Ctrl Pts',(31.2168685521286,-2.43211360954869,33.8804609779984));
#51020=CARTESIAN_POINT('Ctrl Pts',(31.2177839043849,-2.4503426953838,33.8637293696347));
#51021=CARTESIAN_POINT('',(31.2383267633624,-2.40271160649135,33.8969505670765));
#51022=CARTESIAN_POINT('Origin',(31.2297043338602,-2.41343066267494,33.891294700665));
#51023=CARTESIAN_POINT('',(31.2665734631337,-2.42548317353486,33.8637293696319));
#51024=CARTESIAN_POINT('Ctrl Pts',(31.2665734631313,-2.42548317353296,33.8637293696347));
#51025=CARTESIAN_POINT('Ctrl Pts',(31.2523638534557,-2.41402785018508,33.8804609779983));
#51026=CARTESIAN_POINT('Ctrl Pts',(31.238326763356,-2.40271160648617,33.8969505670841));
#51027=CARTESIAN_POINT('',(31.4062815551261,-2.34724288268751,33.8637293696319));
#51028=CARTESIAN_POINT('Origin',(30.,-1.32966554433622E-14,33.8637293696319));
#51029=CARTESIAN_POINT('',(31.401624462548,-2.31126050085554,33.8969505670765));
#51030=CARTESIAN_POINT('Ctrl Pts',(31.4016244625469,-2.31126050084735,33.8969505670841));
#51031=CARTESIAN_POINT('Ctrl Pts',(31.4039387870044,-2.32914180874765,33.8804609779983));
#51032=CARTESIAN_POINT('Ctrl Pts',(31.4062815551258,-2.34724288268448,33.8637293696347));
#51033=CARTESIAN_POINT('',(31.4230239951618,-2.29814685040399,33.8969505670765));
#51034=CARTESIAN_POINT('Origin',(31.4152691174526,-2.30950931155476,33.8912947803757));
#51035=CARTESIAN_POINT('',(31.452970256343,-2.31863200978458,33.8637293696319));
#51036=CARTESIAN_POINT('Ctrl Pts',(31.4529702563405,-2.31863200978284,33.8637293696347));
#51037=CARTESIAN_POINT('Ctrl Pts',(31.4379056758382,-2.30832687249962,33.8804609779984));
#51038=CARTESIAN_POINT('Ctrl Pts',(31.423023995155,-2.29814685039932,33.8969505670841));
#51039=CARTESIAN_POINT('',(31.5861090124437,-2.22967153707895,33.8637293696319));
#51040=CARTESIAN_POINT('Origin',(30.,-1.32966554433622E-14,33.8637293696319));
#51041=CARTESIAN_POINT('',(31.5786431309871,-2.19416546819406,33.8969505670765));
#51042=CARTESIAN_POINT('Ctrl Pts',(31.5786431309854,-2.19416546818597,33.8969505670841));
#51043=CARTESIAN_POINT('Ctrl Pts',(31.5823532724012,-2.21181007417745,33.8804609779984));
#51044=CARTESIAN_POINT('Ctrl Pts',(31.5861090124431,-2.22967153707596,33.8637293696347));
#51045=CARTESIAN_POINT('',(31.5989478108274,-2.17941325477251,33.8969505670765));
#51046=CARTESIAN_POINT('Origin',(31.5921082951429,-2.19134908471607,33.891294843835));
#51047=CARTESIAN_POINT('',(31.6304090047603,-2.1974857086706,33.8637293696319));
#51048=CARTESIAN_POINT('Ctrl Pts',(31.6304090047577,-2.19748570866908,33.8637293696347));
#51049=CARTESIAN_POINT('Ctrl Pts',(31.6145823315769,-2.18839429204867,33.8804609779984));
#51050=CARTESIAN_POINT('Ctrl Pts',(31.5989478108202,-2.1794132547684,33.8969505670841));
#51051=CARTESIAN_POINT('',(31.7561575802648,-2.09835352500328,33.8637293696319));
#51052=CARTESIAN_POINT('Origin',(30.,-1.32966554433622E-14,33.8637293696319));
#51053=CARTESIAN_POINT('',(31.7459289395715,-2.0635426757871,33.8969505670765));
#51054=CARTESIAN_POINT('Ctrl Pts',(31.7459289395692,-2.06354267577917,33.8969505670841));
#51055=CARTESIAN_POINT('Ctrl Pts',(31.7510120236878,-2.08084179499847,33.8804609779983));
#51056=CARTESIAN_POINT('Ctrl Pts',(31.7561575802639,-2.09835352500035,33.8637293696347));
#51057=CARTESIAN_POINT('',(31.7650135815352,-2.04724285169692,33.8969505670765));
#51058=CARTESIAN_POINT('Origin',(31.7591315960217,-2.05967847590834,33.8912948941586));
#51059=CARTESIAN_POINT('',(31.7977957394973,-2.06279117742452,33.8637293696319));
#51060=CARTESIAN_POINT('Ctrl Pts',(31.7977957394945,-2.06279117742322,33.8637293696347));
#51061=CARTESIAN_POINT('Ctrl Pts',(31.7813045503384,-2.05496953307228,33.8804609779984));
#51062=CARTESIAN_POINT('Ctrl Pts',(31.7650135815277,-2.04724285169338,33.8969505670841));
#51063=CARTESIAN_POINT('',(31.9153788526219,-1.9540984656726,33.8637293696319));
#51064=CARTESIAN_POINT('Origin',(30.,-1.32966554433622E-14,33.8637293696319));
#51065=CARTESIAN_POINT('',(31.9024505156632,-1.92019745658634,33.8969505670765));
#51066=CARTESIAN_POINT('Ctrl Pts',(31.9024505156603,-1.92019745657863,33.8969505670841));
#51067=CARTESIAN_POINT('Ctrl Pts',(31.9088752035777,-1.93704443420321,33.8804609779984));
#51068=CARTESIAN_POINT('Ctrl Pts',(31.9153788526208,-1.95409846566976,33.8637293696347));
#51069=CARTESIAN_POINT('',(31.9201974565863,-1.90245051566327,33.8969505670765));
#51070=CARTESIAN_POINT('Origin',(31.9153092670123,-1.91530927561705,33.891294933562));
#51071=CARTESIAN_POINT('',(31.9540984656725,-1.91537885262194,33.8637293696319));
#51072=CARTESIAN_POINT('Ctrl Pts',(31.9540984656697,-1.91537885262084,33.8637293696347));
#51073=CARTESIAN_POINT('Ctrl Pts',(31.9370444342032,-1.90887520357777,33.8804609779984));
#51074=CARTESIAN_POINT('Ctrl Pts',(31.9201974565786,-1.90245051566033,33.8969505670841));
#51075=CARTESIAN_POINT('',(32.0627911774245,-1.79779573949737,33.8637293696319));
#51076=CARTESIAN_POINT('Origin',(30.,-1.32966554433622E-14,33.8637293696319));
#51077=CARTESIAN_POINT('',(32.0472428516969,-1.76501358153528,33.8969505670765));
#51078=CARTESIAN_POINT('Ctrl Pts',(32.0472428516934,-1.76501358152781,33.8969505670841));
#51079=CARTESIAN_POINT('Ctrl Pts',(32.0549695330723,-1.78130455033843,33.8804609779983));
#51080=CARTESIAN_POINT('Ctrl Pts',(32.0627911774232,-1.7977957394946,33.8637293696347));
#51081=CARTESIAN_POINT('',(32.063542675787,-1.74592893957158,33.8969505670765));
#51082=CARTESIAN_POINT('Origin',(32.0596784217459,-1.75913156587025,33.8912949636253));
#51083=CARTESIAN_POINT('',(32.0983535250032,-1.75615758026484,33.8637293696319));
#51084=CARTESIAN_POINT('Ctrl Pts',(32.0983535250003,-1.75615758026399,33.8637293696347));
#51085=CARTESIAN_POINT('Ctrl Pts',(32.0808417949984,-1.75101202368781,33.8804609779984));
#51086=CARTESIAN_POINT('Ctrl Pts',(32.0635426757791,-1.74592893956926,33.8969505670841));
#51087=CARTESIAN_POINT('',(32.1974857086705,-1.63040900476039,33.8637293696319));
#51088=CARTESIAN_POINT('Origin',(30.,-1.32966554433622E-14,33.8637293696319));
#51089=CARTESIAN_POINT('',(32.1794132547725,-1.59894781082747,33.8969505670765));
#51090=CARTESIAN_POINT('Ctrl Pts',(32.1794132547683,-1.59894781082035,33.8969505670841));
#51091=CARTESIAN_POINT('Ctrl Pts',(32.1883942920486,-1.61458233157699,33.8804609779984));
#51092=CARTESIAN_POINT('Ctrl Pts',(32.197485708669,-1.63040900475776,33.8637293696347));
#51093=CARTESIAN_POINT('',(32.194165468194,-1.57864313098713,33.8969505670765));
#51094=CARTESIAN_POINT('Origin',(32.1913489771416,-1.59210823242541,33.8912949854673));
#51095=CARTESIAN_POINT('',(32.2296715370789,-1.58610901244375,33.8637293696319));
#51096=CARTESIAN_POINT('Ctrl Pts',(32.2296715370759,-1.58610901244313,33.8637293696347));
#51097=CARTESIAN_POINT('Ctrl Pts',(32.2118100741774,-1.58235327240121,33.8804609779984));
#51098=CARTESIAN_POINT('Ctrl Pts',(32.1941654681859,-1.57864313098543,33.8969505670841));
#51099=CARTESIAN_POINT('',(32.3186320097845,-1.45297025634306,33.8637293696319));
#51100=CARTESIAN_POINT('Origin',(30.,-1.32966554433622E-14,33.8637293696319));
#51101=CARTESIAN_POINT('',(32.2981468504039,-1.42302399516182,33.8969505670765));
#51102=CARTESIAN_POINT('Ctrl Pts',(32.2981468503993,-1.42302399515499,33.8969505670841));
#51103=CARTESIAN_POINT('Ctrl Pts',(32.3083268724996,-1.4379056758382,33.8804609779984));
#51104=CARTESIAN_POINT('Ctrl Pts',(32.3186320097828,-1.45297025634053,33.8637293696347));
#51105=CARTESIAN_POINT('',(32.3112605008555,-1.40162446254804,33.8969505670765));
#51106=CARTESIAN_POINT('Origin',(32.3095091411127,-1.41526902814879,33.891294999854));
#51107=CARTESIAN_POINT('',(32.3472428826875,-1.40628155512619,33.8637293696319));
#51108=CARTESIAN_POINT('Ctrl Pts',(32.3472428826845,-1.4062815551258,33.8637293696347));
#51109=CARTESIAN_POINT('Ctrl Pts',(32.3291418087476,-1.4039387870044,33.8804609779983));
#51110=CARTESIAN_POINT('Ctrl Pts',(32.3112605008473,-1.40162446254698,33.8969505670841));
#51111=CARTESIAN_POINT('',(32.4254831735348,-1.26657346313373,33.8637293696319));
#51112=CARTESIAN_POINT('Origin',(30.,-1.32966554433622E-14,33.8637293696319));
#51113=CARTESIAN_POINT('',(32.4027116064913,-1.2383267633625,33.8969505670765));
#51114=CARTESIAN_POINT('Ctrl Pts',(32.4027116064861,-1.23832676335608,33.8969505670841));
#51115=CARTESIAN_POINT('Ctrl Pts',(32.414027850185,-1.25236385345577,33.8804609779983));
#51116=CARTESIAN_POINT('Ctrl Pts',(32.4254831735329,-1.26657346313137,33.8637293696347));
#51117=CARTESIAN_POINT('',(32.4141058439571,-1.21596431320991,33.8969505670765));
#51118=CARTESIAN_POINT('Origin',(32.4134304175703,-1.22970422416536,33.8912950072666));
#51119=CARTESIAN_POINT('',(32.4503426953868,-1.21778390438519,33.8637293696319));
#51120=CARTESIAN_POINT('Ctrl Pts',(32.4503426953838,-1.21778390438504,33.8637293696347));
#51121=CARTESIAN_POINT('Ctrl Pts',(32.4321136095486,-1.21686855212869,33.8804609779984));
#51122=CARTESIAN_POINT('Ctrl Pts',(32.4141058439489,-1.2159643132095,33.8969505670841));
#51123=CARTESIAN_POINT('',(32.5173804269652,-1.07236782334576,33.8637293696319));
#51124=CARTESIAN_POINT('Origin',(30.,-1.32966554433622E-14,33.8637293696319));
#51125=CARTESIAN_POINT('',(32.492462846542,-1.0459948352816,33.8969505670765));
#51126=CARTESIAN_POINT('Ctrl Pts',(32.4924628465363,-1.04599483527564,33.8969505670841));
#51127=CARTESIAN_POINT('Ctrl Pts',(32.5048455434283,-1.05910079146353,33.8804609779984));
#51128=CARTESIAN_POINT('Ctrl Pts',(32.5173804269631,-1.07236782334356,33.8637293696347));
#51129=CARTESIAN_POINT('',(32.5020674217591,-1.02280733953168,33.8969505670765));
#51130=CARTESIAN_POINT('Origin',(32.5024720978725,-1.03655788791108,33.8912950079413));
#51131=CARTESIAN_POINT('',(32.5383353305474,-1.02177821091943,33.8637293696319));
#51132=CARTESIAN_POINT('Ctrl Pts',(32.5383353305444,-1.02177821091952,33.8637293696347));
#51133=CARTESIAN_POINT('Ctrl Pts',(32.5200906211869,-1.02229591797926,33.8804609779983));
#51134=CARTESIAN_POINT('Ctrl Pts',(32.5020674217508,-1.02280733953191,33.8969505670841));
#51135=CARTESIAN_POINT('',(32.5937571929495,-0.871550679328387,33.8637293696319));
#51136=CARTESIAN_POINT('Origin',(30.,-1.32966554433622E-14,33.8637293696319));
#51137=CARTESIAN_POINT('',(32.5668472243157,-0.847214001212625,33.8969505670765));
#51138=CARTESIAN_POINT('Ctrl Pts',(32.5668472243096,-0.847214001207098,
33.8969505670841));
#51139=CARTESIAN_POINT('Ctrl Pts',(32.5802200309508,-0.859308020905142,
33.8804609779983));
#51140=CARTESIAN_POINT('Ctrl Pts',(32.5937571929472,-0.871550679326345,
33.8637293696347));
#51141=CARTESIAN_POINT('',(32.574602921884,-0.823344418487278,33.8969505670765));
#51142=CARTESIAN_POINT('Origin',(32.5760852110325,-0.837020829522246,33.8912950018862));
#51143=CARTESIAN_POINT('',(32.6106782843131,-0.819472915007605,33.8637293696319));
#51144=CARTESIAN_POINT('Ctrl Pts',(32.6106782843101,-0.819472915007929,
33.8637293696347));
#51145=CARTESIAN_POINT('Ctrl Pts',(32.5925304361305,-0.821420489547588,
33.8804609779984));
#51146=CARTESIAN_POINT('Ctrl Pts',(32.5746029218758,-0.823344418488157,
33.8969505670841));
#51147=CARTESIAN_POINT('',(32.6541425833274,-0.665360135552938,33.8637293696319));
#51148=CARTESIAN_POINT('Origin',(30.,-1.32966554433622E-14,33.8637293696319));
#51149=CARTESIAN_POINT('',(32.6254061353882,-0.643209811098926,33.8969505670765));
#51150=CARTESIAN_POINT('Ctrl Pts',(32.6254061353816,-0.643209811093906,
33.8969505670841));
#51151=CARTESIAN_POINT('Ctrl Pts',(32.6396866039721,-0.65421733064898,33.8804609779984));
#51152=CARTESIAN_POINT('Ctrl Pts',(32.654142583325,-0.665360135551083,33.8637293696347));
#51153=CARTESIAN_POINT('',(32.6312651388532,-0.6188053053131,33.8969505670765));
#51154=CARTESIAN_POINT('Origin',(32.633815908334,-0.632323260043048,33.8912949888765));
#51155=CARTESIAN_POINT('',(32.6669255383174,-0.612115296072366,33.8637293696319));
#51156=CARTESIAN_POINT('Ctrl Pts',(32.6669255383144,-0.612115296072921,
33.8637293696347));
#51157=CARTESIAN_POINT('Ctrl Pts',(32.6489864388314,-0.615480730647825,
33.8804609779983));
#51158=CARTESIAN_POINT('Ctrl Pts',(32.6312651388451,-0.618805305314621,
33.8969505670841));
#51159=CARTESIAN_POINT('',(32.6981643020872,-0.455067425287109,33.8637293696319));
#51160=CARTESIAN_POINT('Origin',(30.,-1.32966554433622E-14,33.8637293696319));
#51161=CARTESIAN_POINT('',(32.6677785445999,-0.435240018610835,33.8969505670765));
#51162=CARTESIAN_POINT('Ctrl Pts',(32.667778544593,-0.43524001860635,33.8969505670841));
#51163=CARTESIAN_POINT('Ctrl Pts',(32.6828786312952,-0.445093173000037,
33.8804609779984));
#51164=CARTESIAN_POINT('Ctrl Pts',(32.6981643020846,-0.45506742528547,33.8637293696347));
#51165=CARTESIAN_POINT('',(32.6717047312569,-0.410451051658023,33.8969505670765));
#51166=CARTESIAN_POINT('Origin',(32.6753082614924,-0.423727206709312,33.8912949684251));
#51167=CARTESIAN_POINT('',(32.7067303095351,-0.400983782787849,33.8637293696319));
#51168=CARTESIAN_POINT('Ctrl Pts',(32.7067303095322,-0.400983782788643,
33.8637293696347));
#51169=CARTESIAN_POINT('Ctrl Pts',(32.6891105592595,-0.405746328375509,
33.8804609779984));
#51170=CARTESIAN_POINT('Ctrl Pts',(32.6717047312489,-0.410451051660171,
33.8969505670841));
#51171=CARTESIAN_POINT('',(32.7255509406939,-0.241969073019109,33.8637293696319));
#51172=CARTESIAN_POINT('Origin',(30.,-1.32966554433622E-14,33.8637293696319));
#51173=CARTESIAN_POINT('',(32.6937032119577,-0.224586826676015,33.8969505670765));
#51174=CARTESIAN_POINT('Ctrl Pts',(32.6937032119505,-0.224586826672072,
33.8969505670841));
#51175=CARTESIAN_POINT('Ctrl Pts',(32.7095298197086,-0.233224867931026,
33.8804609779984));
#51176=CARTESIAN_POINT('Ctrl Pts',(32.7255509406912,-0.241969073017673,
33.8637293696347));
#51177=CARTESIAN_POINT('',(32.6956723755605,-0.199566230780649,33.8969505670765));
#51178=CARTESIAN_POINT('Origin',(32.7003064571198,-0.212518732061269,33.8912949397143));
#51179=CARTESIAN_POINT('',(32.7298471883155,-0.187380071141808,33.8637293696319));
#51180=CARTESIAN_POINT('Ctrl Pts',(32.7298471883126,-0.187380071142835,
33.8637293696347));
#51181=CARTESIAN_POINT('Ctrl Pts',(32.7126554188699,-0.19351036506442,33.8804609779983));
#51182=CARTESIAN_POINT('Ctrl Pts',(32.6956723755527,-0.199566230783424,
33.8969505670841));
#51183=CARTESIAN_POINT('',(32.7361336514135,-0.0273789009530657,33.8637293696319));
#51184=CARTESIAN_POINT('Origin',(30.,-1.32966554433622E-14,33.8637293696319));
#51185=CARTESIAN_POINT('',(32.7030203032667,-0.0125489822720396,33.8969505670765));
#51186=CARTESIAN_POINT('Ctrl Pts',(32.7030203032592,-0.0125489822686859,
33.8969505670841));
#51187=CARTESIAN_POINT('Ctrl Pts',(32.7194758557734,-0.0199186539960853,
33.8804609779984));
#51188=CARTESIAN_POINT('Ctrl Pts',(32.7361336514107,-0.0273789009518218,
33.8637293696347));
#51189=CARTESIAN_POINT('',(32.7030203032667,0.0125489822719939,33.8969505670765));
#51190=CARTESIAN_POINT('Origin',(32.7086563646857,-6.24428584025816E-9,
33.8912949140187));
#51191=CARTESIAN_POINT('',(32.7361336514135,0.0273789009530202,33.8637293696319));
#51192=CARTESIAN_POINT('Ctrl Pts',(32.7361336514108,0.027378900951751,33.8637293696347));
#51193=CARTESIAN_POINT('Ctrl Pts',(32.7194758557734,0.0199186539960142,
33.8804609779984));
#51194=CARTESIAN_POINT('Ctrl Pts',(32.7030203032592,0.0125489822686146,
33.8969505670841));
#51195=CARTESIAN_POINT('',(32.7298471883155,0.187380071141762,33.8637293696319));
#51196=CARTESIAN_POINT('Origin',(30.,-1.32966554433622E-14,33.8637293696319));
#51197=CARTESIAN_POINT('',(32.6956723755605,0.199566230780603,33.8969505670765));
#51198=CARTESIAN_POINT('Ctrl Pts',(32.6956723755527,0.199566230783364,33.8969505670841));
#51199=CARTESIAN_POINT('Ctrl Pts',(32.7126554188699,0.193510365064359,33.8804609779983));
#51200=CARTESIAN_POINT('Ctrl Pts',(32.7298471883126,0.187380071142775,33.8637293696347));
#51201=CARTESIAN_POINT('',(32.6937032119577,0.224586826675969,33.8969505670765));
#51202=CARTESIAN_POINT('Origin',(32.7003074588901,0.212518788369426,33.8912937927563));
#51203=CARTESIAN_POINT('',(32.7255509406939,0.241969073019064,33.8637293696319));
#51204=CARTESIAN_POINT('Ctrl Pts',(32.7255509406912,0.241969073017624,33.8637293696347));
#51205=CARTESIAN_POINT('Ctrl Pts',(32.7095298197086,0.233224867930978,33.8804609779984));
#51206=CARTESIAN_POINT('Ctrl Pts',(32.6937032119505,0.224586826672025,33.8969505670841));
#51207=CARTESIAN_POINT('',(32.7067303095351,0.400983782787804,33.8637293696319));
#51208=CARTESIAN_POINT('Origin',(30.,-1.32966554433622E-14,33.8637293696319));
#51209=CARTESIAN_POINT('',(32.6717047312569,0.410451051657977,33.8969505670765));
#51210=CARTESIAN_POINT('Ctrl Pts',(32.6717047312489,0.410451051660138,33.8969505670841));
#51211=CARTESIAN_POINT('Ctrl Pts',(32.6891105592595,0.405746328375475,33.8804609779984));
#51212=CARTESIAN_POINT('Ctrl Pts',(32.7067303095322,0.400983782788608,33.8637293696347));
#51213=CARTESIAN_POINT('',(32.6677785445999,0.435240018610789,33.8969505670765));
#51214=CARTESIAN_POINT('Origin',(32.6753090233822,0.423727307748461,33.8912940899386));
#51215=CARTESIAN_POINT('',(32.6981643020872,0.455067425287063,33.8637293696319));
#51216=CARTESIAN_POINT('Ctrl Pts',(32.6981643020846,0.455067425285395,33.8637293696347));
#51217=CARTESIAN_POINT('Ctrl Pts',(32.6828786312952,0.445093172999962,33.8804609779983));
#51218=CARTESIAN_POINT('Ctrl Pts',(32.667778544593,0.435240018606276,33.8969505670841));
#51219=CARTESIAN_POINT('',(32.6669255383174,0.61211529607232,33.8637293696319));
#51220=CARTESIAN_POINT('Origin',(30.,-1.32966554433622E-14,33.8637293696319));
#51221=CARTESIAN_POINT('',(32.6312651388532,0.618805305313054,33.8969505670765));
#51222=CARTESIAN_POINT('Ctrl Pts',(32.6312651388451,0.618805305314574,33.8969505670841));
#51223=CARTESIAN_POINT('Ctrl Pts',(32.6489864388314,0.615480730647778,33.8804609779983));
#51224=CARTESIAN_POINT('Ctrl Pts',(32.6669255383144,0.612115296072874,33.8637293696347));
#51225=CARTESIAN_POINT('',(32.6254061353882,0.64320981109888,33.8969505670765));
#51226=CARTESIAN_POINT('Origin',(32.6338164916465,0.632323382398585,33.8912943077151));
#51227=CARTESIAN_POINT('',(32.6541425833274,0.665360135552893,33.8637293696319));
#51228=CARTESIAN_POINT('Ctrl Pts',(32.654142583325,0.665360135551018,33.8637293696347));
#51229=CARTESIAN_POINT('Ctrl Pts',(32.6396866039721,0.654217330648915,33.8804609779984));
#51230=CARTESIAN_POINT('Ctrl Pts',(32.6254061353817,0.643209811093841,33.8969505670841));
#51231=CARTESIAN_POINT('',(32.6106782843131,0.81947291500756,33.8637293696319));
#51232=CARTESIAN_POINT('Origin',(30.,-1.32966554433622E-14,33.8637293696319));
#51233=CARTESIAN_POINT('',(32.574602921884,0.823344418487232,33.8969505670765));
#51234=CARTESIAN_POINT('Ctrl Pts',(32.5746029218758,0.823344418488117,33.8969505670841));
#51235=CARTESIAN_POINT('Ctrl Pts',(32.5925304361305,0.821420489547548,33.8804609779984));
#51236=CARTESIAN_POINT('Ctrl Pts',(32.6106782843101,0.819472915007888,33.8637293696347));
#51237=CARTESIAN_POINT('',(32.5668472243157,0.84721400121258,33.8969505670765));
#51238=CARTESIAN_POINT('Origin',(32.5760856561636,0.83702095775897,33.891294472568));
#51239=CARTESIAN_POINT('',(32.5937571929495,0.871550679328342,33.8637293696319));
#51240=CARTESIAN_POINT('Ctrl Pts',(32.5937571929473,0.871550679326287,33.8637293696347));
#51241=CARTESIAN_POINT('Ctrl Pts',(32.5802200309508,0.859308020905083,33.8804609779984));
#51242=CARTESIAN_POINT('Ctrl Pts',(32.5668472243096,0.847214001207037,33.8969505670841));
#51243=CARTESIAN_POINT('',(32.5383353305474,1.02177821091938,33.8637293696319));
#51244=CARTESIAN_POINT('Origin',(30.,-1.32966554433622E-14,33.8637293696319));
#51245=CARTESIAN_POINT('',(32.5020674217591,1.02280733953163,33.8969505670765));
#51246=CARTESIAN_POINT('Ctrl Pts',(32.5020674217508,1.02280733953187,33.8969505670841));
#51247=CARTESIAN_POINT('Ctrl Pts',(32.520090621187,1.02229591797922,33.8804609779984));
#51248=CARTESIAN_POINT('Ctrl Pts',(32.5383353305444,1.02177821091947,33.8637293696347));
#51249=CARTESIAN_POINT('',(32.492462846542,1.04599483528156,33.8969505670765));
#51250=CARTESIAN_POINT('Origin',(32.5024724328509,1.03655801106889,33.8912946002427));
#51251=CARTESIAN_POINT('',(32.5173804269653,1.07236782334572,33.8637293696319));
#51252=CARTESIAN_POINT('Ctrl Pts',(32.5173804269632,1.0723678233435,33.8637293696347));
#51253=CARTESIAN_POINT('Ctrl Pts',(32.5048455434284,1.05910079146346,33.8804609779983));
#51254=CARTESIAN_POINT('Ctrl Pts',(32.4924628465363,1.04599483527555,33.8969505670841));
#51255=CARTESIAN_POINT('',(32.4503426953868,1.21778390438515,33.8637293696319));
#51256=CARTESIAN_POINT('Origin',(30.,-1.32966554433622E-14,33.8637293696319));
#51257=CARTESIAN_POINT('',(32.4141058439571,1.21596431320987,33.8969505670765));
#51258=CARTESIAN_POINT('Ctrl Pts',(32.4141058439489,1.21596431320946,33.8969505670841));
#51259=CARTESIAN_POINT('Ctrl Pts',(32.4321136095487,1.21686855212866,33.8804609779984));
#51260=CARTESIAN_POINT('Ctrl Pts',(32.4503426953838,1.217783904385,33.8637293696347));
#51261=CARTESIAN_POINT('',(32.4027116064913,1.23832676336245,33.8969505670765));
#51262=CARTESIAN_POINT('Origin',(32.4134306626749,1.22970433386022,33.891294700665));
#51263=CARTESIAN_POINT('',(32.4254831735348,1.26657346313369,33.8637293696319));
#51264=CARTESIAN_POINT('Ctrl Pts',(32.4254831735329,1.26657346313132,33.8637293696347));
#51265=CARTESIAN_POINT('Ctrl Pts',(32.414027850185,1.25236385345572,33.8804609779984));
#51266=CARTESIAN_POINT('Ctrl Pts',(32.4027116064861,1.23832676335603,33.8969505670841));
#51267=CARTESIAN_POINT('',(32.3472428826875,1.40628155512614,33.8637293696319));
#51268=CARTESIAN_POINT('Origin',(30.,-1.32966554433622E-14,33.8637293696319));
#51269=CARTESIAN_POINT('',(32.3112605008555,1.401624462548,33.8969505670765));
#51270=CARTESIAN_POINT('Ctrl Pts',(32.3112605008473,1.40162446254694,33.8969505670841));
#51271=CARTESIAN_POINT('Ctrl Pts',(32.3291418087476,1.40393878700437,33.8804609779984));
#51272=CARTESIAN_POINT('Ctrl Pts',(32.3472428826845,1.40628155512576,33.8637293696347));
#51273=CARTESIAN_POINT('',(32.298146850404,1.42302399516178,33.8969505670765));
#51274=CARTESIAN_POINT('Origin',(32.3095093115547,1.41526911745259,33.8912947803757));
#51275=CARTESIAN_POINT('',(32.3186320097845,1.45297025634302,33.8637293696319));
#51276=CARTESIAN_POINT('Ctrl Pts',(32.3186320097828,1.45297025634046,33.8637293696347));
#51277=CARTESIAN_POINT('Ctrl Pts',(32.3083268724996,1.43790567583815,33.8804609779983));
#51278=CARTESIAN_POINT('Ctrl Pts',(32.2981468503993,1.42302399515495,33.8969505670841));
#51279=CARTESIAN_POINT('',(32.2296715370789,1.58610901244371,33.8637293696319));
#51280=CARTESIAN_POINT('Origin',(30.,-1.32966554433622E-14,33.8637293696319));
#51281=CARTESIAN_POINT('',(32.194165468194,1.57864313098709,33.8969505670765));
#51282=CARTESIAN_POINT('Ctrl Pts',(32.1941654681859,1.57864313098539,33.8969505670841));
#51283=CARTESIAN_POINT('Ctrl Pts',(32.2118100741774,1.58235327240116,33.8804609779984));
#51284=CARTESIAN_POINT('Ctrl Pts',(32.2296715370759,1.58610901244308,33.8637293696347));
#51285=CARTESIAN_POINT('',(32.1794132547725,1.59894781082743,33.8969505670765));
#51286=CARTESIAN_POINT('Origin',(32.191349084716,1.59210829514292,33.891294843835));
#51287=CARTESIAN_POINT('',(32.1974857086706,1.63040900476035,33.8637293696319));
#51288=CARTESIAN_POINT('Ctrl Pts',(32.1974857086691,1.6304090047577,33.8637293696347));
#51289=CARTESIAN_POINT('Ctrl Pts',(32.1883942920486,1.61458233157692,33.8804609779983));
#51290=CARTESIAN_POINT('Ctrl Pts',(32.1794132547684,1.59894781082026,33.8969505670841));
#51291=CARTESIAN_POINT('',(32.0983535250032,1.7561575802648,33.8637293696319));
#51292=CARTESIAN_POINT('Origin',(30.,-1.32966554433622E-14,33.8637293696319));
#51293=CARTESIAN_POINT('',(32.0635426757871,1.74592893957153,33.8969505670765));
#51294=CARTESIAN_POINT('Ctrl Pts',(32.0635426757792,1.74592893956921,33.8969505670841));
#51295=CARTESIAN_POINT('Ctrl Pts',(32.0808417949984,1.75101202368776,33.8804609779983));
#51296=CARTESIAN_POINT('Ctrl Pts',(32.0983535250003,1.75615758026393,33.8637293696347));
#51297=CARTESIAN_POINT('',(32.0472428516969,1.76501358153524,33.8969505670765));
#51298=CARTESIAN_POINT('Origin',(32.0596784759083,1.75913159602166,33.8912948941586));
#51299=CARTESIAN_POINT('',(32.0627911774245,1.79779573949733,33.8637293696319));
#51300=CARTESIAN_POINT('Ctrl Pts',(32.0627911774232,1.79779573949457,33.8637293696347));
#51301=CARTESIAN_POINT('Ctrl Pts',(32.0549695330723,1.78130455033839,33.8804609779984));
#51302=CARTESIAN_POINT('Ctrl Pts',(32.0472428516934,1.76501358152777,33.8969505670841));
#51303=CARTESIAN_POINT('',(31.9540984656726,1.9153788526219,33.8637293696319));
#51304=CARTESIAN_POINT('Origin',(30.,-1.32966554433622E-14,33.8637293696319));
#51305=CARTESIAN_POINT('',(31.9201974565863,1.90245051566323,33.8969505670765));
#51306=CARTESIAN_POINT('Ctrl Pts',(31.9201974565786,1.90245051566028,33.8969505670841));
#51307=CARTESIAN_POINT('Ctrl Pts',(31.9370444342032,1.90887520357773,33.8804609779983));
#51308=CARTESIAN_POINT('Ctrl Pts',(31.9540984656697,1.91537885262081,33.8637293696347));
#51309=CARTESIAN_POINT('',(31.9024505156632,1.9201974565863,33.8969505670765));
#51310=CARTESIAN_POINT('Origin',(31.915309275617,1.91530926701235,33.891294933562));
#51311=CARTESIAN_POINT('',(31.9153788526219,1.95409846567256,33.8637293696319));
#51312=CARTESIAN_POINT('Ctrl Pts',(31.9153788526208,1.95409846566973,33.8637293696347));
#51313=CARTESIAN_POINT('Ctrl Pts',(31.9088752035777,1.93704443420319,33.8804609779984));
#51314=CARTESIAN_POINT('Ctrl Pts',(31.9024505156603,1.9201974565786,33.8969505670841));
#51315=CARTESIAN_POINT('',(31.7977957394973,2.06279117742448,33.8637293696319));
#51316=CARTESIAN_POINT('Origin',(30.,-1.32966554433622E-14,33.8637293696319));
#51317=CARTESIAN_POINT('',(31.7650135815352,2.04724285169688,33.8969505670765));
#51318=CARTESIAN_POINT('Ctrl Pts',(31.7650135815278,2.04724285169333,33.8969505670841));
#51319=CARTESIAN_POINT('Ctrl Pts',(31.7813045503384,2.05496953307223,33.8804609779984));
#51320=CARTESIAN_POINT('Ctrl Pts',(31.7977957394946,2.06279117742316,33.8637293696347));
#51321=CARTESIAN_POINT('',(31.7459289395715,2.06354267578706,33.8969505670765));
#51322=CARTESIAN_POINT('Origin',(31.7591315658702,2.05967842174595,33.8912949636253));
#51323=CARTESIAN_POINT('',(31.7561575802648,2.09835352500324,33.8637293696319));
#51324=CARTESIAN_POINT('Ctrl Pts',(31.7561575802639,2.09835352500033,33.8637293696347));
#51325=CARTESIAN_POINT('Ctrl Pts',(31.7510120236877,2.08084179499845,33.8804609779984));
#51326=CARTESIAN_POINT('Ctrl Pts',(31.7459289395692,2.06354267577915,33.8969505670841));
#51327=CARTESIAN_POINT('',(31.6304090047604,2.19748570867057,33.8637293696319));
#51328=CARTESIAN_POINT('Origin',(30.,-1.32966554433622E-14,33.8637293696319));
#51329=CARTESIAN_POINT('',(31.5989478108274,2.17941325477248,33.8969505670765));
#51330=CARTESIAN_POINT('Ctrl Pts',(31.5989478108202,2.17941325476838,33.8969505670841));
#51331=CARTESIAN_POINT('Ctrl Pts',(31.6145823315769,2.18839429204865,33.8804609779983));
#51332=CARTESIAN_POINT('Ctrl Pts',(31.6304090047577,2.19748570866908,33.8637293696347));
#51333=CARTESIAN_POINT('',(31.5786431309871,2.19416546819402,33.8969505670765));
#51334=CARTESIAN_POINT('Origin',(31.5921082324254,2.19134897714166,33.8912949854673));
#51335=CARTESIAN_POINT('',(31.5861090124437,2.22967153707891,33.8637293696319));
#51336=CARTESIAN_POINT('Ctrl Pts',(31.5861090124431,2.22967153707593,33.8637293696347));
#51337=CARTESIAN_POINT('Ctrl Pts',(31.5823532724012,2.21181007417742,33.8804609779984));
#51338=CARTESIAN_POINT('Ctrl Pts',(31.5786431309854,2.19416546818594,33.8969505670841));
#51339=CARTESIAN_POINT('',(31.452970256343,2.31863200978455,33.8637293696319));
#51340=CARTESIAN_POINT('Origin',(30.,-1.32966554433622E-14,33.8637293696319));
#51341=CARTESIAN_POINT('',(31.4230239951618,2.29814685040396,33.8969505670765));
#51342=CARTESIAN_POINT('Ctrl Pts',(31.423023995155,2.29814685039929,33.8969505670841));
#51343=CARTESIAN_POINT('Ctrl Pts',(31.4379056758382,2.30832687249959,33.8804609779983));
#51344=CARTESIAN_POINT('Ctrl Pts',(31.4529702563405,2.31863200978281,33.8637293696347));
#51345=CARTESIAN_POINT('',(31.401624462548,2.3112605008555,33.8969505670765));
#51346=CARTESIAN_POINT('Origin',(31.4152690281487,2.30950914111275,33.891294999854));
#51347=CARTESIAN_POINT('',(31.4062815551261,2.34724288268748,33.8637293696319));
#51348=CARTESIAN_POINT('Ctrl Pts',(31.4062815551258,2.34724288268445,33.8637293696347));
#51349=CARTESIAN_POINT('Ctrl Pts',(31.4039387870044,2.32914180874762,33.8804609779983));
#51350=CARTESIAN_POINT('Ctrl Pts',(31.4016244625469,2.31126050084732,33.8969505670841));
#51351=CARTESIAN_POINT('',(31.2665734631337,2.42548317353483,33.8637293696319));
#51352=CARTESIAN_POINT('Origin',(30.,-1.32966554433622E-14,33.8637293696319));
#51353=CARTESIAN_POINT('',(31.2383267633625,2.40271160649132,33.8969505670765));
#51354=CARTESIAN_POINT('Ctrl Pts',(31.2383267633561,2.40271160648613,33.8969505670841));
#51355=CARTESIAN_POINT('Ctrl Pts',(31.2523638534557,2.41402785018503,33.8804609779983));
#51356=CARTESIAN_POINT('Ctrl Pts',(31.2665734631313,2.4254831735329,33.8637293696347));
#51357=CARTESIAN_POINT('',(31.2159643132099,2.41410584395711,33.8969505670765));
#51358=CARTESIAN_POINT('Origin',(31.2297042241653,2.41343041757031,33.8912950072666));
#51359=CARTESIAN_POINT('',(31.2177839043851,2.45034269538681,33.8637293696319));
#51360=CARTESIAN_POINT('Ctrl Pts',(31.217783904385,2.45034269538375,33.8637293696347));
#51361=CARTESIAN_POINT('Ctrl Pts',(31.2168685521287,2.43211360954864,33.8804609779984));
#51362=CARTESIAN_POINT('Ctrl Pts',(31.2159643132095,2.41410584394886,33.8969505670841));
#51363=CARTESIAN_POINT('',(31.0723678233457,2.51738042696526,33.8637293696319));
#51364=CARTESIAN_POINT('Origin',(30.,-1.32966554433622E-14,33.8637293696319));
#51365=CARTESIAN_POINT('',(31.0459948352816,2.49246284654197,33.8969505670765));
#51366=CARTESIAN_POINT('Ctrl Pts',(31.0459948352756,2.4924628465363,33.8969505670841));
#51367=CARTESIAN_POINT('Ctrl Pts',(31.0591007914635,2.50484554342835,33.8804609779983));
#51368=CARTESIAN_POINT('Ctrl Pts',(31.0723678233435,2.51738042696315,33.8637293696347));
#51369=CARTESIAN_POINT('',(31.0228073395316,2.50206742175906,33.8969505670765));
#51370=CARTESIAN_POINT('Origin',(31.036557887911,2.50247209787251,33.8912950079413));
#51371=CARTESIAN_POINT('',(31.0217782109194,2.53833533054745,33.8637293696319));
#51372=CARTESIAN_POINT('Ctrl Pts',(31.0217782109194,2.5383353305444,33.8637293696347));
#51373=CARTESIAN_POINT('Ctrl Pts',(31.0222959179792,2.52009062118696,33.8804609779984));
#51374=CARTESIAN_POINT('Ctrl Pts',(31.0228073395318,2.50206742175081,33.8969505670841));
#51375=CARTESIAN_POINT('',(30.8715506793283,2.59375719294951,33.8637293696319));
#51376=CARTESIAN_POINT('Origin',(30.,-1.32966554433622E-14,33.8637293696319));
#51377=CARTESIAN_POINT('',(30.8472140012126,2.5668472243157,33.8969505670765));
#51378=CARTESIAN_POINT('Ctrl Pts',(30.847214001207,2.56684722430959,33.8969505670841));
#51379=CARTESIAN_POINT('Ctrl Pts',(30.8593080209051,2.58022003095078,33.8804609779984));
#51380=CARTESIAN_POINT('Ctrl Pts',(30.8715506793263,2.59375719294725,33.8637293696347));
#51381=CARTESIAN_POINT('',(30.8233444184872,2.57460292188402,33.8969505670765));
#51382=CARTESIAN_POINT('Origin',(30.8370208295222,2.57608521103255,33.8912950018862));
#51383=CARTESIAN_POINT('',(30.8194729150076,2.61067828431311,33.8637293696319));
#51384=CARTESIAN_POINT('Ctrl Pts',(30.8194729150079,2.61067828431008,33.8637293696347));
#51385=CARTESIAN_POINT('Ctrl Pts',(30.8214204895475,2.59253043613048,33.8804609779984));
#51386=CARTESIAN_POINT('Ctrl Pts',(30.8233444184881,2.57460292187581,33.8969505670841));
#51387=CARTESIAN_POINT('',(30.6653601355529,2.65414258332745,33.8637293696319));
#51388=CARTESIAN_POINT('Origin',(30.,-1.32966554433622E-14,33.8637293696319));
#51389=CARTESIAN_POINT('',(30.6432098110989,2.62540613538819,33.8969505670765));
#51390=CARTESIAN_POINT('Ctrl Pts',(30.6432098110938,2.62540613538167,33.8969505670841));
#51391=CARTESIAN_POINT('Ctrl Pts',(30.6542173306489,2.63968660397217,33.8804609779983));
#51392=CARTESIAN_POINT('Ctrl Pts',(30.665360135551,2.65414258332504,33.8637293696347));
#51393=CARTESIAN_POINT('',(30.6188053053131,2.63126513885322,33.8969505670765));
#51394=CARTESIAN_POINT('Origin',(30.632323260043,2.633815908334,33.8912949888765));
#51395=CARTESIAN_POINT('',(30.6121152960723,2.66692553831736,33.8637293696319));
#51396=CARTESIAN_POINT('Ctrl Pts',(30.6121152960729,2.66692553831437,33.8637293696347));
#51397=CARTESIAN_POINT('Ctrl Pts',(30.6154807306478,2.6489864388314,33.8804609779983));
#51398=CARTESIAN_POINT('Ctrl Pts',(30.6188053053146,2.63126513884509,33.8969505670841));
#51399=CARTESIAN_POINT('',(30.4550674252871,2.69816430208719,33.8637293696319));
#51400=CARTESIAN_POINT('Origin',(30.,-1.32966554433622E-14,33.8637293696319));
#51401=CARTESIAN_POINT('',(30.4352400186108,2.66777854459989,33.8969505670765));
#51402=CARTESIAN_POINT('Ctrl Pts',(30.4352400186063,2.66777854459299,33.8969505670841));
#51403=CARTESIAN_POINT('Ctrl Pts',(30.4450931729999,2.68287863129519,33.8804609779983));
#51404=CARTESIAN_POINT('Ctrl Pts',(30.4550674252854,2.69816430208465,33.8637293696347));
#51405=CARTESIAN_POINT('',(30.410451051658,2.67170473125694,33.8969505670765));
#51406=CARTESIAN_POINT('Origin',(30.4237272067093,2.67530826149246,33.891294968425));
#51407=CARTESIAN_POINT('',(30.4009837827878,2.70673030953515,33.8637293696319));
#51408=CARTESIAN_POINT('Ctrl Pts',(30.4009837827886,2.7067303095322,33.8637293696347));
#51409=CARTESIAN_POINT('Ctrl Pts',(30.4057463283755,2.68911055925956,33.8804609779984));
#51410=CARTESIAN_POINT('Ctrl Pts',(30.4104510516602,2.67170473124897,33.8969505670841));
#51411=CARTESIAN_POINT('',(30.2419690730191,2.72555094069389,33.8637293696319));
#51412=CARTESIAN_POINT('Origin',(30.,-1.32966554433622E-14,33.8637293696319));
#51413=CARTESIAN_POINT('',(30.224586826676,2.69370321195774,33.8969505670765));
#51414=CARTESIAN_POINT('Ctrl Pts',(30.224586826672,2.6937032119505,33.8969505670841));
#51415=CARTESIAN_POINT('Ctrl Pts',(30.233224867931,2.70952981970859,33.8804609779983));
#51416=CARTESIAN_POINT('Ctrl Pts',(30.2419690730176,2.72555094069122,33.8637293696347));
#51417=CARTESIAN_POINT('',(30.1995662307806,2.69567237556048,33.8969505670765));
#51418=CARTESIAN_POINT('Origin',(30.2125187320612,2.70030645711979,33.8912949397143));
#51419=CARTESIAN_POINT('',(30.1873800711418,2.72984718831549,33.8637293696319));
#51420=CARTESIAN_POINT('Ctrl Pts',(30.1873800711428,2.7298471883126,33.8637293696347));
#51421=CARTESIAN_POINT('Ctrl Pts',(30.1935103650644,2.71265541886987,33.8804609779983));
#51422=CARTESIAN_POINT('Ctrl Pts',(30.1995662307834,2.6956723755527,33.8969505670841));
#51423=CARTESIAN_POINT('',(30.027378900953,2.73613365141356,33.8637293696319));
#51424=CARTESIAN_POINT('Origin',(30.,-1.32966554433622E-14,33.8637293696319));
#51425=CARTESIAN_POINT('',(30.012548982272,2.70302030326666,33.8969505670765));
#51426=CARTESIAN_POINT('Ctrl Pts',(30.0125489822686,2.70302030325912,33.8969505670841));
#51427=CARTESIAN_POINT('Ctrl Pts',(30.019918653996,2.71947585577339,33.8804609779983));
#51428=CARTESIAN_POINT('Ctrl Pts',(30.0273789009518,2.73613365141076,33.8637293696347));
#51429=CARTESIAN_POINT('',(29.987451017728,2.70302030326666,33.8969505670765));
#51430=CARTESIAN_POINT('Origin',(30.,2.70866577951602,33.891284862925));
#51431=CARTESIAN_POINT('',(29.9726210990469,2.73613365141356,33.8637293696319));
#51432=CARTESIAN_POINT('Ctrl Pts',(29.9726210990482,2.73613365141079,33.8637293696347));
#51433=CARTESIAN_POINT('Ctrl Pts',(29.980081346004,2.7194758557734,33.8804609779983));
#51434=CARTESIAN_POINT('Ctrl Pts',(29.9874510177314,2.70302030325912,33.8969505670841));
#51435=CARTESIAN_POINT('',(29.8126199288582,2.72984718831549,33.8637293696319));
#51436=CARTESIAN_POINT('Origin',(30.,-1.32966554433622E-14,33.8637293696319));
#51437=CARTESIAN_POINT('',(29.8004337692194,2.69567237556048,33.8969505670765));
#51438=CARTESIAN_POINT('Ctrl Pts',(29.8004337692166,2.6956723755527,33.8969505670841));
#51439=CARTESIAN_POINT('Ctrl Pts',(29.8064896349356,2.71265541886987,33.8804609779983));
#51440=CARTESIAN_POINT('Ctrl Pts',(29.8126199288572,2.7298471883126,33.8637293696347));
#51441=CARTESIAN_POINT('',(29.775413173324,2.69370321195775,33.8969505670765));
#51442=CARTESIAN_POINT('Origin',(29.7874812116306,2.70030745889017,33.8912937927563));
#51443=CARTESIAN_POINT('',(29.7580309269809,2.72555094069389,33.8637293696319));
#51444=CARTESIAN_POINT('Ctrl Pts',(29.7580309269824,2.72555094069121,33.8637293696347));
#51445=CARTESIAN_POINT('Ctrl Pts',(29.766775132069,2.70952981970858,33.8804609779983));
#51446=CARTESIAN_POINT('Ctrl Pts',(29.775413173328,2.69370321195049,33.8969505670841));
#51447=CARTESIAN_POINT('',(29.5990162172122,2.70673030953515,33.8637293696319));
#51448=CARTESIAN_POINT('Origin',(30.,-1.32966554433622E-14,33.8637293696319));
#51449=CARTESIAN_POINT('',(29.589548948342,2.67170473125694,33.8969505670765));
#51450=CARTESIAN_POINT('Ctrl Pts',(29.5895489483398,2.67170473124897,33.8969505670841));
#51451=CARTESIAN_POINT('Ctrl Pts',(29.5942536716245,2.68911055925956,33.8804609779983));
#51452=CARTESIAN_POINT('Ctrl Pts',(29.5990162172114,2.7067303095322,33.8637293696347));
#51453=CARTESIAN_POINT('',(29.5647599813892,2.6677785445999,33.8969505670765));
#51454=CARTESIAN_POINT('Origin',(29.5762726922515,2.67530902338217,33.8912940899386));
#51455=CARTESIAN_POINT('',(29.5449325747129,2.6981643020872,33.8637293696319));
#51456=CARTESIAN_POINT('Ctrl Pts',(29.5449325747146,2.69816430208465,33.8637293696347));
#51457=CARTESIAN_POINT('Ctrl Pts',(29.554906827,2.68287863129518,33.8804609779983));
#51458=CARTESIAN_POINT('Ctrl Pts',(29.5647599813937,2.66777854459298,33.8969505670841));
#51459=CARTESIAN_POINT('',(29.3878847039277,2.66692553831737,33.8637293696319));
#51460=CARTESIAN_POINT('Origin',(30.,-1.32966554433622E-14,33.8637293696319));
#51461=CARTESIAN_POINT('',(29.3811946946869,2.63126513885323,33.8969505670765));
#51462=CARTESIAN_POINT('Ctrl Pts',(29.3811946946854,2.6312651388451,33.8969505670841));
#51463=CARTESIAN_POINT('Ctrl Pts',(29.3845192693522,2.64898643883141,33.8804609779983));
#51464=CARTESIAN_POINT('Ctrl Pts',(29.3878847039271,2.66692553831437,33.8637293696347));
#51465=CARTESIAN_POINT('',(29.3567901889011,2.6254061353882,33.8969505670765));
#51466=CARTESIAN_POINT('Origin',(29.3676766176014,2.6338164916465,33.8912943077151));
#51467=CARTESIAN_POINT('',(29.3346398644471,2.65414258332745,33.8637293696319));
#51468=CARTESIAN_POINT('Ctrl Pts',(29.334639864449,2.65414258332502,33.8637293696347));
#51469=CARTESIAN_POINT('Ctrl Pts',(29.3457826693511,2.63968660397215,33.8804609779983));
#51470=CARTESIAN_POINT('Ctrl Pts',(29.3567901889061,2.62540613538165,33.8969505670841));
#51471=CARTESIAN_POINT('',(29.1805270849924,2.61067828431312,33.8637293696319));
#51472=CARTESIAN_POINT('Origin',(30.,-1.32966554433622E-14,33.8637293696319));
#51473=CARTESIAN_POINT('',(29.1766555815128,2.57460292188403,33.8969505670765));
#51474=CARTESIAN_POINT('Ctrl Pts',(29.1766555815118,2.57460292187581,33.8969505670841));
#51475=CARTESIAN_POINT('Ctrl Pts',(29.1785795104524,2.59253043613048,33.8804609779983));
#51476=CARTESIAN_POINT('Ctrl Pts',(29.1805270849921,2.61067828431008,33.8637293696347));
#51477=CARTESIAN_POINT('',(29.1527859987874,2.56684722431571,33.8969505670765));
#51478=CARTESIAN_POINT('Origin',(29.162979042241,2.57608565616365,33.891294472568));
#51479=CARTESIAN_POINT('',(29.1284493206716,2.59375719294953,33.8637293696319));
#51480=CARTESIAN_POINT('Ctrl Pts',(29.1284493206737,2.59375719294727,33.8637293696347));
#51481=CARTESIAN_POINT('Ctrl Pts',(29.1406919790949,2.58022003095078,33.8804609779983));
#51482=CARTESIAN_POINT('Ctrl Pts',(29.1527859987929,2.56684722430958,33.8969505670841));
#51483=CARTESIAN_POINT('',(28.9782217890806,2.53833533054746,33.8637293696319));
#51484=CARTESIAN_POINT('Origin',(30.,-1.32966554433622E-14,33.8637293696319));
#51485=CARTESIAN_POINT('',(28.9771926604684,2.50206742175908,33.8969505670765));
#51486=CARTESIAN_POINT('Ctrl Pts',(28.9771926604681,2.50206742175082,33.8969505670841));
#51487=CARTESIAN_POINT('Ctrl Pts',(28.9777040820208,2.52009062118696,33.8804609779983));
#51488=CARTESIAN_POINT('Ctrl Pts',(28.9782217890805,2.5383353305444,33.8637293696347));
#51489=CARTESIAN_POINT('',(28.9540051647184,2.49246284654199,33.8969505670765));
#51490=CARTESIAN_POINT('Origin',(28.9634419889311,2.50247243285091,33.8912946002427));
#51491=CARTESIAN_POINT('',(28.9276321766543,2.51738042696527,33.8637293696319));
#51492=CARTESIAN_POINT('Ctrl Pts',(28.9276321766565,2.51738042696315,33.8637293696347));
#51493=CARTESIAN_POINT('Ctrl Pts',(28.9408992085365,2.50484554342835,33.8804609779983));
#51494=CARTESIAN_POINT('Ctrl Pts',(28.9540051647244,2.49246284653631,33.8969505670841));
#51495=CARTESIAN_POINT('',(28.7822160956148,2.45034269538683,33.8637293696319));
#51496=CARTESIAN_POINT('Origin',(30.,-1.32966554433622E-14,33.8637293696319));
#51497=CARTESIAN_POINT('Ctrl Pts',(28.7840356867905,2.41410584394887,33.8969505670841));
#51498=CARTESIAN_POINT('Ctrl Pts',(28.7831314478713,2.43211360954865,33.8804609779983));
#51499=CARTESIAN_POINT('Ctrl Pts',(28.782216095615,2.45034269538377,33.8637293696347));
#51500=CARTESIAN_POINT('',(28.7334265368663,2.42548317353484,33.8637293696319));
#51501=CARTESIAN_POINT('Ctrl Pts',(28.7334265368687,2.42548317353291,33.8637293696347));
#51502=CARTESIAN_POINT('Ctrl Pts',(28.7476361465443,2.41402785018503,33.8804609779983));
#51503=CARTESIAN_POINT('Ctrl Pts',(28.7616732366439,2.40271160648614,33.8969505670841));
#51504=CARTESIAN_POINT('',(28.5937184448738,2.3472428826875,33.8637293696319));
#51505=CARTESIAN_POINT('Origin',(30.,-1.32966554433622E-14,33.8637293696319));
#51506=CARTESIAN_POINT('Ctrl Pts',(28.5983755374531,2.31126050084732,33.8969505670841));
#51507=CARTESIAN_POINT('Ctrl Pts',(28.5960612129956,2.32914180874763,33.8804609779983));
#51508=CARTESIAN_POINT('Ctrl Pts',(28.5937184448742,2.34724288268447,33.8637293696347));
#51509=CARTESIAN_POINT('',(28.547029743657,2.31863200978457,33.8637293696319));
#51510=CARTESIAN_POINT('Ctrl Pts',(28.5470297436595,2.31863200978283,33.8637293696347));
#51511=CARTESIAN_POINT('Ctrl Pts',(28.5620943241618,2.30832687249961,33.8804609779983));
#51512=CARTESIAN_POINT('Ctrl Pts',(28.576976004845,2.29814685039931,33.8969505670841));
#51513=CARTESIAN_POINT('',(28.4138909875563,2.22967153707894,33.8637293696319));
#51514=CARTESIAN_POINT('Origin',(30.,-1.32966554433622E-14,33.8637293696319));
#51515=CARTESIAN_POINT('Ctrl Pts',(28.4213568690146,2.19416546818595,33.8969505670841));
#51516=CARTESIAN_POINT('Ctrl Pts',(28.4176467275988,2.21181007417744,33.8804609779983));
#51517=CARTESIAN_POINT('Ctrl Pts',(28.4138909875569,2.22967153707594,33.8637293696347));
#51518=CARTESIAN_POINT('',(28.3695909952396,2.19748570867059,33.8637293696319));
#51519=CARTESIAN_POINT('Ctrl Pts',(28.3695909952423,2.19748570866909,33.8637293696347));
#51520=CARTESIAN_POINT('Ctrl Pts',(28.3854176684231,2.18839429204867,33.8804609779983));
#51521=CARTESIAN_POINT('Ctrl Pts',(28.4010521891798,2.17941325476839,33.8969505670841));
#51522=CARTESIAN_POINT('',(28.2438424197352,2.09835352500326,33.8637293696319));
#51523=CARTESIAN_POINT('Origin',(30.,-1.32966554433622E-14,33.8637293696319));
#51524=CARTESIAN_POINT('Ctrl Pts',(28.2540710604308,2.06354267577915,33.8969505670841));
#51525=CARTESIAN_POINT('Ctrl Pts',(28.2489879763122,2.08084179499845,33.8804609779983));
#51526=CARTESIAN_POINT('Ctrl Pts',(28.2438424197361,2.09835352500033,33.8637293696347));
#51527=CARTESIAN_POINT('',(28.2022042605027,2.0627911774245,33.8637293696319));
#51528=CARTESIAN_POINT('Ctrl Pts',(28.2022042605055,2.0627911774232,33.8637293696347));
#51529=CARTESIAN_POINT('Ctrl Pts',(28.2186954496616,2.05496953307227,33.8804609779984));
#51530=CARTESIAN_POINT('Ctrl Pts',(28.2349864184722,2.04724285169337,33.8969505670841));
#51531=CARTESIAN_POINT('',(28.0846211473781,1.95409846567259,33.8637293696319));
#51532=CARTESIAN_POINT('Origin',(30.,-1.32966554433622E-14,33.8637293696319));
#51533=CARTESIAN_POINT('Ctrl Pts',(28.0975494843397,1.92019745657863,33.8969505670841));
#51534=CARTESIAN_POINT('Ctrl Pts',(28.0911247964223,1.9370444342032,33.8804609779983));
#51535=CARTESIAN_POINT('Ctrl Pts',(28.0846211473792,1.95409846566974,33.8637293696347));
#51536=CARTESIAN_POINT('',(28.0459015343274,1.91537885262192,33.8637293696319));
#51537=CARTESIAN_POINT('Ctrl Pts',(28.0459015343303,1.91537885262084,33.8637293696347));
#51538=CARTESIAN_POINT('Ctrl Pts',(28.0629555657968,1.90887520357776,33.8804609779983));
#51539=CARTESIAN_POINT('Ctrl Pts',(28.0798025434214,1.90245051566032,33.8969505670841));
#51540=CARTESIAN_POINT('',(27.9372088225755,1.79779573949736,33.8637293696319));
#51541=CARTESIAN_POINT('Origin',(30.,-1.32966554433622E-14,33.8637293696319));
#51542=CARTESIAN_POINT('Ctrl Pts',(27.9527571483066,1.76501358152779,33.8969505670841));
#51543=CARTESIAN_POINT('Ctrl Pts',(27.9450304669277,1.78130455033841,33.8804609779983));
#51544=CARTESIAN_POINT('Ctrl Pts',(27.9372088225768,1.79779573949458,33.8637293696347));
#51545=CARTESIAN_POINT('',(27.9016464749967,1.75615758026483,33.8637293696319));
#51546=CARTESIAN_POINT('Ctrl Pts',(27.9016464749997,1.75615758026397,33.8637293696347));
#51547=CARTESIAN_POINT('Ctrl Pts',(27.9191582050016,1.75101202368779,33.8804609779983));
#51548=CARTESIAN_POINT('Ctrl Pts',(27.9364573242208,1.74592893956924,33.8969505670841));
#51549=CARTESIAN_POINT('',(27.8025142913294,1.63040900476038,33.8637293696319));
#51550=CARTESIAN_POINT('Origin',(30.,-1.32966554433622E-14,33.8637293696319));
#51551=CARTESIAN_POINT('Ctrl Pts',(27.8205867452316,1.59894781082027,33.8969505670841));
#51552=CARTESIAN_POINT('Ctrl Pts',(27.8116057079513,1.61458233157693,33.8804609779983));
#51553=CARTESIAN_POINT('Ctrl Pts',(27.8025142913309,1.63040900475771,33.8637293696347));
#51554=CARTESIAN_POINT('',(27.7703284629211,1.58610901244374,33.8637293696319));
#51555=CARTESIAN_POINT('Ctrl Pts',(27.7703284629241,1.58610901244311,33.8637293696347));
#51556=CARTESIAN_POINT('Ctrl Pts',(27.7881899258226,1.5823532724012,33.8804609779984));
#51557=CARTESIAN_POINT('Ctrl Pts',(27.8058345318141,1.57864313098542,33.8969505670841));
#51558=CARTESIAN_POINT('',(27.6813679902154,1.45297025634305,33.8637293696319));
#51559=CARTESIAN_POINT('Origin',(30.,-1.32966554433622E-14,33.8637293696319));
#51560=CARTESIAN_POINT('Ctrl Pts',(27.7018531496007,1.423023995155,33.8969505670841));
#51561=CARTESIAN_POINT('Ctrl Pts',(27.6916731275004,1.43790567583821,33.8804609779983));
#51562=CARTESIAN_POINT('Ctrl Pts',(27.6813679902172,1.45297025634054,33.8637293696347));
#51563=CARTESIAN_POINT('',(27.6527571173125,1.40628155512618,33.8637293696319));
#51564=CARTESIAN_POINT('Ctrl Pts',(27.6527571173155,1.40628155512578,33.8637293696347));
#51565=CARTESIAN_POINT('Ctrl Pts',(27.6708581912524,1.40393878700439,33.8804609779983));
#51566=CARTESIAN_POINT('Ctrl Pts',(27.6887394991527,1.40162446254697,33.8969505670841));
#51567=CARTESIAN_POINT('',(27.5745168264652,1.26657346313372,33.8637293696319));
#51568=CARTESIAN_POINT('Origin',(30.,-1.32966554433622E-14,33.8637293696319));
#51569=CARTESIAN_POINT('Ctrl Pts',(27.5972883935138,1.23832676335601,33.8969505670841));
#51570=CARTESIAN_POINT('Ctrl Pts',(27.5859721498149,1.2523638534557,33.8804609779984));
#51571=CARTESIAN_POINT('Ctrl Pts',(27.5745168264671,1.26657346313129,33.8637293696347));
#51572=CARTESIAN_POINT('',(27.5496573046132,1.21778390438518,33.8637293696319));
#51573=CARTESIAN_POINT('Ctrl Pts',(27.5496573046163,1.21778390438503,33.8637293696347));
#51574=CARTESIAN_POINT('Ctrl Pts',(27.5678863904514,1.21686855212868,33.8804609779984));
#51575=CARTESIAN_POINT('Ctrl Pts',(27.5858941560511,1.21596431320949,33.8969505670841));
#51576=CARTESIAN_POINT('',(27.4826195730347,1.07236782334576,33.8637293696319));
#51577=CARTESIAN_POINT('Origin',(30.,-1.32966554433622E-14,33.8637293696319));
#51578=CARTESIAN_POINT('Ctrl Pts',(27.5075371534637,1.04599483527557,33.8969505670841));
#51579=CARTESIAN_POINT('Ctrl Pts',(27.4951544565716,1.05910079146348,33.8804609779983));
#51580=CARTESIAN_POINT('Ctrl Pts',(27.4826195730368,1.07236782334352,33.8637293696347));
#51581=CARTESIAN_POINT('',(27.4616646694525,1.02177821091942,33.8637293696319));
#51582=CARTESIAN_POINT('Ctrl Pts',(27.4616646694556,1.0217782109195,33.8637293696347));
#51583=CARTESIAN_POINT('Ctrl Pts',(27.479909378813,1.02229591797925,33.8804609779983));
#51584=CARTESIAN_POINT('Ctrl Pts',(27.4979325782492,1.0228073395319,33.8969505670841));
#51585=CARTESIAN_POINT('',(27.4062428070505,0.871550679328378,33.8637293696319));
#51586=CARTESIAN_POINT('Origin',(30.,-1.32966554433622E-14,33.8637293696319));
#51587=CARTESIAN_POINT('Ctrl Pts',(27.4331527756904,0.847214001207086,33.8969505670841));
#51588=CARTESIAN_POINT('Ctrl Pts',(27.4197799690492,0.859308020905129,33.8804609779984));
#51589=CARTESIAN_POINT('Ctrl Pts',(27.4062428070528,0.871550679326332,33.8637293696347));
#51590=CARTESIAN_POINT('',(27.3893217156869,0.819472915007596,33.8637293696319));
#51591=CARTESIAN_POINT('Ctrl Pts',(27.3893217156899,0.819472915007932,33.8637293696347));
#51592=CARTESIAN_POINT('Ctrl Pts',(27.4074695638695,0.821420489547589,33.8804609779983));
#51593=CARTESIAN_POINT('Ctrl Pts',(27.4253970781241,0.823344418488154,33.8969505670841));
#51594=CARTESIAN_POINT('',(27.3458574166725,0.665360135552929,33.8637293696319));
#51595=CARTESIAN_POINT('Origin',(30.,-1.32966554433622E-14,33.8637293696319));
#51596=CARTESIAN_POINT('Ctrl Pts',(27.3745938646183,0.643209811093841,33.8969505670841));
#51597=CARTESIAN_POINT('Ctrl Pts',(27.3603133960278,0.654217330648928,33.8804609779983));
#51598=CARTESIAN_POINT('Ctrl Pts',(27.3458574166749,0.665360135551045,33.8637293696347));
#51599=CARTESIAN_POINT('',(27.3330744616826,0.612115296072357,33.8637293696319));
#51600=CARTESIAN_POINT('Ctrl Pts',(27.3330744616856,0.612115296072913,33.8637293696347));
#51601=CARTESIAN_POINT('Ctrl Pts',(27.3510135611686,0.615480730647817,33.8804609779983));
#51602=CARTESIAN_POINT('Ctrl Pts',(27.3687348611549,0.618805305314613,33.8969505670841));
#51603=CARTESIAN_POINT('',(27.3018356979128,0.455067425287102,33.8637293696319));
#51604=CARTESIAN_POINT('Origin',(30.,-1.32966554433622E-14,33.8637293696319));
#51605=CARTESIAN_POINT('Ctrl Pts',(27.332221455407,0.435240018606297,33.8969505670841));
#51606=CARTESIAN_POINT('Ctrl Pts',(27.3171213687048,0.445093172999983,33.8804609779983));
#51607=CARTESIAN_POINT('Ctrl Pts',(27.3018356979154,0.455067425285416,33.8637293696347));
#51608=CARTESIAN_POINT('',(27.2932696904648,0.400983782787843,33.8637293696319));
#51609=CARTESIAN_POINT('Ctrl Pts',(27.2932696904678,0.40098378278865,33.8637293696347));
#51610=CARTESIAN_POINT('Ctrl Pts',(27.3108894407404,0.405746328375518,33.8804609779983));
#51611=CARTESIAN_POINT('Ctrl Pts',(27.328295268751,0.410451051660182,33.8969505670841));
#51612=CARTESIAN_POINT('',(27.2744490593061,0.241969073019103,33.8637293696319));
#51613=CARTESIAN_POINT('Origin',(30.,-1.32966554433622E-14,33.8637293696319));
#51614=CARTESIAN_POINT('Ctrl Pts',(27.3062967880495,0.224586826672042,33.8969505670841));
#51615=CARTESIAN_POINT('Ctrl Pts',(27.2904701802914,0.233224867930985,33.8804609779983));
#51616=CARTESIAN_POINT('Ctrl Pts',(27.2744490593088,0.24196907301762,33.8637293696347));
#51617=CARTESIAN_POINT('',(27.2701528116845,0.1873800711418,33.8637293696319));
#51618=CARTESIAN_POINT('Ctrl Pts',(27.2701528116874,0.187380071142834,33.8637293696347));
#51619=CARTESIAN_POINT('Ctrl Pts',(27.2873445811301,0.193510365064418,33.8804609779983));
#51620=CARTESIAN_POINT('Ctrl Pts',(27.3043276244473,0.199566230783421,33.8969505670841));
#51621=CARTESIAN_POINT('',(27.2638663485864,0.0273789009530583,33.8637293696319));
#51622=CARTESIAN_POINT('Origin',(30.,-1.32966554433622E-14,33.8637293696319));
#51623=CARTESIAN_POINT('Ctrl Pts',(27.2969796967408,0.0125489822686371,
33.8969505670841));
#51624=CARTESIAN_POINT('Ctrl Pts',(27.2805241442266,0.0199186539960461,
33.8804609779983));
#51625=CARTESIAN_POINT('Ctrl Pts',(27.2638663485892,0.0273789009517924,
33.8637293696347));
#51626=CARTESIAN_POINT('',(27.2638663485864,-0.0273789009530277,33.8637293696319));
#51627=CARTESIAN_POINT('Ctrl Pts',(27.2638663485892,-0.0273789009517733,
33.8637293696347));
#51628=CARTESIAN_POINT('Ctrl Pts',(27.2805241442266,-0.0199186539960275,
33.8804609779983));
#51629=CARTESIAN_POINT('Ctrl Pts',(27.2969796967409,-0.012548982268619,
33.8969505670841));
#51630=CARTESIAN_POINT('',(27.2701528116845,-0.18738007114177,33.8637293696319));
#51631=CARTESIAN_POINT('Origin',(30.,-1.32966554433622E-14,33.8637293696319));
#51632=CARTESIAN_POINT('',(27.3043276244395,-0.199566230780611,33.8969505670765));
#51633=CARTESIAN_POINT('Ctrl Pts',(27.3043276244473,-0.199566230783401,
33.8969505670841));
#51634=CARTESIAN_POINT('Ctrl Pts',(27.2873445811301,-0.193510365064398,
33.8804609779983));
#51635=CARTESIAN_POINT('Ctrl Pts',(27.2701528116874,-0.187380071142813,
33.8637293696347));
#51636=CARTESIAN_POINT('',(27.3062967880422,-0.224586826675978,33.8969505670765));
#51637=CARTESIAN_POINT('Origin',(27.2996925411099,-0.212518788369432,33.8912937927564));
#51638=CARTESIAN_POINT('',(27.2744490593061,-0.241969073019072,33.8637293696319));
#51639=CARTESIAN_POINT('Ctrl Pts',(27.2744490593088,-0.241969073017592,
33.8637293696347));
#51640=CARTESIAN_POINT('Ctrl Pts',(27.2904701802914,-0.233224867930958,
33.8804609779983));
#51641=CARTESIAN_POINT('Ctrl Pts',(27.3062967880495,-0.224586826672017,
33.8969505670841));
#51642=CARTESIAN_POINT('',(27.2932696904648,-0.400983782787811,33.8637293696319));
#51643=CARTESIAN_POINT('Origin',(30.,-1.32966554433622E-14,33.8637293696319));
#51644=CARTESIAN_POINT('',(27.328295268743,-0.410451051657984,33.8969505670765));
#51645=CARTESIAN_POINT('Ctrl Pts',(27.328295268751,-0.410451051660133,33.8969505670841));
#51646=CARTESIAN_POINT('Ctrl Pts',(27.3108894407404,-0.40574632837547,33.8804609779983));
#51647=CARTESIAN_POINT('Ctrl Pts',(27.2932696904678,-0.400983782788603,
33.8637293696347));
#51648=CARTESIAN_POINT('',(27.3322214554001,-0.435240018610796,33.8969505670765));
#51649=CARTESIAN_POINT('Origin',(27.3246909766178,-0.423727307748468,33.8912940899386));
#51650=CARTESIAN_POINT('',(27.3018356979128,-0.45506742528707,33.8637293696319));
#51651=CARTESIAN_POINT('Ctrl Pts',(27.3018356979154,-0.455067425285398,
33.8637293696347));
#51652=CARTESIAN_POINT('Ctrl Pts',(27.3171213687048,-0.445093172999969,
33.8804609779984));
#51653=CARTESIAN_POINT('Ctrl Pts',(27.332221455407,-0.435240018606285,33.8969505670841));
#51654=CARTESIAN_POINT('',(27.3330744616826,-0.612115296072328,33.8637293696319));
#51655=CARTESIAN_POINT('Origin',(30.,-1.32966554433622E-14,33.8637293696319));
#51656=CARTESIAN_POINT('',(27.3687348611467,-0.618805305313063,33.8969505670765));
#51657=CARTESIAN_POINT('Ctrl Pts',(27.3687348611549,-0.618805305314591,
33.8969505670841));
#51658=CARTESIAN_POINT('Ctrl Pts',(27.3510135611686,-0.615480730647799,
33.8804609779983));
#51659=CARTESIAN_POINT('Ctrl Pts',(27.3330744616856,-0.6121152960729,33.8637293696347));
#51660=CARTESIAN_POINT('',(27.3745938646118,-0.643209811098888,33.8969505670765));
#51661=CARTESIAN_POINT('Origin',(27.3661835083535,-0.632323382398592,33.8912943077151));
#51662=CARTESIAN_POINT('',(27.3458574166725,-0.665360135552901,33.8637293696319));
#51663=CARTESIAN_POINT('Ctrl Pts',(27.345857416675,-0.665360135551053,33.8637293696347));
#51664=CARTESIAN_POINT('Ctrl Pts',(27.3603133960278,-0.654217330648938,
33.8804609779984));
#51665=CARTESIAN_POINT('Ctrl Pts',(27.3745938646183,-0.643209811093851,
33.8969505670841));
#51666=CARTESIAN_POINT('',(27.3893217156868,-0.819472915007569,33.8637293696319));
#51667=CARTESIAN_POINT('Origin',(30.,-1.32966554433622E-14,33.8637293696319));
#51668=CARTESIAN_POINT('',(27.4253970781159,-0.823344418487241,33.8969505670765));
#51669=CARTESIAN_POINT('Ctrl Pts',(27.4253970781241,-0.823344418488121,
33.8969505670841));
#51670=CARTESIAN_POINT('Ctrl Pts',(27.4074695638695,-0.821420489547552,
33.8804609779983));
#51671=CARTESIAN_POINT('Ctrl Pts',(27.3893217156899,-0.819472915007892,
33.8637293696347));
#51672=CARTESIAN_POINT('',(27.4331527756843,-0.847214001212589,33.8969505670765));
#51673=CARTESIAN_POINT('Origin',(27.4239143438363,-0.837020957758988,33.8912944725679));
#51674=CARTESIAN_POINT('',(27.4062428070504,-0.871550679328351,33.8637293696319));
#51675=CARTESIAN_POINT('Ctrl Pts',(27.4062428070527,-0.871550679326329,
33.8637293696347));
#51676=CARTESIAN_POINT('Ctrl Pts',(27.4197799690492,-0.859308020905111,
33.8804609779983));
#51677=CARTESIAN_POINT('Ctrl Pts',(27.4331527756904,-0.847214001207053,
33.8969505670841));
#51678=CARTESIAN_POINT('',(27.4616646694525,-1.02177821091939,33.8637293696319));
#51679=CARTESIAN_POINT('Origin',(30.,-1.32966554433622E-14,33.8637293696319));
#51680=CARTESIAN_POINT('',(27.4979325782409,-1.02280733953164,33.8969505670765));
#51681=CARTESIAN_POINT('Ctrl Pts',(27.4979325782492,-1.02280733953187,33.8969505670841));
#51682=CARTESIAN_POINT('Ctrl Pts',(27.479909378813,-1.02229591797922,33.8804609779983));
#51683=CARTESIAN_POINT('Ctrl Pts',(27.4616646694556,-1.02177821091947,33.8637293696347));
#51684=CARTESIAN_POINT('',(27.507537153458,-1.04599483528157,33.8969505670765));
#51685=CARTESIAN_POINT('Origin',(27.4975275671491,-1.03655801106889,33.8912946002427));
#51686=CARTESIAN_POINT('',(27.4826195730347,-1.07236782334573,33.8637293696319));
#51687=CARTESIAN_POINT('Ctrl Pts',(27.4826195730368,-1.07236782334351,33.8637293696347));
#51688=CARTESIAN_POINT('Ctrl Pts',(27.4951544565716,-1.05910079146347,33.8804609779983));
#51689=CARTESIAN_POINT('Ctrl Pts',(27.5075371534637,-1.04599483527557,33.8969505670841));
#51690=CARTESIAN_POINT('',(27.5496573046131,-1.21778390438516,33.8637293696319));
#51691=CARTESIAN_POINT('Origin',(30.,-1.32966554433622E-14,33.8637293696319));
#51692=CARTESIAN_POINT('',(27.5858941560428,-1.21596431320988,33.8969505670765));
#51693=CARTESIAN_POINT('Ctrl Pts',(27.5858941560511,-1.21596431320946,33.8969505670841));
#51694=CARTESIAN_POINT('Ctrl Pts',(27.5678863904513,-1.21686855212866,33.8804609779983));
#51695=CARTESIAN_POINT('Ctrl Pts',(27.5496573046162,-1.217783904385,33.8637293696347));
#51696=CARTESIAN_POINT('',(27.5972883935086,-1.23832676336246,33.8969505670765));
#51697=CARTESIAN_POINT('Origin',(27.5865693373251,-1.22970433386023,33.891294700665));
#51698=CARTESIAN_POINT('',(27.5745168264651,-1.2665734631337,33.8637293696319));
#51699=CARTESIAN_POINT('Ctrl Pts',(27.574516826467,-1.26657346313129,33.8637293696347));
#51700=CARTESIAN_POINT('Ctrl Pts',(27.5859721498149,-1.2523638534557,33.8804609779983));
#51701=CARTESIAN_POINT('Ctrl Pts',(27.5972883935138,-1.23832676335601,33.8969505670841));
#51702=CARTESIAN_POINT('',(27.6527571173125,-1.40628155512615,33.8637293696319));
#51703=CARTESIAN_POINT('Origin',(30.,-1.32966554433622E-14,33.8637293696319));
#51704=CARTESIAN_POINT('',(27.6887394991444,-1.40162446254801,33.8969505670765));
#51705=CARTESIAN_POINT('Ctrl Pts',(27.6887394991526,-1.40162446254695,33.8969505670841));
#51706=CARTESIAN_POINT('Ctrl Pts',(27.6708581912523,-1.40393878700437,33.8804609779983));
#51707=CARTESIAN_POINT('Ctrl Pts',(27.6527571173155,-1.40628155512576,33.8637293696347));
#51708=CARTESIAN_POINT('',(27.701853149596,-1.42302399516179,33.8969505670765));
#51709=CARTESIAN_POINT('Origin',(27.6904906884452,-1.4152691174526,33.8912947803756));
#51710=CARTESIAN_POINT('',(27.6813679902154,-1.45297025634303,33.8637293696319));
#51711=CARTESIAN_POINT('Ctrl Pts',(27.6813679902171,-1.4529702563405,33.8637293696347));
#51712=CARTESIAN_POINT('Ctrl Pts',(27.6916731275004,-1.43790567583818,33.8804609779983));
#51713=CARTESIAN_POINT('Ctrl Pts',(27.7018531496007,-1.42302399515497,33.8969505670841));
#51714=CARTESIAN_POINT('',(27.770328462921,-1.58610901244372,33.8637293696319));
#51715=CARTESIAN_POINT('Origin',(30.,-1.32966554433622E-14,33.8637293696319));
#51716=CARTESIAN_POINT('',(27.8058345318059,-1.5786431309871,33.8969505670765));
#51717=CARTESIAN_POINT('Ctrl Pts',(27.805834531814,-1.5786431309854,33.8969505670841));
#51718=CARTESIAN_POINT('Ctrl Pts',(27.7881899258225,-1.58235327240118,33.8804609779983));
#51719=CARTESIAN_POINT('Ctrl Pts',(27.770328462924,-1.5861090124431,33.8637293696347));
#51720=CARTESIAN_POINT('',(27.8205867452275,-1.59894781082744,33.8969505670765));
#51721=CARTESIAN_POINT('Origin',(27.8086509152839,-1.59210829514295,33.8912948438349));
#51722=CARTESIAN_POINT('',(27.8025142913294,-1.63040900476036,33.8637293696319));
#51723=CARTESIAN_POINT('Ctrl Pts',(27.8025142913309,-1.63040900475772,33.8637293696347));
#51724=CARTESIAN_POINT('Ctrl Pts',(27.8116057079513,-1.61458233157693,33.8804609779984));
#51725=CARTESIAN_POINT('Ctrl Pts',(27.8205867452316,-1.59894781082027,33.8969505670841));
#51726=CARTESIAN_POINT('',(27.9016464749967,-1.75615758026481,33.8637293696319));
#51727=CARTESIAN_POINT('Origin',(30.,-1.32966554433622E-14,33.8637293696319));
#51728=CARTESIAN_POINT('',(27.9364573242129,-1.74592893957155,33.8969505670765));
#51729=CARTESIAN_POINT('Ctrl Pts',(27.9364573242208,-1.74592893956922,33.8969505670841));
#51730=CARTESIAN_POINT('Ctrl Pts',(27.9191582050015,-1.75101202368778,33.8804609779983));
#51731=CARTESIAN_POINT('Ctrl Pts',(27.9016464749996,-1.75615758026396,33.8637293696347));
#51732=CARTESIAN_POINT('',(27.9527571483031,-1.76501358153525,33.8969505670765));
#51733=CARTESIAN_POINT('Origin',(27.9403215240917,-1.75913159602167,33.8912948941586));
#51734=CARTESIAN_POINT('',(27.9372088225755,-1.79779573949734,33.8637293696319));
#51735=CARTESIAN_POINT('Ctrl Pts',(27.9372088225768,-1.79779573949458,33.8637293696347));
#51736=CARTESIAN_POINT('Ctrl Pts',(27.9450304669278,-1.78130455033841,33.8804609779984));
#51737=CARTESIAN_POINT('Ctrl Pts',(27.9527571483066,-1.76501358152779,33.8969505670841));
#51738=CARTESIAN_POINT('',(28.0459015343274,-1.91537885262191,33.8637293696319));
#51739=CARTESIAN_POINT('Origin',(30.,-1.32966554433622E-14,33.8637293696319));
#51740=CARTESIAN_POINT('',(28.0798025434136,-1.90245051566325,33.8969505670765));
#51741=CARTESIAN_POINT('Ctrl Pts',(28.0798025434214,-1.90245051566032,33.8969505670841));
#51742=CARTESIAN_POINT('Ctrl Pts',(28.0629555657968,-1.90887520357775,33.8804609779983));
#51743=CARTESIAN_POINT('Ctrl Pts',(28.0459015343303,-1.91537885262082,33.8637293696347));
#51744=CARTESIAN_POINT('',(28.0975494843367,-1.92019745658631,33.8969505670765));
#51745=CARTESIAN_POINT('Origin',(28.0846907243829,-1.91530926701236,33.891294933562));
#51746=CARTESIAN_POINT('',(28.084621147378,-1.95409846567257,33.8637293696319));
#51747=CARTESIAN_POINT('Ctrl Pts',(28.0846211473791,-1.9540984656697,33.8637293696347));
#51748=CARTESIAN_POINT('Ctrl Pts',(28.0911247964222,-1.93704443420316,33.8804609779983));
#51749=CARTESIAN_POINT('Ctrl Pts',(28.0975494843396,-1.92019745657857,33.8969505670841));
#51750=CARTESIAN_POINT('',(28.2022042605026,-2.06279117742449,33.8637293696319));
#51751=CARTESIAN_POINT('Origin',(30.,-1.32966554433622E-14,33.8637293696319));
#51752=CARTESIAN_POINT('',(28.2349864184647,-2.04724285169689,33.8969505670765));
#51753=CARTESIAN_POINT('Ctrl Pts',(28.2349864184722,-2.04724285169334,33.8969505670841));
#51754=CARTESIAN_POINT('Ctrl Pts',(28.2186954496616,-2.05496953307223,33.8804609779983));
#51755=CARTESIAN_POINT('Ctrl Pts',(28.2022042605054,-2.06279117742317,33.8637293696347));
#51756=CARTESIAN_POINT('',(28.2540710604284,-2.06354267578707,33.8969505670765));
#51757=CARTESIAN_POINT('Origin',(28.2408684341297,-2.05967842174595,33.8912949636253));
#51758=CARTESIAN_POINT('',(28.2438424197351,-2.09835352500325,33.8637293696319));
#51759=CARTESIAN_POINT('Ctrl Pts',(28.243842419736,-2.09835352500031,33.8637293696347));
#51760=CARTESIAN_POINT('Ctrl Pts',(28.2489879763122,-2.08084179499844,33.8804609779983));
#51761=CARTESIAN_POINT('Ctrl Pts',(28.2540710604307,-2.06354267577914,33.8969505670841));
#51762=CARTESIAN_POINT('',(28.3695909952396,-2.19748570867058,33.8637293696319));
#51763=CARTESIAN_POINT('Origin',(30.,-1.32966554433622E-14,33.8637293696319));
#51764=CARTESIAN_POINT('',(28.4010521891725,-2.17941325477249,33.8969505670765));
#51765=CARTESIAN_POINT('Ctrl Pts',(28.4010521891797,-2.17941325476838,33.8969505670841));
#51766=CARTESIAN_POINT('Ctrl Pts',(28.385417668423,-2.18839429204864,33.8804609779983));
#51767=CARTESIAN_POINT('Ctrl Pts',(28.3695909952423,-2.19748570866905,33.8637293696347));
#51768=CARTESIAN_POINT('',(28.4213568690129,-2.19416546819403,33.8969505670765));
#51769=CARTESIAN_POINT('Origin',(28.4078917675746,-2.19134897714168,33.8912949854673));
#51770=CARTESIAN_POINT('',(28.4138909875562,-2.22967153707893,33.8637293696319));
#51771=CARTESIAN_POINT('Ctrl Pts',(28.4138909875569,-2.22967153707595,33.8637293696347));
#51772=CARTESIAN_POINT('Ctrl Pts',(28.4176467275988,-2.21181007417744,33.8804609779984));
#51773=CARTESIAN_POINT('Ctrl Pts',(28.4213568690146,-2.19416546818595,33.8969505670841));
#51774=CARTESIAN_POINT('',(28.5470297436569,-2.31863200978456,33.8637293696319));
#51775=CARTESIAN_POINT('Origin',(30.,-1.32966554433622E-14,33.8637293696319));
#51776=CARTESIAN_POINT('',(28.5769760048382,-2.29814685040397,33.8969505670765));
#51777=CARTESIAN_POINT('Ctrl Pts',(28.576976004845,-2.29814685039931,33.8969505670841));
#51778=CARTESIAN_POINT('Ctrl Pts',(28.5620943241618,-2.30832687249962,33.8804609779983));
#51779=CARTESIAN_POINT('Ctrl Pts',(28.5470297436595,-2.31863200978285,33.8637293696347));
#51780=CARTESIAN_POINT('',(28.5983755374519,-2.31126050085552,33.8969505670765));
#51781=CARTESIAN_POINT('Origin',(28.5847309718512,-2.30950914111276,33.891294999854));
#51782=CARTESIAN_POINT('',(28.5937184448738,-2.3472428826875,33.8637293696319));
#51783=CARTESIAN_POINT('Ctrl Pts',(28.5937184448742,-2.34724288268445,33.8637293696347));
#51784=CARTESIAN_POINT('Ctrl Pts',(28.5960612129955,-2.32914180874762,33.8804609779983));
#51785=CARTESIAN_POINT('Ctrl Pts',(28.598375537453,-2.31126050084731,33.8969505670841));
#51786=CARTESIAN_POINT('',(28.7334265368663,-2.42548317353484,33.8637293696319));
#51787=CARTESIAN_POINT('Origin',(30.,-1.32966554433622E-14,33.8637293696319));
#51788=CARTESIAN_POINT('',(28.7616732366375,-2.40271160649133,33.8969505670765));
#51789=CARTESIAN_POINT('Ctrl Pts',(28.761673236644,-2.40271160648615,33.8969505670841));
#51790=CARTESIAN_POINT('Ctrl Pts',(28.7476361465443,-2.41402785018505,33.8804609779983));
#51791=CARTESIAN_POINT('Ctrl Pts',(28.7334265368687,-2.42548317353292,33.8637293696347));
#51792=CARTESIAN_POINT('',(28.7840356867901,-2.41410584395713,33.8969505670765));
#51793=CARTESIAN_POINT('Origin',(28.7702957758346,-2.41343041757033,33.8912950072666));
#51794=CARTESIAN_POINT('',(28.7822160956148,-2.45034269538683,33.8637293696319));
#51795=CARTESIAN_POINT('Ctrl Pts',(28.782216095615,-2.45034269538378,33.8637293696347));
#51796=CARTESIAN_POINT('Ctrl Pts',(28.7831314478713,-2.43211360954867,33.8804609779983));
#51797=CARTESIAN_POINT('Ctrl Pts',(28.7840356867905,-2.41410584394888,33.8969505670841));
#51798=CARTESIAN_POINT('',(28.9276321766542,-2.51738042696528,33.8637293696319));
#51799=CARTESIAN_POINT('Origin',(30.,-1.32966554433622E-14,33.8637293696319));
#51800=CARTESIAN_POINT('',(28.9540051647184,-2.49246284654199,33.8969505670765));
#51801=CARTESIAN_POINT('Ctrl Pts',(28.9540051647244,-2.49246284653629,33.8969505670841));
#51802=CARTESIAN_POINT('Ctrl Pts',(28.9408992085365,-2.50484554342835,33.8804609779984));
#51803=CARTESIAN_POINT('Ctrl Pts',(28.9276321766564,-2.51738042696316,33.8637293696347));
#51804=CARTESIAN_POINT('',(28.9771926604683,-2.50206742175908,33.8969505670765));
#51805=CARTESIAN_POINT('Origin',(28.9634421120889,-2.50247209787259,33.8912950079413));
#51806=CARTESIAN_POINT('',(28.9782217890806,-2.53833533054747,33.8637293696319));
#51807=CARTESIAN_POINT('Ctrl Pts',(28.9782217890805,-2.53833533054441,33.8637293696347));
#51808=CARTESIAN_POINT('Ctrl Pts',(28.9777040820207,-2.52009062118697,33.8804609779983));
#51809=CARTESIAN_POINT('Ctrl Pts',(28.9771926604681,-2.50206742175082,33.8969505670841));
#51810=CARTESIAN_POINT('',(29.1284493206716,-2.59375719294953,33.8637293696319));
#51811=CARTESIAN_POINT('Origin',(30.,-1.32966554433622E-14,33.8637293696319));
#51812=CARTESIAN_POINT('',(29.1527859987874,-2.56684722431572,33.8969505670765));
#51813=CARTESIAN_POINT('Ctrl Pts',(29.1527859987929,-2.56684722430957,33.8969505670841));
#51814=CARTESIAN_POINT('Ctrl Pts',(29.1406919790949,-2.58022003095078,33.8804609779984));
#51815=CARTESIAN_POINT('Ctrl Pts',(29.1284493206736,-2.59375719294726,33.8637293696347));
#51816=CARTESIAN_POINT('',(29.1766555815127,-2.57460292188404,33.8969505670765));
#51817=CARTESIAN_POINT('Origin',(29.1629791704777,-2.57608521103258,33.8912950018861));
#51818=CARTESIAN_POINT('',(29.1805270849924,-2.61067828431313,33.8637293696319));
#51819=CARTESIAN_POINT('Ctrl Pts',(29.1805270849921,-2.61067828431009,33.8637293696347));
#51820=CARTESIAN_POINT('Ctrl Pts',(29.1785795104524,-2.59253043613049,33.8804609779983));
#51821=CARTESIAN_POINT('Ctrl Pts',(29.1766555815118,-2.57460292187582,33.8969505670841));
#51822=CARTESIAN_POINT('',(29.334639864447,-2.65414258332747,33.8637293696319));
#51823=CARTESIAN_POINT('Origin',(30.,-1.32966554433622E-14,33.8637293696319));
#51824=CARTESIAN_POINT('',(29.3567901889011,-2.62540613538822,33.8969505670765));
#51825=CARTESIAN_POINT('Ctrl Pts',(29.3567901889061,-2.62540613538166,33.8969505670841));
#51826=CARTESIAN_POINT('Ctrl Pts',(29.345782669351,-2.63968660397217,33.8804609779983));
#51827=CARTESIAN_POINT('Ctrl Pts',(29.3346398644489,-2.65414258332506,33.8637293696347));
#51828=CARTESIAN_POINT('',(29.3811946946869,-2.63126513885324,33.8969505670765));
#51829=CARTESIAN_POINT('Origin',(29.3676767399569,-2.63381590833404,33.8912949888765));
#51830=CARTESIAN_POINT('',(29.3878847039276,-2.66692553831738,33.8637293696319));
#51831=CARTESIAN_POINT('Ctrl Pts',(29.3878847039271,-2.66692553831437,33.8637293696347));
#51832=CARTESIAN_POINT('Ctrl Pts',(29.3845192693522,-2.64898643883142,33.8804609779983));
#51833=CARTESIAN_POINT('Ctrl Pts',(29.3811946946854,-2.63126513884512,33.8969505670841));
#51834=CARTESIAN_POINT('',(29.5449325747129,-2.69816430208721,33.8637293696319));
#51835=CARTESIAN_POINT('Origin',(30.,-1.32966554433622E-14,33.8637293696319));
#51836=CARTESIAN_POINT('',(29.5647599813891,-2.66777854459992,33.8969505670765));
#51837=CARTESIAN_POINT('Ctrl Pts',(29.5647599813936,-2.667778544593,33.8969505670841));
#51838=CARTESIAN_POINT('Ctrl Pts',(29.554906827,-2.68287863129519,33.8804609779983));
#51839=CARTESIAN_POINT('Ctrl Pts',(29.5449325747145,-2.69816430208464,33.8637293696347));
#51840=CARTESIAN_POINT('',(29.589548948342,-2.67170473125696,33.8969505670765));
#51841=CARTESIAN_POINT('Origin',(29.5762727932907,-2.67530826149246,33.8912949684251));
#51842=CARTESIAN_POINT('',(29.5990162172121,-2.70673030953517,33.8637293696319));
#51843=CARTESIAN_POINT('Ctrl Pts',(29.5990162172114,-2.70673030953221,33.8637293696347));
#51844=CARTESIAN_POINT('Ctrl Pts',(29.5942536716245,-2.68911055925957,33.8804609779984));
#51845=CARTESIAN_POINT('Ctrl Pts',(29.5895489483398,-2.67170473124899,33.8969505670841));
#51846=CARTESIAN_POINT('',(29.7580309269809,-2.72555094069392,33.8637293696319));
#51847=CARTESIAN_POINT('Origin',(30.,-1.32966554433622E-14,33.8637293696319));
#51848=CARTESIAN_POINT('',(29.775413173324,-2.69370321195777,33.8969505670765));
#51849=CARTESIAN_POINT('Ctrl Pts',(29.7754131733279,-2.6937032119505,33.8969505670841));
#51850=CARTESIAN_POINT('Ctrl Pts',(29.766775132069,-2.70952981970859,33.8804609779984));
#51851=CARTESIAN_POINT('Ctrl Pts',(29.7580309269823,-2.72555094069122,33.8637293696347));
#51852=CARTESIAN_POINT('',(29.8004337692193,-2.6956723755605,33.8969505670765));
#51853=CARTESIAN_POINT('Origin',(29.7874812679387,-2.70030645711978,33.8912949397144));
#51854=CARTESIAN_POINT('',(29.8126199288582,-2.72984718831551,33.8637293696319));
#51855=CARTESIAN_POINT('Ctrl Pts',(29.8126199288571,-2.72984718831264,33.8637293696347));
#51856=CARTESIAN_POINT('Ctrl Pts',(29.8064896349355,-2.7126554188699,33.8804609779983));
#51857=CARTESIAN_POINT('Ctrl Pts',(29.8004337692165,-2.69567237555272,33.8969505670841));
#51858=CARTESIAN_POINT('',(29.9726210990469,-2.73613365141358,33.8637293696319));
#51859=CARTESIAN_POINT('Origin',(30.,-1.32966554433622E-14,33.8637293696319));
#51860=CARTESIAN_POINT('',(29.987451017728,-2.70302030326669,33.8969505670765));
#51861=CARTESIAN_POINT('Ctrl Pts',(29.9874510177314,-2.70302030325915,33.8969505670841));
#51862=CARTESIAN_POINT('Ctrl Pts',(29.980081346004,-2.71947585577343,33.8804609779983));
#51863=CARTESIAN_POINT('Ctrl Pts',(29.9726210990482,-2.73613365141081,33.8637293696347));
#51864=CARTESIAN_POINT('Ctrl Pts',(30.,-2.69489040503949,33.9051095949605));
#51865=CARTESIAN_POINT('Ctrl Pts',(29.9982996971592,-2.69489040503949,33.9051095949605));
#51866=CARTESIAN_POINT('Ctrl Pts',(29.9965490639354,-2.69522714758869,33.9047710768107));
#51867=CARTESIAN_POINT('Ctrl Pts',(29.9934248389279,-2.69644647069985,33.9035459832655));
#51868=CARTESIAN_POINT('Ctrl Pts',(29.9920523583067,-2.69733049287042,33.9026580100842));
#51869=CARTESIAN_POINT('Ctrl Pts',(29.9894391186861,-2.69960157002983,33.9003782103613));
#51870=CARTESIAN_POINT('Ctrl Pts',(29.9882404972758,-2.7012574944688,33.8987170220582));
#51871=CARTESIAN_POINT('Ctrl Pts',(29.987451017728,-2.7030203032667,33.8969505670765));
#51872=CARTESIAN_POINT('',(30.,-2.73627063036813,33.8637293696319));
#51873=CARTESIAN_POINT('Origin',(30.,-1.32966554433622E-14,31.5762293696319));
#51874=CARTESIAN_POINT('',(30.012548982272,2.70302030326666,31.5905494329235));
#51875=CARTESIAN_POINT('',(30.,2.69489040503946,31.5823904050395));
#51876=CARTESIAN_POINT('Ctrl Pts',(30.012548982272,2.70302030326668,31.5905494329235));
#51877=CARTESIAN_POINT('Ctrl Pts',(30.0117595027242,2.70125749446877,31.5887829779419));
#51878=CARTESIAN_POINT('Ctrl Pts',(30.0105608813139,2.6996015700298,31.5871217896387));
#51879=CARTESIAN_POINT('Ctrl Pts',(30.0079476416933,2.69733049287039,31.5848419899159));
#51880=CARTESIAN_POINT('Ctrl Pts',(30.0065751610721,2.69644647069982,31.5839540167345));
#51881=CARTESIAN_POINT('Ctrl Pts',(30.0034509360646,2.69522714758867,31.5827289231894));
#51882=CARTESIAN_POINT('Ctrl Pts',(30.0017003028408,2.69489040503946,31.5823904050395));
#51883=CARTESIAN_POINT('Ctrl Pts',(30.,2.69489040503946,31.5823904050395));
#51884=CARTESIAN_POINT('',(30.0273789009535,2.73613365141461,31.6237706303691));
#51885=CARTESIAN_POINT('Ctrl Pts',(30.0273789009505,2.73613365140797,31.6237706303625));
#51886=CARTESIAN_POINT('Ctrl Pts',(30.0199186539932,2.71947585576695,31.6070390219952));
#51887=CARTESIAN_POINT('Ctrl Pts',(30.0125489822642,2.70302030324912,31.5905494329059));
#51888=CARTESIAN_POINT('',(30.1873800711414,2.72984718831658,31.6237706303691));
#51889=CARTESIAN_POINT('Origin',(30.,-1.32966554433622E-14,31.6237706303681));
#51890=CARTESIAN_POINT('',(30.1995662307806,2.69567237556048,31.5905494329235));
#51891=CARTESIAN_POINT('Ctrl Pts',(30.1995662307774,2.69567237556935,31.5905494329321));
#51892=CARTESIAN_POINT('Ctrl Pts',(30.1935103650619,2.71265541887687,31.6070390220085));
#51893=CARTESIAN_POINT('Ctrl Pts',(30.1873800711438,2.72984718830972,31.6237706303625));
#51894=CARTESIAN_POINT('',(30.224586826676,2.69370321195774,31.5905494329235));
#51895=CARTESIAN_POINT('Origin',(30.2125187883694,2.70030745889013,31.5962062072437));
#51896=CARTESIAN_POINT('',(30.2419690730196,2.72555094069491,31.6237706303691));
#51897=CARTESIAN_POINT('Ctrl Pts',(30.2419690730161,2.72555094068852,31.6237706303625));
#51898=CARTESIAN_POINT('Ctrl Pts',(30.2332248679276,2.70952981970239,31.6070390219952));
#51899=CARTESIAN_POINT('Ctrl Pts',(30.2245868266668,2.69370321194088,31.5905494329059));
#51900=CARTESIAN_POINT('',(30.4009837827875,2.70673030953627,31.6237706303691));
#51901=CARTESIAN_POINT('Origin',(30.,-1.32966554433622E-14,31.6237706303681));
#51902=CARTESIAN_POINT('',(30.410451051658,2.67170473125694,31.5905494329235));
#51903=CARTESIAN_POINT('Ctrl Pts',(30.4104510516555,2.67170473126603,31.5905494329321));
#51904=CARTESIAN_POINT('Ctrl Pts',(30.4057463283736,2.68911055926674,31.6070390220085));
#51905=CARTESIAN_POINT('Ctrl Pts',(30.4009837827894,2.70673030952925,31.6237706303625));
#51906=CARTESIAN_POINT('',(30.4352400186108,2.66777854459989,31.5905494329235));
#51907=CARTESIAN_POINT('Origin',(30.4237273077485,2.6753090233822,31.5962059100614));
#51908=CARTESIAN_POINT('',(30.4550674252877,2.69816430208816,31.6237706303691));
#51909=CARTESIAN_POINT('Ctrl Pts',(30.4550674252837,2.69816430208208,31.6237706303625));
#51910=CARTESIAN_POINT('Ctrl Pts',(30.4450931729961,2.68287863128927,31.6070390219952));
#51911=CARTESIAN_POINT('Ctrl Pts',(30.4352400186003,2.66777854458381,31.5905494329059));
#51912=CARTESIAN_POINT('',(30.6121152960721,2.6669255383185,31.6237706303691));
#51913=CARTESIAN_POINT('Origin',(30.,-1.32966554433622E-14,31.6237706303681));
#51914=CARTESIAN_POINT('',(30.6188053053131,2.63126513885322,31.5905494329235));
#51915=CARTESIAN_POINT('Ctrl Pts',(30.6188053053114,2.63126513886247,31.5905494329321));
#51916=CARTESIAN_POINT('Ctrl Pts',(30.6154807306465,2.64898643883871,31.6070390220085));
#51917=CARTESIAN_POINT('Ctrl Pts',(30.6121152960735,2.66692553831135,31.6237706303626));
#51918=CARTESIAN_POINT('',(30.6432098110989,2.62540613538819,31.5905494329235));
#51919=CARTESIAN_POINT('Origin',(30.6323233823986,2.63381649164648,31.5962056922849));
#51920=CARTESIAN_POINT('',(30.6653601355536,2.65414258332836,31.6237706303691));
#51921=CARTESIAN_POINT('Ctrl Pts',(30.6653601355491,2.65414258332261,31.6237706303625));
#51922=CARTESIAN_POINT('Ctrl Pts',(30.6542173306446,2.63968660396658,31.6070390219952));
#51923=CARTESIAN_POINT('Ctrl Pts',(30.6432098110871,2.62540613537299,31.5905494329059));
#51924=CARTESIAN_POINT('',(30.8194729150074,2.61067828431427,31.6237706303691));
#51925=CARTESIAN_POINT('Origin',(30.,-1.32966554433622E-14,31.6237706303681));
#51926=CARTESIAN_POINT('',(30.8233444184872,2.57460292188402,31.5905494329235));
#51927=CARTESIAN_POINT('Ctrl Pts',(30.8233444184862,2.57460292189339,31.5905494329321));
#51928=CARTESIAN_POINT('Ctrl Pts',(30.8214204895467,2.59253043613788,31.6070390220085));
#51929=CARTESIAN_POINT('Ctrl Pts',(30.8194729150082,2.61067828430704,31.6237706303625));
#51930=CARTESIAN_POINT('',(30.8472140012126,2.5668472243157,31.5905494329235));
#51931=CARTESIAN_POINT('Origin',(30.837020957759,2.57608565616362,31.596205527432));
#51932=CARTESIAN_POINT('',(30.8715506793291,2.59375719295037,31.6237706303691));
#51933=CARTESIAN_POINT('Ctrl Pts',(30.8715506793242,2.59375719294498,31.6237706303625));
#51934=CARTESIAN_POINT('Ctrl Pts',(30.8593080209003,2.58022003094555,31.6070390219952));
#51935=CARTESIAN_POINT('Ctrl Pts',(30.8472140011997,2.56684722430147,31.5905494329059));
#51936=CARTESIAN_POINT('',(31.0217782109193,2.53833533054861,31.6237706303691));
#51937=CARTESIAN_POINT('Origin',(30.,-1.32966554433622E-14,31.6237706303681));
#51938=CARTESIAN_POINT('',(31.0228073395316,2.50206742175906,31.5905494329235));
#51939=CARTESIAN_POINT('Ctrl Pts',(31.0228073395313,2.50206742176848,31.5905494329321));
#51940=CARTESIAN_POINT('Ctrl Pts',(31.022295917979,2.52009062119439,31.6070390220085));
#51941=CARTESIAN_POINT('Ctrl Pts',(31.0217782109195,2.53833533054134,31.6237706303625));
#51942=CARTESIAN_POINT('',(31.0459948352816,2.49246284654197,31.5905494329235));
#51943=CARTESIAN_POINT('Origin',(31.0365580110689,2.5024724328509,31.5962053997573));
#51944=CARTESIAN_POINT('',(31.0723678233466,2.51738042696606,31.6237706303691));
#51945=CARTESIAN_POINT('Ctrl Pts',(31.0723678233413,2.51738042696106,31.6237706303625));
#51946=CARTESIAN_POINT('Ctrl Pts',(31.0591007914584,2.50484554342351,31.6070390219952));
#51947=CARTESIAN_POINT('Ctrl Pts',(31.0459948352676,2.49246284652878,31.5905494329059));
#51948=CARTESIAN_POINT('',(31.2177839043852,2.45034269538797,31.6237706303691));
#51949=CARTESIAN_POINT('Origin',(30.,-1.32966554433622E-14,31.6237706303681));
#51950=CARTESIAN_POINT('',(31.2159643132099,2.41410584395711,31.5905494329235));
#51951=CARTESIAN_POINT('Ctrl Pts',(31.2159643132104,2.41410584396651,31.5905494329321));
#51952=CARTESIAN_POINT('Ctrl Pts',(31.216868552129,2.43211360955606,31.6070390220085));
#51953=CARTESIAN_POINT('Ctrl Pts',(31.2177839043849,2.4503426953807,31.6237706303625));
#51954=CARTESIAN_POINT('',(31.2383267633625,2.40271160649132,31.5905494329235));
#51955=CARTESIAN_POINT('Origin',(31.2297043338602,2.41343066267493,31.5962052993351));
#51956=CARTESIAN_POINT('',(31.2665734631346,2.42548317353555,31.6237706303691));
#51957=CARTESIAN_POINT('Ctrl Pts',(31.266573463129,2.42548317353098,31.6237706303625));
#51958=CARTESIAN_POINT('Ctrl Pts',(31.2523638534503,2.4140278501806,31.6070390219952));
#51959=CARTESIAN_POINT('Ctrl Pts',(31.2383267633475,2.40271160647926,31.5905494329059));
#51960=CARTESIAN_POINT('',(31.4062815551263,2.34724288268863,31.6237706303691));
#51961=CARTESIAN_POINT('Origin',(30.,-1.32966554433622E-14,31.6237706303681));
#51962=CARTESIAN_POINT('',(31.401624462548,2.3112605008555,31.5905494329235));
#51963=CARTESIAN_POINT('Ctrl Pts',(31.4016244625492,2.31126050086484,31.5905494329321));
#51964=CARTESIAN_POINT('Ctrl Pts',(31.4039387870053,2.32914180875499,31.6070390220085));
#51965=CARTESIAN_POINT('Ctrl Pts',(31.4062815551254,2.34724288268141,31.6237706303625));
#51966=CARTESIAN_POINT('',(31.4230239951618,2.29814685040396,31.5905494329235));
#51967=CARTESIAN_POINT('Origin',(31.4152691174526,2.30950931155475,31.5962052196244));
#51968=CARTESIAN_POINT('',(31.452970256344,2.3186320097852,31.6237706303691));
#51969=CARTESIAN_POINT('Ctrl Pts',(31.452970256338,2.31863200978109,31.6237706303625));
#51970=CARTESIAN_POINT('Ctrl Pts',(31.4379056758324,2.30832687249561,31.6070390219952));
#51971=CARTESIAN_POINT('Ctrl Pts',(31.4230239951459,2.2981468503931,31.5905494329059));
#51972=CARTESIAN_POINT('',(31.5861090124439,2.22967153708005,31.6237706303691));
#51973=CARTESIAN_POINT('Origin',(30.,-1.32966554433622E-14,31.6237706303681));
#51974=CARTESIAN_POINT('',(31.5786431309871,2.19416546819402,31.5905494329235));
#51975=CARTESIAN_POINT('Ctrl Pts',(31.578643130989,2.19416546820324,31.5905494329321));
#51976=CARTESIAN_POINT('Ctrl Pts',(31.5823532724027,2.21181007418469,31.6070390220085));
#51977=CARTESIAN_POINT('Ctrl Pts',(31.5861090124425,2.22967153707293,31.6237706303625));
#51978=CARTESIAN_POINT('',(31.5989478108274,2.17941325477248,31.5905494329235));
#51979=CARTESIAN_POINT('Origin',(31.5921082951429,2.19134908471604,31.596205156165));
#51980=CARTESIAN_POINT('',(31.6304090047614,2.19748570867114,31.6237706303691));
#51981=CARTESIAN_POINT('Ctrl Pts',(31.6304090047551,2.19748570866755,31.6237706303626));
#51982=CARTESIAN_POINT('Ctrl Pts',(31.6145823315708,2.18839429204514,31.6070390219952));
#51983=CARTESIAN_POINT('Ctrl Pts',(31.5989478108108,2.17941325476293,31.5905494329059));
#51984=CARTESIAN_POINT('',(31.7561575802651,2.09835352500435,31.6237706303691));
#51985=CARTESIAN_POINT('Origin',(30.,-1.32966554433622E-14,31.6237706303681));
#51986=CARTESIAN_POINT('',(31.7459289395715,2.06354267578706,31.5905494329235));
#51987=CARTESIAN_POINT('Ctrl Pts',(31.7459289395742,2.06354267579611,31.5905494329321));
#51988=CARTESIAN_POINT('Ctrl Pts',(31.7510120236898,2.08084179500558,31.6070390220085));
#51989=CARTESIAN_POINT('Ctrl Pts',(31.7561575802631,2.09835352499738,31.6237706303625));
#51990=CARTESIAN_POINT('',(31.7650135815352,2.04724285169688,31.5905494329235));
#51991=CARTESIAN_POINT('Origin',(31.7591315960216,2.05967847590828,31.5962051058414));
#51992=CARTESIAN_POINT('',(31.7977957394984,2.06279117742498,31.6237706303691));
#51993=CARTESIAN_POINT('Ctrl Pts',(31.7977957394918,2.06279117742187,31.6237706303625));
#51994=CARTESIAN_POINT('Ctrl Pts',(31.781304550332,2.05496953306921,31.6070390219952));
#51995=CARTESIAN_POINT('Ctrl Pts',(31.7650135815179,2.04724285168864,31.5905494329059));
#51996=CARTESIAN_POINT('',(31.9153788526223,1.95409846567364,31.6237706303691));
#51997=CARTESIAN_POINT('Origin',(30.,-1.32966554433622E-14,31.6237706303681));
#51998=CARTESIAN_POINT('',(31.9024505156632,1.9201974565863,31.5905494329235));
#51999=CARTESIAN_POINT('Ctrl Pts',(31.9024505156666,1.92019745659511,31.5905494329321));
#52000=CARTESIAN_POINT('Ctrl Pts',(31.9088752035804,1.93704443421013,31.6070390220085));
#52001=CARTESIAN_POINT('Ctrl Pts',(31.9153788526197,1.95409846566686,31.6237706303625));
#52002=CARTESIAN_POINT('',(31.9201974565863,1.90245051566323,31.5905494329235));
#52003=CARTESIAN_POINT('Origin',(31.9153092670123,1.91530927561703,31.596205066438));
#52004=CARTESIAN_POINT('',(31.9540984656736,1.91537885262231,31.6237706303691));
#52005=CARTESIAN_POINT('Ctrl Pts',(31.9540984656668,1.9153788526197,31.6237706303625));
#52006=CARTESIAN_POINT('Ctrl Pts',(31.9370444341966,1.90887520357521,31.6070390219952));
#52007=CARTESIAN_POINT('Ctrl Pts',(31.9201974565683,1.90245051565638,31.5905494329059));
#52008=CARTESIAN_POINT('',(32.062791177425,1.79779573949838,31.6237706303691));
#52009=CARTESIAN_POINT('Origin',(30.,-1.32966554433622E-14,31.6237706303681));
#52010=CARTESIAN_POINT('',(32.0472428516969,1.76501358153524,31.5905494329235));
#52011=CARTESIAN_POINT('Ctrl Pts',(32.0472428517009,1.76501358154374,31.5905494329321));
#52012=CARTESIAN_POINT('Ctrl Pts',(32.0549695330754,1.78130455034511,31.6070390220085));
#52013=CARTESIAN_POINT('Ctrl Pts',(32.0627911774219,1.7977957394918,31.6237706303625));
#52014=CARTESIAN_POINT('',(32.0635426757871,1.74592893957153,31.5905494329235));
#52015=CARTESIAN_POINT('Origin',(32.059678421746,1.75913156587022,31.5962050363748));
#52016=CARTESIAN_POINT('',(32.0983535250043,1.75615758026513,31.6237706303691));
#52017=CARTESIAN_POINT('Ctrl Pts',(32.0983535249974,1.75615758026307,31.6237706303625));
#52018=CARTESIAN_POINT('Ctrl Pts',(32.0808417949917,1.75101202368577,31.6070390219952));
#52019=CARTESIAN_POINT('Ctrl Pts',(32.0635426757687,1.74592893956612,31.5905494329059));
#52020=CARTESIAN_POINT('',(32.1974857086711,1.63040900476136,31.6237706303691));
#52021=CARTESIAN_POINT('Origin',(30.,-1.32966554433622E-14,31.6237706303681));
#52022=CARTESIAN_POINT('',(32.1794132547725,1.59894781082743,31.5905494329235));
#52023=CARTESIAN_POINT('Ctrl Pts',(32.1794132547772,1.59894781083559,31.5905494329321));
#52024=CARTESIAN_POINT('Ctrl Pts',(32.1883942920524,1.61458233158336,31.6070390220085));
#52025=CARTESIAN_POINT('Ctrl Pts',(32.1974857086675,1.63040900475503,31.6237706303625));
#52026=CARTESIAN_POINT('',(32.194165468194,1.57864313098709,31.5905494329235));
#52027=CARTESIAN_POINT('Origin',(32.1913489771416,1.59210823242537,31.5962050145327));
#52028=CARTESIAN_POINT('',(32.22967153708,1.58610901244395,31.6237706303691));
#52029=CARTESIAN_POINT('Ctrl Pts',(32.2296715370729,1.58610901244245,31.6237706303625));
#52030=CARTESIAN_POINT('Ctrl Pts',(32.2118100741705,1.58235327239971,31.6070390219952));
#52031=CARTESIAN_POINT('Ctrl Pts',(32.1941654681752,1.57864313098313,31.5905494329059));
#52032=CARTESIAN_POINT('',(32.3186320097852,1.45297025634397,31.6237706303691));
#52033=CARTESIAN_POINT('Origin',(30.,-1.32966554433622E-14,31.6237706303681));
#52034=CARTESIAN_POINT('',(32.298146850404,1.42302399516178,31.5905494329235));
#52035=CARTESIAN_POINT('Ctrl Pts',(32.2981468504093,1.42302399516954,31.5905494329321));
#52036=CARTESIAN_POINT('Ctrl Pts',(32.3083268725038,1.43790567584429,31.6070390220085));
#52037=CARTESIAN_POINT('Ctrl Pts',(32.3186320097811,1.45297025633794,31.6237706303625));
#52038=CARTESIAN_POINT('',(32.3112605008555,1.401624462548,31.5905494329235));
#52039=CARTESIAN_POINT('Origin',(32.3095091411128,1.41526902814876,31.596205000146));
#52040=CARTESIAN_POINT('',(32.3472428826886,1.40628155512629,31.6237706303691));
#52041=CARTESIAN_POINT('Ctrl Pts',(32.3472428826814,1.40628155512536,31.6237706303625));
#52042=CARTESIAN_POINT('Ctrl Pts',(32.3291418087406,1.40393878700346,31.6070390219952));
#52043=CARTESIAN_POINT('Ctrl Pts',(32.3112605008365,1.40162446254554,31.5905494329059));
#52044=CARTESIAN_POINT('',(32.4254831735355,1.26657346313459,31.6237706303691));
#52045=CARTESIAN_POINT('Origin',(30.,-1.32966554433622E-14,31.6237706303681));
#52046=CARTESIAN_POINT('',(32.4027116064913,1.23832676336245,31.5905494329235));
#52047=CARTESIAN_POINT('Ctrl Pts',(32.4027116064972,1.23832676336979,31.5905494329321));
#52048=CARTESIAN_POINT('Ctrl Pts',(32.4140278501897,1.2523638534615,31.6070390220085));
#52049=CARTESIAN_POINT('Ctrl Pts',(32.425483173531,1.26657346312893,31.6237706303625));
#52050=CARTESIAN_POINT('',(32.4141058439571,1.21596431320987,31.5905494329235));
#52051=CARTESIAN_POINT('Origin',(32.4134304175703,1.22970422416531,31.5962049927334));
#52052=CARTESIAN_POINT('',(32.450342695388,1.21778390438521,31.6237706303691));
#52053=CARTESIAN_POINT('Ctrl Pts',(32.4503426953807,1.21778390438485,31.6237706303625));
#52054=CARTESIAN_POINT('Ctrl Pts',(32.4321136095416,1.2168685521283,31.6070390219952));
#52055=CARTESIAN_POINT('Ctrl Pts',(32.4141058439379,1.21596431320891,31.5905494329059));
#52056=CARTESIAN_POINT('',(32.517380426966,1.07236782334656,31.6237706303691));
#52057=CARTESIAN_POINT('Origin',(30.,-1.32966554433622E-14,31.6237706303681));
#52058=CARTESIAN_POINT('',(32.492462846542,1.04599483528156,31.5905494329235));
#52059=CARTESIAN_POINT('Ctrl Pts',(32.4924628465485,1.04599483528841,31.5905494329321));
#52060=CARTESIAN_POINT('Ctrl Pts',(32.5048455434335,1.05910079146886,31.6070390220085));
#52061=CARTESIAN_POINT('Ctrl Pts',(32.5173804269611,1.07236782334125,31.6237706303625));
#52062=CARTESIAN_POINT('',(32.5020674217591,1.02280733953163,31.5905494329235));
#52063=CARTESIAN_POINT('Origin',(32.5024720978725,1.03655788791103,31.5962049920587));
#52064=CARTESIAN_POINT('',(32.5383353305486,1.02177821091935,31.6237706303691));
#52065=CARTESIAN_POINT('Ctrl Pts',(32.5383353305413,1.02177821091956,31.6237706303625));
#52066=CARTESIAN_POINT('Ctrl Pts',(32.5200906211799,1.02229591797942,31.6070390219952));
#52067=CARTESIAN_POINT('Ctrl Pts',(32.5020674217399,1.02280733953218,31.5905494329059));
#52068=CARTESIAN_POINT('',(32.5937571929504,0.87155067932912,31.6237706303691));
#52069=CARTESIAN_POINT('Origin',(30.,-1.32966554433622E-14,31.6237706303681));
#52070=CARTESIAN_POINT('',(32.5668472243157,0.84721400121258,31.5905494329235));
#52071=CARTESIAN_POINT('Ctrl Pts',(32.5668472243227,0.847214001218895,31.5905494329321));
#52072=CARTESIAN_POINT('Ctrl Pts',(32.5802200309563,0.859308020910075,31.6070390220085));
#52073=CARTESIAN_POINT('Ctrl Pts',(32.593757192945,0.871550679324244,31.6237706303625));
#52074=CARTESIAN_POINT('',(32.574602921884,0.823344418487232,31.5905494329235));
#52075=CARTESIAN_POINT('Origin',(32.5760852110325,0.837020829522203,31.5962049981138));
#52076=CARTESIAN_POINT('',(32.6106782843143,0.819472915007436,31.6237706303691));
#52077=CARTESIAN_POINT('Ctrl Pts',(32.6106782843071,0.819472915008212,31.6237706303625));
#52078=CARTESIAN_POINT('Ctrl Pts',(32.5925304361235,0.8214204895483,31.6070390219952));
#52079=CARTESIAN_POINT('Ctrl Pts',(32.5746029218649,0.823344418489286,31.5905494329059));
#52080=CARTESIAN_POINT('',(32.6541425833284,0.665360135553601,31.6237706303691));
#52081=CARTESIAN_POINT('Origin',(30.,-1.32966554433622E-14,31.6237706303681));
#52082=CARTESIAN_POINT('',(32.6254061353882,0.64320981109888,31.5905494329235));
#52083=CARTESIAN_POINT('Ctrl Pts',(32.6254061353957,0.643209811104633,31.5905494329321));
#52084=CARTESIAN_POINT('Ctrl Pts',(32.639686603978,0.654217330653466,31.6070390220085));
#52085=CARTESIAN_POINT('Ctrl Pts',(32.6541425833226,0.665360135549173,31.6237706303625));
#52086=CARTESIAN_POINT('',(32.6312651388532,0.618805305313054,31.5905494329235));
#52087=CARTESIAN_POINT('Origin',(32.633815908334,0.632323260043002,31.5962050111235));
#52088=CARTESIAN_POINT('',(32.6669255383185,0.612115296072106,31.6237706303691));
#52089=CARTESIAN_POINT('Ctrl Pts',(32.6669255383114,0.61211529607344,31.6237706303625));
#52090=CARTESIAN_POINT('Ctrl Pts',(32.6489864388245,0.61548073064908,31.6070390219952));
#52091=CARTESIAN_POINT('Ctrl Pts',(32.6312651388343,0.618805305316593,31.5905494329059));
#52092=CARTESIAN_POINT('',(32.6981643020882,0.455067425287697,31.6237706303691));
#52093=CARTESIAN_POINT('Origin',(30.,-1.32966554433622E-14,31.6237706303681));
#52094=CARTESIAN_POINT('',(32.6677785445999,0.435240018610789,31.5905494329235));
#52095=CARTESIAN_POINT('Ctrl Pts',(32.6677785446078,0.435240018615936,31.5905494329321));
#52096=CARTESIAN_POINT('Ctrl Pts',(32.6828786313014,0.44509317300403,31.6070390220085));
#52097=CARTESIAN_POINT('Ctrl Pts',(32.6981643020821,0.455067425283731,31.6237706303625));
#52098=CARTESIAN_POINT('',(32.6717047312569,0.410451051657977,31.5905494329235));
#52099=CARTESIAN_POINT('Origin',(32.6753082614925,0.423727206709275,31.596205031575));
#52100=CARTESIAN_POINT('',(32.7067303095363,0.400983782787501,31.6237706303691));
#52101=CARTESIAN_POINT('Ctrl Pts',(32.7067303095293,0.400983782789396,31.6237706303625));
#52102=CARTESIAN_POINT('Ctrl Pts',(32.6891105592528,0.405746328377311,31.6070390219952));
#52103=CARTESIAN_POINT('Ctrl Pts',(32.6717047312384,0.410451051662997,31.5905494329059));
#52104=CARTESIAN_POINT('',(32.7255509406949,0.24196907301962,31.6237706303691));
#52105=CARTESIAN_POINT('Origin',(30.,-1.32966554433622E-14,31.6237706303681));
#52106=CARTESIAN_POINT('',(32.6937032119577,0.224586826675969,31.5905494329235));
#52107=CARTESIAN_POINT('Ctrl Pts',(32.693703211966,0.224586826680493,31.5905494329321));
#52108=CARTESIAN_POINT('Ctrl Pts',(32.7095298197151,0.233224867934539,31.6070390220085));
#52109=CARTESIAN_POINT('Ctrl Pts',(32.7255509406885,0.241969073016156,31.6237706303625));
#52110=CARTESIAN_POINT('',(32.6956723755605,0.199566230780603,31.5905494329235));
#52111=CARTESIAN_POINT('Origin',(32.7003064571198,0.212518732061222,31.5962050602857));
#52112=CARTESIAN_POINT('',(32.7298471883166,0.187380071141372,31.6237706303691));
#52113=CARTESIAN_POINT('Ctrl Pts',(32.7298471883097,0.187380071143799,31.6237706303625));
#52114=CARTESIAN_POINT('Ctrl Pts',(32.7126554188632,0.193510365066728,31.6070390219952));
#52115=CARTESIAN_POINT('Ctrl Pts',(32.6956723755424,0.199566230787043,31.5905494329059));
#52116=CARTESIAN_POINT('',(32.7361336514146,0.0273789009534945,31.6237706303691));
#52117=CARTESIAN_POINT('Origin',(30.,-1.32966554433622E-14,31.6237706303681));
#52118=CARTESIAN_POINT('',(32.7030203032667,0.0125489822719939,31.5905494329235));
#52119=CARTESIAN_POINT('Ctrl Pts',(32.7030203032753,0.0125489822758371,
31.5905494329321));
#52120=CARTESIAN_POINT('Ctrl Pts',(32.7194758557802,0.0199186539990537,
31.6070390220085));
#52121=CARTESIAN_POINT('Ctrl Pts',(32.736133651408,0.0273789009505039,31.6237706303625));
#52122=CARTESIAN_POINT('',(32.7030203032667,-0.0125489822720396,31.5905494329235));
#52123=CARTESIAN_POINT('Origin',(32.7086563646858,6.24424376688964E-9,31.5962050859813));
#52124=CARTESIAN_POINT('',(32.7361336514146,-0.02737890095354,31.6237706303691));
#52125=CARTESIAN_POINT('Ctrl Pts',(32.736133651408,-0.0273789009505768,
31.6237706303625));
#52126=CARTESIAN_POINT('Ctrl Pts',(32.719475855767,-0.0199186539932038,
31.6070390219952));
#52127=CARTESIAN_POINT('Ctrl Pts',(32.7030203032491,-0.0125489822642076,
31.5905494329059));
#52128=CARTESIAN_POINT('',(32.7298471883166,-0.187380071141418,31.6237706303691));
#52129=CARTESIAN_POINT('Origin',(30.,-1.32966554433622E-14,31.6237706303681));
#52130=CARTESIAN_POINT('',(32.6956723755605,-0.199566230780649,31.5905494329235));
#52131=CARTESIAN_POINT('Ctrl Pts',(32.6956723755694,-0.199566230777489,
31.5905494329321));
#52132=CARTESIAN_POINT('Ctrl Pts',(32.7126554188769,-0.193510365061924,
31.6070390220085));
#52133=CARTESIAN_POINT('Ctrl Pts',(32.7298471883097,-0.187380071143864,
31.6237706303625));
#52134=CARTESIAN_POINT('',(32.6937032119577,-0.224586826676015,31.5905494329235));
#52135=CARTESIAN_POINT('Origin',(32.7003074588902,-0.212518788369472,31.5962062072437));
#52136=CARTESIAN_POINT('',(32.7255509406949,-0.241969073019665,31.6237706303691));
#52137=CARTESIAN_POINT('Ctrl Pts',(32.7255509406885,-0.241969073016199,
31.6237706303625));
#52138=CARTESIAN_POINT('Ctrl Pts',(32.7095298197024,-0.23322486792764,31.6070390219952));
#52139=CARTESIAN_POINT('Ctrl Pts',(32.6937032119408,-0.22458682666682,31.5905494329059));
#52140=CARTESIAN_POINT('',(32.7067303095363,-0.400983782787547,31.6237706303691));
#52141=CARTESIAN_POINT('Origin',(30.,-1.32966554433622E-14,31.6237706303681));
#52142=CARTESIAN_POINT('',(32.6717047312569,-0.410451051658023,31.5905494329235));
#52143=CARTESIAN_POINT('Ctrl Pts',(32.671704731266,-0.41045105165556,31.5905494329321));
#52144=CARTESIAN_POINT('Ctrl Pts',(32.6891105592667,-0.405746328373564,
31.6070390220085));
#52145=CARTESIAN_POINT('Ctrl Pts',(32.7067303095293,-0.40098378278943,31.6237706303625));
#52146=CARTESIAN_POINT('',(32.6677785445999,-0.435240018610835,31.5905494329235));
#52147=CARTESIAN_POINT('Origin',(32.6753090233822,-0.42372730774851,31.5962059100614));
#52148=CARTESIAN_POINT('',(32.6981643020882,-0.455067425287743,31.6237706303691));
#52149=CARTESIAN_POINT('Ctrl Pts',(32.6981643020821,-0.455067425283808,
31.6237706303625));
#52150=CARTESIAN_POINT('Ctrl Pts',(32.6828786312893,-0.445093172996188,
31.6070390219952));
#52151=CARTESIAN_POINT('Ctrl Pts',(32.6677785445838,-0.435240018600367,
31.5905494329059));
#52152=CARTESIAN_POINT('',(32.6669255383185,-0.612115296072152,31.6237706303691));
#52153=CARTESIAN_POINT('Origin',(30.,-1.32966554433622E-14,31.6237706303681));
#52154=CARTESIAN_POINT('',(32.6312651388532,-0.6188053053131,31.5905494329235));
#52155=CARTESIAN_POINT('Ctrl Pts',(32.6312651388625,-0.618805305311361,
31.5905494329321));
#52156=CARTESIAN_POINT('Ctrl Pts',(32.6489864388387,-0.615480730646455,
31.6070390220085));
#52157=CARTESIAN_POINT('Ctrl Pts',(32.6669255383114,-0.612115296073488,
31.6237706303625));
#52158=CARTESIAN_POINT('',(32.6254061353882,-0.643209811098926,31.5905494329235));
#52159=CARTESIAN_POINT('Origin',(32.6338164916465,-0.632323382398633,31.5962056922849));
#52160=CARTESIAN_POINT('',(32.6541425833284,-0.665360135553646,31.6237706303691));
#52161=CARTESIAN_POINT('Ctrl Pts',(32.6541425833226,-0.665360135549238,
31.6237706303625));
#52162=CARTESIAN_POINT('Ctrl Pts',(32.6396866039666,-0.654217330644686,
31.6070390219952));
#52163=CARTESIAN_POINT('Ctrl Pts',(32.625406135373,-0.643209811087222,31.5905494329059));
#52164=CARTESIAN_POINT('',(32.6106782843143,-0.819472915007481,31.6237706303691));
#52165=CARTESIAN_POINT('Origin',(30.,-1.32966554433622E-14,31.6237706303681));
#52166=CARTESIAN_POINT('',(32.574602921884,-0.823344418487278,31.5905494329235));
#52167=CARTESIAN_POINT('Ctrl Pts',(32.5746029218934,-0.823344418486272,
31.5905494329321));
#52168=CARTESIAN_POINT('Ctrl Pts',(32.5925304361379,-0.821420489546795,
31.6070390220085));
#52169=CARTESIAN_POINT('Ctrl Pts',(32.610678284307,-0.819472915008254,31.6237706303626));
#52170=CARTESIAN_POINT('',(32.5668472243157,-0.847214001212625,31.5905494329235));
#52171=CARTESIAN_POINT('Origin',(32.5760856561636,-0.837020957759021,31.596205527432));
#52172=CARTESIAN_POINT('',(32.5937571929504,-0.871550679329165,31.6237706303691));
#52173=CARTESIAN_POINT('Ctrl Pts',(32.593757192945,-0.871550679324299,31.6237706303625));
#52174=CARTESIAN_POINT('Ctrl Pts',(32.5802200309455,-0.859308020900409,
31.6070390219952));
#52175=CARTESIAN_POINT('Ctrl Pts',(32.5668472243014,-0.847214001199744,
31.5905494329059));
#52176=CARTESIAN_POINT('',(32.5383353305486,-1.02177821091939,31.6237706303691));
#52177=CARTESIAN_POINT('Origin',(30.,-1.32966554433622E-14,31.6237706303681));
#52178=CARTESIAN_POINT('',(32.5020674217591,-1.02280733953168,31.5905494329235));
#52179=CARTESIAN_POINT('Ctrl Pts',(32.5020674217685,-1.02280733953141,31.5905494329321));
#52180=CARTESIAN_POINT('Ctrl Pts',(32.5200906211944,-1.02229591797905,31.6070390220085));
#52181=CARTESIAN_POINT('Ctrl Pts',(32.5383353305413,-1.0217782109196,31.6237706303625));
#52182=CARTESIAN_POINT('',(32.492462846542,-1.0459948352816,31.5905494329235));
#52183=CARTESIAN_POINT('Origin',(32.5024724328509,-1.03655801106895,31.5962053997573));
#52184=CARTESIAN_POINT('',(32.517380426966,-1.07236782334661,31.6237706303691));
#52185=CARTESIAN_POINT('Ctrl Pts',(32.517380426961,-1.07236782334134,31.6237706303625));
#52186=CARTESIAN_POINT('Ctrl Pts',(32.5048455434235,-1.0591007914584,31.6070390219952));
#52187=CARTESIAN_POINT('Ctrl Pts',(32.4924628465288,-1.04599483526767,31.5905494329059));
#52188=CARTESIAN_POINT('',(32.450342695388,-1.21778390438525,31.6237706303691));
#52189=CARTESIAN_POINT('Origin',(30.,-1.32966554433622E-14,31.6237706303681));
#52190=CARTESIAN_POINT('',(32.4141058439571,-1.21596431320991,31.5905494329235));
#52191=CARTESIAN_POINT('Ctrl Pts',(32.4141058439665,-1.21596431321038,31.5905494329321));
#52192=CARTESIAN_POINT('Ctrl Pts',(32.4321136095561,-1.21686855212907,31.6070390220085));
#52193=CARTESIAN_POINT('Ctrl Pts',(32.4503426953807,-1.21778390438489,31.6237706303625));
#52194=CARTESIAN_POINT('',(32.4027116064913,-1.2383267633625,31.5905494329235));
#52195=CARTESIAN_POINT('Origin',(32.4134306626749,-1.2297043338603,31.5962052993351));
#52196=CARTESIAN_POINT('',(32.4254831735355,-1.26657346313463,31.6237706303691));
#52197=CARTESIAN_POINT('Ctrl Pts',(32.425483173531,-1.26657346312898,31.6237706303625));
#52198=CARTESIAN_POINT('Ctrl Pts',(32.4140278501806,-1.25236385345028,31.6070390219952));
#52199=CARTESIAN_POINT('Ctrl Pts',(32.4027116064792,-1.23832676334755,31.5905494329059));
#52200=CARTESIAN_POINT('',(32.3472428826886,-1.40628155512633,31.6237706303691));
#52201=CARTESIAN_POINT('Origin',(30.,-1.32966554433622E-14,31.6237706303681));
#52202=CARTESIAN_POINT('',(32.3112605008555,-1.40162446254804,31.5905494329235));
#52203=CARTESIAN_POINT('Ctrl Pts',(32.3112605008648,-1.40162446254925,31.5905494329321));
#52204=CARTESIAN_POINT('Ctrl Pts',(32.329141808755,-1.40393878700536,31.6070390220085));
#52205=CARTESIAN_POINT('Ctrl Pts',(32.3472428826814,-1.4062815551254,31.6237706303625));
#52206=CARTESIAN_POINT('',(32.2981468504039,-1.42302399516182,31.5905494329235));
#52207=CARTESIAN_POINT('Origin',(32.3095093115547,-1.41526911745265,31.5962052196244));
#52208=CARTESIAN_POINT('',(32.3186320097852,-1.45297025634402,31.6237706303691));
#52209=CARTESIAN_POINT('Ctrl Pts',(32.3186320097811,-1.45297025633802,31.6237706303625));
#52210=CARTESIAN_POINT('Ctrl Pts',(32.3083268724956,-1.43790567583238,31.6070390219952));
#52211=CARTESIAN_POINT('Ctrl Pts',(32.2981468503931,-1.42302399514595,31.5905494329059));
#52212=CARTESIAN_POINT('',(32.22967153708,-1.58610901244399,31.6237706303691));
#52213=CARTESIAN_POINT('Origin',(30.,-1.32966554433622E-14,31.6237706303681));
#52214=CARTESIAN_POINT('',(32.194165468194,-1.57864313098713,31.5905494329235));
#52215=CARTESIAN_POINT('Ctrl Pts',(32.1941654682032,-1.57864313098907,31.5905494329321));
#52216=CARTESIAN_POINT('Ctrl Pts',(32.2118100741847,-1.58235327240274,31.6070390220085));
#52217=CARTESIAN_POINT('Ctrl Pts',(32.2296715370729,-1.58610901244249,31.6237706303625));
#52218=CARTESIAN_POINT('',(32.1794132547725,-1.59894781082747,31.5905494329235));
#52219=CARTESIAN_POINT('Origin',(32.191349084716,-1.59210829514296,31.596205156165));
#52220=CARTESIAN_POINT('',(32.1974857086711,-1.6304090047614,31.6237706303691));
#52221=CARTESIAN_POINT('Ctrl Pts',(32.1974857086675,-1.63040900475512,31.6237706303625));
#52222=CARTESIAN_POINT('Ctrl Pts',(32.1883942920451,-1.61458233157088,31.6070390219952));
#52223=CARTESIAN_POINT('Ctrl Pts',(32.1794132547629,-1.59894781081085,31.5905494329059));
#52224=CARTESIAN_POINT('',(32.0983535250043,-1.75615758026517,31.6237706303691));
#52225=CARTESIAN_POINT('Origin',(30.,-1.32966554433622E-14,31.6237706303681));
#52226=CARTESIAN_POINT('',(32.063542675787,-1.74592893957158,31.5905494329235));
#52227=CARTESIAN_POINT('Ctrl Pts',(32.0635426757961,-1.74592893957424,31.5905494329321));
#52228=CARTESIAN_POINT('Ctrl Pts',(32.0808417950055,-1.75101202368991,31.6070390220085));
#52229=CARTESIAN_POINT('Ctrl Pts',(32.0983535249973,-1.75615758026313,31.6237706303625));
#52230=CARTESIAN_POINT('',(32.0472428516969,-1.76501358153528,31.5905494329235));
#52231=CARTESIAN_POINT('Origin',(32.0596784759083,-1.75913159602171,31.5962051058414));
#52232=CARTESIAN_POINT('',(32.062791177425,-1.79779573949842,31.6237706303691));
#52233=CARTESIAN_POINT('Ctrl Pts',(32.0627911774219,-1.79779573949184,31.6237706303625));
#52234=CARTESIAN_POINT('Ctrl Pts',(32.0549695330692,-1.78130455033205,31.6070390219952));
#52235=CARTESIAN_POINT('Ctrl Pts',(32.0472428516887,-1.76501358151791,31.5905494329059));
#52236=CARTESIAN_POINT('',(31.9540984656736,-1.91537885262235,31.6237706303691));
#52237=CARTESIAN_POINT('Origin',(30.,-1.32966554433622E-14,31.6237706303681));
#52238=CARTESIAN_POINT('',(31.9201974565863,-1.90245051566327,31.5905494329235));
#52239=CARTESIAN_POINT('Ctrl Pts',(31.9201974565951,-1.90245051566663,31.5905494329321));
#52240=CARTESIAN_POINT('Ctrl Pts',(31.9370444342101,-1.90887520358042,31.6070390220085));
#52241=CARTESIAN_POINT('Ctrl Pts',(31.9540984656668,-1.91537885261975,31.6237706303625));
#52242=CARTESIAN_POINT('',(31.9024505156632,-1.92019745658634,31.5905494329235));
#52243=CARTESIAN_POINT('Origin',(31.915309275617,-1.91530926701241,31.5962050664381));
#52244=CARTESIAN_POINT('',(31.9153788526223,-1.95409846567368,31.6237706303691));
#52245=CARTESIAN_POINT('Ctrl Pts',(31.9153788526197,-1.9540984656669,31.6237706303625));
#52246=CARTESIAN_POINT('Ctrl Pts',(31.9088752035752,-1.93704443419662,31.6070390219952));
#52247=CARTESIAN_POINT('Ctrl Pts',(31.9024505156564,-1.92019745656839,31.5905494329059));
#52248=CARTESIAN_POINT('',(31.7977957394984,-2.06279117742501,31.6237706303691));
#52249=CARTESIAN_POINT('Origin',(30.,-1.32966554433622E-14,31.6237706303681));
#52250=CARTESIAN_POINT('',(31.7650135815352,-2.04724285169692,31.5905494329235));
#52251=CARTESIAN_POINT('Ctrl Pts',(31.7650135815437,-2.04724285170096,31.5905494329321));
#52252=CARTESIAN_POINT('Ctrl Pts',(31.7813045503451,-2.05496953307547,31.6070390220085));
#52253=CARTESIAN_POINT('Ctrl Pts',(31.7977957394918,-2.06279117742192,31.6237706303625));
#52254=CARTESIAN_POINT('',(31.7459289395715,-2.0635426757871,31.5905494329235));
#52255=CARTESIAN_POINT('Origin',(31.7591315658702,-2.05967842174604,31.5962050363748));
#52256=CARTESIAN_POINT('',(31.7561575802651,-2.09835352500439,31.6237706303691));
#52257=CARTESIAN_POINT('Ctrl Pts',(31.7561575802631,-2.09835352499741,31.6237706303625));
#52258=CARTESIAN_POINT('Ctrl Pts',(31.7510120236858,-2.08084179499169,31.6070390219952));
#52259=CARTESIAN_POINT('Ctrl Pts',(31.7459289395661,-2.06354267576866,31.5905494329059));
#52260=CARTESIAN_POINT('',(31.6304090047613,-2.19748570867118,31.6237706303691));
#52261=CARTESIAN_POINT('Origin',(30.,-1.32966554433622E-14,31.6237706303681));
#52262=CARTESIAN_POINT('',(31.5989478108274,-2.17941325477251,31.5905494329235));
#52263=CARTESIAN_POINT('Ctrl Pts',(31.5989478108356,-2.17941325477721,31.5905494329321));
#52264=CARTESIAN_POINT('Ctrl Pts',(31.6145823315833,-2.18839429205237,31.6070390220085));
#52265=CARTESIAN_POINT('Ctrl Pts',(31.630409004755,-2.19748570866756,31.6237706303625));
#52266=CARTESIAN_POINT('',(31.5786431309871,-2.19416546819406,31.5905494329235));
#52267=CARTESIAN_POINT('Origin',(31.5921082324253,-2.19134897714169,31.5962050145327));
#52268=CARTESIAN_POINT('',(31.5861090124439,-2.22967153708009,31.6237706303691));
#52269=CARTESIAN_POINT('Ctrl Pts',(31.5861090124425,-2.22967153707296,31.6237706303625));
#52270=CARTESIAN_POINT('Ctrl Pts',(31.5823532723997,-2.21181007417054,31.6070390219952));
#52271=CARTESIAN_POINT('Ctrl Pts',(31.5786431309832,-2.19416546817524,31.5905494329059));
#52272=CARTESIAN_POINT('',(31.452970256344,-2.31863200978524,31.6237706303691));
#52273=CARTESIAN_POINT('Origin',(30.,-1.32966554433622E-14,31.6237706303681));
#52274=CARTESIAN_POINT('',(31.4230239951618,-2.29814685040399,31.5905494329235));
#52275=CARTESIAN_POINT('Ctrl Pts',(31.4230239951696,-2.2981468504093,31.5905494329321));
#52276=CARTESIAN_POINT('Ctrl Pts',(31.4379056758443,-2.30832687250383,31.6070390220085));
#52277=CARTESIAN_POINT('Ctrl Pts',(31.452970256338,-2.31863200978113,31.6237706303625));
#52278=CARTESIAN_POINT('',(31.401624462548,-2.31126050085554,31.5905494329235));
#52279=CARTESIAN_POINT('Origin',(31.4152690281487,-2.30950914111279,31.596205000146));
#52280=CARTESIAN_POINT('',(31.4062815551263,-2.34724288268866,31.6237706303691));
#52281=CARTESIAN_POINT('Ctrl Pts',(31.4062815551254,-2.34724288268144,31.6237706303625));
#52282=CARTESIAN_POINT('Ctrl Pts',(31.4039387870035,-2.32914180874065,31.6070390219952));
#52283=CARTESIAN_POINT('Ctrl Pts',(31.4016244625455,-2.31126050083648,31.5905494329059));
#52284=CARTESIAN_POINT('',(31.2665734631346,-2.42548317353559,31.6237706303691));
#52285=CARTESIAN_POINT('Origin',(30.,-1.32966554433622E-14,31.6237706303681));
#52286=CARTESIAN_POINT('',(31.2383267633624,-2.40271160649135,31.5905494329235));
#52287=CARTESIAN_POINT('Ctrl Pts',(31.2383267633697,-2.40271160649727,31.5905494329321));
#52288=CARTESIAN_POINT('Ctrl Pts',(31.2523638534615,-2.41402785018975,31.6070390220085));
#52289=CARTESIAN_POINT('Ctrl Pts',(31.2665734631289,-2.42548317353104,31.6237706303625));
#52290=CARTESIAN_POINT('',(31.2159643132098,-2.41410584395714,31.5905494329235));
#52291=CARTESIAN_POINT('Origin',(31.2297042241653,-2.41343041757036,31.5962049927334));
#52292=CARTESIAN_POINT('',(31.2177839043852,-2.450342695388,31.6237706303691));
#52293=CARTESIAN_POINT('Ctrl Pts',(31.2177839043848,-2.45034269538075,31.6237706303625));
#52294=CARTESIAN_POINT('Ctrl Pts',(31.2168685521282,-2.43211360954164,31.6070390219952));
#52295=CARTESIAN_POINT('Ctrl Pts',(31.2159643132088,-2.41410584393796,31.5905494329059));
#52296=CARTESIAN_POINT('',(31.0723678233465,-2.51738042696609,31.6237706303691));
#52297=CARTESIAN_POINT('Origin',(30.,-1.32966554433622E-14,31.6237706303681));
#52298=CARTESIAN_POINT('',(31.0459948352815,-2.49246284654201,31.5905494329235));
#52299=CARTESIAN_POINT('Ctrl Pts',(31.0459948352884,-2.49246284654849,31.5905494329321));
#52300=CARTESIAN_POINT('Ctrl Pts',(31.0591007914688,-2.5048455434335,31.6070390220085));
#52301=CARTESIAN_POINT('Ctrl Pts',(31.0723678233412,-2.51738042696111,31.6237706303625));
#52302=CARTESIAN_POINT('',(31.0228073395316,-2.5020674217591,31.5905494329235));
#52303=CARTESIAN_POINT('Origin',(31.036557887911,-2.50247209787259,31.5962049920587));
#52304=CARTESIAN_POINT('',(31.0217782109193,-2.53833533054864,31.6237706303691));
#52305=CARTESIAN_POINT('Ctrl Pts',(31.0217782109196,-2.53833533054137,31.6237706303625));
#52306=CARTESIAN_POINT('Ctrl Pts',(31.0222959179794,-2.52009062117993,31.6070390219952));
#52307=CARTESIAN_POINT('Ctrl Pts',(31.0228073395322,-2.50206742173989,31.5905494329059));
#52308=CARTESIAN_POINT('',(30.8715506793291,-2.59375719295041,31.6237706303691));
#52309=CARTESIAN_POINT('Origin',(30.,-1.32966554433622E-14,31.6237706303681));
#52310=CARTESIAN_POINT('',(30.8472140012126,-2.56684722431573,31.5905494329235));
#52311=CARTESIAN_POINT('Ctrl Pts',(30.8472140012189,-2.56684722432271,31.5905494329321));
#52312=CARTESIAN_POINT('Ctrl Pts',(30.8593080209101,-2.58022003095631,31.6070390220085));
#52313=CARTESIAN_POINT('Ctrl Pts',(30.8715506793242,-2.593757192945,31.6237706303625));
#52314=CARTESIAN_POINT('',(30.8233444184872,-2.57460292188405,31.5905494329235));
#52315=CARTESIAN_POINT('Origin',(30.8370208295222,-2.5760852110326,31.5962049981139));
#52316=CARTESIAN_POINT('',(30.8194729150074,-2.6106782843143,31.6237706303691));
#52317=CARTESIAN_POINT('Ctrl Pts',(30.8194729150082,-2.61067828430707,31.6237706303625));
#52318=CARTESIAN_POINT('Ctrl Pts',(30.8214204895483,-2.5925304361235,31.6070390219952));
#52319=CARTESIAN_POINT('Ctrl Pts',(30.8233444184892,-2.57460292186495,31.5905494329059));
#52320=CARTESIAN_POINT('',(30.6653601355536,-2.65414258332839,31.6237706303691));
#52321=CARTESIAN_POINT('Origin',(30.,-1.32966554433622E-14,31.6237706303681));
#52322=CARTESIAN_POINT('',(30.6432098110989,-2.62540613538822,31.5905494329235));
#52323=CARTESIAN_POINT('Ctrl Pts',(30.6432098111046,-2.62540613539568,31.5905494329321));
#52324=CARTESIAN_POINT('Ctrl Pts',(30.6542173306535,-2.63968660397806,31.6070390220085));
#52325=CARTESIAN_POINT('Ctrl Pts',(30.6653601355492,-2.65414258332262,31.6237706303625));
#52326=CARTESIAN_POINT('',(30.618805305313,-2.63126513885325,31.5905494329235));
#52327=CARTESIAN_POINT('Origin',(30.632323260043,-2.63381590833404,31.5962050111235));
#52328=CARTESIAN_POINT('',(30.6121152960721,-2.66692553831853,31.6237706303691));
#52329=CARTESIAN_POINT('Ctrl Pts',(30.6121152960734,-2.66692553831138,31.6237706303625));
#52330=CARTESIAN_POINT('Ctrl Pts',(30.615480730649,-2.6489864388245,31.6070390219952));
#52331=CARTESIAN_POINT('Ctrl Pts',(30.6188053053166,-2.63126513883437,31.5905494329059));
#52332=CARTESIAN_POINT('',(30.4550674252877,-2.69816430208819,31.6237706303691));
#52333=CARTESIAN_POINT('Origin',(30.,-1.32966554433622E-14,31.6237706303681));
#52334=CARTESIAN_POINT('',(30.4352400186108,-2.66777854459992,31.5905494329235));
#52335=CARTESIAN_POINT('Ctrl Pts',(30.435240018616,-2.6677785446078,31.5905494329321));
#52336=CARTESIAN_POINT('Ctrl Pts',(30.445093173004,-2.68287863130142,31.6070390220085));
#52337=CARTESIAN_POINT('Ctrl Pts',(30.4550674252837,-2.69816430208209,31.6237706303625));
#52338=CARTESIAN_POINT('',(30.410451051658,-2.67170473125697,31.5905494329235));
#52339=CARTESIAN_POINT('Origin',(30.4237272067093,-2.67530826149246,31.5962050315749));
#52340=CARTESIAN_POINT('',(30.4009837827875,-2.7067303095363,31.6237706303691));
#52341=CARTESIAN_POINT('Ctrl Pts',(30.4009837827894,-2.70673030952928,31.6237706303625));
#52342=CARTESIAN_POINT('Ctrl Pts',(30.4057463283773,-2.68911055925278,31.6070390219952));
#52343=CARTESIAN_POINT('Ctrl Pts',(30.410451051663,-2.67170473123841,31.5905494329059));
#52344=CARTESIAN_POINT('',(30.2419690730196,-2.72555094069494,31.6237706303691));
#52345=CARTESIAN_POINT('Origin',(30.,-1.32966554433622E-14,31.6237706303681));
#52346=CARTESIAN_POINT('',(30.224586826676,-2.69370321195777,31.5905494329235));
#52347=CARTESIAN_POINT('Ctrl Pts',(30.2245868266805,-2.69370321196604,31.5905494329321));
#52348=CARTESIAN_POINT('Ctrl Pts',(30.2332248679346,-2.70952981971513,31.6070390220085));
#52349=CARTESIAN_POINT('Ctrl Pts',(30.2419690730162,-2.72555094068854,31.6237706303625));
#52350=CARTESIAN_POINT('',(30.1995662307806,-2.69567237556051,31.5905494329235));
#52351=CARTESIAN_POINT('Origin',(30.2125187320612,-2.70030645711985,31.5962050602857));
#52352=CARTESIAN_POINT('',(30.1873800711414,-2.72984718831661,31.6237706303691));
#52353=CARTESIAN_POINT('Ctrl Pts',(30.1873800711438,-2.72984718830975,31.6237706303625));
#52354=CARTESIAN_POINT('Ctrl Pts',(30.1935103650667,-2.71265541886325,31.6070390219952));
#52355=CARTESIAN_POINT('Ctrl Pts',(30.199566230787,-2.6956723755424,31.5905494329059));
#52356=CARTESIAN_POINT('',(30.0273789009535,-2.73613365141464,31.6237706303691));
#52357=CARTESIAN_POINT('Origin',(30.,-1.32966554433622E-14,31.6237706303681));
#52358=CARTESIAN_POINT('',(30.012548982272,-2.70302030326669,31.5905494329235));
#52359=CARTESIAN_POINT('Ctrl Pts',(30.0125489822759,-2.70302030327528,31.5905494329321));
#52360=CARTESIAN_POINT('Ctrl Pts',(30.0199186539991,-2.7194758557802,31.6070390220085));
#52361=CARTESIAN_POINT('Ctrl Pts',(30.0273789009505,-2.736133651408,31.6237706303625));
#52362=CARTESIAN_POINT('',(29.987451017728,-2.70302030326669,31.5905494329235));
#52363=CARTESIAN_POINT('Origin',(30.,-2.7086657795165,31.5962151370754));
#52364=CARTESIAN_POINT('',(29.9726210990465,-2.73613365141464,31.6237706303691));
#52365=CARTESIAN_POINT('Ctrl Pts',(29.9726210990495,-2.73613365140799,31.6237706303625));
#52366=CARTESIAN_POINT('Ctrl Pts',(29.9800813460068,-2.71947585576697,31.6070390219952));
#52367=CARTESIAN_POINT('Ctrl Pts',(29.9874510177359,-2.70302030324915,31.5905494329059));
#52368=CARTESIAN_POINT('',(29.8126199288586,-2.72984718831661,31.6237706303691));
#52369=CARTESIAN_POINT('Origin',(30.,-1.32966554433622E-14,31.6237706303681));
#52370=CARTESIAN_POINT('',(29.8004337692193,-2.6956723755605,31.5905494329235));
#52371=CARTESIAN_POINT('Ctrl Pts',(29.8004337692225,-2.69567237556937,31.5905494329321));
#52372=CARTESIAN_POINT('Ctrl Pts',(29.806489634938,-2.71265541887691,31.6070390220085));
#52373=CARTESIAN_POINT('Ctrl Pts',(29.8126199288561,-2.72984718830976,31.6237706303625));
#52374=CARTESIAN_POINT('',(29.775413173324,-2.69370321195777,31.5905494329235));
#52375=CARTESIAN_POINT('Origin',(29.7874812116305,-2.70030745889015,31.5962062072437));
#52376=CARTESIAN_POINT('',(29.7580309269803,-2.72555094069494,31.6237706303691));
#52377=CARTESIAN_POINT('Ctrl Pts',(29.7580309269838,-2.72555094068855,31.6237706303625));
#52378=CARTESIAN_POINT('Ctrl Pts',(29.7667751320723,-2.7095298197024,31.6070390219952));
#52379=CARTESIAN_POINT('Ctrl Pts',(29.7754131733332,-2.69370321194088,31.5905494329059));
#52380=CARTESIAN_POINT('',(29.5990162172124,-2.70673030953629,31.6237706303691));
#52381=CARTESIAN_POINT('Origin',(30.,-1.32966554433622E-14,31.6237706303681));
#52382=CARTESIAN_POINT('',(29.589548948342,-2.67170473125696,31.5905494329235));
#52383=CARTESIAN_POINT('Ctrl Pts',(29.5895489483445,-2.67170473126605,31.5905494329321));
#52384=CARTESIAN_POINT('Ctrl Pts',(29.5942536716264,-2.68911055926676,31.6070390220085));
#52385=CARTESIAN_POINT('Ctrl Pts',(29.5990162172106,-2.70673030952926,31.6237706303625));
#52386=CARTESIAN_POINT('',(29.5647599813891,-2.66777854459992,31.5905494329235));
#52387=CARTESIAN_POINT('Origin',(29.5762726922515,-2.67530902338218,31.5962059100614));
#52388=CARTESIAN_POINT('',(29.5449325747122,-2.69816430208819,31.6237706303691));
#52389=CARTESIAN_POINT('Ctrl Pts',(29.5449325747162,-2.6981643020821,31.6237706303625));
#52390=CARTESIAN_POINT('Ctrl Pts',(29.5549068270038,-2.68287863128929,31.6070390219952));
#52391=CARTESIAN_POINT('Ctrl Pts',(29.5647599813996,-2.66777854458383,31.5905494329059));
#52392=CARTESIAN_POINT('',(29.3878847039278,-2.66692553831852,31.6237706303691));
#52393=CARTESIAN_POINT('Origin',(30.,-1.32966554433622E-14,31.6237706303681));
#52394=CARTESIAN_POINT('',(29.3811946946869,-2.63126513885324,31.5905494329235));
#52395=CARTESIAN_POINT('Ctrl Pts',(29.3811946946886,-2.63126513886249,31.5905494329321));
#52396=CARTESIAN_POINT('Ctrl Pts',(29.3845192693535,-2.64898643883873,31.6070390220085));
#52397=CARTESIAN_POINT('Ctrl Pts',(29.3878847039265,-2.66692553831137,31.6237706303625));
#52398=CARTESIAN_POINT('',(29.3567901889011,-2.62540613538822,31.5905494329235));
#52399=CARTESIAN_POINT('Origin',(29.3676766176013,-2.63381649164654,31.5962056922849));
#52400=CARTESIAN_POINT('',(29.3346398644463,-2.65414258332839,31.6237706303691));
#52401=CARTESIAN_POINT('Ctrl Pts',(29.3346398644508,-2.65414258332263,31.6237706303626));
#52402=CARTESIAN_POINT('Ctrl Pts',(29.3457826693553,-2.63968660396658,31.6070390219952));
#52403=CARTESIAN_POINT('Ctrl Pts',(29.3567901889128,-2.62540613537299,31.5905494329059));
#52404=CARTESIAN_POINT('',(29.1805270849925,-2.61067828431429,31.6237706303691));
#52405=CARTESIAN_POINT('Origin',(30.,-1.32966554433622E-14,31.6237706303681));
#52406=CARTESIAN_POINT('',(29.1766555815127,-2.57460292188404,31.5905494329235));
#52407=CARTESIAN_POINT('Ctrl Pts',(29.1766555815137,-2.5746029218934,31.5905494329321));
#52408=CARTESIAN_POINT('Ctrl Pts',(29.1785795104532,-2.59253043613788,31.6070390220085));
#52409=CARTESIAN_POINT('Ctrl Pts',(29.1805270849917,-2.61067828430705,31.6237706303625));
#52410=CARTESIAN_POINT('',(29.1527859987874,-2.56684722431572,31.5905494329235));
#52411=CARTESIAN_POINT('Origin',(29.162979042241,-2.57608565616368,31.5962055274321));
#52412=CARTESIAN_POINT('',(29.1284493206708,-2.59375719295039,31.6237706303691));
#52413=CARTESIAN_POINT('Ctrl Pts',(29.1284493206757,-2.593757192945,31.6237706303625));
#52414=CARTESIAN_POINT('Ctrl Pts',(29.1406919790996,-2.58022003094555,31.6070390219952));
#52415=CARTESIAN_POINT('Ctrl Pts',(29.1527859988003,-2.56684722430145,31.5905494329059));
#52416=CARTESIAN_POINT('',(28.9782217890806,-2.53833533054863,31.6237706303691));
#52417=CARTESIAN_POINT('Origin',(30.,-1.32966554433622E-14,31.6237706303681));
#52418=CARTESIAN_POINT('',(28.9771926604683,-2.50206742175908,31.5905494329235));
#52419=CARTESIAN_POINT('Ctrl Pts',(28.9771926604686,-2.50206742176849,31.5905494329321));
#52420=CARTESIAN_POINT('Ctrl Pts',(28.9777040820209,-2.5200906211944,31.6070390220085));
#52421=CARTESIAN_POINT('Ctrl Pts',(28.9782217890804,-2.53833533054136,31.6237706303625));
#52422=CARTESIAN_POINT('',(28.9540051647184,-2.49246284654199,31.5905494329235));
#52423=CARTESIAN_POINT('Origin',(28.963441988931,-2.50247243285095,31.5962053997573));
#52424=CARTESIAN_POINT('',(28.9276321766534,-2.51738042696608,31.6237706303691));
#52425=CARTESIAN_POINT('Ctrl Pts',(28.9276321766587,-2.51738042696105,31.6237706303625));
#52426=CARTESIAN_POINT('Ctrl Pts',(28.9408992085416,-2.5048455434235,31.6070390219952));
#52427=CARTESIAN_POINT('Ctrl Pts',(28.9540051647323,-2.49246284652876,31.5905494329059));
#52428=CARTESIAN_POINT('',(28.7822160956147,-2.45034269538798,31.6237706303691));
#52429=CARTESIAN_POINT('Origin',(30.,-1.32966554433622E-14,31.6237706303681));
#52430=CARTESIAN_POINT('',(28.7840356867901,-2.41410584395713,31.5905494329235));
#52431=CARTESIAN_POINT('Ctrl Pts',(28.7840356867896,-2.41410584396654,31.5905494329321));
#52432=CARTESIAN_POINT('Ctrl Pts',(28.783131447871,-2.43211360955609,31.6070390220085));
#52433=CARTESIAN_POINT('Ctrl Pts',(28.7822160956151,-2.45034269538072,31.6237706303625));
#52434=CARTESIAN_POINT('',(28.7616732366375,-2.40271160649133,31.5905494329235));
#52435=CARTESIAN_POINT('Origin',(28.7702956661397,-2.41343066267495,31.5962052993351));
#52436=CARTESIAN_POINT('',(28.7334265368654,-2.42548317353557,31.6237706303691));
#52437=CARTESIAN_POINT('Ctrl Pts',(28.7334265368711,-2.425483173531,31.6237706303625));
#52438=CARTESIAN_POINT('Ctrl Pts',(28.7476361465498,-2.41402785018062,31.6070390219952));
#52439=CARTESIAN_POINT('Ctrl Pts',(28.7616732366525,-2.40271160647928,31.5905494329059));
#52440=CARTESIAN_POINT('',(28.5937184448736,-2.34724288268865,31.6237706303691));
#52441=CARTESIAN_POINT('Origin',(30.,-1.32966554433622E-14,31.6237706303681));
#52442=CARTESIAN_POINT('',(28.5983755374519,-2.31126050085552,31.5905494329235));
#52443=CARTESIAN_POINT('Ctrl Pts',(28.5983755374507,-2.31126050086484,31.5905494329321));
#52444=CARTESIAN_POINT('Ctrl Pts',(28.5960612129946,-2.32914180875499,31.6070390220085));
#52445=CARTESIAN_POINT('Ctrl Pts',(28.5937184448745,-2.34724288268142,31.6237706303625));
#52446=CARTESIAN_POINT('',(28.5769760048382,-2.29814685040397,31.5905494329235));
#52447=CARTESIAN_POINT('Origin',(28.5847308825473,-2.30950931155478,31.5962052196244));
#52448=CARTESIAN_POINT('',(28.547029743656,-2.31863200978522,31.6237706303691));
#52449=CARTESIAN_POINT('Ctrl Pts',(28.547029743662,-2.31863200978111,31.6237706303625));
#52450=CARTESIAN_POINT('Ctrl Pts',(28.5620943241676,-2.30832687249563,31.6070390219952));
#52451=CARTESIAN_POINT('Ctrl Pts',(28.5769760048541,-2.29814685039312,31.5905494329059));
#52452=CARTESIAN_POINT('',(28.413890987556,-2.22967153708007,31.6237706303691));
#52453=CARTESIAN_POINT('Origin',(30.,-1.32966554433622E-14,31.6237706303681));
#52454=CARTESIAN_POINT('',(28.4213568690129,-2.19416546819403,31.5905494329235));
#52455=CARTESIAN_POINT('Ctrl Pts',(28.421356869011,-2.19416546820326,31.5905494329321));
#52456=CARTESIAN_POINT('Ctrl Pts',(28.4176467275973,-2.21181007418472,31.6070390220085));
#52457=CARTESIAN_POINT('Ctrl Pts',(28.4138909875575,-2.22967153707296,31.6237706303625));
#52458=CARTESIAN_POINT('',(28.4010521891725,-2.17941325477249,31.5905494329235));
#52459=CARTESIAN_POINT('Origin',(28.407891704857,-2.19134908471608,31.596205156165));
#52460=CARTESIAN_POINT('',(28.3695909952386,-2.19748570867116,31.6237706303691));
#52461=CARTESIAN_POINT('Ctrl Pts',(28.3695909952449,-2.19748570866753,31.6237706303625));
#52462=CARTESIAN_POINT('Ctrl Pts',(28.3854176684292,-2.18839429204513,31.6070390219952));
#52463=CARTESIAN_POINT('Ctrl Pts',(28.4010521891892,-2.17941325476292,31.5905494329059));
#52464=CARTESIAN_POINT('',(28.2438424197348,-2.09835352500436,31.6237706303691));
#52465=CARTESIAN_POINT('Origin',(30.,-1.32966554433622E-14,31.6237706303681));
#52466=CARTESIAN_POINT('',(28.2540710604284,-2.06354267578707,31.5905494329235));
#52467=CARTESIAN_POINT('Ctrl Pts',(28.2540710604258,-2.0635426757961,31.5905494329321));
#52468=CARTESIAN_POINT('Ctrl Pts',(28.2489879763101,-2.08084179500557,31.6070390220085));
#52469=CARTESIAN_POINT('Ctrl Pts',(28.2438424197369,-2.09835352499738,31.6237706303625));
#52470=CARTESIAN_POINT('',(28.2349864184647,-2.04724285169689,31.5905494329235));
#52471=CARTESIAN_POINT('Origin',(28.2408684039783,-2.05967847590829,31.5962051058414));
#52472=CARTESIAN_POINT('',(28.2022042605016,-2.06279117742499,31.6237706303691));
#52473=CARTESIAN_POINT('Ctrl Pts',(28.2022042605082,-2.06279117742185,31.6237706303625));
#52474=CARTESIAN_POINT('Ctrl Pts',(28.2186954496679,-2.0549695330692,31.6070390219952));
#52475=CARTESIAN_POINT('Ctrl Pts',(28.2349864184821,-2.04724285168864,31.5905494329059));
#52476=CARTESIAN_POINT('',(28.0846211473776,-1.95409846567366,31.6237706303691));
#52477=CARTESIAN_POINT('Origin',(30.,-1.32966554433622E-14,31.6237706303681));
#52478=CARTESIAN_POINT('',(28.0975494843367,-1.92019745658631,31.5905494329235));
#52479=CARTESIAN_POINT('Ctrl Pts',(28.0975494843333,-1.92019745659509,31.5905494329321));
#52480=CARTESIAN_POINT('Ctrl Pts',(28.0911247964195,-1.93704443421011,31.6070390220085));
#52481=CARTESIAN_POINT('Ctrl Pts',(28.0846211473802,-1.95409846566685,31.6237706303626));
#52482=CARTESIAN_POINT('',(28.0798025434136,-1.90245051566325,31.5905494329235));
#52483=CARTESIAN_POINT('Origin',(28.0846907329876,-1.91530927561707,31.5962050664381));
#52484=CARTESIAN_POINT('',(28.0459015343263,-1.91537885262232,31.6237706303691));
#52485=CARTESIAN_POINT('Ctrl Pts',(28.0459015343331,-1.91537885261973,31.6237706303625));
#52486=CARTESIAN_POINT('Ctrl Pts',(28.0629555658034,-1.90887520357524,31.6070390219952));
#52487=CARTESIAN_POINT('Ctrl Pts',(28.0798025434316,-1.90245051565641,31.5905494329059));
#52488=CARTESIAN_POINT('',(27.937208822575,-1.79779573949839,31.6237706303691));
#52489=CARTESIAN_POINT('Origin',(30.,-1.32966554433622E-14,31.6237706303681));
#52490=CARTESIAN_POINT('',(27.9527571483031,-1.76501358153525,31.5905494329235));
#52491=CARTESIAN_POINT('Ctrl Pts',(27.9527571482991,-1.76501358154376,31.5905494329321));
#52492=CARTESIAN_POINT('Ctrl Pts',(27.9450304669246,-1.78130455034514,31.6070390220085));
#52493=CARTESIAN_POINT('Ctrl Pts',(27.9372088225781,-1.79779573949183,31.6237706303625));
#52494=CARTESIAN_POINT('',(27.9364573242129,-1.74592893957155,31.5905494329235));
#52495=CARTESIAN_POINT('Origin',(27.940321578254,-1.75913156587022,31.5962050363747));
#52496=CARTESIAN_POINT('',(27.9016464749956,-1.75615758026514,31.6237706303691));
#52497=CARTESIAN_POINT('Ctrl Pts',(27.9016464750026,-1.75615758026309,31.6237706303625));
#52498=CARTESIAN_POINT('Ctrl Pts',(27.9191582050083,-1.75101202368579,31.6070390219952));
#52499=CARTESIAN_POINT('Ctrl Pts',(27.9364573242313,-1.74592893956614,31.5905494329059));
#52500=CARTESIAN_POINT('',(27.8025142913288,-1.63040900476137,31.6237706303691));
#52501=CARTESIAN_POINT('Origin',(30.,-1.32966554433622E-14,31.6237706303681));
#52502=CARTESIAN_POINT('',(27.8205867452275,-1.59894781082744,31.5905494329235));
#52503=CARTESIAN_POINT('Ctrl Pts',(27.8205867452228,-1.59894781083561,31.5905494329321));
#52504=CARTESIAN_POINT('Ctrl Pts',(27.8116057079476,-1.61458233158338,31.6070390220085));
#52505=CARTESIAN_POINT('Ctrl Pts',(27.8025142913325,-1.63040900475507,31.6237706303625));
#52506=CARTESIAN_POINT('',(27.8058345318059,-1.5786431309871,31.5905494329235));
#52507=CARTESIAN_POINT('Origin',(27.8086510228583,-1.5921082324254,31.5962050145327));
#52508=CARTESIAN_POINT('',(27.7703284629199,-1.58610901244396,31.6237706303691));
#52509=CARTESIAN_POINT('Ctrl Pts',(27.770328462927,-1.58610901244246,31.6237706303625));
#52510=CARTESIAN_POINT('Ctrl Pts',(27.7881899258294,-1.58235327239973,31.6070390219952));
#52511=CARTESIAN_POINT('Ctrl Pts',(27.8058345318247,-1.57864313098315,31.5905494329059));
#52512=CARTESIAN_POINT('',(27.6813679902147,-1.45297025634398,31.6237706303691));
#52513=CARTESIAN_POINT('Origin',(30.,-1.32966554433622E-14,31.6237706303681));
#52514=CARTESIAN_POINT('',(27.701853149596,-1.42302399516179,31.5905494329235));
#52515=CARTESIAN_POINT('Ctrl Pts',(27.7018531495907,-1.42302399516956,31.5905494329321));
#52516=CARTESIAN_POINT('Ctrl Pts',(27.6916731274962,-1.43790567584432,31.6070390220085));
#52517=CARTESIAN_POINT('Ctrl Pts',(27.6813679902189,-1.45297025633799,31.6237706303626));
#52518=CARTESIAN_POINT('',(27.6887394991444,-1.40162446254801,31.5905494329235));
#52519=CARTESIAN_POINT('Origin',(27.6904908588872,-1.41526902814876,31.596205000146));
#52520=CARTESIAN_POINT('',(27.6527571173113,-1.4062815551263,31.6237706303691));
#52521=CARTESIAN_POINT('Ctrl Pts',(27.6527571173185,-1.40628155512537,31.6237706303626));
#52522=CARTESIAN_POINT('Ctrl Pts',(27.6708581912593,-1.40393878700346,31.6070390219953));
#52523=CARTESIAN_POINT('Ctrl Pts',(27.6887394991635,-1.40162446254554,31.5905494329059));
#52524=CARTESIAN_POINT('',(27.5745168264644,-1.2665734631346,31.6237706303691));
#52525=CARTESIAN_POINT('Origin',(30.,-1.32966554433622E-14,31.6237706303681));
#52526=CARTESIAN_POINT('',(27.5972883935086,-1.23832676336246,31.5905494329235));
#52527=CARTESIAN_POINT('Ctrl Pts',(27.5972883935027,-1.23832676336977,31.5905494329321));
#52528=CARTESIAN_POINT('Ctrl Pts',(27.5859721498102,-1.25236385346148,31.6070390220085));
#52529=CARTESIAN_POINT('Ctrl Pts',(27.574516826469,-1.2665734631289,31.6237706303626));
#52530=CARTESIAN_POINT('',(27.5858941560428,-1.21596431320988,31.5905494329235));
#52531=CARTESIAN_POINT('Origin',(27.5865695824296,-1.22970422416533,31.5962049927334));
#52532=CARTESIAN_POINT('',(27.549657304612,-1.21778390438522,31.6237706303691));
#52533=CARTESIAN_POINT('Ctrl Pts',(27.5496573046193,-1.21778390438485,31.6237706303625));
#52534=CARTESIAN_POINT('Ctrl Pts',(27.5678863904584,-1.2168685521283,31.6070390219952));
#52535=CARTESIAN_POINT('Ctrl Pts',(27.585894156062,-1.21596431320891,31.5905494329059));
#52536=CARTESIAN_POINT('',(27.4826195730339,-1.07236782334657,31.6237706303691));
#52537=CARTESIAN_POINT('Origin',(30.,-1.32966554433622E-14,31.6237706303681));
#52538=CARTESIAN_POINT('',(27.507537153458,-1.04599483528157,31.5905494329235));
#52539=CARTESIAN_POINT('Ctrl Pts',(27.5075371534515,-1.04599483528841,31.5905494329321));
#52540=CARTESIAN_POINT('Ctrl Pts',(27.4951544565665,-1.05910079146888,31.6070390220085));
#52541=CARTESIAN_POINT('Ctrl Pts',(27.4826195730389,-1.07236782334129,31.6237706303626));
#52542=CARTESIAN_POINT('',(27.4979325782409,-1.02280733953164,31.5905494329235));
#52543=CARTESIAN_POINT('Origin',(27.4975279021274,-1.03655788791105,31.5962049920587));
#52544=CARTESIAN_POINT('',(27.4616646694513,-1.02177821091936,31.6237706303691));
#52545=CARTESIAN_POINT('Ctrl Pts',(27.4616646694586,-1.02177821091956,31.6237706303626));
#52546=CARTESIAN_POINT('Ctrl Pts',(27.4799093788201,-1.02229591797942,31.6070390219952));
#52547=CARTESIAN_POINT('Ctrl Pts',(27.4979325782601,-1.02280733953218,31.5905494329059));
#52548=CARTESIAN_POINT('',(27.4062428070496,-0.871550679329129,31.6237706303691));
#52549=CARTESIAN_POINT('Origin',(30.,-1.32966554433622E-14,31.6237706303681));
#52550=CARTESIAN_POINT('',(27.4331527756843,-0.847214001212589,31.5905494329235));
#52551=CARTESIAN_POINT('Ctrl Pts',(27.4331527756773,-0.847214001218912,
31.5905494329321));
#52552=CARTESIAN_POINT('Ctrl Pts',(27.4197799690437,-0.859308020910092,
31.6070390220085));
#52553=CARTESIAN_POINT('Ctrl Pts',(27.406242807055,-0.871550679324261,31.6237706303625));
#52554=CARTESIAN_POINT('',(27.4253970781159,-0.823344418487241,31.5905494329235));
#52555=CARTESIAN_POINT('Origin',(27.4239147889674,-0.837020829522197,31.5962049981138));
#52556=CARTESIAN_POINT('',(27.3893217156857,-0.819472915007445,31.6237706303691));
#52557=CARTESIAN_POINT('Ctrl Pts',(27.3893217156929,-0.819472915008222,
31.6237706303625));
#52558=CARTESIAN_POINT('Ctrl Pts',(27.4074695638765,-0.821420489548307,
31.6070390219952));
#52559=CARTESIAN_POINT('Ctrl Pts',(27.425397078135,-0.823344418489291,31.590549432906));
#52560=CARTESIAN_POINT('',(27.3458574166716,-0.665360135553609,31.6237706303691));
#52561=CARTESIAN_POINT('Origin',(30.,-1.32966554433622E-14,31.6237706303681));
#52562=CARTESIAN_POINT('',(27.3745938646118,-0.643209811098888,31.5905494329235));
#52563=CARTESIAN_POINT('Ctrl Pts',(27.3745938646043,-0.643209811104637,
31.5905494329321));
#52564=CARTESIAN_POINT('Ctrl Pts',(27.3603133960219,-0.65421733065347,31.6070390220085));
#52565=CARTESIAN_POINT('Ctrl Pts',(27.3458574166774,-0.665360135549176,
31.6237706303625));
#52566=CARTESIAN_POINT('',(27.3687348611467,-0.618805305313063,31.5905494329235));
#52567=CARTESIAN_POINT('Origin',(27.3661840916659,-0.632323260043008,31.5962050111235));
#52568=CARTESIAN_POINT('',(27.3330744616815,-0.612115296072114,31.6237706303691));
#52569=CARTESIAN_POINT('Ctrl Pts',(27.3330744616886,-0.612115296073467,
31.6237706303625));
#52570=CARTESIAN_POINT('Ctrl Pts',(27.3510135611755,-0.615480730649101,
31.6070390219952));
#52571=CARTESIAN_POINT('Ctrl Pts',(27.3687348611656,-0.61880530531661,31.590549432906));
#52572=CARTESIAN_POINT('',(27.3018356979118,-0.455067425287704,31.6237706303691));
#52573=CARTESIAN_POINT('Origin',(30.,-1.32966554433622E-14,31.6237706303681));
#52574=CARTESIAN_POINT('',(27.3322214554001,-0.435240018610796,31.5905494329235));
#52575=CARTESIAN_POINT('Ctrl Pts',(27.3322214553922,-0.435240018615941,
31.5905494329321));
#52576=CARTESIAN_POINT('Ctrl Pts',(27.3171213686986,-0.445093173004034,
31.6070390220085));
#52577=CARTESIAN_POINT('Ctrl Pts',(27.3018356979179,-0.455067425283735,
31.6237706303625));
#52578=CARTESIAN_POINT('',(27.328295268743,-0.410451051657984,31.5905494329235));
#52579=CARTESIAN_POINT('Origin',(27.3246917385075,-0.423727206709274,31.5962050315749));
#52580=CARTESIAN_POINT('',(27.2932696904637,-0.400983782787508,31.6237706303691));
#52581=CARTESIAN_POINT('Ctrl Pts',(27.2932696904707,-0.400983782789399,
31.6237706303625));
#52582=CARTESIAN_POINT('Ctrl Pts',(27.3108894407472,-0.405746328377308,
31.6070390219952));
#52583=CARTESIAN_POINT('Ctrl Pts',(27.3282952687616,-0.410451051662988,
31.5905494329059));
#52584=CARTESIAN_POINT('',(27.274449059305,-0.241969073019628,31.6237706303691));
#52585=CARTESIAN_POINT('Origin',(30.,-1.32966554433622E-14,31.6237706303681));
#52586=CARTESIAN_POINT('',(27.3062967880422,-0.224586826675978,31.5905494329235));
#52587=CARTESIAN_POINT('Ctrl Pts',(27.306296788034,-0.224586826680481,31.5905494329321));
#52588=CARTESIAN_POINT('Ctrl Pts',(27.2904701802848,-0.233224867934527,
31.6070390220085));
#52589=CARTESIAN_POINT('Ctrl Pts',(27.2744490593114,-0.241969073016143,
31.6237706303626));
#52590=CARTESIAN_POINT('',(27.3043276244395,-0.199566230780611,31.5905494329235));
#52591=CARTESIAN_POINT('Origin',(27.2996935428802,-0.212518732061225,31.5962050602856));
#52592=CARTESIAN_POINT('',(27.2701528116834,-0.18738007114138,31.6237706303691));
#52593=CARTESIAN_POINT('Ctrl Pts',(27.2701528116903,-0.187380071143839,
31.6237706303625));
#52594=CARTESIAN_POINT('Ctrl Pts',(27.2873445811368,-0.193510365066767,
31.6070390219952));
#52595=CARTESIAN_POINT('Ctrl Pts',(27.3043276244576,-0.199566230787083,
31.5905494329059));
#52596=CARTESIAN_POINT('',(27.2638663485853,-0.027378900953502,31.6237706303691));
#52597=CARTESIAN_POINT('Origin',(30.,-1.32966554433622E-14,31.6237706303681));
#52598=CARTESIAN_POINT('Ctrl Pts',(27.2969796967247,-0.0125489822758455,
31.5905494329321));
#52599=CARTESIAN_POINT('Ctrl Pts',(27.2805241442198,-0.0199186539990725,
31.6070390220085));
#52600=CARTESIAN_POINT('Ctrl Pts',(27.263866348592,-0.0273789009505331,
31.6237706303626));
#52601=CARTESIAN_POINT('',(27.2638663485853,0.0273789009535324,31.6237706303691));
#52602=CARTESIAN_POINT('Ctrl Pts',(27.263866348592,0.0273789009505529,31.6237706303626));
#52603=CARTESIAN_POINT('Ctrl Pts',(27.280524144233,0.0199186539931685,31.6070390219952));
#52604=CARTESIAN_POINT('Ctrl Pts',(27.2969796967508,0.012548982264161,31.5905494329059));
#52605=CARTESIAN_POINT('',(27.2701528116834,0.187380071141411,31.6237706303691));
#52606=CARTESIAN_POINT('Origin',(30.,-1.32966554433622E-14,31.6237706303681));
#52607=CARTESIAN_POINT('Ctrl Pts',(27.3043276244306,0.199566230777481,31.5905494329321));
#52608=CARTESIAN_POINT('Ctrl Pts',(27.2873445811231,0.193510365061917,31.6070390220085));
#52609=CARTESIAN_POINT('Ctrl Pts',(27.2701528116902,0.187380071143857,31.6237706303625));
#52610=CARTESIAN_POINT('',(27.2744490593051,0.241969073019658,31.6237706303691));
#52611=CARTESIAN_POINT('Ctrl Pts',(27.2744490593115,0.241969073016152,31.6237706303625));
#52612=CARTESIAN_POINT('Ctrl Pts',(27.2904701802976,0.233224867927605,31.6070390219952));
#52613=CARTESIAN_POINT('Ctrl Pts',(27.3062967880591,0.224586826666795,31.5905494329059));
#52614=CARTESIAN_POINT('',(27.2932696904637,0.40098378278754,31.6237706303691));
#52615=CARTESIAN_POINT('Origin',(30.,-1.32966554433622E-14,31.6237706303681));
#52616=CARTESIAN_POINT('Ctrl Pts',(27.3282952687339,0.410451051655568,31.5905494329321));
#52617=CARTESIAN_POINT('Ctrl Pts',(27.3108894407332,0.405746328373579,31.6070390220085));
#52618=CARTESIAN_POINT('Ctrl Pts',(27.2932696904707,0.400983782789452,31.6237706303626));
#52619=CARTESIAN_POINT('',(27.3018356979118,0.455067425287736,31.6237706303691));
#52620=CARTESIAN_POINT('Ctrl Pts',(27.3018356979179,0.455067425283746,31.6237706303626));
#52621=CARTESIAN_POINT('Ctrl Pts',(27.3171213687107,0.445093172996126,31.6070390219952));
#52622=CARTESIAN_POINT('Ctrl Pts',(27.3322214554162,0.435240018600305,31.5905494329059));
#52623=CARTESIAN_POINT('',(27.3330744616815,0.612115296072143,31.6237706303691));
#52624=CARTESIAN_POINT('Origin',(30.,-1.32966554433622E-14,31.6237706303681));
#52625=CARTESIAN_POINT('Ctrl Pts',(27.3687348611375,0.618805305311351,31.5905494329321));
#52626=CARTESIAN_POINT('Ctrl Pts',(27.3510135611613,0.615480730646445,31.6070390220085));
#52627=CARTESIAN_POINT('Ctrl Pts',(27.3330744616886,0.612115296073478,31.6237706303625));
#52628=CARTESIAN_POINT('',(27.3458574166716,0.665360135553637,31.6237706303691));
#52629=CARTESIAN_POINT('Ctrl Pts',(27.3458574166774,0.665360135549173,31.6237706303626));
#52630=CARTESIAN_POINT('Ctrl Pts',(27.3603133960334,0.65421733064462,31.6070390219952));
#52631=CARTESIAN_POINT('Ctrl Pts',(27.374593864627,0.643209811087154,31.5905494329059));
#52632=CARTESIAN_POINT('',(27.3893217156857,0.819472915007473,31.6237706303691));
#52633=CARTESIAN_POINT('Origin',(30.,-1.32966554433622E-14,31.6237706303681));
#52634=CARTESIAN_POINT('Ctrl Pts',(27.4253970781066,0.823344418486268,31.5905494329322));
#52635=CARTESIAN_POINT('Ctrl Pts',(27.4074695638621,0.821420489546793,31.6070390220085));
#52636=CARTESIAN_POINT('Ctrl Pts',(27.3893217156929,0.819472915008255,31.6237706303625));
#52637=CARTESIAN_POINT('',(27.4062428070496,0.871550679329156,31.6237706303691));
#52638=CARTESIAN_POINT('Ctrl Pts',(27.406242807055,0.87155067932429,31.6237706303625));
#52639=CARTESIAN_POINT('Ctrl Pts',(27.4197799690545,0.8593080209004,31.6070390219952));
#52640=CARTESIAN_POINT('Ctrl Pts',(27.4331527756986,0.847214001199735,31.5905494329059));
#52641=CARTESIAN_POINT('',(27.4616646694514,1.02177821091938,31.6237706303691));
#52642=CARTESIAN_POINT('Origin',(30.,-1.32966554433622E-14,31.6237706303681));
#52643=CARTESIAN_POINT('Ctrl Pts',(27.4979325782315,1.0228073395314,31.5905494329321));
#52644=CARTESIAN_POINT('Ctrl Pts',(27.4799093788056,1.02229591797904,31.6070390220085));
#52645=CARTESIAN_POINT('Ctrl Pts',(27.4616646694587,1.02177821091959,31.6237706303625));
#52646=CARTESIAN_POINT('',(27.4826195730339,1.0723678233466,31.6237706303691));
#52647=CARTESIAN_POINT('Ctrl Pts',(27.4826195730389,1.0723678233413,31.6237706303626));
#52648=CARTESIAN_POINT('Ctrl Pts',(27.4951544565765,1.05910079145835,31.6070390219952));
#52649=CARTESIAN_POINT('Ctrl Pts',(27.5075371534712,1.04599483526761,31.5905494329059));
#52650=CARTESIAN_POINT('',(27.549657304612,1.21778390438524,31.6237706303691));
#52651=CARTESIAN_POINT('Origin',(30.,-1.32966554433622E-14,31.6237706303681));
#52652=CARTESIAN_POINT('Ctrl Pts',(27.5858941560335,1.21596431321037,31.5905494329321));
#52653=CARTESIAN_POINT('Ctrl Pts',(27.5678863904439,1.21686855212906,31.6070390220085));
#52654=CARTESIAN_POINT('Ctrl Pts',(27.5496573046193,1.21778390438488,31.6237706303626));
#52655=CARTESIAN_POINT('',(27.5745168264644,1.26657346313462,31.6237706303691));
#52656=CARTESIAN_POINT('Ctrl Pts',(27.574516826469,1.26657346312892,31.6237706303626));
#52657=CARTESIAN_POINT('Ctrl Pts',(27.5859721498194,1.25236385345021,31.6070390219952));
#52658=CARTESIAN_POINT('Ctrl Pts',(27.5972883935207,1.23832676334747,31.5905494329059));
#52659=CARTESIAN_POINT('',(27.6527571173114,1.40628155512632,31.6237706303691));
#52660=CARTESIAN_POINT('Origin',(30.,-1.32966554433622E-14,31.6237706303681));
#52661=CARTESIAN_POINT('Ctrl Pts',(27.6887394991352,1.40162446254924,31.5905494329321));
#52662=CARTESIAN_POINT('Ctrl Pts',(27.670858191245,1.40393878700535,31.6070390220085));
#52663=CARTESIAN_POINT('Ctrl Pts',(27.6527571173186,1.40628155512539,31.6237706303625));
#52664=CARTESIAN_POINT('',(27.6813679902148,1.45297025634401,31.6237706303691));
#52665=CARTESIAN_POINT('Ctrl Pts',(27.6813679902189,1.452970256338,31.6237706303625));
#52666=CARTESIAN_POINT('Ctrl Pts',(27.6916731275044,1.43790567583238,31.6070390219952));
#52667=CARTESIAN_POINT('Ctrl Pts',(27.7018531496069,1.42302399514596,31.5905494329059));
#52668=CARTESIAN_POINT('',(27.7703284629199,1.58610901244398,31.6237706303691));
#52669=CARTESIAN_POINT('Origin',(30.,-1.32966554433622E-14,31.6237706303681));
#52670=CARTESIAN_POINT('Ctrl Pts',(27.8058345317968,1.57864313098906,31.5905494329321));
#52671=CARTESIAN_POINT('Ctrl Pts',(27.7881899258153,1.58235327240273,31.6070390220085));
#52672=CARTESIAN_POINT('Ctrl Pts',(27.770328462927,1.58610901244249,31.6237706303626));
#52673=CARTESIAN_POINT('',(27.8025142913288,1.63040900476139,31.6237706303691));
#52674=CARTESIAN_POINT('Ctrl Pts',(27.8025142913324,1.63040900475507,31.6237706303626));
#52675=CARTESIAN_POINT('Ctrl Pts',(27.8116057079549,1.61458233157081,31.6070390219952));
#52676=CARTESIAN_POINT('Ctrl Pts',(27.8205867452371,1.59894781081078,31.5905494329059));
#52677=CARTESIAN_POINT('',(27.9016464749956,1.75615758026516,31.6237706303691));
#52678=CARTESIAN_POINT('Origin',(30.,-1.32966554433622E-14,31.6237706303681));
#52679=CARTESIAN_POINT('Ctrl Pts',(27.9364573242039,1.74592893957422,31.5905494329321));
#52680=CARTESIAN_POINT('Ctrl Pts',(27.9191582049944,1.75101202368989,31.6070390220085));
#52681=CARTESIAN_POINT('Ctrl Pts',(27.9016464750026,1.7561575802631,31.6237706303626));
#52682=CARTESIAN_POINT('',(27.937208822575,1.79779573949841,31.6237706303691));
#52683=CARTESIAN_POINT('Ctrl Pts',(27.9372088225781,1.79779573949182,31.6237706303625));
#52684=CARTESIAN_POINT('Ctrl Pts',(27.9450304669308,1.78130455033204,31.6070390219952));
#52685=CARTESIAN_POINT('Ctrl Pts',(27.9527571483113,1.76501358151789,31.5905494329059));
#52686=CARTESIAN_POINT('',(28.0459015343263,1.91537885262234,31.6237706303691));
#52687=CARTESIAN_POINT('Origin',(30.,-1.32966554433622E-14,31.6237706303681));
#52688=CARTESIAN_POINT('Ctrl Pts',(28.0798025434049,1.90245051566662,31.5905494329321));
#52689=CARTESIAN_POINT('Ctrl Pts',(28.0629555657899,1.90887520358041,31.6070390220085));
#52690=CARTESIAN_POINT('Ctrl Pts',(28.0459015343331,1.91537885261975,31.6237706303626));
#52691=CARTESIAN_POINT('',(28.0846211473777,1.95409846567367,31.6237706303691));
#52692=CARTESIAN_POINT('Ctrl Pts',(28.0846211473803,1.95409846566688,31.6237706303625));
#52693=CARTESIAN_POINT('Ctrl Pts',(28.0911247964248,1.93704443419661,31.6070390219952));
#52694=CARTESIAN_POINT('Ctrl Pts',(28.0975494843436,1.9201974565684,31.5905494329059));
#52695=CARTESIAN_POINT('',(28.2022042605016,2.062791177425,31.6237706303691));
#52696=CARTESIAN_POINT('Origin',(30.,-1.32966554433622E-14,31.6237706303681));
#52697=CARTESIAN_POINT('Ctrl Pts',(28.2349864184563,2.04724285170094,31.5905494329321));
#52698=CARTESIAN_POINT('Ctrl Pts',(28.2186954496549,2.05496953307545,31.6070390220085));
#52699=CARTESIAN_POINT('Ctrl Pts',(28.2022042605082,2.0627911774219,31.6237706303626));
#52700=CARTESIAN_POINT('',(28.2438424197349,2.09835352500437,31.6237706303691));
#52701=CARTESIAN_POINT('Ctrl Pts',(28.2438424197369,2.09835352499738,31.6237706303625));
#52702=CARTESIAN_POINT('Ctrl Pts',(28.2489879763142,2.08084179499167,31.6070390219952));
#52703=CARTESIAN_POINT('Ctrl Pts',(28.2540710604339,2.06354267576863,31.5905494329059));
#52704=CARTESIAN_POINT('',(28.3695909952386,2.19748570867117,31.6237706303691));
#52705=CARTESIAN_POINT('Origin',(30.,-1.32966554433622E-14,31.6237706303681));
#52706=CARTESIAN_POINT('Ctrl Pts',(28.4010521891644,2.17941325477719,31.5905494329321));
#52707=CARTESIAN_POINT('Ctrl Pts',(28.3854176684167,2.18839429205237,31.6070390220085));
#52708=CARTESIAN_POINT('Ctrl Pts',(28.369590995245,2.19748570866756,31.6237706303626));
#52709=CARTESIAN_POINT('',(28.413890987556,2.22967153708007,31.6237706303691));
#52710=CARTESIAN_POINT('Ctrl Pts',(28.4138909875575,2.22967153707294,31.6237706303625));
#52711=CARTESIAN_POINT('Ctrl Pts',(28.4176467276003,2.21181007417053,31.6070390219952));
#52712=CARTESIAN_POINT('Ctrl Pts',(28.4213568690169,2.19416546817523,31.5905494329059));
#52713=CARTESIAN_POINT('',(28.547029743656,2.31863200978522,31.6237706303691));
#52714=CARTESIAN_POINT('Origin',(30.,-1.32966554433622E-14,31.6237706303681));
#52715=CARTESIAN_POINT('Ctrl Pts',(28.5769760048304,2.29814685040929,31.5905494329321));
#52716=CARTESIAN_POINT('Ctrl Pts',(28.5620943241557,2.30832687250382,31.6070390220085));
#52717=CARTESIAN_POINT('Ctrl Pts',(28.547029743662,2.31863200978111,31.6237706303625));
#52718=CARTESIAN_POINT('',(28.5937184448737,2.34724288268865,31.6237706303691));
#52719=CARTESIAN_POINT('Ctrl Pts',(28.5937184448746,2.34724288268143,31.6237706303626));
#52720=CARTESIAN_POINT('Ctrl Pts',(28.5960612129965,2.32914180874063,31.6070390219952));
#52721=CARTESIAN_POINT('Ctrl Pts',(28.5983755374545,2.31126050083645,31.5905494329059));
#52722=CARTESIAN_POINT('',(28.7334265368654,2.42548317353557,31.6237706303691));
#52723=CARTESIAN_POINT('Origin',(30.,-1.32966554433622E-14,31.6237706303681));
#52724=CARTESIAN_POINT('Ctrl Pts',(28.7616732366302,2.40271160649724,31.5905494329321));
#52725=CARTESIAN_POINT('Ctrl Pts',(28.7476361465385,2.4140278501897,31.6070390220085));
#52726=CARTESIAN_POINT('Ctrl Pts',(28.7334265368711,2.42548317353099,31.6237706303625));
#52727=CARTESIAN_POINT('',(28.7822160956148,2.45034269538798,31.6237706303691));
#52728=CARTESIAN_POINT('Ctrl Pts',(28.7822160956151,2.45034269538071,31.6237706303626));
#52729=CARTESIAN_POINT('Ctrl Pts',(28.7831314478717,2.4321136095416,31.6070390219952));
#52730=CARTESIAN_POINT('Ctrl Pts',(28.7840356867911,2.41410584393792,31.5905494329059));
#52731=CARTESIAN_POINT('',(28.9276321766534,2.51738042696607,31.6237706303691));
#52732=CARTESIAN_POINT('Origin',(30.,-1.32966554433622E-14,31.6237706303681));
#52733=CARTESIAN_POINT('',(28.9540051647184,2.49246284654199,31.5905494329235));
#52734=CARTESIAN_POINT('Ctrl Pts',(28.9540051647116,2.49246284654845,31.5905494329321));
#52735=CARTESIAN_POINT('Ctrl Pts',(28.9408992085311,2.50484554343346,31.6070390220085));
#52736=CARTESIAN_POINT('Ctrl Pts',(28.9276321766587,2.51738042696107,31.6237706303625));
#52737=CARTESIAN_POINT('',(28.9771926604684,2.50206742175908,31.5905494329235));
#52738=CARTESIAN_POINT('Origin',(28.9634421120889,2.50247209787257,31.5962049920587));
#52739=CARTESIAN_POINT('',(28.9782217890806,2.53833533054862,31.6237706303691));
#52740=CARTESIAN_POINT('Ctrl Pts',(28.9782217890804,2.53833533054134,31.6237706303625));
#52741=CARTESIAN_POINT('Ctrl Pts',(28.9777040820206,2.52009062117991,31.6070390219952));
#52742=CARTESIAN_POINT('Ctrl Pts',(28.9771926604678,2.50206742173986,31.5905494329059));
#52743=CARTESIAN_POINT('',(29.1284493206709,2.59375719295039,31.6237706303691));
#52744=CARTESIAN_POINT('Origin',(30.,-1.32966554433622E-14,31.6237706303681));
#52745=CARTESIAN_POINT('',(29.1527859987874,2.56684722431571,31.5905494329235));
#52746=CARTESIAN_POINT('Ctrl Pts',(29.1527859987811,2.56684722432269,31.5905494329321));
#52747=CARTESIAN_POINT('Ctrl Pts',(29.1406919790899,2.58022003095629,31.6070390220085));
#52748=CARTESIAN_POINT('Ctrl Pts',(29.1284493206758,2.59375719294498,31.6237706303625));
#52749=CARTESIAN_POINT('',(29.1766555815128,2.57460292188403,31.5905494329235));
#52750=CARTESIAN_POINT('Origin',(29.1629791704778,2.57608521103256,31.5962049981139));
#52751=CARTESIAN_POINT('',(29.1805270849926,2.61067828431428,31.6237706303691));
#52752=CARTESIAN_POINT('Ctrl Pts',(29.1805270849917,2.61067828430704,31.6237706303626));
#52753=CARTESIAN_POINT('Ctrl Pts',(29.1785795104516,2.59253043612347,31.6070390219952));
#52754=CARTESIAN_POINT('Ctrl Pts',(29.1766555815107,2.57460292186492,31.5905494329059));
#52755=CARTESIAN_POINT('',(29.3346398644464,2.65414258332837,31.6237706303691));
#52756=CARTESIAN_POINT('Origin',(30.,-1.32966554433622E-14,31.6237706303681));
#52757=CARTESIAN_POINT('',(29.3567901889011,2.6254061353882,31.5905494329235));
#52758=CARTESIAN_POINT('Ctrl Pts',(29.3567901888954,2.62540613539565,31.5905494329321));
#52759=CARTESIAN_POINT('Ctrl Pts',(29.3457826693465,2.63968660397804,31.6070390220085));
#52760=CARTESIAN_POINT('Ctrl Pts',(29.3346398644508,2.6541425833226,31.6237706303625));
#52761=CARTESIAN_POINT('',(29.3811946946869,2.63126513885323,31.5905494329235));
#52762=CARTESIAN_POINT('Origin',(29.367676739957,2.63381590833401,31.5962050111235));
#52763=CARTESIAN_POINT('',(29.3878847039279,2.66692553831851,31.6237706303691));
#52764=CARTESIAN_POINT('Ctrl Pts',(29.3878847039265,2.66692553831136,31.6237706303626));
#52765=CARTESIAN_POINT('Ctrl Pts',(29.3845192693509,2.64898643882447,31.6070390219952));
#52766=CARTESIAN_POINT('Ctrl Pts',(29.3811946946833,2.63126513883434,31.5905494329059));
#52767=CARTESIAN_POINT('',(29.5449325747123,2.69816430208817,31.6237706303691));
#52768=CARTESIAN_POINT('Origin',(30.,-1.32966554433622E-14,31.6237706303681));
#52769=CARTESIAN_POINT('',(29.5647599813892,2.6677785445999,31.5905494329235));
#52770=CARTESIAN_POINT('Ctrl Pts',(29.5647599813841,2.66777854460778,31.5905494329321));
#52771=CARTESIAN_POINT('Ctrl Pts',(29.554906826996,2.6828786313014,31.6070390220085));
#52772=CARTESIAN_POINT('Ctrl Pts',(29.5449325747163,2.69816430208207,31.6237706303625));
#52773=CARTESIAN_POINT('',(29.589548948342,2.67170473125694,31.5905494329235));
#52774=CARTESIAN_POINT('Origin',(29.5762727932907,2.67530826149244,31.5962050315749));
#52775=CARTESIAN_POINT('',(29.5990162172125,2.70673030953627,31.6237706303691));
#52776=CARTESIAN_POINT('Ctrl Pts',(29.5990162172106,2.70673030952925,31.6237706303625));
#52777=CARTESIAN_POINT('Ctrl Pts',(29.5942536716227,2.68911055925274,31.6070390219952));
#52778=CARTESIAN_POINT('Ctrl Pts',(29.589548948337,2.67170473123838,31.5905494329059));
#52779=CARTESIAN_POINT('',(29.7580309269804,2.72555094069491,31.6237706303691));
#52780=CARTESIAN_POINT('Origin',(30.,-1.32966554433622E-14,31.6237706303681));
#52781=CARTESIAN_POINT('',(29.775413173324,2.69370321195775,31.5905494329235));
#52782=CARTESIAN_POINT('Ctrl Pts',(29.7754131733195,2.69370321196601,31.5905494329321));
#52783=CARTESIAN_POINT('Ctrl Pts',(29.7667751320655,2.7095298197151,31.6070390220085));
#52784=CARTESIAN_POINT('Ctrl Pts',(29.7580309269838,2.72555094068851,31.6237706303625));
#52785=CARTESIAN_POINT('',(29.8004337692194,2.69567237556048,31.5905494329235));
#52786=CARTESIAN_POINT('Origin',(29.7874812679388,2.70030645711977,31.5962050602857));
#52787=CARTESIAN_POINT('',(29.8126199288586,2.72984718831658,31.6237706303691));
#52788=CARTESIAN_POINT('Ctrl Pts',(29.8126199288562,2.72984718830972,31.6237706303625));
#52789=CARTESIAN_POINT('Ctrl Pts',(29.8064896349333,2.71265541886322,31.6070390219952));
#52790=CARTESIAN_POINT('Ctrl Pts',(29.800433769213,2.69567237554238,31.5905494329059));
#52791=CARTESIAN_POINT('',(29.9726210990465,2.73613365141461,31.6237706303691));
#52792=CARTESIAN_POINT('Origin',(30.,-1.32966554433622E-14,31.6237706303681));
#52793=CARTESIAN_POINT('',(29.987451017728,2.70302030326666,31.5905494329235));
#52794=CARTESIAN_POINT('Ctrl Pts',(29.9874510177241,2.70302030327525,31.5905494329321));
#52795=CARTESIAN_POINT('Ctrl Pts',(29.9800813460009,2.71947585578017,31.6070390220085));
#52796=CARTESIAN_POINT('Ctrl Pts',(29.9726210990495,2.73613365140797,31.6237706303625));
#52797=CARTESIAN_POINT('Ctrl Pts',(30.,2.69489040503946,31.5823904050395));
#52798=CARTESIAN_POINT('Ctrl Pts',(29.9982996971592,2.69489040503946,31.5823904050395));
#52799=CARTESIAN_POINT('Ctrl Pts',(29.9965490639354,2.69522714758866,31.5827289231894));
#52800=CARTESIAN_POINT('Ctrl Pts',(29.9934248389279,2.69644647069982,31.5839540167345));
#52801=CARTESIAN_POINT('Ctrl Pts',(29.9920523583067,2.69733049287039,31.5848419899159));
#52802=CARTESIAN_POINT('Ctrl Pts',(29.9894391186861,2.6996015700298,31.5871217896387));
#52803=CARTESIAN_POINT('Ctrl Pts',(29.9882404972758,2.70125749446876,31.5887829779419));
#52804=CARTESIAN_POINT('Ctrl Pts',(29.987451017728,2.70302030326666,31.5905494329235));
#52805=CARTESIAN_POINT('',(30.,2.68872936963187,31.5762293696319));
#52806=CARTESIAN_POINT('',(30.,2.68872936963187,31.5762293696319));
#52807=CARTESIAN_POINT('',(30.,-2.68872936963189,31.5762293696319));
#52808=CARTESIAN_POINT('Origin',(30.,-1.32966554433622E-14,31.5762293696319));
#52809=CARTESIAN_POINT('Origin',(30.,-1.32966554433622E-14,31.5762293696319));
#52810=CARTESIAN_POINT('Origin',(30.,-1.32966554433622E-14,31.5430837392638));
#52811=CARTESIAN_POINT('',(30.,-2.67500000000001,31.5430837392638));
#52812=CARTESIAN_POINT('Origin',(30.,-1.32966554433622E-14,31.5430837392638));
#52813=CARTESIAN_POINT('Origin',(30.,-2.72187500000001,31.5430837392638));
#52814=CARTESIAN_POINT('Origin',(30.,-1.32966554433622E-14,16.));
#52815=CARTESIAN_POINT('',(30.,-2.67500000000001,31.06875));
#52816=CARTESIAN_POINT('Origin',(30.,-1.32966554433622E-14,31.06875));
#52817=CARTESIAN_POINT('',(30.,-2.67500000000001,16.));
#52818=CARTESIAN_POINT('Origin',(30.,-1.32966554433622E-14,31.06875));
#52819=CARTESIAN_POINT('',(30.,-2.60625000000001,31.));
#52820=CARTESIAN_POINT('Origin',(30.,-1.32966554433622E-14,31.));
#52821=CARTESIAN_POINT('Origin',(30.,-2.60625000000001,31.06875));
#52822=CARTESIAN_POINT('Origin',(30.,-1.32966554433622E-14,30.85));
#52823=CARTESIAN_POINT('',(30.,-1.65000000000002,31.));
#52824=CARTESIAN_POINT('Origin',(30.,-1.65000000000001,30.85));
#52825=CARTESIAN_POINT('Origin',(30.,-1.32966554433622E-14,31.));
#52826=CARTESIAN_POINT('Origin',(30.,-1.32966554433622E-14,31.6569162607362));
#52827=CARTESIAN_POINT('',(27.4723387620945,1.08324912480478,31.6569162607362));
#52828=CARTESIAN_POINT('Origin',(27.5075595450194,1.04598613791953,31.6570432561871));
#52829=CARTESIAN_POINT('',(27.5347062454699,1.21853465435945,31.6569162607362));
#52830=CARTESIAN_POINT('Origin',(30.,-1.32966554433622E-14,31.6569162607362));
#52831=CARTESIAN_POINT('Origin',(27.5859112932463,1.21595145595199,31.6570220656254));
#52832=CARTESIAN_POINT('Origin',(30.,-1.32966554433622E-14,31.6569162607362));
#52833=CARTESIAN_POINT('',(27.4467007962708,1.0213536000015,31.6569162607362));
#52834=CARTESIAN_POINT('Origin',(27.4979506713832,1.02279586647784,31.6570220656247));
#52835=CARTESIAN_POINT('',(27.3951399513465,0.881591814236737,31.6569162607362));
#52836=CARTESIAN_POINT('Origin',(27.4331757806072,0.847207087483285,31.6570432561871));
#52837=CARTESIAN_POINT('Origin',(30.,-1.32966554433622E-14,31.6569162607362));
#52838=CARTESIAN_POINT('Origin',(30.,-1.32966554433622E-14,31.6569162607362));
#52839=CARTESIAN_POINT('',(27.3744372857209,0.817875561065013,31.6569162607362));
#52840=CARTESIAN_POINT('Origin',(27.4254160156494,0.82333440037271,31.6570220656251));
#52841=CARTESIAN_POINT('',(27.3340009690024,0.674499196974899,31.6569162607362));
#52842=CARTESIAN_POINT('Origin',(27.3746173410621,0.643204723628532,31.6570432561866));
#52843=CARTESIAN_POINT('Origin',(30.,-1.32966554433622E-14,31.6569162607362));
#52844=CARTESIAN_POINT('Origin',(30.,-1.32966554433622E-14,31.6569162607362));
#52845=CARTESIAN_POINT('',(27.3183612423927,0.609355047323335,31.6569162607362));
#52846=CARTESIAN_POINT('Origin',(27.3687545263143,0.61879680390278,31.6570220656251));
#52847=CARTESIAN_POINT('',(27.2892987572189,0.463248067869971,31.6569162607362));
#52848=CARTESIAN_POINT('Origin',(27.3322452586394,0.435236788764015,31.6570432561869));
#52849=CARTESIAN_POINT('Origin',(30.,-1.32966554433622E-14,31.6569162607362));
#52850=CARTESIAN_POINT('Origin',(30.,-1.32966554433622E-14,31.6569162607362));
#52851=CARTESIAN_POINT('',(27.2788183937405,0.397077657083795,31.6569162607362));
#52852=CARTESIAN_POINT('Origin',(27.3283155403022,0.41044411936593,31.6570220656249));
#52853=CARTESIAN_POINT('',(27.2613089199969,0.249140860381007,31.6569162607362));
#52854=CARTESIAN_POINT('Origin',(27.3063207713152,0.224585474366194,31.6570432561871));
#52855=CARTESIAN_POINT('Origin',(30.,-1.32966554433622E-14,31.6569162607362));
#52856=CARTESIAN_POINT('Origin',(30.,-1.32966554433622E-14,31.6569162607362));
#52857=CARTESIAN_POINT('',(27.2560525345756,0.182352151046611,31.6569162607362));
#52858=CARTESIAN_POINT('Origin',(27.3043483774102,0.199560910346922,31.6570220656251));
#52859=CARTESIAN_POINT('',(27.2502040239902,0.0334976166400503,31.6569162607362));
#52860=CARTESIAN_POINT('Origin',(27.2970037121761,0.0125495158363338,31.6570432561875));
#52861=CARTESIAN_POINT('Origin',(30.,-1.32966554433622E-14,31.6569162607362));
#52862=CARTESIAN_POINT('Origin',(30.,-1.32966554433622E-14,31.6569162607362));
#52863=CARTESIAN_POINT('',(27.2502040239902,-0.0334976166400194,31.6569162607362));
#52864=CARTESIAN_POINT('Origin',(27.297000803166,-0.0125526580452972,31.6570220656252));
#52865=CARTESIAN_POINT('',(27.2560525345756,-0.18235215104658,31.6569162607362));
#52866=CARTESIAN_POINT('Origin',(27.3043515239857,-0.199563814630509,31.6570432561868));
#52867=CARTESIAN_POINT('Origin',(30.,-1.32966554433622E-14,31.6569162607362));
#52868=CARTESIAN_POINT('Origin',(30.,-1.32966554433622E-14,31.6569162607362));
#52869=CARTESIAN_POINT('',(27.2613089199969,-0.249140860380976,31.6569162607362));
#52870=CARTESIAN_POINT('Origin',(27.3063181178117,-0.22458883512474,31.6570220656265));
#52871=CARTESIAN_POINT('',(27.2788183937405,-0.397077657083763,31.6569162607362));
#52872=CARTESIAN_POINT('Origin',(27.3283189050458,-0.410446767819208,31.6570432561867));
#52873=CARTESIAN_POINT('Origin',(30.,-1.32966554433622E-14,31.6569162607362));
#52874=CARTESIAN_POINT('Origin',(30.,-1.32966554433622E-14,31.6569162607362));
#52875=CARTESIAN_POINT('',(27.2892987572189,-0.463248067869938,31.6569162607362));
#52876=CARTESIAN_POINT('Origin',(27.3322428769935,-0.4352403473568,31.6570220656245));
#52877=CARTESIAN_POINT('',(27.3183612423927,-0.609355047323306,31.6569162607362));
#52878=CARTESIAN_POINT('Origin',(27.3687580884808,-0.618799180197033,31.6570432561867));
#52879=CARTESIAN_POINT('Origin',(30.,-1.32966554433622E-14,31.6569162607362));
#52880=CARTESIAN_POINT('Origin',(30.,-1.32966554433622E-14,31.6569162607362));
#52881=CARTESIAN_POINT('',(27.3340009690024,-0.674499196974871,31.6569162607362));
#52882=CARTESIAN_POINT('Origin',(27.3746152459701,-0.643208458106799,31.6570220656281));
#52883=CARTESIAN_POINT('',(27.3744372857209,-0.817875561064986,31.6569162607362));
#52884=CARTESIAN_POINT('Origin',(27.4254197532793,-0.823336489857566,31.6570432561877));
#52885=CARTESIAN_POINT('Origin',(30.,-1.32966554433622E-14,31.6569162607362));
#52886=CARTESIAN_POINT('Origin',(30.,-1.32966554433622E-14,31.6569162607362));
#52887=CARTESIAN_POINT('',(27.3951399513465,-0.88159181423671,31.6569162607362));
#52888=CARTESIAN_POINT('Origin',(27.4331739849698,-0.847210974835381,31.6570220656246));
#52889=CARTESIAN_POINT('',(27.4467007962708,-1.02135360000148,31.6569162607362));
#52890=CARTESIAN_POINT('Origin',(27.4979545614299,-1.02279765627042,31.6570432561873));
#52891=CARTESIAN_POINT('Origin',(30.,-1.32966554433622E-14,31.6569162607362));
#52892=CARTESIAN_POINT('Origin',(30.,-1.32966554433622E-14,31.6569162607362));
#52893=CARTESIAN_POINT('',(27.4723387620945,-1.08324912480475,31.6569162607362));
#52894=CARTESIAN_POINT('Origin',(27.5075580599161,-1.04599015417175,31.657022065625));
#52895=CARTESIAN_POINT('',(27.5347062454699,-1.21853465435942,31.6569162607362));
#52896=CARTESIAN_POINT('Origin',(27.5859153117243,-1.21595293501783,31.6570432561869));
#52897=CARTESIAN_POINT('Origin',(30.,-1.32966554433622E-14,31.6569162607362));
#52898=CARTESIAN_POINT('Origin',(30.,-1.32966554433622E-14,31.6569162607362));
#52899=CARTESIAN_POINT('',(27.5651214449068,-1.27822784430149,31.6569162607362));
#52900=CARTESIAN_POINT('Origin',(27.5973088682438,-1.23832045638074,31.6570220656251));
#52901=CARTESIAN_POINT('',(27.637911050459,-1.40820303736935,31.6569162607362));
#52902=CARTESIAN_POINT('Origin',(27.6887596968882,-1.40161145957539,31.6570432561872));
#52903=CARTESIAN_POINT('Origin',(30.,-1.32966554433622E-14,31.6569162607362));
#52904=CARTESIAN_POINT('Origin',(30.,-1.32966554433622E-14,31.6569162607362));
#52905=CARTESIAN_POINT('',(27.6729159636906,-1.46532586408421,31.6569162607362));
#52906=CARTESIAN_POINT('Origin',(27.7018730663766,-1.42301610118967,31.6570220656267));
#52907=CARTESIAN_POINT('',(27.7556789192963,-1.58918938037887,31.6569162607362));
#52908=CARTESIAN_POINT('Origin',(27.8058536470839,-1.57862858340189,31.6570432561867));
#52909=CARTESIAN_POINT('Origin',(30.,-1.32966554433622E-14,31.6569162607362));
#52910=CARTESIAN_POINT('Origin',(30.,-1.32966554433622E-14,31.6569162607362));
#52911=CARTESIAN_POINT('',(27.7950577293922,-1.64338966264456,31.6569162607362));
#52912=CARTESIAN_POINT('Origin',(27.8206059812726,-1.59893837851,31.6570220656387));
#52913=CARTESIAN_POINT('',(27.8872837739086,-1.76037784239926,31.6569162607362));
#52914=CARTESIAN_POINT('Origin',(27.9364752391763,-1.7459129370637,31.6570432561874));
#52915=CARTESIAN_POINT('Origin',(30.,-1.32966554433622E-14,31.6569162607362));
#52916=CARTESIAN_POINT('Origin',(30.,-1.32966554433622E-14,31.6569162607362));
#52917=CARTESIAN_POINT('',(27.9307936974098,-1.81132141745219,31.6569162607362));
#52918=CARTESIAN_POINT('Origin',(27.9527755849842,-1.76500266908356,31.6570220656253));
#52919=CARTESIAN_POINT('',(28.0319142266042,-1.92071298963622,31.6569162607362));
#52920=CARTESIAN_POINT('Origin',(28.0798191476078,-1.90243315689441,31.657043256187));
#52921=CARTESIAN_POINT('Origin',(30.,-1.32966554433622E-14,31.6569162607362));
#52922=CARTESIAN_POINT('Origin',(30.,-1.32966554433622E-14,31.6569162607362));
#52923=CARTESIAN_POINT('',(28.0792870103637,-1.96808577339573,31.6569162607362));
#52924=CARTESIAN_POINT('Origin',(28.097567008002,-1.92018513125043,31.6570220656245));
#52925=CARTESIAN_POINT('',(28.1886785825478,-2.06920630259019,31.6569162607362));
#52926=CARTESIAN_POINT('Origin',(28.2350016095212,-2.0472242436889,31.6570432561873));
#52927=CARTESIAN_POINT('Origin',(30.,-1.32966554433622E-14,31.6569162607362));
#52928=CARTESIAN_POINT('Origin',(30.,-1.32966554433622E-14,31.6569162607362));
#52929=CARTESIAN_POINT('',(28.2396221576007,-2.11271622609136,31.6569162607362));
#52930=CARTESIAN_POINT('Origin',(28.2540875630401,-2.06352901355267,31.6570220656256));
#52931=CARTESIAN_POINT('',(28.3566103373554,-2.20494227060778,31.6569162607362));
#52932=CARTESIAN_POINT('Origin',(28.4010658734316,-2.17939351225073,31.6570432561869));
#52933=CARTESIAN_POINT('Origin',(30.,-1.32966554433622E-14,31.6569162607362));
#52934=CARTESIAN_POINT('Origin',(30.,-1.32966554433622E-14,31.6569162607362));
#52935=CARTESIAN_POINT('',(28.4108106196211,-2.2443210807037,31.6569162607362));
#52936=CARTESIAN_POINT('Origin',(28.4213722488256,-2.19415055329735,31.6570220656249));
#52937=CARTESIAN_POINT('',(28.5346741359157,-2.32708403630936,31.6569162607362));
#52938=CARTESIAN_POINT('Origin',(28.5769880979323,-2.29812609508764,31.6570432561867));
#52939=CARTESIAN_POINT('Origin',(30.,-1.32966554433622E-14,31.6569162607362));
#52940=CARTESIAN_POINT('Origin',(30.,-1.32966554433622E-14,31.6569162607362));
#52941=CARTESIAN_POINT('',(28.5917969626306,-2.362088949541,31.6569162607362));
#52942=CARTESIAN_POINT('Origin',(28.5983896996446,-2.31124442525031,31.6570220656249));
#52943=CARTESIAN_POINT('',(28.7217721556985,-2.43487855509312,31.6569162607362));
#52944=CARTESIAN_POINT('Origin',(28.7616836640096,-2.40268996634326,31.6570432561868));
#52945=CARTESIAN_POINT('Origin',(30.,-1.32966554433622E-14,31.6569162607362));
#52946=CARTESIAN_POINT('Origin',(30.,-1.32966554433622E-14,31.6569162607362));
#52947=CARTESIAN_POINT('',(28.7814653456405,-2.46529375453011,31.6569162607362));
#52948=CARTESIAN_POINT('Origin',(28.784048544048,-2.41408870675338,31.6570220656255));
#52949=CARTESIAN_POINT('',(28.9167508751952,-2.52766123790546,31.6569162607362));
#52950=CARTESIAN_POINT('Origin',(28.9540138620808,-2.49244045498024,31.6570432561872));
#52951=CARTESIAN_POINT('Origin',(30.,-1.32966554433622E-14,31.6569162607362));
#52952=CARTESIAN_POINT('Origin',(30.,-1.32966554433622E-14,31.6569162607362));
#52953=CARTESIAN_POINT('',(28.9786463999985,-2.55329920372917,31.6569162607362));
#52954=CARTESIAN_POINT('Origin',(28.9772041335221,-2.50204932861609,31.657022065625));
#52955=CARTESIAN_POINT('',(29.1184081857632,-2.60486004865345,31.6569162607362));
#52956=CARTESIAN_POINT('Origin',(29.1527929125168,-2.56682421939275,31.6570432561872));
#52957=CARTESIAN_POINT('Origin',(30.,-1.32966554433622E-14,31.6569162607362));
#52958=CARTESIAN_POINT('Origin',(30.,-1.32966554433622E-14,31.6569162607362));
#52959=CARTESIAN_POINT('',(29.182124438935,-2.6255627142791,31.6569162607362));
#52960=CARTESIAN_POINT('Origin',(29.1766655996274,-2.57458398435135,31.6570220656246));
#52961=CARTESIAN_POINT('',(29.3255008030251,-2.66599903099763,31.6569162607362));
#52962=CARTESIAN_POINT('Origin',(29.3567952763715,-2.62538265893786,31.6570432561866));
#52963=CARTESIAN_POINT('Origin',(30.,-1.32966554433622E-14,31.6569162607362));
#52964=CARTESIAN_POINT('Origin',(30.,-1.32966554433622E-14,31.6569162607362));
#52965=CARTESIAN_POINT('',(29.3906449526766,-2.6816387576073,31.6569162607362));
#52966=CARTESIAN_POINT('Origin',(29.3812031960972,-2.63124547368565,31.6570220656251));
#52967=CARTESIAN_POINT('',(29.53675193213,-2.71070124278106,31.6569162607362));
#52968=CARTESIAN_POINT('Origin',(29.5647632112362,-2.66775474136028,31.6570432561871));
#52969=CARTESIAN_POINT('Origin',(30.,-1.32966554433622E-14,31.6569162607362));
#52970=CARTESIAN_POINT('Origin',(30.,-1.32966554433622E-14,31.6569162607362));
#52971=CARTESIAN_POINT('',(29.6029223429162,-2.72118160625948,31.6569162607362));
#52972=CARTESIAN_POINT('Origin',(29.5895558806344,-2.67168445969898,31.6570220656245));
#52973=CARTESIAN_POINT('',(29.750859139619,-2.73869108000313,31.6569162607362));
#52974=CARTESIAN_POINT('Origin',(29.7754145256345,-2.69367922868347,31.6570432561876));
#52975=CARTESIAN_POINT('Origin',(30.,-1.32966554433622E-14,31.6569162607362));
#52976=CARTESIAN_POINT('Origin',(30.,-1.32966554433622E-14,31.6569162607362));
#52977=CARTESIAN_POINT('',(29.8176478489534,-2.74394746542436,31.6569162607362));
#52978=CARTESIAN_POINT('Origin',(29.800439089653,-2.69565162258972,31.6570220656252));
#52979=CARTESIAN_POINT('',(29.9665023833599,-2.74979597600977,31.6569162607362));
#52980=CARTESIAN_POINT('Origin',(29.9874504841626,-2.70299628782621,31.6570432561866));
#52981=CARTESIAN_POINT('Origin',(30.,-1.32966554433622E-14,31.6569162607362));
#52982=CARTESIAN_POINT('Origin',(30.,-1.32966554433622E-14,31.6569162607362));
#52983=CARTESIAN_POINT('',(30.03349761664,-2.74979597600977,31.6569162607362));
#52984=CARTESIAN_POINT('Origin',(30.0125526580435,-2.70299919683014,31.6570220656269));
#52985=CARTESIAN_POINT('',(30.1823521510466,-2.74394746542436,31.6569162607362));
#52986=CARTESIAN_POINT('Origin',(30.1995638146306,-2.69564847601399,31.6570432561868));
#52987=CARTESIAN_POINT('Origin',(30.,-1.32966554433622E-14,31.6569162607362));
#52988=CARTESIAN_POINT('Origin',(30.,-1.32966554433622E-14,31.6569162607362));
#52989=CARTESIAN_POINT('',(30.2491408603809,-2.73869108000313,31.6569162607362));
#52990=CARTESIAN_POINT('Origin',(30.2245888351274,-2.69368188219317,31.6570220656245));
#52991=CARTESIAN_POINT('',(30.3970776570837,-2.72118160625948,31.6569162607362));
#52992=CARTESIAN_POINT('Origin',(30.4104467678196,-2.67168109495285,31.6570432561872));
#52993=CARTESIAN_POINT('Origin',(30.,-1.32966554433622E-14,31.6569162607362));
#52994=CARTESIAN_POINT('Origin',(30.,-1.32966554433622E-14,31.6569162607362));
#52995=CARTESIAN_POINT('',(30.4632480678699,-2.71070124278107,31.6569162607362));
#52996=CARTESIAN_POINT('Origin',(30.4352403473562,-2.66775712300563,31.6570220656249));
#52997=CARTESIAN_POINT('',(30.6093550473233,-2.68163875760731,31.6569162607362));
#52998=CARTESIAN_POINT('Origin',(30.6187991801974,-2.63124191151731,31.6570432561874));
#52999=CARTESIAN_POINT('Origin',(30.,-1.32966554433622E-14,31.6569162607362));
#53000=CARTESIAN_POINT('Origin',(30.,-1.32966554433622E-14,31.6569162607362));
#53001=CARTESIAN_POINT('',(30.6744991969748,-2.66599903099764,31.6569162607362));
#53002=CARTESIAN_POINT('Origin',(30.6432084581108,-2.62538475403506,31.6570220656255));
#53003=CARTESIAN_POINT('',(30.817875561065,-2.62556271427912,31.6569162607362));
#53004=CARTESIAN_POINT('Origin',(30.8233364898573,-2.57458024672293,31.6570432561868));
#53005=CARTESIAN_POINT('Origin',(30.,-1.32966554433622E-14,31.6569162607362));
#53006=CARTESIAN_POINT('Origin',(30.,-1.32966554433622E-14,31.6569162607362));
#53007=CARTESIAN_POINT('',(30.8815918142367,-2.60486004865346,31.6569162607362));
#53008=CARTESIAN_POINT('Origin',(30.8472109748348,-2.56682601502956,31.6570220656249));
#53009=CARTESIAN_POINT('',(31.0213536000014,-2.55329920372919,31.6569162607362));
#53010=CARTESIAN_POINT('Origin',(31.0227976562703,-2.50204543857134,31.6570432561867));
#53011=CARTESIAN_POINT('Origin',(30.,-1.32966554433622E-14,31.6569162607362));
#53012=CARTESIAN_POINT('Origin',(30.,-1.32966554433622E-14,31.6569162607362));
#53013=CARTESIAN_POINT('',(31.0832491248047,-2.52766123790547,31.6569162607362));
#53014=CARTESIAN_POINT('Origin',(31.0459901541642,-2.49244194007693,31.6570220656289));
#53015=CARTESIAN_POINT('',(31.2185346543594,-2.46529375453013,31.6569162607362));
#53016=CARTESIAN_POINT('Origin',(31.2159529350178,-2.41408468827489,31.6570432561872));
#53017=CARTESIAN_POINT('Origin',(30.,-1.32966554433622E-14,31.6569162607362));
#53018=CARTESIAN_POINT('Origin',(30.,-1.32966554433622E-14,31.6569162607362));
#53019=CARTESIAN_POINT('',(31.2782278443015,-2.43487855509314,31.6569162607362));
#53020=CARTESIAN_POINT('Origin',(31.238320456382,-2.40269113175716,31.6570220656245));
#53021=CARTESIAN_POINT('',(31.4082030373693,-2.36208894954102,31.6569162607362));
#53022=CARTESIAN_POINT('Origin',(31.4016114595753,-2.31124030311134,31.6570432561875));
#53023=CARTESIAN_POINT('Origin',(30.,-1.32966554433622E-14,31.6569162607362));
#53024=CARTESIAN_POINT('Origin',(30.,-1.32966554433622E-14,31.6569162607362));
#53025=CARTESIAN_POINT('',(31.4653258640842,-2.32708403630938,31.6569162607362));
#53026=CARTESIAN_POINT('Origin',(31.4230161011935,-2.29812693362589,31.657022065625));
#53027=CARTESIAN_POINT('',(31.5891893803788,-2.24432108070372,31.6569162607362));
#53028=CARTESIAN_POINT('Origin',(31.5786285834021,-2.1941463529175,31.6570432561862));
#53029=CARTESIAN_POINT('Origin',(30.,-1.32966554433622E-14,31.6569162607362));
#53030=CARTESIAN_POINT('Origin',(30.,-1.32966554433622E-14,31.6569162607362));
#53031=CARTESIAN_POINT('',(31.6433896626445,-2.2049422706078,31.6569162607362));
#53032=CARTESIAN_POINT('Origin',(31.5989383785409,-2.17939401874466,31.6570220656252));
#53033=CARTESIAN_POINT('',(31.7603778423992,-2.11271622609138,31.6569162607362));
#53034=CARTESIAN_POINT('Origin',(31.7459129370641,-2.0635247608251,31.6570432561869));
#53035=CARTESIAN_POINT('Origin',(30.,-1.32966554433622E-14,31.6569162607362));
#53036=CARTESIAN_POINT('Origin',(30.,-1.32966554433622E-14,31.6569162607362));
#53037=CARTESIAN_POINT('',(31.8113214174522,-2.06920630259022,31.6569162607362));
#53038=CARTESIAN_POINT('Origin',(31.7650026690826,-2.04722441501533,31.6570220656257));
#53039=CARTESIAN_POINT('',(31.9207129896362,-1.96808577339576,31.6569162607362));
#53040=CARTESIAN_POINT('Origin',(31.9024331568943,-1.92018085239205,31.657043256187));
#53041=CARTESIAN_POINT('Origin',(30.,-1.32966554433622E-14,31.6569162607362));
#53042=CARTESIAN_POINT('Origin',(30.,-1.32966554433622E-14,31.6569162607362));
#53043=CARTESIAN_POINT('',(31.9680857733957,-1.92071298963625,31.6569162607362));
#53044=CARTESIAN_POINT('Origin',(31.9201851312437,-1.90243299199549,31.6570220656273));
#53045=CARTESIAN_POINT('',(32.0692063025902,-1.81132141745222,31.6569162607362));
#53046=CARTESIAN_POINT('Origin',(32.0472242436891,-1.76499839047944,31.6570432561871));
#53047=CARTESIAN_POINT('Origin',(30.,-1.32966554433622E-14,31.6569162607362));
#53048=CARTESIAN_POINT('Origin',(30.,-1.32966554433622E-14,31.6569162607362));
#53049=CARTESIAN_POINT('',(32.1127162260913,-1.76037784239929,31.6569162607362));
#53050=CARTESIAN_POINT('Origin',(32.0635290135546,-1.74591243696045,31.6570220656248));
#53051=CARTESIAN_POINT('',(32.2049422706077,-1.64338966264459,31.6569162607362));
#53052=CARTESIAN_POINT('Origin',(32.1793935122505,-1.59893412656801,31.6570432561871));
#53053=CARTESIAN_POINT('Origin',(30.,-1.32966554433622E-14,31.6569162607362));
#53054=CARTESIAN_POINT('Origin',(30.,-1.32966554433622E-14,31.6569162607362));
#53055=CARTESIAN_POINT('',(32.2443210807037,-1.5891893803789,31.6569162607362));
#53056=CARTESIAN_POINT('Origin',(32.1941505532956,-1.57862775117404,31.6570220656256));
#53057=CARTESIAN_POINT('',(32.3270840363093,-1.46532586408424,31.6569162607362));
#53058=CARTESIAN_POINT('Origin',(32.2981260950875,-1.42301190206755,31.6570432561867));
#53059=CARTESIAN_POINT('Origin',(30.,-1.32966554433622E-14,31.6569162607362));
#53060=CARTESIAN_POINT('Origin',(30.,-1.32966554433622E-14,31.6569162607362));
#53061=CARTESIAN_POINT('',(32.362088949541,-1.40820303736938,31.6569162607362));
#53062=CARTESIAN_POINT('Origin',(32.3112444252322,-1.40161030035328,31.657022065632));
#53063=CARTESIAN_POINT('',(32.4348785550931,-1.27822784430152,31.6569162607362));
#53064=CARTESIAN_POINT('Origin',(32.4026899663432,-1.23831633599041,31.6570432561868));
#53065=CARTESIAN_POINT('Origin',(30.,-1.32966554433622E-14,31.6569162607362));
#53066=CARTESIAN_POINT('Origin',(30.,-1.32966554433622E-14,31.6569162607362));
#53067=CARTESIAN_POINT('',(32.4652937545301,-1.21853465435946,31.6569162607362));
#53068=CARTESIAN_POINT('Origin',(32.414088706754,-1.21595145595202,31.6570220656252));
#53069=CARTESIAN_POINT('',(32.5276612379054,-1.08324912480479,31.6569162607362));
#53070=CARTESIAN_POINT('Origin',(32.4924404549811,-1.04598613792014,31.6570432561868));
#53071=CARTESIAN_POINT('Origin',(30.,-1.32966554433622E-14,31.6569162607362));
#53072=CARTESIAN_POINT('Origin',(30.,-1.32966554433622E-14,31.6569162607362));
#53073=CARTESIAN_POINT('',(32.5532992037291,-1.02135360000151,31.6569162607362));
#53074=CARTESIAN_POINT('Origin',(32.5020493286151,-1.0227958664779,31.6570220656254));
#53075=CARTESIAN_POINT('',(32.6048600486534,-0.881591814236746,31.6569162607362));
#53076=CARTESIAN_POINT('Origin',(32.5668242193914,-0.847207087482045,31.6570432561878));
#53077=CARTESIAN_POINT('Origin',(30.,-1.32966554433622E-14,31.6569162607362));
#53078=CARTESIAN_POINT('Origin',(30.,-1.32966554433622E-14,31.6569162607362));
#53079=CARTESIAN_POINT('',(32.6255627142791,-0.817875561065022,31.6569162607362));
#53080=CARTESIAN_POINT('Origin',(32.5745839843496,-0.82333440037284,31.6570220656255));
#53081=CARTESIAN_POINT('',(32.6659990309976,-0.674499196974908,31.6569162607362));
#53082=CARTESIAN_POINT('Origin',(32.6253826589374,-0.643204723628158,31.6570432561868));
#53083=CARTESIAN_POINT('Origin',(30.,-1.32966554433622E-14,31.6569162607362));
#53084=CARTESIAN_POINT('Origin',(30.,-1.32966554433622E-14,31.6569162607362));
#53085=CARTESIAN_POINT('',(32.6816387576073,-0.609355047323343,31.6569162607362));
#53086=CARTESIAN_POINT('Origin',(32.6312454736857,-0.618796803902764,31.657022065625));
#53087=CARTESIAN_POINT('',(32.710701242781,-0.463248067869977,31.6569162607362));
#53088=CARTESIAN_POINT('Origin',(32.6677547413593,-0.435236788763208,31.6570432561875));
#53089=CARTESIAN_POINT('Origin',(30.,-1.32966554433622E-14,31.6569162607362));
#53090=CARTESIAN_POINT('Origin',(30.,-1.32966554433622E-14,31.6569162607362));
#53091=CARTESIAN_POINT('',(32.7211816062594,-0.397077657083801,31.6569162607362));
#53092=CARTESIAN_POINT('Origin',(32.6716844596186,-0.410444119388296,31.6570220656567));
#53093=CARTESIAN_POINT('',(32.7386910800031,-0.249140860381013,31.6569162607362));
#53094=CARTESIAN_POINT('Origin',(32.6936792286845,-0.224585474366052,31.6570432561872));
#53095=CARTESIAN_POINT('Origin',(30.,-1.32966554433622E-14,31.6569162607362));
#53096=CARTESIAN_POINT('Origin',(30.,-1.32966554433622E-14,31.6569162607362));
#53097=CARTESIAN_POINT('',(32.7439474654243,-0.182352151046618,31.6569162607362));
#53098=CARTESIAN_POINT('Origin',(32.695651622591,-0.19956091034649,31.6570220656247));
#53099=CARTESIAN_POINT('',(32.7497959760097,-0.0334976166400576,31.6569162607362));
#53100=CARTESIAN_POINT('Origin',(32.702996287825,-0.0125495158368562,31.657043256187));
#53101=CARTESIAN_POINT('Origin',(30.,-1.32966554433622E-14,31.6569162607362));
#53102=CARTESIAN_POINT('Origin',(30.,-1.32966554433622E-14,31.6569162607362));
#53103=CARTESIAN_POINT('',(32.7497959760097,0.0334976166400122,31.6569162607362));
#53104=CARTESIAN_POINT('Origin',(32.7029991968315,0.0125526580441019,31.6570220656263));
#53105=CARTESIAN_POINT('',(32.7439474654243,0.182352151046572,31.6569162607362));
#53106=CARTESIAN_POINT('Origin',(32.695648476013,0.199563814630937,31.6570432561873));
#53107=CARTESIAN_POINT('Origin',(30.,-1.32966554433622E-14,31.6569162607362));
#53108=CARTESIAN_POINT('Origin',(30.,-1.32966554433622E-14,31.6569162607362));
#53109=CARTESIAN_POINT('',(32.7386910800031,0.249140860380968,31.6569162607362));
#53110=CARTESIAN_POINT('Origin',(32.6936818821912,0.224588835126342,31.6570220656253));
#53111=CARTESIAN_POINT('',(32.7211816062594,0.397077657083756,31.6569162607362));
#53112=CARTESIAN_POINT('Origin',(32.6716810949533,0.410446767819417,31.657043256187));
#53113=CARTESIAN_POINT('Origin',(30.,-1.32966554433622E-14,31.6569162607362));
#53114=CARTESIAN_POINT('Origin',(30.,-1.32966554433622E-14,31.6569162607362));
#53115=CARTESIAN_POINT('',(32.710701242781,0.463248067869931,31.6569162607362));
#53116=CARTESIAN_POINT('Origin',(32.6677571230054,0.435240347356078,31.6570220656249));
#53117=CARTESIAN_POINT('',(32.6816387576073,0.609355047323298,31.6569162607362));
#53118=CARTESIAN_POINT('Origin',(32.6312419115184,0.618799180197174,31.657043256187));
#53119=CARTESIAN_POINT('Origin',(30.,-1.32966554433622E-14,31.6569162607362));
#53120=CARTESIAN_POINT('Origin',(30.,-1.32966554433622E-14,31.6569162607362));
#53121=CARTESIAN_POINT('',(32.6659990309976,0.674499196974863,31.6569162607362));
#53122=CARTESIAN_POINT('Origin',(32.6253847539863,0.643208458072405,31.6570220656495));
#53123=CARTESIAN_POINT('',(32.6255627142791,0.817875561064977,31.6569162607362));
#53124=CARTESIAN_POINT('Origin',(32.574580246722,0.823336489857403,31.6570432561872));
#53125=CARTESIAN_POINT('Origin',(30.,-1.32966554433622E-14,31.6569162607362));
#53126=CARTESIAN_POINT('Origin',(30.,-1.32966554433622E-14,31.6569162607362));
#53127=CARTESIAN_POINT('',(32.6048600486534,0.881591814236701,31.6569162607362));
#53128=CARTESIAN_POINT('Origin',(32.5668260150295,0.847210974834854,31.6570220656249));
#53129=CARTESIAN_POINT('',(32.5532992037291,1.02135360000147,31.6569162607362));
#53130=CARTESIAN_POINT('Origin',(32.5020454385711,1.02279765627039,31.6570432561869));
#53131=CARTESIAN_POINT('Origin',(30.,-1.32966554433622E-14,31.6569162607362));
#53132=CARTESIAN_POINT('Origin',(30.,-1.32966554433622E-14,31.6569162607362));
#53133=CARTESIAN_POINT('',(32.5276612379054,1.08324912480474,31.6569162607362));
#53134=CARTESIAN_POINT('Origin',(32.4924419400839,1.04599015417185,31.6570220656248));
#53135=CARTESIAN_POINT('',(32.4652937545301,1.21853465435941,31.6569162607362));
#53136=CARTESIAN_POINT('Origin',(32.4140846882753,1.2159529350178,31.657043256187));
#53137=CARTESIAN_POINT('Origin',(30.,-1.32966554433622E-14,31.6569162607362));
#53138=CARTESIAN_POINT('Origin',(30.,-1.32966554433622E-14,31.6569162607362));
#53139=CARTESIAN_POINT('',(32.4348785550931,1.27822784430148,31.6569162607362));
#53140=CARTESIAN_POINT('Origin',(32.4026911317566,1.23832045638126,31.6570220656248));
#53141=CARTESIAN_POINT('',(32.362088949541,1.40820303736934,31.6569162607362));
#53142=CARTESIAN_POINT('Origin',(32.3112403031114,1.40161145957535,31.6570432561874));
#53143=CARTESIAN_POINT('Origin',(30.,-1.32966554433622E-14,31.6569162607362));
#53144=CARTESIAN_POINT('Origin',(30.,-1.32966554433622E-14,31.6569162607362));
#53145=CARTESIAN_POINT('',(32.3270840363093,1.4653258640842,31.6569162607362));
#53146=CARTESIAN_POINT('Origin',(32.2981269336259,1.42301610119356,31.657022065625));
#53147=CARTESIAN_POINT('',(32.2443210807037,1.58918938037886,31.6569162607362));
#53148=CARTESIAN_POINT('Origin',(32.1941463529162,1.57862858340189,31.6570432561866));
#53149=CARTESIAN_POINT('Origin',(30.,-1.32966554433622E-14,31.6569162607362));
#53150=CARTESIAN_POINT('Origin',(30.,-1.32966554433622E-14,31.6569162607362));
#53151=CARTESIAN_POINT('',(32.2049422706078,1.64338966264455,31.6569162607362));
#53152=CARTESIAN_POINT('Origin',(32.1793940187453,1.59893837854221,31.6570220656245));
#53153=CARTESIAN_POINT('',(32.1127162260913,1.76037784239925,31.6569162607362));
#53154=CARTESIAN_POINT('Origin',(32.0635247608241,1.74591293706383,31.6570432561872));
#53155=CARTESIAN_POINT('Origin',(30.,-1.32966554433622E-14,31.6569162607362));
#53156=CARTESIAN_POINT('Origin',(30.,-1.32966554433622E-14,31.6569162607362));
#53157=CARTESIAN_POINT('',(32.0692063025902,1.81132141745218,31.6569162607362));
#53158=CARTESIAN_POINT('Origin',(32.0472244150162,1.76500266908448,31.6570220656248));
#53159=CARTESIAN_POINT('',(31.9680857733957,1.92071298963621,31.6569162607362));
#53160=CARTESIAN_POINT('Origin',(31.9201808523931,1.90243315689474,31.6570432561866));
#53161=CARTESIAN_POINT('Origin',(30.,-1.32966554433622E-14,31.6569162607362));
#53162=CARTESIAN_POINT('Origin',(30.,-1.32966554433622E-14,31.6569162607362));
#53163=CARTESIAN_POINT('',(31.9207129896362,1.96808577339572,31.6569162607362));
#53164=CARTESIAN_POINT('Origin',(31.9024329919958,1.92018513124459,31.657022065627));
#53165=CARTESIAN_POINT('',(31.8113214174522,2.06920630259018,31.6569162607362));
#53166=CARTESIAN_POINT('Origin',(31.7649983904793,2.04722424368911,31.6570432561871));
#53167=CARTESIAN_POINT('Origin',(30.,-1.32966554433622E-14,31.6569162607362));
#53168=CARTESIAN_POINT('Origin',(30.,-1.32966554433622E-14,31.6569162607362));
#53169=CARTESIAN_POINT('',(31.7603778423992,2.11271622609134,31.6569162607362));
#53170=CARTESIAN_POINT('Origin',(31.7459124369604,2.06352901355459,31.6570220656248));
#53171=CARTESIAN_POINT('',(31.6433896626445,2.20494227060776,31.6569162607362));
#53172=CARTESIAN_POINT('Origin',(31.5989341265682,2.17939351225069,31.657043256187));
#53173=CARTESIAN_POINT('Origin',(30.,-1.32966554433622E-14,31.6569162607362));
#53174=CARTESIAN_POINT('Origin',(30.,-1.32966554433622E-14,31.6569162607362));
#53175=CARTESIAN_POINT('',(31.5891893803789,2.24432108070368,31.6569162607362));
#53176=CARTESIAN_POINT('Origin',(31.5786277511742,2.19415055329685,31.6570220656251));
#53177=CARTESIAN_POINT('',(31.4653258640842,2.32708403630934,31.6569162607362));
#53178=CARTESIAN_POINT('Origin',(31.4230119020666,2.29812609508688,31.6570432561872));
#53179=CARTESIAN_POINT('Origin',(30.,-1.32966554433622E-14,31.6569162607362));
#53180=CARTESIAN_POINT('Origin',(30.,-1.32966554433622E-14,31.6569162607362));
#53181=CARTESIAN_POINT('',(31.4082030373693,2.36208894954099,31.6569162607362));
#53182=CARTESIAN_POINT('Origin',(31.4016103003533,2.31124442523252,31.6570220656319));
#53183=CARTESIAN_POINT('',(31.2782278443015,2.4348785550931,31.6569162607362));
#53184=CARTESIAN_POINT('Origin',(31.2383163359906,2.4026899663434,31.6570432561867));
#53185=CARTESIAN_POINT('Origin',(30.,-1.32966554433622E-14,31.6569162607362));
#53186=CARTESIAN_POINT('Origin',(30.,-1.32966554433622E-14,31.6569162607362));
#53187=CARTESIAN_POINT('',(31.2185346543594,2.46529375453009,31.6569162607362));
#53188=CARTESIAN_POINT('Origin',(31.215951455952,2.4140887067551,31.6570220656248));
#53189=CARTESIAN_POINT('',(31.0832491248047,2.52766123790544,31.6569162607362));
#53190=CARTESIAN_POINT('Origin',(31.045986137919,2.49244045498011,31.6570432561873));
#53191=CARTESIAN_POINT('Origin',(30.,-1.32966554433622E-14,31.6569162607362));
#53192=CARTESIAN_POINT('Origin',(30.,-1.32966554433622E-14,31.6569162607362));
#53193=CARTESIAN_POINT('',(31.0213536000015,2.55329920372915,31.6569162607362));
#53194=CARTESIAN_POINT('Origin',(31.0227958664779,2.50204932861496,31.6570220656254));
#53195=CARTESIAN_POINT('',(30.8815918142367,2.60486004865343,31.6569162607362));
#53196=CARTESIAN_POINT('Origin',(30.8472070874836,2.56682421939316,31.6570432561869));
#53197=CARTESIAN_POINT('Origin',(30.,-1.32966554433622E-14,31.6569162607362));
#53198=CARTESIAN_POINT('Origin',(30.,-1.32966554433622E-14,31.6569162607362));
#53199=CARTESIAN_POINT('',(30.817875561065,2.62556271427908,31.6569162607362));
#53200=CARTESIAN_POINT('Origin',(30.8233344003728,2.5745839843498,31.6570220656254));
#53201=CARTESIAN_POINT('',(30.6744991969749,2.6659990309976,31.6569162607362));
#53202=CARTESIAN_POINT('Origin',(30.6432047236281,2.62538265893739,31.6570432561868));
#53203=CARTESIAN_POINT('Origin',(30.,-1.32966554433622E-14,31.6569162607362));
#53204=CARTESIAN_POINT('Origin',(30.,-1.32966554433622E-14,31.6569162607362));
#53205=CARTESIAN_POINT('',(30.6093550473233,2.68163875760728,31.6569162607362));
#53206=CARTESIAN_POINT('Origin',(30.6187968039028,2.63124547368537,31.6570220656252));
#53207=CARTESIAN_POINT('',(30.4632480678699,2.71070124278104,31.6569162607362));
#53208=CARTESIAN_POINT('Origin',(30.4352367887645,2.66775474136143,31.6570432561865));
#53209=CARTESIAN_POINT('Origin',(30.,-1.32966554433622E-14,31.6569162607362));
#53210=CARTESIAN_POINT('Origin',(30.,-1.32966554433622E-14,31.6569162607362));
#53211=CARTESIAN_POINT('',(27.5651214449069,1.27822784430151,31.6569162607362));
#53212=CARTESIAN_POINT('Origin',(27.5973100336575,1.23831633598946,31.6570432561873));
#53213=CARTESIAN_POINT('',(27.637911050459,1.40820303736937,31.6569162607362));
#53214=CARTESIAN_POINT('Origin',(30.,-1.32966554433622E-14,31.6569162607362));
#53215=CARTESIAN_POINT('Origin',(27.6887555747495,1.40161030035545,31.6570220656248));
#53216=CARTESIAN_POINT('Origin',(30.,-1.32966554433622E-14,31.6569162607362));
#53217=CARTESIAN_POINT('',(27.6729159636906,1.46532586408423,31.6569162607362));
#53218=CARTESIAN_POINT('Origin',(27.7018739049127,1.42301190206727,31.6570432561868));
#53219=CARTESIAN_POINT('',(27.7556789192963,1.58918938037889,31.6569162607362));
#53220=CARTESIAN_POINT('Origin',(30.,-1.32966554433622E-14,31.6569162607362));
#53221=CARTESIAN_POINT('Origin',(27.805849446702,1.5786277511745,31.6570220656247));
#53222=CARTESIAN_POINT('Origin',(30.,-1.32966554433622E-14,31.6569162607362));
#53223=CARTESIAN_POINT('',(27.7950577293922,1.64338966264458,31.6569162607362));
#53224=CARTESIAN_POINT('Origin',(27.8206064877494,1.59893412656804,31.6570432561871));
#53225=CARTESIAN_POINT('',(27.8872837739086,1.76037784239928,31.6569162607362));
#53226=CARTESIAN_POINT('Origin',(30.,-1.32966554433622E-14,31.6569162607362));
#53227=CARTESIAN_POINT('Origin',(27.936470986445,1.74591243696058,31.6570220656246));
#53228=CARTESIAN_POINT('Origin',(30.,-1.32966554433622E-14,31.6569162607362));
#53229=CARTESIAN_POINT('',(27.9307936974098,1.81132141745221,31.6569162607362));
#53230=CARTESIAN_POINT('Origin',(27.9527757563104,1.76499839048029,31.6570432561867));
#53231=CARTESIAN_POINT('',(28.0319142266043,1.92071298963623,31.6569162607362));
#53232=CARTESIAN_POINT('Origin',(30.,-1.32966554433622E-14,31.6569162607362));
#53233=CARTESIAN_POINT('Origin',(28.0798148687497,1.90243299199796,31.6570220656246));
#53234=CARTESIAN_POINT('Origin',(30.,-1.32966554433622E-14,31.6569162607362));
#53235=CARTESIAN_POINT('',(28.0792870103638,1.96808577339574,31.6569162607362));
#53236=CARTESIAN_POINT('Origin',(28.0975668431059,1.92018085239124,31.6570432561874));
#53237=CARTESIAN_POINT('',(28.1886785825478,2.0692063025902,31.6569162607362));
#53238=CARTESIAN_POINT('Origin',(30.,-1.32966554433622E-14,31.6569162607362));
#53239=CARTESIAN_POINT('Origin',(28.2349973309159,2.04722441501599,31.657022065625));
#53240=CARTESIAN_POINT('Origin',(30.,-1.32966554433622E-14,31.6569162607362));
#53241=CARTESIAN_POINT('',(28.2396221576007,2.11271622609137,31.6569162607362));
#53242=CARTESIAN_POINT('Origin',(28.2540870629359,2.06352476082518,31.6570432561869));
#53243=CARTESIAN_POINT('',(28.3566103373554,2.20494227060779,31.6569162607362));
#53244=CARTESIAN_POINT('Origin',(30.,-1.32966554433622E-14,31.6569162607362));
#53245=CARTESIAN_POINT('Origin',(28.4010616214895,2.17939401872761,31.6570220656385));
#53246=CARTESIAN_POINT('Origin',(30.,-1.32966554433622E-14,31.6569162607362));
#53247=CARTESIAN_POINT('',(28.4108106196211,2.2443210807037,31.6569162607362));
#53248=CARTESIAN_POINT('Origin',(28.4213714165984,2.19414635291463,31.6570432561873));
#53249=CARTESIAN_POINT('',(28.5346741359158,2.32708403630936,31.6569162607362));
#53250=CARTESIAN_POINT('Origin',(30.,-1.32966554433622E-14,31.6569162607362));
#53251=CARTESIAN_POINT('Origin',(28.5769838988101,2.29812693362349,31.6570220656266));
#53252=CARTESIAN_POINT('Origin',(30.,-1.32966554433622E-14,31.6569162607362));
#53253=CARTESIAN_POINT('',(28.5917969626306,2.36208894954101,31.6569162607362));
#53254=CARTESIAN_POINT('Origin',(28.5983885404246,2.31124030311217,31.6570432561871));
#53255=CARTESIAN_POINT('',(28.7217721556985,2.43487855509312,31.6569162607362));
#53256=CARTESIAN_POINT('Origin',(30.,-1.32966554433622E-14,31.6569162607362));
#53257=CARTESIAN_POINT('Origin',(28.7616795436181,2.40269113175706,31.6570220656245));
#53258=CARTESIAN_POINT('Origin',(30.,-1.32966554433622E-14,31.6569162607362));
#53259=CARTESIAN_POINT('',(28.7814653456406,2.46529375453011,31.6569162607362));
#53260=CARTESIAN_POINT('Origin',(28.7840470649822,2.41408468827519,31.6570432561871));
#53261=CARTESIAN_POINT('',(28.9167508751953,2.52766123790545,31.6569162607362));
#53262=CARTESIAN_POINT('Origin',(30.,-1.32966554433622E-14,31.6569162607362));
#53263=CARTESIAN_POINT('Origin',(28.9540098458282,2.49244194008388,31.6570220656249));
#53264=CARTESIAN_POINT('Origin',(30.,-1.32966554433622E-14,31.6569162607362));
#53265=CARTESIAN_POINT('',(28.9786463999985,2.55329920372917,31.6569162607362));
#53266=CARTESIAN_POINT('Origin',(28.9772023437296,2.50204543857058,31.657043256187));
#53267=CARTESIAN_POINT('',(29.1184081857633,2.60486004865344,31.6569162607362));
#53268=CARTESIAN_POINT('Origin',(30.,-1.32966554433622E-14,31.6569162607362));
#53269=CARTESIAN_POINT('Origin',(29.1527890251647,2.56682601503002,31.6570220656247));
#53270=CARTESIAN_POINT('Origin',(30.,-1.32966554433622E-14,31.6569162607362));
#53271=CARTESIAN_POINT('',(29.182124438935,2.62556271427909,31.6569162607362));
#53272=CARTESIAN_POINT('Origin',(29.1766635101426,2.57458024672254,31.657043256187));
#53273=CARTESIAN_POINT('',(29.3255008030251,2.66599903099761,31.6569162607362));
#53274=CARTESIAN_POINT('Origin',(30.,-1.32966554433622E-14,31.6569162607362));
#53275=CARTESIAN_POINT('Origin',(29.356791541893,2.62538475403008,31.657022065628));
#53276=CARTESIAN_POINT('Origin',(30.,-1.32966554433622E-14,31.6569162607362));
#53277=CARTESIAN_POINT('',(29.3906449526767,2.68163875760729,31.6569162607362));
#53278=CARTESIAN_POINT('Origin',(29.3812008198028,2.6312419115181,31.6570432561872));
#53279=CARTESIAN_POINT('',(29.5367519321301,2.71070124278105,31.6569162607362));
#53280=CARTESIAN_POINT('Origin',(30.,-1.32966554433622E-14,31.6569162607362));
#53281=CARTESIAN_POINT('Origin',(29.5647596526443,2.66775712300484,31.6570220656252));
#53282=CARTESIAN_POINT('Origin',(30.,-1.32966554433622E-14,31.6569162607362));
#53283=CARTESIAN_POINT('',(29.6029223429162,2.72118160625946,31.6569162607362));
#53284=CARTESIAN_POINT('Origin',(29.5895532321803,2.67168109495224,31.6570432561874));
#53285=CARTESIAN_POINT('',(29.750859139619,2.7386910800031,31.6569162607362));
#53286=CARTESIAN_POINT('Origin',(30.,-1.32966554433622E-14,31.6569162607362));
#53287=CARTESIAN_POINT('Origin',(29.7754111648735,2.69368188219135,31.6570220656252));
#53288=CARTESIAN_POINT('Origin',(30.,-1.32966554433622E-14,31.6569162607362));
#53289=CARTESIAN_POINT('',(29.8176478489534,2.74394746542433,31.6569162607362));
#53290=CARTESIAN_POINT('Origin',(29.8004361853695,2.6956484760142,31.6570432561868));
#53291=CARTESIAN_POINT('',(29.9665023833599,2.74979597600974,31.6569162607362));
#53292=CARTESIAN_POINT('Origin',(30.,-1.32966554433622E-14,31.6569162607362));
#53293=CARTESIAN_POINT('Origin',(29.9874473419551,2.70299919683309,31.6570220656256));
#53294=CARTESIAN_POINT('Origin',(30.,-1.32966554433622E-14,31.6569162607362));
#53295=CARTESIAN_POINT('',(30.3970776570838,2.72118160625945,31.6569162607362));
#53296=CARTESIAN_POINT('Origin',(30.4104441193885,2.67168445961759,31.6570220656571));
#53297=CARTESIAN_POINT('',(30.249140860381,2.7386910800031,31.6569162607362));
#53298=CARTESIAN_POINT('Origin',(30.2245854743662,2.69367922868485,31.657043256187));
#53299=CARTESIAN_POINT('Origin',(30.,-1.32966554433622E-14,31.6569162607362));
#53300=CARTESIAN_POINT('Origin',(30.,-1.32966554433622E-14,16.));
#53301=CARTESIAN_POINT('',(27.4723387620945,1.08324912480478,33.8305837392638));
#53302=CARTESIAN_POINT('',(27.4723387620945,1.08324912480478,16.));
#53303=CARTESIAN_POINT('',(27.5347062454699,1.21853465435945,33.8305837392638));
#53304=CARTESIAN_POINT('Origin',(30.,-1.32966554433622E-14,33.8305837392638));
#53305=CARTESIAN_POINT('',(27.5347062454699,1.21853465435945,16.));
#53306=CARTESIAN_POINT('Origin',(30.,-1.32966554433622E-14,16.));
#53307=CARTESIAN_POINT('',(27.4467007962708,1.0213536000015,33.8305837392638));
#53308=CARTESIAN_POINT('',(27.4467007962708,1.0213536000015,16.));
#53309=CARTESIAN_POINT('',(27.3951399513465,0.881591814236741,33.8305837392638));
#53310=CARTESIAN_POINT('',(27.3951399513465,0.881591814236737,16.));
#53311=CARTESIAN_POINT('Origin',(30.,-1.32966554433622E-14,33.8305837392638));
#53312=CARTESIAN_POINT('Origin',(30.,-1.32966554433622E-14,16.));
#53313=CARTESIAN_POINT('',(27.3744372857209,0.817875561065013,33.8305837392638));
#53314=CARTESIAN_POINT('',(27.3744372857209,0.817875561065013,16.));
#53315=CARTESIAN_POINT('',(27.3340009690024,0.674499196974903,33.8305837392638));
#53316=CARTESIAN_POINT('',(27.3340009690024,0.674499196974899,16.));
#53317=CARTESIAN_POINT('Origin',(30.,-1.32966554433622E-14,33.8305837392638));
#53318=CARTESIAN_POINT('Origin',(30.,-1.32966554433622E-14,16.));
#53319=CARTESIAN_POINT('',(27.3183612423927,0.609355047323334,33.8305837392638));
#53320=CARTESIAN_POINT('',(27.3183612423927,0.609355047323335,16.));
#53321=CARTESIAN_POINT('',(27.2892987572189,0.463248067869974,33.8305837392638));
#53322=CARTESIAN_POINT('',(27.2892987572189,0.463248067869971,16.));
#53323=CARTESIAN_POINT('Origin',(30.,-1.32966554433622E-14,33.8305837392638));
#53324=CARTESIAN_POINT('Origin',(30.,-1.32966554433622E-14,16.));
#53325=CARTESIAN_POINT('',(27.2788183937405,0.397077657083793,33.8305837392638));
#53326=CARTESIAN_POINT('',(27.2788183937405,0.397077657083795,16.));
#53327=CARTESIAN_POINT('',(27.2613089199969,0.24914086038101,33.8305837392638));
#53328=CARTESIAN_POINT('',(27.2613089199969,0.249140860381007,16.));
#53329=CARTESIAN_POINT('Origin',(30.,-1.32966554433622E-14,33.8305837392638));
#53330=CARTESIAN_POINT('Origin',(30.,-1.32966554433622E-14,16.));
#53331=CARTESIAN_POINT('',(27.2560525345756,0.182352151046609,33.8305837392638));
#53332=CARTESIAN_POINT('',(27.2560525345756,0.182352151046611,16.));
#53333=CARTESIAN_POINT('',(27.2502040239902,0.0334976166400525,33.8305837392638));
#53334=CARTESIAN_POINT('',(27.2502040239902,0.0334976166400503,16.));
#53335=CARTESIAN_POINT('Origin',(30.,-1.32966554433622E-14,33.8305837392638));
#53336=CARTESIAN_POINT('Origin',(30.,-1.32966554433622E-14,16.));
#53337=CARTESIAN_POINT('',(27.2502040239902,-0.0334976166400219,33.8305837392638));
#53338=CARTESIAN_POINT('',(27.2502040239902,-0.0334976166400194,16.));
#53339=CARTESIAN_POINT('',(27.2560525345756,-0.182352151046578,33.8305837392638));
#53340=CARTESIAN_POINT('',(27.2560525345756,-0.18235215104658,16.));
#53341=CARTESIAN_POINT('Origin',(30.,-1.32966554433622E-14,33.8305837392638));
#53342=CARTESIAN_POINT('Origin',(30.,-1.32966554433622E-14,16.));
#53343=CARTESIAN_POINT('',(27.2613089199969,-0.249140860380979,33.8305837392638));
#53344=CARTESIAN_POINT('',(27.2613089199969,-0.249140860380976,16.));
#53345=CARTESIAN_POINT('',(27.2788183937405,-0.397077657083761,33.8305837392638));
#53346=CARTESIAN_POINT('',(27.2788183937405,-0.397077657083763,16.));
#53347=CARTESIAN_POINT('Origin',(30.,-1.32966554433622E-14,33.8305837392638));
#53348=CARTESIAN_POINT('Origin',(30.,-1.32966554433622E-14,16.));
#53349=CARTESIAN_POINT('',(27.2892987572189,-0.463248067869942,33.8305837392638));
#53350=CARTESIAN_POINT('',(27.2892987572189,-0.463248067869938,16.));
#53351=CARTESIAN_POINT('',(27.3183612423927,-0.609355047323305,33.8305837392638));
#53352=CARTESIAN_POINT('',(27.3183612423927,-0.609355047323306,16.));
#53353=CARTESIAN_POINT('Origin',(30.,-1.32966554433622E-14,33.8305837392638));
#53354=CARTESIAN_POINT('Origin',(30.,-1.32966554433622E-14,16.));
#53355=CARTESIAN_POINT('',(27.3340009690023,-0.674499196974875,33.8305837392638));
#53356=CARTESIAN_POINT('',(27.3340009690024,-0.674499196974871,16.));
#53357=CARTESIAN_POINT('',(27.3744372857209,-0.817875561064985,33.8305837392638));
#53358=CARTESIAN_POINT('',(27.3744372857209,-0.817875561064986,16.));
#53359=CARTESIAN_POINT('Origin',(30.,-1.32966554433622E-14,33.8305837392638));
#53360=CARTESIAN_POINT('Origin',(30.,-1.32966554433622E-14,16.));
#53361=CARTESIAN_POINT('',(27.3951399513465,-0.881591814236714,33.8305837392638));
#53362=CARTESIAN_POINT('',(27.3951399513465,-0.88159181423671,16.));
#53363=CARTESIAN_POINT('',(27.4467007962708,-1.02135360000148,33.8305837392638));
#53364=CARTESIAN_POINT('',(27.4467007962708,-1.02135360000148,16.));
#53365=CARTESIAN_POINT('Origin',(30.,-1.32966554433622E-14,33.8305837392638));
#53366=CARTESIAN_POINT('Origin',(30.,-1.32966554433622E-14,16.));
#53367=CARTESIAN_POINT('',(27.4723387620945,-1.08324912480476,33.8305837392638));
#53368=CARTESIAN_POINT('',(27.4723387620945,-1.08324912480475,16.));
#53369=CARTESIAN_POINT('',(27.5347062454699,-1.21853465435942,33.8305837392638));
#53370=CARTESIAN_POINT('',(27.5347062454699,-1.21853465435942,16.));
#53371=CARTESIAN_POINT('Origin',(30.,-1.32966554433622E-14,33.8305837392638));
#53372=CARTESIAN_POINT('Origin',(30.,-1.32966554433622E-14,16.));
#53373=CARTESIAN_POINT('',(27.5651214449068,-1.27822784430149,33.8305837392638));
#53374=CARTESIAN_POINT('',(27.5651214449068,-1.27822784430149,16.));
#53375=CARTESIAN_POINT('',(27.637911050459,-1.40820303736935,33.8305837392638));
#53376=CARTESIAN_POINT('',(27.637911050459,-1.40820303736935,16.));
#53377=CARTESIAN_POINT('Origin',(30.,-1.32966554433622E-14,33.8305837392638));
#53378=CARTESIAN_POINT('Origin',(30.,-1.32966554433622E-14,16.));
#53379=CARTESIAN_POINT('',(27.6729159636906,-1.46532586408422,33.8305837392638));
#53380=CARTESIAN_POINT('',(27.6729159636906,-1.46532586408421,16.));
#53381=CARTESIAN_POINT('',(27.7556789192963,-1.58918938037887,33.8305837392638));
#53382=CARTESIAN_POINT('',(27.7556789192963,-1.58918938037887,16.));
#53383=CARTESIAN_POINT('Origin',(30.,-1.32966554433622E-14,33.8305837392638));
#53384=CARTESIAN_POINT('Origin',(30.,-1.32966554433622E-14,16.));
#53385=CARTESIAN_POINT('',(27.7950577293922,-1.64338966264456,33.8305837392638));
#53386=CARTESIAN_POINT('',(27.7950577293922,-1.64338966264456,16.));
#53387=CARTESIAN_POINT('',(27.8872837739086,-1.76037784239926,33.8305837392638));
#53388=CARTESIAN_POINT('',(27.8872837739086,-1.76037784239926,16.));
#53389=CARTESIAN_POINT('Origin',(30.,-1.32966554433622E-14,33.8305837392638));
#53390=CARTESIAN_POINT('Origin',(30.,-1.32966554433622E-14,16.));
#53391=CARTESIAN_POINT('',(27.9307936974098,-1.81132141745219,33.8305837392638));
#53392=CARTESIAN_POINT('',(27.9307936974098,-1.81132141745219,16.));
#53393=CARTESIAN_POINT('',(28.0319142266042,-1.92071298963622,33.8305837392638));
#53394=CARTESIAN_POINT('',(28.0319142266042,-1.92071298963622,16.));
#53395=CARTESIAN_POINT('Origin',(30.,-1.32966554433622E-14,33.8305837392638));
#53396=CARTESIAN_POINT('Origin',(30.,-1.32966554433622E-14,16.));
#53397=CARTESIAN_POINT('',(28.0792870103637,-1.96808577339574,33.8305837392638));
#53398=CARTESIAN_POINT('',(28.0792870103637,-1.96808577339573,16.));
#53399=CARTESIAN_POINT('',(28.1886785825478,-2.06920630259019,33.8305837392638));
#53400=CARTESIAN_POINT('',(28.1886785825478,-2.06920630259019,16.));
#53401=CARTESIAN_POINT('Origin',(30.,-1.32966554433622E-14,33.8305837392638));
#53402=CARTESIAN_POINT('Origin',(30.,-1.32966554433622E-14,16.));
#53403=CARTESIAN_POINT('',(28.2396221576007,-2.11271622609136,33.8305837392638));
#53404=CARTESIAN_POINT('',(28.2396221576007,-2.11271622609136,16.));
#53405=CARTESIAN_POINT('',(28.3566103373554,-2.20494227060778,33.8305837392638));
#53406=CARTESIAN_POINT('',(28.3566103373554,-2.20494227060778,16.));
#53407=CARTESIAN_POINT('Origin',(30.,-1.32966554433622E-14,33.8305837392638));
#53408=CARTESIAN_POINT('Origin',(30.,-1.32966554433622E-14,16.));
#53409=CARTESIAN_POINT('',(28.4108106196211,-2.2443210807037,33.8305837392638));
#53410=CARTESIAN_POINT('',(28.4108106196211,-2.2443210807037,16.));
#53411=CARTESIAN_POINT('',(28.5346741359157,-2.32708403630936,33.8305837392638));
#53412=CARTESIAN_POINT('',(28.5346741359157,-2.32708403630936,16.));
#53413=CARTESIAN_POINT('Origin',(30.,-1.32966554433622E-14,33.8305837392638));
#53414=CARTESIAN_POINT('Origin',(30.,-1.32966554433622E-14,16.));
#53415=CARTESIAN_POINT('',(28.5917969626306,-2.36208894954101,33.8305837392638));
#53416=CARTESIAN_POINT('',(28.5917969626306,-2.362088949541,16.));
#53417=CARTESIAN_POINT('',(28.7217721556985,-2.43487855509313,33.8305837392638));
#53418=CARTESIAN_POINT('',(28.7217721556985,-2.43487855509312,16.));
#53419=CARTESIAN_POINT('Origin',(30.,-1.32966554433622E-14,33.8305837392638));
#53420=CARTESIAN_POINT('Origin',(30.,-1.32966554433622E-14,16.));
#53421=CARTESIAN_POINT('',(28.7814653456405,-2.46529375453011,33.8305837392638));
#53422=CARTESIAN_POINT('',(28.7814653456405,-2.46529375453011,16.));
#53423=CARTESIAN_POINT('',(28.9167508751952,-2.52766123790546,33.8305837392638));
#53424=CARTESIAN_POINT('',(28.9167508751952,-2.52766123790546,16.));
#53425=CARTESIAN_POINT('Origin',(30.,-1.32966554433622E-14,33.8305837392638));
#53426=CARTESIAN_POINT('Origin',(30.,-1.32966554433622E-14,16.));
#53427=CARTESIAN_POINT('',(28.9786463999985,-2.55329920372918,33.8305837392638));
#53428=CARTESIAN_POINT('',(28.9786463999985,-2.55329920372917,16.));
#53429=CARTESIAN_POINT('',(29.1184081857632,-2.60486004865345,33.8305837392638));
#53430=CARTESIAN_POINT('',(29.1184081857632,-2.60486004865345,16.));
#53431=CARTESIAN_POINT('Origin',(30.,-1.32966554433622E-14,33.8305837392638));
#53432=CARTESIAN_POINT('Origin',(30.,-1.32966554433622E-14,16.));
#53433=CARTESIAN_POINT('',(29.182124438935,-2.62556271427911,33.8305837392638));
#53434=CARTESIAN_POINT('',(29.182124438935,-2.6255627142791,16.));
#53435=CARTESIAN_POINT('',(29.3255008030251,-2.66599903099763,33.8305837392638));
#53436=CARTESIAN_POINT('',(29.3255008030251,-2.66599903099763,16.));
#53437=CARTESIAN_POINT('Origin',(30.,-1.32966554433622E-14,33.8305837392638));
#53438=CARTESIAN_POINT('Origin',(30.,-1.32966554433622E-14,16.));
#53439=CARTESIAN_POINT('',(29.3906449526766,-2.68163875760731,33.8305837392638));
#53440=CARTESIAN_POINT('',(29.3906449526766,-2.6816387576073,16.));
#53441=CARTESIAN_POINT('',(29.53675193213,-2.71070124278107,33.8305837392638));
#53442=CARTESIAN_POINT('',(29.53675193213,-2.71070124278106,16.));
#53443=CARTESIAN_POINT('Origin',(30.,-1.32966554433622E-14,33.8305837392638));
#53444=CARTESIAN_POINT('Origin',(30.,-1.32966554433622E-14,16.));
#53445=CARTESIAN_POINT('',(29.6029223429162,-2.72118160625948,33.8305837392638));
#53446=CARTESIAN_POINT('',(29.6029223429162,-2.72118160625948,16.));
#53447=CARTESIAN_POINT('',(29.750859139619,-2.73869108000313,33.8305837392638));
#53448=CARTESIAN_POINT('',(29.750859139619,-2.73869108000313,16.));
#53449=CARTESIAN_POINT('Origin',(30.,-1.32966554433622E-14,33.8305837392638));
#53450=CARTESIAN_POINT('Origin',(30.,-1.32966554433622E-14,16.));
#53451=CARTESIAN_POINT('',(29.8176478489534,-2.74394746542436,33.8305837392638));
#53452=CARTESIAN_POINT('',(29.8176478489534,-2.74394746542436,16.));
#53453=CARTESIAN_POINT('',(29.9665023833599,-2.74979597600977,33.8305837392638));
#53454=CARTESIAN_POINT('',(29.9665023833599,-2.74979597600977,16.));
#53455=CARTESIAN_POINT('Origin',(30.,-1.32966554433622E-14,33.8305837392638));
#53456=CARTESIAN_POINT('Origin',(30.,-1.32966554433622E-14,16.));
#53457=CARTESIAN_POINT('',(30.03349761664,-2.74979597600977,33.8305837392638));
#53458=CARTESIAN_POINT('',(30.03349761664,-2.74979597600977,16.));
#53459=CARTESIAN_POINT('',(30.1823521510466,-2.74394746542436,33.8305837392638));
#53460=CARTESIAN_POINT('',(30.1823521510466,-2.74394746542436,16.));
#53461=CARTESIAN_POINT('Origin',(30.,-1.32966554433622E-14,33.8305837392638));
#53462=CARTESIAN_POINT('Origin',(30.,-1.32966554433622E-14,16.));
#53463=CARTESIAN_POINT('',(30.249140860381,-2.73869108000313,33.8305837392638));
#53464=CARTESIAN_POINT('',(30.2491408603809,-2.73869108000313,16.));
#53465=CARTESIAN_POINT('',(30.3970776570837,-2.72118160625949,33.8305837392638));
#53466=CARTESIAN_POINT('',(30.3970776570837,-2.72118160625948,16.));
#53467=CARTESIAN_POINT('Origin',(30.,-1.32966554433622E-14,33.8305837392638));
#53468=CARTESIAN_POINT('Origin',(30.,-1.32966554433622E-14,16.));
#53469=CARTESIAN_POINT('',(30.4632480678699,-2.71070124278108,33.8305837392638));
#53470=CARTESIAN_POINT('',(30.4632480678699,-2.71070124278107,16.));
#53471=CARTESIAN_POINT('',(30.6093550473233,-2.68163875760732,33.8305837392638));
#53472=CARTESIAN_POINT('',(30.6093550473233,-2.68163875760731,16.));
#53473=CARTESIAN_POINT('Origin',(30.,-1.32966554433622E-14,33.8305837392638));
#53474=CARTESIAN_POINT('Origin',(30.,-1.32966554433622E-14,16.));
#53475=CARTESIAN_POINT('',(30.6744991969748,-2.66599903099764,33.8305837392638));
#53476=CARTESIAN_POINT('',(30.6744991969748,-2.66599903099764,16.));
#53477=CARTESIAN_POINT('',(30.817875561065,-2.62556271427912,33.8305837392638));
#53478=CARTESIAN_POINT('',(30.817875561065,-2.62556271427912,16.));
#53479=CARTESIAN_POINT('Origin',(30.,-1.32966554433622E-14,33.8305837392638));
#53480=CARTESIAN_POINT('Origin',(30.,-1.32966554433622E-14,16.));
#53481=CARTESIAN_POINT('',(30.8815918142367,-2.60486004865346,33.8305837392638));
#53482=CARTESIAN_POINT('',(30.8815918142367,-2.60486004865346,16.));
#53483=CARTESIAN_POINT('',(31.0213536000014,-2.55329920372919,33.8305837392638));
#53484=CARTESIAN_POINT('',(31.0213536000014,-2.55329920372919,16.));
#53485=CARTESIAN_POINT('Origin',(30.,-1.32966554433622E-14,33.8305837392638));
#53486=CARTESIAN_POINT('Origin',(30.,-1.32966554433622E-14,16.));
#53487=CARTESIAN_POINT('',(31.0832491248047,-2.52766123790547,33.8305837392638));
#53488=CARTESIAN_POINT('',(31.0832491248047,-2.52766123790547,16.));
#53489=CARTESIAN_POINT('',(31.2185346543594,-2.46529375453013,33.8305837392638));
#53490=CARTESIAN_POINT('',(31.2185346543594,-2.46529375453013,16.));
#53491=CARTESIAN_POINT('Origin',(30.,-1.32966554433622E-14,33.8305837392638));
#53492=CARTESIAN_POINT('Origin',(30.,-1.32966554433622E-14,16.));
#53493=CARTESIAN_POINT('',(31.2782278443015,-2.43487855509314,33.8305837392638));
#53494=CARTESIAN_POINT('',(31.2782278443015,-2.43487855509314,16.));
#53495=CARTESIAN_POINT('',(31.4082030373693,-2.36208894954103,33.8305837392638));
#53496=CARTESIAN_POINT('',(31.4082030373693,-2.36208894954102,16.));
#53497=CARTESIAN_POINT('Origin',(30.,-1.32966554433622E-14,33.8305837392638));
#53498=CARTESIAN_POINT('Origin',(30.,-1.32966554433622E-14,16.));
#53499=CARTESIAN_POINT('',(31.4653258640842,-2.32708403630938,33.8305837392638));
#53500=CARTESIAN_POINT('',(31.4653258640842,-2.32708403630938,16.));
#53501=CARTESIAN_POINT('',(31.5891893803788,-2.24432108070372,33.8305837392638));
#53502=CARTESIAN_POINT('',(31.5891893803788,-2.24432108070372,16.));
#53503=CARTESIAN_POINT('Origin',(30.,-1.32966554433622E-14,33.8305837392638));
#53504=CARTESIAN_POINT('Origin',(30.,-1.32966554433622E-14,16.));
#53505=CARTESIAN_POINT('',(31.6433896626445,-2.2049422706078,33.8305837392638));
#53506=CARTESIAN_POINT('',(31.6433896626445,-2.2049422706078,16.));
#53507=CARTESIAN_POINT('',(31.7603778423992,-2.11271622609139,33.8305837392638));
#53508=CARTESIAN_POINT('',(31.7603778423992,-2.11271622609138,16.));
#53509=CARTESIAN_POINT('Origin',(30.,-1.32966554433622E-14,33.8305837392638));
#53510=CARTESIAN_POINT('Origin',(30.,-1.32966554433622E-14,16.));
#53511=CARTESIAN_POINT('',(31.8113214174522,-2.06920630259022,33.8305837392638));
#53512=CARTESIAN_POINT('',(31.8113214174522,-2.06920630259022,16.));
#53513=CARTESIAN_POINT('',(31.9207129896362,-1.96808577339576,33.8305837392638));
#53514=CARTESIAN_POINT('',(31.9207129896362,-1.96808577339576,16.));
#53515=CARTESIAN_POINT('Origin',(30.,-1.32966554433622E-14,33.8305837392638));
#53516=CARTESIAN_POINT('Origin',(30.,-1.32966554433622E-14,16.));
#53517=CARTESIAN_POINT('',(31.9680857733957,-1.92071298963625,33.8305837392638));
#53518=CARTESIAN_POINT('',(31.9680857733957,-1.92071298963625,16.));
#53519=CARTESIAN_POINT('',(32.0692063025902,-1.81132141745222,33.8305837392638));
#53520=CARTESIAN_POINT('',(32.0692063025902,-1.81132141745222,16.));
#53521=CARTESIAN_POINT('Origin',(30.,-1.32966554433622E-14,33.8305837392638));
#53522=CARTESIAN_POINT('Origin',(30.,-1.32966554433622E-14,16.));
#53523=CARTESIAN_POINT('',(32.1127162260913,-1.76037784239929,33.8305837392638));
#53524=CARTESIAN_POINT('',(32.1127162260913,-1.76037784239929,16.));
#53525=CARTESIAN_POINT('',(32.2049422706078,-1.6433896626446,33.8305837392638));
#53526=CARTESIAN_POINT('',(32.2049422706077,-1.64338966264459,16.));
#53527=CARTESIAN_POINT('Origin',(30.,-1.32966554433622E-14,33.8305837392638));
#53528=CARTESIAN_POINT('Origin',(30.,-1.32966554433622E-14,16.));
#53529=CARTESIAN_POINT('',(32.2443210807037,-1.5891893803789,33.8305837392638));
#53530=CARTESIAN_POINT('',(32.2443210807037,-1.5891893803789,16.));
#53531=CARTESIAN_POINT('',(32.3270840363093,-1.46532586408425,33.8305837392638));
#53532=CARTESIAN_POINT('',(32.3270840363093,-1.46532586408424,16.));
#53533=CARTESIAN_POINT('Origin',(30.,-1.32966554433622E-14,33.8305837392638));
#53534=CARTESIAN_POINT('Origin',(30.,-1.32966554433622E-14,16.));
#53535=CARTESIAN_POINT('',(32.362088949541,-1.40820303736938,33.8305837392638));
#53536=CARTESIAN_POINT('',(32.362088949541,-1.40820303736938,16.));
#53537=CARTESIAN_POINT('',(32.4348785550931,-1.27822784430152,33.8305837392638));
#53538=CARTESIAN_POINT('',(32.4348785550931,-1.27822784430152,16.));
#53539=CARTESIAN_POINT('Origin',(30.,-1.32966554433622E-14,33.8305837392638));
#53540=CARTESIAN_POINT('Origin',(30.,-1.32966554433622E-14,16.));
#53541=CARTESIAN_POINT('',(32.4652937545301,-1.21853465435946,33.8305837392638));
#53542=CARTESIAN_POINT('',(32.4652937545301,-1.21853465435946,16.));
#53543=CARTESIAN_POINT('',(32.5276612379054,-1.08324912480479,33.8305837392638));
#53544=CARTESIAN_POINT('',(32.5276612379054,-1.08324912480479,16.));
#53545=CARTESIAN_POINT('Origin',(30.,-1.32966554433622E-14,33.8305837392638));
#53546=CARTESIAN_POINT('Origin',(30.,-1.32966554433622E-14,16.));
#53547=CARTESIAN_POINT('',(32.5532992037291,-1.02135360000151,33.8305837392638));
#53548=CARTESIAN_POINT('',(32.5532992037291,-1.02135360000151,16.));
#53549=CARTESIAN_POINT('',(32.6048600486534,-0.88159181423675,33.8305837392638));
#53550=CARTESIAN_POINT('',(32.6048600486534,-0.881591814236746,16.));
#53551=CARTESIAN_POINT('Origin',(30.,-1.32966554433622E-14,33.8305837392638));
#53552=CARTESIAN_POINT('Origin',(30.,-1.32966554433622E-14,16.));
#53553=CARTESIAN_POINT('',(32.6255627142791,-0.817875561065022,33.8305837392638));
#53554=CARTESIAN_POINT('',(32.6255627142791,-0.817875561065022,16.));
#53555=CARTESIAN_POINT('',(32.6659990309976,-0.674499196974912,33.8305837392638));
#53556=CARTESIAN_POINT('',(32.6659990309976,-0.674499196974908,16.));
#53557=CARTESIAN_POINT('Origin',(30.,-1.32966554433622E-14,33.8305837392638));
#53558=CARTESIAN_POINT('Origin',(30.,-1.32966554433622E-14,16.));
#53559=CARTESIAN_POINT('',(32.6816387576073,-0.609355047323342,33.8305837392638));
#53560=CARTESIAN_POINT('',(32.6816387576073,-0.609355047323343,16.));
#53561=CARTESIAN_POINT('',(32.710701242781,-0.463248067869981,33.8305837392638));
#53562=CARTESIAN_POINT('',(32.710701242781,-0.463248067869977,16.));
#53563=CARTESIAN_POINT('Origin',(30.,-1.32966554433622E-14,33.8305837392638));
#53564=CARTESIAN_POINT('Origin',(30.,-1.32966554433622E-14,16.));
#53565=CARTESIAN_POINT('',(32.7211816062594,-0.3970776570838,33.8305837392638));
#53566=CARTESIAN_POINT('',(32.7211816062594,-0.397077657083801,16.));
#53567=CARTESIAN_POINT('',(32.7386910800031,-0.249140860381016,33.8305837392638));
#53568=CARTESIAN_POINT('',(32.7386910800031,-0.249140860381013,16.));
#53569=CARTESIAN_POINT('Origin',(30.,-1.32966554433622E-14,33.8305837392638));
#53570=CARTESIAN_POINT('Origin',(30.,-1.32966554433622E-14,16.));
#53571=CARTESIAN_POINT('',(32.7439474654243,-0.182352151046616,33.8305837392638));
#53572=CARTESIAN_POINT('',(32.7439474654243,-0.182352151046618,16.));
#53573=CARTESIAN_POINT('',(32.7497959760097,-0.03349761664006,33.8305837392638));
#53574=CARTESIAN_POINT('',(32.7497959760097,-0.0334976166400576,16.));
#53575=CARTESIAN_POINT('Origin',(30.,-1.32966554433622E-14,33.8305837392638));
#53576=CARTESIAN_POINT('Origin',(30.,-1.32966554433622E-14,16.));
#53577=CARTESIAN_POINT('',(32.7497959760097,0.0334976166400146,33.8305837392638));
#53578=CARTESIAN_POINT('',(32.7497959760097,0.0334976166400122,16.));
#53579=CARTESIAN_POINT('',(32.7439474654243,0.18235215104657,33.8305837392638));
#53580=CARTESIAN_POINT('',(32.7439474654243,0.182352151046572,16.));
#53581=CARTESIAN_POINT('Origin',(30.,-1.32966554433622E-14,33.8305837392638));
#53582=CARTESIAN_POINT('Origin',(30.,-1.32966554433622E-14,16.));
#53583=CARTESIAN_POINT('',(32.7386910800031,0.249140860380971,33.8305837392638));
#53584=CARTESIAN_POINT('',(32.7386910800031,0.249140860380968,16.));
#53585=CARTESIAN_POINT('',(32.7211816062594,0.397077657083754,33.8305837392638));
#53586=CARTESIAN_POINT('',(32.7211816062594,0.397077657083756,16.));
#53587=CARTESIAN_POINT('Origin',(30.,-1.32966554433622E-14,33.8305837392638));
#53588=CARTESIAN_POINT('Origin',(30.,-1.32966554433622E-14,16.));
#53589=CARTESIAN_POINT('',(32.710701242781,0.463248067869934,33.8305837392638));
#53590=CARTESIAN_POINT('',(32.710701242781,0.463248067869931,16.));
#53591=CARTESIAN_POINT('',(32.6816387576073,0.609355047323297,33.8305837392638));
#53592=CARTESIAN_POINT('',(32.6816387576073,0.609355047323298,16.));
#53593=CARTESIAN_POINT('Origin',(30.,-1.32966554433622E-14,33.8305837392638));
#53594=CARTESIAN_POINT('Origin',(30.,-1.32966554433622E-14,16.));
#53595=CARTESIAN_POINT('',(32.6659990309976,0.674499196974867,33.8305837392638));
#53596=CARTESIAN_POINT('',(32.6659990309976,0.674499196974863,16.));
#53597=CARTESIAN_POINT('',(32.6255627142791,0.817875561064977,33.8305837392638));
#53598=CARTESIAN_POINT('',(32.6255627142791,0.817875561064977,16.));
#53599=CARTESIAN_POINT('Origin',(30.,-1.32966554433622E-14,33.8305837392638));
#53600=CARTESIAN_POINT('Origin',(30.,-1.32966554433622E-14,16.));
#53601=CARTESIAN_POINT('',(32.6048600486534,0.881591814236705,33.8305837392638));
#53602=CARTESIAN_POINT('',(32.6048600486534,0.881591814236701,16.));
#53603=CARTESIAN_POINT('',(32.5532992037292,1.02135360000147,33.8305837392638));
#53604=CARTESIAN_POINT('',(32.5532992037291,1.02135360000147,16.));
#53605=CARTESIAN_POINT('Origin',(30.,-1.32966554433622E-14,33.8305837392638));
#53606=CARTESIAN_POINT('Origin',(30.,-1.32966554433622E-14,16.));
#53607=CARTESIAN_POINT('',(32.5276612379054,1.08324912480475,33.8305837392638));
#53608=CARTESIAN_POINT('',(32.5276612379054,1.08324912480474,16.));
#53609=CARTESIAN_POINT('',(32.4652937545301,1.21853465435941,33.8305837392638));
#53610=CARTESIAN_POINT('',(32.4652937545301,1.21853465435941,16.));
#53611=CARTESIAN_POINT('Origin',(30.,-1.32966554433622E-14,33.8305837392638));
#53612=CARTESIAN_POINT('Origin',(30.,-1.32966554433622E-14,16.));
#53613=CARTESIAN_POINT('',(32.4348785550931,1.27822784430148,33.8305837392638));
#53614=CARTESIAN_POINT('',(32.4348785550931,1.27822784430148,16.));
#53615=CARTESIAN_POINT('',(32.362088949541,1.40820303736934,33.8305837392638));
#53616=CARTESIAN_POINT('',(32.362088949541,1.40820303736934,16.));
#53617=CARTESIAN_POINT('Origin',(30.,-1.32966554433622E-14,33.8305837392638));
#53618=CARTESIAN_POINT('Origin',(30.,-1.32966554433622E-14,16.));
#53619=CARTESIAN_POINT('',(32.3270840363093,1.4653258640842,33.8305837392638));
#53620=CARTESIAN_POINT('',(32.3270840363093,1.4653258640842,16.));
#53621=CARTESIAN_POINT('',(32.2443210807037,1.58918938037886,33.8305837392638));
#53622=CARTESIAN_POINT('',(32.2443210807037,1.58918938037886,16.));
#53623=CARTESIAN_POINT('Origin',(30.,-1.32966554433622E-14,33.8305837392638));
#53624=CARTESIAN_POINT('Origin',(30.,-1.32966554433622E-14,16.));
#53625=CARTESIAN_POINT('',(32.2049422706078,1.64338966264455,33.8305837392638));
#53626=CARTESIAN_POINT('',(32.2049422706078,1.64338966264455,16.));
#53627=CARTESIAN_POINT('',(32.1127162260914,1.76037784239925,33.8305837392638));
#53628=CARTESIAN_POINT('',(32.1127162260913,1.76037784239925,16.));
#53629=CARTESIAN_POINT('Origin',(30.,-1.32966554433622E-14,33.8305837392638));
#53630=CARTESIAN_POINT('Origin',(30.,-1.32966554433622E-14,16.));
#53631=CARTESIAN_POINT('',(32.0692063025902,1.81132141745218,33.8305837392638));
#53632=CARTESIAN_POINT('',(32.0692063025902,1.81132141745218,16.));
#53633=CARTESIAN_POINT('',(31.9680857733957,1.92071298963621,33.8305837392638));
#53634=CARTESIAN_POINT('',(31.9680857733957,1.92071298963621,16.));
#53635=CARTESIAN_POINT('Origin',(30.,-1.32966554433622E-14,33.8305837392638));
#53636=CARTESIAN_POINT('Origin',(30.,-1.32966554433622E-14,16.));
#53637=CARTESIAN_POINT('',(31.9207129896362,1.96808577339572,33.8305837392638));
#53638=CARTESIAN_POINT('',(31.9207129896362,1.96808577339572,16.));
#53639=CARTESIAN_POINT('',(31.8113214174522,2.06920630259018,33.8305837392638));
#53640=CARTESIAN_POINT('',(31.8113214174522,2.06920630259018,16.));
#53641=CARTESIAN_POINT('Origin',(30.,-1.32966554433622E-14,33.8305837392638));
#53642=CARTESIAN_POINT('Origin',(30.,-1.32966554433622E-14,16.));
#53643=CARTESIAN_POINT('',(31.7603778423992,2.11271622609135,33.8305837392638));
#53644=CARTESIAN_POINT('',(31.7603778423992,2.11271622609134,16.));
#53645=CARTESIAN_POINT('',(31.6433896626446,2.20494227060777,33.8305837392638));
#53646=CARTESIAN_POINT('',(31.6433896626445,2.20494227060776,16.));
#53647=CARTESIAN_POINT('Origin',(30.,-1.32966554433622E-14,33.8305837392638));
#53648=CARTESIAN_POINT('Origin',(30.,-1.32966554433622E-14,16.));
#53649=CARTESIAN_POINT('',(31.5891893803789,2.24432108070369,33.8305837392638));
#53650=CARTESIAN_POINT('',(31.5891893803789,2.24432108070368,16.));
#53651=CARTESIAN_POINT('',(31.4653258640842,2.32708403630934,33.8305837392638));
#53652=CARTESIAN_POINT('',(31.4653258640842,2.32708403630934,16.));
#53653=CARTESIAN_POINT('Origin',(30.,-1.32966554433622E-14,33.8305837392638));
#53654=CARTESIAN_POINT('Origin',(30.,-1.32966554433622E-14,16.));
#53655=CARTESIAN_POINT('',(31.4082030373693,2.36208894954099,33.8305837392638));
#53656=CARTESIAN_POINT('',(31.4082030373693,2.36208894954099,16.));
#53657=CARTESIAN_POINT('',(31.2782278443015,2.43487855509311,33.8305837392638));
#53658=CARTESIAN_POINT('',(31.2782278443015,2.4348785550931,16.));
#53659=CARTESIAN_POINT('Origin',(30.,-1.32966554433622E-14,33.8305837392638));
#53660=CARTESIAN_POINT('Origin',(30.,-1.32966554433622E-14,16.));
#53661=CARTESIAN_POINT('',(31.2185346543594,2.4652937545301,33.8305837392638));
#53662=CARTESIAN_POINT('',(31.2185346543594,2.46529375453009,16.));
#53663=CARTESIAN_POINT('',(31.0832491248047,2.52766123790544,33.8305837392638));
#53664=CARTESIAN_POINT('',(31.0832491248047,2.52766123790544,16.));
#53665=CARTESIAN_POINT('Origin',(30.,-1.32966554433622E-14,33.8305837392638));
#53666=CARTESIAN_POINT('Origin',(30.,-1.32966554433622E-14,16.));
#53667=CARTESIAN_POINT('',(31.0213536000015,2.55329920372916,33.8305837392638));
#53668=CARTESIAN_POINT('',(31.0213536000015,2.55329920372915,16.));
#53669=CARTESIAN_POINT('',(30.8815918142367,2.60486004865343,33.8305837392638));
#53670=CARTESIAN_POINT('',(30.8815918142367,2.60486004865343,16.));
#53671=CARTESIAN_POINT('Origin',(30.,-1.32966554433622E-14,33.8305837392638));
#53672=CARTESIAN_POINT('Origin',(30.,-1.32966554433622E-14,16.));
#53673=CARTESIAN_POINT('',(30.817875561065,2.62556271427909,33.8305837392638));
#53674=CARTESIAN_POINT('',(30.817875561065,2.62556271427908,16.));
#53675=CARTESIAN_POINT('',(30.6744991969749,2.66599903099761,33.8305837392638));
#53676=CARTESIAN_POINT('',(30.6744991969749,2.6659990309976,16.));
#53677=CARTESIAN_POINT('Origin',(30.,-1.32966554433622E-14,33.8305837392638));
#53678=CARTESIAN_POINT('Origin',(30.,-1.32966554433622E-14,16.));
#53679=CARTESIAN_POINT('',(30.6093550473233,2.68163875760729,33.8305837392638));
#53680=CARTESIAN_POINT('',(30.6093550473233,2.68163875760728,16.));
#53681=CARTESIAN_POINT('',(30.4632480678699,2.71070124278105,33.8305837392638));
#53682=CARTESIAN_POINT('',(30.4632480678699,2.71070124278104,16.));
#53683=CARTESIAN_POINT('Origin',(30.,-1.32966554433622E-14,33.8305837392638));
#53684=CARTESIAN_POINT('Origin',(30.,-1.32966554433622E-14,16.));
#53685=CARTESIAN_POINT('',(27.5651214449069,1.27822784430151,33.8305837392638));
#53686=CARTESIAN_POINT('',(27.5651214449069,1.27822784430151,16.));
#53687=CARTESIAN_POINT('',(27.637911050459,1.40820303736937,33.8305837392638));
#53688=CARTESIAN_POINT('Origin',(30.,-1.32966554433622E-14,33.8305837392638));
#53689=CARTESIAN_POINT('',(27.637911050459,1.40820303736937,16.));
#53690=CARTESIAN_POINT('Origin',(30.,-1.32966554433622E-14,16.));
#53691=CARTESIAN_POINT('',(27.6729159636906,1.46532586408424,33.8305837392638));
#53692=CARTESIAN_POINT('',(27.6729159636906,1.46532586408423,16.));
#53693=CARTESIAN_POINT('',(27.7556789192963,1.58918938037889,33.8305837392638));
#53694=CARTESIAN_POINT('Origin',(30.,-1.32966554433622E-14,33.8305837392638));
#53695=CARTESIAN_POINT('',(27.7556789192963,1.58918938037889,16.));
#53696=CARTESIAN_POINT('Origin',(30.,-1.32966554433622E-14,16.));
#53697=CARTESIAN_POINT('',(27.7950577293922,1.64338966264458,33.8305837392638));
#53698=CARTESIAN_POINT('',(27.7950577293922,1.64338966264458,16.));
#53699=CARTESIAN_POINT('',(27.8872837739086,1.76037784239928,33.8305837392638));
#53700=CARTESIAN_POINT('Origin',(30.,-1.32966554433622E-14,33.8305837392638));
#53701=CARTESIAN_POINT('',(27.8872837739086,1.76037784239928,16.));
#53702=CARTESIAN_POINT('Origin',(30.,-1.32966554433622E-14,16.));
#53703=CARTESIAN_POINT('',(27.9307936974098,1.81132141745221,33.8305837392638));
#53704=CARTESIAN_POINT('',(27.9307936974098,1.81132141745221,16.));
#53705=CARTESIAN_POINT('',(28.0319142266043,1.92071298963624,33.8305837392638));
#53706=CARTESIAN_POINT('Origin',(30.,-1.32966554433622E-14,33.8305837392638));
#53707=CARTESIAN_POINT('',(28.0319142266043,1.92071298963623,16.));
#53708=CARTESIAN_POINT('Origin',(30.,-1.32966554433622E-14,16.));
#53709=CARTESIAN_POINT('',(28.0792870103638,1.96808577339575,33.8305837392638));
#53710=CARTESIAN_POINT('',(28.0792870103638,1.96808577339574,16.));
#53711=CARTESIAN_POINT('',(28.1886785825478,2.06920630259021,33.8305837392638));
#53712=CARTESIAN_POINT('Origin',(30.,-1.32966554433622E-14,33.8305837392638));
#53713=CARTESIAN_POINT('',(28.1886785825478,2.0692063025902,16.));
#53714=CARTESIAN_POINT('Origin',(30.,-1.32966554433622E-14,16.));
#53715=CARTESIAN_POINT('',(28.2396221576007,2.11271622609138,33.8305837392638));
#53716=CARTESIAN_POINT('',(28.2396221576007,2.11271622609137,16.));
#53717=CARTESIAN_POINT('',(28.3566103373554,2.20494227060779,33.8305837392638));
#53718=CARTESIAN_POINT('Origin',(30.,-1.32966554433622E-14,33.8305837392638));
#53719=CARTESIAN_POINT('',(28.3566103373554,2.20494227060779,16.));
#53720=CARTESIAN_POINT('Origin',(30.,-1.32966554433622E-14,16.));
#53721=CARTESIAN_POINT('',(28.4108106196211,2.24432108070371,33.8305837392638));
#53722=CARTESIAN_POINT('',(28.4108106196211,2.2443210807037,16.));
#53723=CARTESIAN_POINT('',(28.5346741359158,2.32708403630936,33.8305837392638));
#53724=CARTESIAN_POINT('Origin',(30.,-1.32966554433622E-14,33.8305837392638));
#53725=CARTESIAN_POINT('',(28.5346741359158,2.32708403630936,16.));
#53726=CARTESIAN_POINT('Origin',(30.,-1.32966554433622E-14,16.));
#53727=CARTESIAN_POINT('',(28.5917969626306,2.36208894954101,33.8305837392638));
#53728=CARTESIAN_POINT('',(28.5917969626306,2.36208894954101,16.));
#53729=CARTESIAN_POINT('',(28.7217721556985,2.43487855509313,33.8305837392638));
#53730=CARTESIAN_POINT('Origin',(30.,-1.32966554433622E-14,33.8305837392638));
#53731=CARTESIAN_POINT('',(28.7217721556985,2.43487855509312,16.));
#53732=CARTESIAN_POINT('Origin',(30.,-1.32966554433622E-14,16.));
#53733=CARTESIAN_POINT('',(28.7814653456406,2.46529375453011,33.8305837392638));
#53734=CARTESIAN_POINT('',(28.7814653456406,2.46529375453011,16.));
#53735=CARTESIAN_POINT('',(28.9167508751952,2.52766123790546,33.8305837392638));
#53736=CARTESIAN_POINT('Origin',(30.,-1.32966554433622E-14,33.8305837392638));
#53737=CARTESIAN_POINT('',(28.9167508751953,2.52766123790545,16.));
#53738=CARTESIAN_POINT('Origin',(30.,-1.32966554433622E-14,16.));
#53739=CARTESIAN_POINT('',(28.9786463999985,2.55329920372917,33.8305837392638));
#53740=CARTESIAN_POINT('',(28.9786463999985,2.55329920372917,16.));
#53741=CARTESIAN_POINT('',(29.1184081857633,2.60486004865344,33.8305837392638));
#53742=CARTESIAN_POINT('Origin',(30.,-1.32966554433622E-14,33.8305837392638));
#53743=CARTESIAN_POINT('',(29.1184081857633,2.60486004865344,16.));
#53744=CARTESIAN_POINT('Origin',(30.,-1.32966554433622E-14,16.));
#53745=CARTESIAN_POINT('',(29.182124438935,2.6255627142791,33.8305837392638));
#53746=CARTESIAN_POINT('',(29.182124438935,2.62556271427909,16.));
#53747=CARTESIAN_POINT('',(29.3255008030251,2.66599903099762,33.8305837392638));
#53748=CARTESIAN_POINT('Origin',(30.,-1.32966554433622E-14,33.8305837392638));
#53749=CARTESIAN_POINT('',(29.3255008030251,2.66599903099761,16.));
#53750=CARTESIAN_POINT('Origin',(30.,-1.32966554433622E-14,16.));
#53751=CARTESIAN_POINT('',(29.3906449526767,2.6816387576073,33.8305837392638));
#53752=CARTESIAN_POINT('',(29.3906449526767,2.68163875760729,16.));
#53753=CARTESIAN_POINT('',(29.5367519321301,2.71070124278105,33.8305837392638));
#53754=CARTESIAN_POINT('Origin',(30.,-1.32966554433622E-14,33.8305837392638));
#53755=CARTESIAN_POINT('',(29.5367519321301,2.71070124278105,16.));
#53756=CARTESIAN_POINT('Origin',(30.,-1.32966554433622E-14,16.));
#53757=CARTESIAN_POINT('',(29.6029223429162,2.72118160625947,33.8305837392638));
#53758=CARTESIAN_POINT('',(29.6029223429162,2.72118160625946,16.));
#53759=CARTESIAN_POINT('',(29.750859139619,2.73869108000311,33.8305837392638));
#53760=CARTESIAN_POINT('Origin',(30.,-1.32966554433622E-14,33.8305837392638));
#53761=CARTESIAN_POINT('',(29.750859139619,2.7386910800031,16.));
#53762=CARTESIAN_POINT('Origin',(30.,-1.32966554433622E-14,16.));
#53763=CARTESIAN_POINT('',(29.8176478489534,2.74394746542434,33.8305837392638));
#53764=CARTESIAN_POINT('',(29.8176478489534,2.74394746542433,16.));
#53765=CARTESIAN_POINT('',(29.9665023833599,2.74979597600975,33.8305837392638));
#53766=CARTESIAN_POINT('Origin',(30.,-1.32966554433622E-14,33.8305837392638));
#53767=CARTESIAN_POINT('',(29.9665023833599,2.74979597600974,16.));
#53768=CARTESIAN_POINT('Origin',(30.,-1.32966554433622E-14,16.));
#53769=CARTESIAN_POINT('',(30.3970776570838,2.72118160625946,33.8305837392638));
#53770=CARTESIAN_POINT('',(30.3970776570838,2.72118160625945,16.));
#53771=CARTESIAN_POINT('',(30.249140860381,2.73869108000311,33.8305837392638));
#53772=CARTESIAN_POINT('',(30.249140860381,2.7386910800031,16.));
#53773=CARTESIAN_POINT('Origin',(30.,-1.32966554433622E-14,33.8305837392638));
#53774=CARTESIAN_POINT('Origin',(30.,-1.32966554433622E-14,33.8305837392638));
#53775=CARTESIAN_POINT('Origin',(27.5075580599235,1.0459901541636,33.8304779343707));
#53776=CARTESIAN_POINT('Origin',(27.5859153117241,1.21595293501799,33.830456743813));
#53777=CARTESIAN_POINT('Origin',(30.,-1.32966554433622E-14,33.8305837392638));
#53778=CARTESIAN_POINT('Origin',(27.4979545614264,1.02279765627048,33.8304567438139));
#53779=CARTESIAN_POINT('Origin',(27.4331739849704,0.847210974834779,33.830477934375));
#53780=CARTESIAN_POINT('Origin',(30.,-1.32966554433622E-14,33.8305837392638));
#53781=CARTESIAN_POINT('Origin',(27.4254197532764,0.823336489857381,33.8304567438132));
#53782=CARTESIAN_POINT('Origin',(27.3746152459633,0.643208458112014,33.8304779343751));
#53783=CARTESIAN_POINT('Origin',(30.,-1.32966554433622E-14,33.8305837392638));
#53784=CARTESIAN_POINT('Origin',(27.368758088479,0.618799180196873,33.8304567438137));
#53785=CARTESIAN_POINT('Origin',(27.3322428769935,0.435240347356666,33.8304779343754));
#53786=CARTESIAN_POINT('Origin',(30.,-1.32966554433622E-14,33.8305837392638));
#53787=CARTESIAN_POINT('Origin',(27.3283189050469,0.410446767819665,33.8304567438127));
#53788=CARTESIAN_POINT('Origin',(27.3063181178076,0.224588835126915,33.8304779343751));
#53789=CARTESIAN_POINT('Origin',(30.,-1.32966554433622E-14,33.8305837392638));
#53790=CARTESIAN_POINT('Origin',(27.3043515239852,0.199563814630461,33.8304567438133));
#53791=CARTESIAN_POINT('Origin',(27.2970008031678,0.0125526580442922,33.8304779343738));
#53792=CARTESIAN_POINT('Origin',(30.,-1.32966554433622E-14,33.8305837392638));
#53793=CARTESIAN_POINT('Origin',(27.2970037121732,-0.012549515837469,33.8304567438135));
#53794=CARTESIAN_POINT('Origin',(27.3043483774083,-0.199560910346332,33.8304779343754));
#53795=CARTESIAN_POINT('Origin',(30.,-1.32966554433622E-14,33.8305837392638));
#53796=CARTESIAN_POINT('Origin',(27.3063207713147,-0.224585474366301,33.8304567438129));
#53797=CARTESIAN_POINT('Origin',(27.3283155403039,-0.410444119366497,33.8304779343742));
#53798=CARTESIAN_POINT('Origin',(30.,-1.32966554433622E-14,33.8305837392638));
#53799=CARTESIAN_POINT('Origin',(27.3322452586388,-0.435236788764194,33.8304567438132));
#53800=CARTESIAN_POINT('Origin',(27.3687545263134,-0.618796803902706,33.8304779343752));
#53801=CARTESIAN_POINT('Origin',(30.,-1.32966554433622E-14,33.8305837392638));
#53802=CARTESIAN_POINT('Origin',(27.3746173410614,-0.643204723628853,33.8304567438136));
#53803=CARTESIAN_POINT('Origin',(27.4254160156486,-0.823334400372707,33.8304779343751));
#53804=CARTESIAN_POINT('Origin',(30.,-1.32966554433622E-14,33.8305837392638));
#53805=CARTESIAN_POINT('Origin',(27.433175780606,-0.847207087484101,33.8304567438133));
#53806=CARTESIAN_POINT('Origin',(27.4979506713824,-1.02279586647791,33.8304779343754));
#53807=CARTESIAN_POINT('Origin',(30.,-1.32966554433622E-14,33.8305837392638));
#53808=CARTESIAN_POINT('Origin',(27.5075595450189,-1.04598613791989,33.830456743813));
#53809=CARTESIAN_POINT('Origin',(27.5859112932449,-1.21595145595217,33.830477934375));
#53810=CARTESIAN_POINT('Origin',(30.,-1.32966554433622E-14,33.8305837392638));
#53811=CARTESIAN_POINT('Origin',(27.5973100336554,-1.23831633599182,33.8304567438138));
#53812=CARTESIAN_POINT('Origin',(27.6887555747498,-1.40161030035549,33.8304779343749));
#53813=CARTESIAN_POINT('Origin',(30.,-1.32966554433622E-14,33.8305837392638));
#53814=CARTESIAN_POINT('Origin',(27.7018739049122,-1.42301190206769,33.8304567438132));
#53815=CARTESIAN_POINT('Origin',(27.8058494467036,-1.57862775117429,33.8304779343746));
#53816=CARTESIAN_POINT('Origin',(30.,-1.32966554433622E-14,33.8305837392638));
#53817=CARTESIAN_POINT('Origin',(27.8206064877493,-1.59893412656796,33.8304567438128));
#53818=CARTESIAN_POINT('Origin',(27.9364709864456,-1.74591243696051,33.830477934375));
#53819=CARTESIAN_POINT('Origin',(30.,-1.32966554433622E-14,33.8305837392638));
#53820=CARTESIAN_POINT('Origin',(27.9527757563098,-1.76499839048126,33.8304567438135));
#53821=CARTESIAN_POINT('Origin',(28.0798148687495,-1.90243299199812,33.8304779343753));
#53822=CARTESIAN_POINT('Origin',(30.,-1.32966554433622E-14,33.8305837392638));
#53823=CARTESIAN_POINT('Origin',(28.0975668431045,-1.92018085239454,33.8304567438138));
#53824=CARTESIAN_POINT('Origin',(28.234997330915,-2.04722441501659,33.8304779343752));
#53825=CARTESIAN_POINT('Origin',(30.,-1.32966554433622E-14,33.8305837392638));
#53826=CARTESIAN_POINT('Origin',(28.2540870629355,-2.06352476082575,33.8304567438132));
#53827=CARTESIAN_POINT('Origin',(28.4010616214883,-2.1793940187284,33.8304779343619));
#53828=CARTESIAN_POINT('Origin',(30.,-1.32966554433622E-14,33.8305837392638));
#53829=CARTESIAN_POINT('Origin',(28.4213714165976,-2.19414635291788,33.8304567438138));
#53830=CARTESIAN_POINT('Origin',(28.5769838988107,-2.29812693362319,33.8304779343729));
#53831=CARTESIAN_POINT('Origin',(30.,-1.32966554433622E-14,33.8305837392638));
#53832=CARTESIAN_POINT('Origin',(28.5983885404242,-2.31124030311337,33.8304567438133));
#53833=CARTESIAN_POINT('Origin',(28.7616795436178,-2.40269113175742,33.8304779343754));
#53834=CARTESIAN_POINT('Origin',(30.,-1.32966554433622E-14,33.8305837392638));
#53835=CARTESIAN_POINT('Origin',(28.7840470649819,-2.41408468827727,33.8304567438135));
#53836=CARTESIAN_POINT('Origin',(28.9540098458287,-2.49244194008352,33.8304779343747));
#53837=CARTESIAN_POINT('Origin',(30.,-1.32966554433622E-14,33.8305837392638));
#53838=CARTESIAN_POINT('Origin',(28.9772023437295,-2.50204543857419,33.8304567438141));
#53839=CARTESIAN_POINT('Origin',(29.1527890251654,-2.5668260150294,33.8304779343748));
#53840=CARTESIAN_POINT('Origin',(30.,-1.32966554433622E-14,33.8305837392638));
#53841=CARTESIAN_POINT('Origin',(29.1766635101425,-2.57458024672298,33.8304567438129));
#53842=CARTESIAN_POINT('Origin',(29.3567915418921,-2.62538475403142,33.8304779343725));
#53843=CARTESIAN_POINT('Origin',(30.,-1.32966554433622E-14,33.8305837392638));
#53844=CARTESIAN_POINT('Origin',(29.3812008198029,-2.63124191151983,33.8304567438133));
#53845=CARTESIAN_POINT('Origin',(29.5647596526443,-2.66775712300496,33.8304779343746));
#53846=CARTESIAN_POINT('Origin',(30.,-1.32966554433622E-14,33.8305837392638));
#53847=CARTESIAN_POINT('Origin',(29.589553232181,-2.67168109495555,33.8304567438136));
#53848=CARTESIAN_POINT('Origin',(29.7754111648755,-2.69368188218804,33.8304779343731));
#53849=CARTESIAN_POINT('Origin',(30.,-1.32966554433622E-14,33.8305837392638));
#53850=CARTESIAN_POINT('Origin',(29.8004361853699,-2.69564847601571,33.8304567438137));
#53851=CARTESIAN_POINT('Origin',(29.9874473419542,-2.70299919683539,33.8304779343752));
#53852=CARTESIAN_POINT('Origin',(30.,-1.32966554433622E-14,33.8305837392638));
#53853=CARTESIAN_POINT('Origin',(30.0125495158367,-2.70299628782517,33.8304567438128));
#53854=CARTESIAN_POINT('Origin',(30.199560910346,-2.6956516225925,33.8304779343757));
#53855=CARTESIAN_POINT('Origin',(30.,-1.32966554433622E-14,33.8305837392638));
#53856=CARTESIAN_POINT('Origin',(30.2245854743665,-2.69367922868563,33.8304567438131));
#53857=CARTESIAN_POINT('Origin',(30.4104441193657,-2.67168445969903,33.8304779343754));
#53858=CARTESIAN_POINT('Origin',(30.,-1.32966554433622E-14,33.8305837392638));
#53859=CARTESIAN_POINT('Origin',(30.4352367887642,-2.66775474136125,33.8304567438132));
#53860=CARTESIAN_POINT('Origin',(30.6187968039027,-2.63124547368644,33.8304779343751));
#53861=CARTESIAN_POINT('Origin',(30.,-1.32966554433622E-14,33.8305837392638));
#53862=CARTESIAN_POINT('Origin',(30.6432047236274,-2.6253826589367,33.8304567438126));
#53863=CARTESIAN_POINT('Origin',(30.8233344003726,-2.57458398435223,33.8304779343755));
#53864=CARTESIAN_POINT('Origin',(30.,-1.32966554433622E-14,33.8305837392638));
#53865=CARTESIAN_POINT('Origin',(30.8472070874839,-2.5668242193938,33.8304567438132));
#53866=CARTESIAN_POINT('Origin',(31.0227958664778,-2.50204932861793,33.8304779343756));
#53867=CARTESIAN_POINT('Origin',(30.,-1.32966554433622E-14,33.8305837392638));
#53868=CARTESIAN_POINT('Origin',(31.0459861379201,-2.49244045498134,33.8304567438131));
#53869=CARTESIAN_POINT('Origin',(31.2159514559521,-2.41408870675381,33.8304779343746));
#53870=CARTESIAN_POINT('Origin',(30.,-1.32966554433622E-14,33.8305837392638));
#53871=CARTESIAN_POINT('Origin',(31.2383163359911,-2.402689966344,33.8304567438135));
#53872=CARTESIAN_POINT('Origin',(31.4016103003557,-2.3112444252517,33.8304779343755));
#53873=CARTESIAN_POINT('Origin',(30.,-1.32966554433622E-14,33.8305837392638));
#53874=CARTESIAN_POINT('Origin',(31.4230119020685,-2.29812609508837,33.8304567438136));
#53875=CARTESIAN_POINT('Origin',(31.5786277511746,-2.19415055329817,33.8304779343753));
#53876=CARTESIAN_POINT('Origin',(30.,-1.32966554433622E-14,33.8305837392638));
#53877=CARTESIAN_POINT('Origin',(31.5989341265715,-2.17939351225268,33.8304567438143));
#53878=CARTESIAN_POINT('Origin',(31.7459124369605,-2.06352901355452,33.8304779343751));
#53879=CARTESIAN_POINT('Origin',(30.,-1.32966554433622E-14,33.8305837392638));
#53880=CARTESIAN_POINT('Origin',(31.764998390482,-2.04722424369058,33.8304567438139));
#53881=CARTESIAN_POINT('Origin',(31.9024329919978,-1.92018513124985,33.8304779343751));
#53882=CARTESIAN_POINT('Origin',(30.,-1.32966554433622E-14,33.8305837392638));
#53883=CARTESIAN_POINT('Origin',(31.9201808523926,-1.90243315689474,33.8304567438131));
#53884=CARTESIAN_POINT('Origin',(32.0472244150163,-1.76500266908446,33.830477934375));
#53885=CARTESIAN_POINT('Origin',(30.,-1.32966554433622E-14,33.8305837392638));
#53886=CARTESIAN_POINT('Origin',(32.0635247608254,-1.74591293706441,33.8304567438131));
#53887=CARTESIAN_POINT('Origin',(32.1793940187282,-1.59893837851134,33.8304779343617));
#53888=CARTESIAN_POINT('Origin',(30.,-1.32966554433622E-14,33.8305837392638));
#53889=CARTESIAN_POINT('Origin',(32.1941463529172,-1.57862858340229,33.8304567438136));
#53890=CARTESIAN_POINT('Origin',(32.2981269336233,-1.42301610118952,33.830477934373));
#53891=CARTESIAN_POINT('Origin',(30.,-1.32966554433622E-14,33.8305837392638));
#53892=CARTESIAN_POINT('Origin',(32.311240303114,-1.40161145957583,33.8304567438134));
#53893=CARTESIAN_POINT('Origin',(32.4026911317571,-1.23832045638176,33.8304779343753));
#53894=CARTESIAN_POINT('Origin',(30.,-1.32966554433622E-14,33.8305837392638));
#53895=CARTESIAN_POINT('Origin',(32.4140846882749,-1.21595293501797,33.8304567438127));
#53896=CARTESIAN_POINT('Origin',(32.4924419400838,-1.04599015417152,33.8304779343749));
#53897=CARTESIAN_POINT('Origin',(30.,-1.32966554433622E-14,33.8305837392638));
#53898=CARTESIAN_POINT('Origin',(32.5020454385714,-1.02279765627054,33.8304567438132));
#53899=CARTESIAN_POINT('Origin',(32.56682601503,-0.847210974835106,33.8304779343751));
#53900=CARTESIAN_POINT('Origin',(30.,-1.32966554433622E-14,33.8305837392638));
#53901=CARTESIAN_POINT('Origin',(32.5745802467237,-0.823336489857386,33.8304567438133));
#53902=CARTESIAN_POINT('Origin',(32.6253847540299,-0.643208458106727,33.8304779343718));
#53903=CARTESIAN_POINT('Origin',(30.,-1.32966554433622E-14,33.8305837392638));
#53904=CARTESIAN_POINT('Origin',(32.6312419115182,-0.618799180197391,33.8304567438127));
#53905=CARTESIAN_POINT('Origin',(32.6677571230055,-0.435240347356057,33.830477934375));
#53906=CARTESIAN_POINT('Origin',(30.,-1.32966554433622E-14,33.8305837392638));
#53907=CARTESIAN_POINT('Origin',(32.6716810949544,-0.410446767819313,33.8304567438133));
#53908=CARTESIAN_POINT('Origin',(32.6936818821919,-0.224588835126652,33.8304779343749));
#53909=CARTESIAN_POINT('Origin',(30.,-1.32966554433622E-14,33.8305837392638));
#53910=CARTESIAN_POINT('Origin',(32.6956484760151,-0.199563814630355,33.8304567438134));
#53911=CARTESIAN_POINT('Origin',(32.7029991968333,-0.0125526580448477,33.8304779343743));
#53912=CARTESIAN_POINT('Origin',(30.,-1.32966554433622E-14,33.8305837392638));
#53913=CARTESIAN_POINT('Origin',(32.7029962878262,0.0125495158371826,33.8304567438133));
#53914=CARTESIAN_POINT('Origin',(32.6956516225903,0.19956091034681,33.8304779343749));
#53915=CARTESIAN_POINT('Origin',(30.,-1.32966554433622E-14,33.8305837392638));
#53916=CARTESIAN_POINT('Origin',(32.6936792286859,0.22458547436666,33.8304567438133));
#53917=CARTESIAN_POINT('Origin',(32.6716844596177,0.410444119388619,33.8304779343428));
#53918=CARTESIAN_POINT('Origin',(30.,-1.32966554433622E-14,33.8305837392638));
#53919=CARTESIAN_POINT('Origin',(32.6677547413622,0.435236788764869,33.8304567438136));
#53920=CARTESIAN_POINT('Origin',(32.6312454736863,0.618796803902747,33.8304779343751));
#53921=CARTESIAN_POINT('Origin',(30.,-1.32966554433622E-14,33.8305837392638));
#53922=CARTESIAN_POINT('Origin',(32.625382658939,0.643204723629168,33.8304567438138));
#53923=CARTESIAN_POINT('Origin',(32.5745839843506,0.823334400372804,33.8304779343749));
#53924=CARTESIAN_POINT('Origin',(30.,-1.32966554433622E-14,33.8305837392638));
#53925=CARTESIAN_POINT('Origin',(32.5668242193939,0.847207087484111,33.8304567438133));
#53926=CARTESIAN_POINT('Origin',(32.5020493286164,1.02279586647793,33.830477934375));
#53927=CARTESIAN_POINT('Origin',(30.,-1.32966554433622E-14,33.8305837392638));
#53928=CARTESIAN_POINT('Origin',(32.4924404549818,1.04598613792066,33.8304567438134));
#53929=CARTESIAN_POINT('Origin',(32.4140887067556,1.21595145595219,33.8304779343752));
#53930=CARTESIAN_POINT('Origin',(30.,-1.32966554433622E-14,33.8305837392638));
#53931=CARTESIAN_POINT('Origin',(32.4026899663445,1.2383163359917,33.8304567438137));
#53932=CARTESIAN_POINT('Origin',(32.3112444252326,1.40161030035344,33.830477934368));
#53933=CARTESIAN_POINT('Origin',(30.,-1.32966554433622E-14,33.8305837392638));
#53934=CARTESIAN_POINT('Origin',(32.2981260950878,1.42301190206775,33.8304567438133));
#53935=CARTESIAN_POINT('Origin',(32.1941505532983,1.57862775117468,33.8304779343753));
#53936=CARTESIAN_POINT('Origin',(30.,-1.32966554433622E-14,33.8305837392638));
#53937=CARTESIAN_POINT('Origin',(32.1793935122518,1.59893412656992,33.8304567438136));
#53938=CARTESIAN_POINT('Origin',(32.0635290135536,1.74591243696026,33.8304779343747));
#53939=CARTESIAN_POINT('Origin',(30.,-1.32966554433622E-14,33.8305837392638));
#53940=CARTESIAN_POINT('Origin',(32.04722424369,1.76499839048088,33.8304567438134));
#53941=CARTESIAN_POINT('Origin',(31.9201851312459,1.90243299199643,33.8304779343734));
#53942=CARTESIAN_POINT('Origin',(30.,-1.32966554433622E-14,33.8305837392638));
#53943=CARTESIAN_POINT('Origin',(31.9024331568948,1.92018085239292,33.8304567438132));
#53944=CARTESIAN_POINT('Origin',(31.7650026690842,2.0472244150162,33.8304779343749));
#53945=CARTESIAN_POINT('Origin',(30.,-1.32966554433622E-14,33.8305837392638));
#53946=CARTESIAN_POINT('Origin',(31.7459129370645,2.06352476082576,33.8304567438132));
#53947=CARTESIAN_POINT('Origin',(31.5989383785419,2.17939401874533,33.8304779343753));
#53948=CARTESIAN_POINT('Origin',(30.,-1.32966554433622E-14,33.8305837392638));
#53949=CARTESIAN_POINT('Origin',(31.5786285834019,2.1941463529156,33.830456743813));
#53950=CARTESIAN_POINT('Origin',(31.4230161011941,2.29812693362645,33.8304779343752));
#53951=CARTESIAN_POINT('Origin',(30.,-1.32966554433622E-14,33.8305837392638));
#53952=CARTESIAN_POINT('Origin',(31.4016114595758,2.31124030311394,33.8304567438134));
#53953=CARTESIAN_POINT('Origin',(31.2383204563814,2.40269113175683,33.8304779343751));
#53954=CARTESIAN_POINT('Origin',(30.,-1.32966554433622E-14,33.8305837392638));
#53955=CARTESIAN_POINT('Origin',(31.215952935018,2.41408468827632,33.8304567438131));
#53956=CARTESIAN_POINT('Origin',(31.0459901541714,2.49244194008366,33.8304779343748));
#53957=CARTESIAN_POINT('Origin',(30.,-1.32966554433622E-14,33.8305837392638));
#53958=CARTESIAN_POINT('Origin',(31.0227976562705,2.50204543857161,33.8304567438132));
#53959=CARTESIAN_POINT('Origin',(30.8472109748356,2.56682601503055,33.8304779343754));
#53960=CARTESIAN_POINT('Origin',(30.,-1.32966554433622E-14,33.8305837392638));
#53961=CARTESIAN_POINT('Origin',(30.8233364898573,2.574580246724,33.8304567438134));
#53962=CARTESIAN_POINT('Origin',(30.6432084580721,2.62538475398616,33.8304779343503));
#53963=CARTESIAN_POINT('Origin',(30.,-1.32966554433622E-14,33.8305837392638));
#53964=CARTESIAN_POINT('Origin',(30.6187991801972,2.63124191151918,33.8304567438131));
#53965=CARTESIAN_POINT('Origin',(30.4352403473569,2.66775712300684,33.8304779343755));
#53966=CARTESIAN_POINT('Origin',(30.,-1.32966554433622E-14,33.8305837392638));
#53967=CARTESIAN_POINT('Origin',(27.5973088682432,1.23832045638137,33.8304779343751));
#53968=CARTESIAN_POINT('Origin',(27.6887596968862,1.40161145957579,33.8304567438134));
#53969=CARTESIAN_POINT('Origin',(30.,-1.32966554433622E-14,33.8305837392638));
#53970=CARTESIAN_POINT('Origin',(27.7018730663741,1.4230161011934,33.8304779343749));
#53971=CARTESIAN_POINT('Origin',(27.8058536470835,1.57862858340213,33.8304567438133));
#53972=CARTESIAN_POINT('Origin',(30.,-1.32966554433622E-14,33.8305837392638));
#53973=CARTESIAN_POINT('Origin',(27.8206059812548,1.59893837854177,33.8304779343751));
#53974=CARTESIAN_POINT('Origin',(27.9364752391745,1.7459129370644,33.8304567438132));
#53975=CARTESIAN_POINT('Origin',(30.,-1.32966554433622E-14,33.8305837392638));
#53976=CARTESIAN_POINT('Origin',(27.952775584984,1.76500266908388,33.8304779343747));
#53977=CARTESIAN_POINT('Origin',(28.0798191476065,1.90243315689505,33.8304567438134));
#53978=CARTESIAN_POINT('Origin',(30.,-1.32966554433622E-14,33.8305837392638));
#53979=CARTESIAN_POINT('Origin',(28.0975670080041,1.92018513124447,33.8304779343728));
#53980=CARTESIAN_POINT('Origin',(28.23500160952,2.04722424368963,33.830456743813));
#53981=CARTESIAN_POINT('Origin',(30.,-1.32966554433622E-14,33.8305837392638));
#53982=CARTESIAN_POINT('Origin',(28.2540875630398,2.06352901355343,33.8304779343746));
#53983=CARTESIAN_POINT('Origin',(28.4010658734306,2.17939351225149,33.8304567438134));
#53984=CARTESIAN_POINT('Origin',(30.,-1.32966554433622E-14,33.8305837392638));
#53985=CARTESIAN_POINT('Origin',(28.4213722488255,2.19415055329726,33.8304779343749));
#53986=CARTESIAN_POINT('Origin',(28.5769880979325,2.29812609508769,33.8304567438131));
#53987=CARTESIAN_POINT('Origin',(30.,-1.32966554433622E-14,33.8305837392638));
#53988=CARTESIAN_POINT('Origin',(28.5983896996467,2.31124442523142,33.8304779343677));
#53989=CARTESIAN_POINT('Origin',(28.7616836640084,2.40268996634441,33.8304567438137));
#53990=CARTESIAN_POINT('Origin',(30.,-1.32966554433622E-14,33.8305837392638));
#53991=CARTESIAN_POINT('Origin',(28.7840485440478,2.41408870675589,33.8304779343753));
#53992=CARTESIAN_POINT('Origin',(28.9540138620795,2.49244045498167,33.8304567438133));
#53993=CARTESIAN_POINT('Origin',(30.,-1.32966554433622E-14,33.8305837392638));
#53994=CARTESIAN_POINT('Origin',(28.9772041335221,2.50204932861683,33.8304779343752));
#53995=CARTESIAN_POINT('Origin',(29.1527929125161,2.56682421939371,33.8304567438132));
#53996=CARTESIAN_POINT('Origin',(30.,-1.32966554433622E-14,33.8305837392638));
#53997=CARTESIAN_POINT('Origin',(29.1766655996273,2.57458398435145,33.8304779343752));
#53998=CARTESIAN_POINT('Origin',(29.3567952763716,2.62538265893797,33.8304567438133));
#53999=CARTESIAN_POINT('Origin',(30.,-1.32966554433622E-14,33.8305837392638));
#54000=CARTESIAN_POINT('Origin',(29.3812031960975,2.63124547368767,33.8304779343756));
#54001=CARTESIAN_POINT('Origin',(29.5647632112354,2.66775474136179,33.8304567438135));
#54002=CARTESIAN_POINT('Origin',(30.,-1.32966554433622E-14,33.8305837392638));
#54003=CARTESIAN_POINT('Origin',(29.5895558806117,2.67168445961877,33.8304779343432));
#54004=CARTESIAN_POINT('Origin',(29.775414525633,2.69367922868643,33.8304567438135));
#54005=CARTESIAN_POINT('Origin',(30.,-1.32966554433622E-14,33.8305837392638));
#54006=CARTESIAN_POINT('Origin',(29.8004390896529,2.69565162258947,33.8304779343745));
#54007=CARTESIAN_POINT('Origin',(29.9874504841622,2.70299628782743,33.8304567438137));
#54008=CARTESIAN_POINT('Origin',(30.,-1.32966554433622E-14,33.8305837392638));
#54009=CARTESIAN_POINT('Origin',(30.4104467678198,2.67168109495229,33.8304567438124));
#54010=CARTESIAN_POINT('Origin',(30.2245888351268,2.69368188219228,33.830477934375));
#54011=CARTESIAN_POINT('Origin',(30.,1.17524047358083,16.));
#54012=CARTESIAN_POINT('Origin',(30.,2.60624999999999,31.));
#54013=CARTESIAN_POINT('Origin',(30.,-1.32966554433622E-14,31.6569162607362));
#54014=CARTESIAN_POINT('',(30.1823521510466,2.74394746542433,31.6569162607362));
#54015=CARTESIAN_POINT('Origin',(30.1995609103462,2.69565162259179,31.6570220656244));
#54016=CARTESIAN_POINT('',(30.03349761664,2.74979597600974,31.6569162607362));
#54017=CARTESIAN_POINT('Origin',(30.0125495158372,2.70299628782596,31.6570432561867));
#54018=CARTESIAN_POINT('Origin',(30.,-1.32966554433622E-14,31.6569162607362));
#54019=CARTESIAN_POINT('Origin',(30.,-1.32966554433622E-14,16.));
#54020=CARTESIAN_POINT('',(30.1823521510466,2.74394746542434,33.8305837392638));
#54021=CARTESIAN_POINT('',(30.1823521510466,2.74394746542433,16.));
#54022=CARTESIAN_POINT('',(30.03349761664,2.74979597600975,33.8305837392638));
#54023=CARTESIAN_POINT('',(30.03349761664,2.74979597600974,16.));
#54024=CARTESIAN_POINT('Origin',(30.,-1.32966554433622E-14,33.8305837392638));
#54025=CARTESIAN_POINT('Origin',(30.,-1.32966554433622E-14,33.8305837392638));
#54026=CARTESIAN_POINT('Origin',(30.1995638146302,2.69564847601544,33.8304567438135));
#54027=CARTESIAN_POINT('Origin',(30.0125526580447,2.70299919683307,33.8304779343742));
#54028=CARTESIAN_POINT('Origin',(30.,-1.32966554433622E-14,34.));
#54029=CARTESIAN_POINT('Origin',(30.,-1.32966554433622E-14,32.5));
#54030=CARTESIAN_POINT('',(30.,-1.44337567297407,32.5));
#54031=CARTESIAN_POINT('',(31.25,-0.72168783648704,32.5));
#54032=CARTESIAN_POINT('',(30.,-1.44337567297407,32.5));
#54033=CARTESIAN_POINT('',(31.25,0.721687836487017,32.5));
#54034=CARTESIAN_POINT('',(31.25,-0.72168783648704,32.5));
#54035=CARTESIAN_POINT('',(30.,1.44337567297405,32.5));
#54036=CARTESIAN_POINT('',(31.25,0.721687836487017,32.5));
#54037=CARTESIAN_POINT('',(28.75,0.721687836487017,32.5));
#54038=CARTESIAN_POINT('',(30.,1.44337567297405,32.5));
#54039=CARTESIAN_POINT('',(28.75,-0.721687836487044,32.5));
#54040=CARTESIAN_POINT('',(28.75,0.721687836487017,32.5));
#54041=CARTESIAN_POINT('',(28.75,-0.721687836487044,32.5));
#54042=CARTESIAN_POINT('Origin',(31.25,-0.72168783648704,32.5));
#54043=CARTESIAN_POINT('',(31.25,-0.72168783648704,32.5));
#54044=CARTESIAN_POINT('',(31.25,0.721687836487017,32.5));
#54045=CARTESIAN_POINT('Origin',(31.25,0.721687836487017,32.5));
#54046=CARTESIAN_POINT('',(30.,1.44337567297405,32.5));
#54047=CARTESIAN_POINT('Origin',(30.,1.44337567297405,32.5));
#54048=CARTESIAN_POINT('',(28.75,0.721687836487017,32.5));
#54049=CARTESIAN_POINT('Origin',(28.75,0.721687836487017,32.5));
#54050=CARTESIAN_POINT('',(28.75,-0.721687836487044,32.5));
#54051=CARTESIAN_POINT('Origin',(28.75,-0.721687836487044,32.5));
#54052=CARTESIAN_POINT('',(30.,-1.44337567297407,32.5));
#54053=CARTESIAN_POINT('Origin',(30.,-1.44337567297407,32.5));
#54054=CARTESIAN_POINT('Ctrl Pts',(30.,1.17523237272422,15.7500046770317));
#54055=CARTESIAN_POINT('Ctrl Pts',(29.3214792732473,1.17523237272422,15.7916713436984));
#54056=CARTESIAN_POINT('Ctrl Pts',(28.9822189098709,0.587616186362105,15.8333380103651));
#54057=CARTESIAN_POINT('Ctrl Pts',(28.6429585464946,-1.32141491426617E-14,
15.8750046770317));
#54058=CARTESIAN_POINT('Ctrl Pts',(28.9822189098709,-0.587616186362132,
15.9166713436984));
#54059=CARTESIAN_POINT('Ctrl Pts',(29.3214792732473,-1.17523237272425,15.9583380103651));
#54060=CARTESIAN_POINT('Ctrl Pts',(30.,-1.17523237272425,16.0000046770317));
#54061=CARTESIAN_POINT('Ctrl Pts',(30.6785207267527,-1.17523237272425,16.0416713436984));
#54062=CARTESIAN_POINT('Ctrl Pts',(31.017781090129,-0.587616186362132,16.0833380103651));
#54063=CARTESIAN_POINT('Ctrl Pts',(31.3570414535054,-1.35453513912972E-14,
16.1250046770317));
#54064=CARTESIAN_POINT('Ctrl Pts',(31.017781090129,0.587616186362104,16.1666713436984));
#54065=CARTESIAN_POINT('Ctrl Pts',(30.6785207267527,1.17523237272422,16.2083380103651));
#54066=CARTESIAN_POINT('Ctrl Pts',(30.,1.17523237272422,16.2500046770317));
#54067=CARTESIAN_POINT('Ctrl Pts',(29.3214792732473,1.17523237272422,16.2916713436984));
#54068=CARTESIAN_POINT('Ctrl Pts',(28.9822189098709,0.587616186362105,16.3333380103651));
#54069=CARTESIAN_POINT('Ctrl Pts',(28.6429585464946,-1.32141491426617E-14,
16.3750046770317));
#54070=CARTESIAN_POINT('Ctrl Pts',(28.9822189098709,-0.587616186362132,
16.4166713436984));
#54071=CARTESIAN_POINT('Ctrl Pts',(29.3214792732473,-1.17523237272425,16.4583380103651));
#54072=CARTESIAN_POINT('Ctrl Pts',(30.,-1.17523237272425,16.5000046770317));
#54073=CARTESIAN_POINT('Ctrl Pts',(30.6785207267527,-1.17523237272425,16.5416713436984));
#54074=CARTESIAN_POINT('Ctrl Pts',(31.017781090129,-0.587616186362132,16.5833380103651));
#54075=CARTESIAN_POINT('Ctrl Pts',(31.3570414535054,-1.35453513912972E-14,
16.6250046770317));
#54076=CARTESIAN_POINT('Ctrl Pts',(31.017781090129,0.587616186362104,16.6666713436984));
#54077=CARTESIAN_POINT('Ctrl Pts',(30.6785207267527,1.17523237272422,16.7083380103651));
#54078=CARTESIAN_POINT('Ctrl Pts',(30.,1.17523237272422,16.7500046770317));
#54079=CARTESIAN_POINT('Ctrl Pts',(29.3214792732473,1.17523237272422,16.7916713436984));
#54080=CARTESIAN_POINT('Ctrl Pts',(28.9822189098709,0.587616186362105,16.8333380103651));
#54081=CARTESIAN_POINT('Ctrl Pts',(28.6429585464946,-1.32141491426617E-14,
16.8750046770317));
#54082=CARTESIAN_POINT('Ctrl Pts',(28.9822189098709,-0.587616186362132,
16.9166713436984));
#54083=CARTESIAN_POINT('Ctrl Pts',(29.3214792732473,-1.17523237272425,16.9583380103651));
#54084=CARTESIAN_POINT('Ctrl Pts',(30.,-1.17523237272425,17.0000046770317));
#54085=CARTESIAN_POINT('Ctrl Pts',(30.6785207267527,-1.17523237272425,17.0416713436984));
#54086=CARTESIAN_POINT('Ctrl Pts',(31.017781090129,-0.587616186362132,17.0833380103651));
#54087=CARTESIAN_POINT('Ctrl Pts',(31.3570414535054,-1.35453513912972E-14,
17.1250046770317));
#54088=CARTESIAN_POINT('Ctrl Pts',(31.017781090129,0.587616186362104,17.1666713436984));
#54089=CARTESIAN_POINT('Ctrl Pts',(30.6785207267527,1.17523237272422,17.2083380103651));
#54090=CARTESIAN_POINT('Ctrl Pts',(30.,1.17523237272422,17.2500046770317));
#54091=CARTESIAN_POINT('Ctrl Pts',(29.3214792732473,1.17523237272422,17.2916713436984));
#54092=CARTESIAN_POINT('Ctrl Pts',(28.9822189098709,0.587616186362105,17.3333380103651));
#54093=CARTESIAN_POINT('Ctrl Pts',(28.6429585464946,-1.32141491426617E-14,
17.3750046770317));
#54094=CARTESIAN_POINT('Ctrl Pts',(28.9822189098709,-0.587616186362132,
17.4166713436984));
#54095=CARTESIAN_POINT('Ctrl Pts',(29.3214792732473,-1.17523237272425,17.4583380103651));
#54096=CARTESIAN_POINT('Ctrl Pts',(30.,-1.17523237272425,17.5000046770317));
#54097=CARTESIAN_POINT('Ctrl Pts',(30.6785207267527,-1.17523237272425,17.5416713436984));
#54098=CARTESIAN_POINT('Ctrl Pts',(31.017781090129,-0.587616186362132,17.5833380103651));
#54099=CARTESIAN_POINT('Ctrl Pts',(31.3570414535054,-1.35453513912972E-14,
17.6250046770317));
#54100=CARTESIAN_POINT('Ctrl Pts',(31.017781090129,0.587616186362104,17.6666713436984));
#54101=CARTESIAN_POINT('Ctrl Pts',(30.6785207267527,1.17523237272422,17.7083380103651));
#54102=CARTESIAN_POINT('Ctrl Pts',(30.,1.17523237272422,17.7500046770317));
#54103=CARTESIAN_POINT('Ctrl Pts',(29.3214792732473,1.17523237272422,17.7916713436984));
#54104=CARTESIAN_POINT('Ctrl Pts',(28.9822189098709,0.587616186362105,17.8333380103651));
#54105=CARTESIAN_POINT('Ctrl Pts',(28.6429585464946,-1.32141491426617E-14,
17.8750046770317));
#54106=CARTESIAN_POINT('Ctrl Pts',(28.9822189098709,-0.587616186362132,
17.9166713436984));
#54107=CARTESIAN_POINT('Ctrl Pts',(29.3214792732473,-1.17523237272425,17.9583380103651));
#54108=CARTESIAN_POINT('Ctrl Pts',(30.,-1.17523237272425,18.0000046770317));
#54109=CARTESIAN_POINT('Ctrl Pts',(30.6785207267527,-1.17523237272425,18.0416713436984));
#54110=CARTESIAN_POINT('Ctrl Pts',(31.017781090129,-0.587616186362132,18.0833380103651));
#54111=CARTESIAN_POINT('Ctrl Pts',(31.3570414535054,-1.35453513912972E-14,
18.1250046770317));
#54112=CARTESIAN_POINT('Ctrl Pts',(31.017781090129,0.587616186362104,18.1666713436984));
#54113=CARTESIAN_POINT('Ctrl Pts',(30.6785207267527,1.17523237272422,18.2083380103651));
#54114=CARTESIAN_POINT('Ctrl Pts',(30.,1.17523237272422,18.2500046770317));
#54115=CARTESIAN_POINT('Ctrl Pts',(29.3214792732473,1.17523237272422,18.2916713436984));
#54116=CARTESIAN_POINT('Ctrl Pts',(28.9822189098709,0.587616186362105,18.3333380103651));
#54117=CARTESIAN_POINT('Ctrl Pts',(28.6429585464946,-1.32141491426617E-14,
18.3750046770317));
#54118=CARTESIAN_POINT('Ctrl Pts',(28.9822189098709,-0.587616186362132,
18.4166713436984));
#54119=CARTESIAN_POINT('Ctrl Pts',(29.3214792732473,-1.17523237272425,18.4583380103651));
#54120=CARTESIAN_POINT('Ctrl Pts',(30.,-1.17523237272425,18.5000046770317));
#54121=CARTESIAN_POINT('Ctrl Pts',(30.6785207267527,-1.17523237272425,18.5416713436984));
#54122=CARTESIAN_POINT('Ctrl Pts',(31.017781090129,-0.587616186362132,18.5833380103651));
#54123=CARTESIAN_POINT('Ctrl Pts',(31.3570414535054,-1.35453513912972E-14,
18.6250046770317));
#54124=CARTESIAN_POINT('Ctrl Pts',(31.017781090129,0.587616186362104,18.6666713436984));
#54125=CARTESIAN_POINT('Ctrl Pts',(30.6785207267527,1.17523237272422,18.7083380103651));
#54126=CARTESIAN_POINT('Ctrl Pts',(30.,1.17523237272422,18.7500046770317));
#54127=CARTESIAN_POINT('Ctrl Pts',(29.3214792732473,1.17523237272422,18.7916713436984));
#54128=CARTESIAN_POINT('Ctrl Pts',(28.9822189098709,0.587616186362105,18.8333380103651));
#54129=CARTESIAN_POINT('Ctrl Pts',(28.6429585464946,-1.32141491426617E-14,
18.8750046770317));
#54130=CARTESIAN_POINT('Ctrl Pts',(28.9822189098709,-0.587616186362132,
18.9166713436984));
#54131=CARTESIAN_POINT('Ctrl Pts',(29.3214792732473,-1.17523237272425,18.9583380103651));
#54132=CARTESIAN_POINT('Ctrl Pts',(30.,-1.17523237272425,19.0000046770317));
#54133=CARTESIAN_POINT('Ctrl Pts',(30.6785207267527,-1.17523237272425,19.0416713436984));
#54134=CARTESIAN_POINT('Ctrl Pts',(31.017781090129,-0.587616186362132,19.0833380103651));
#54135=CARTESIAN_POINT('Ctrl Pts',(31.3570414535054,-1.35453513912972E-14,
19.1250046770317));
#54136=CARTESIAN_POINT('Ctrl Pts',(31.017781090129,0.587616186362104,19.1666713436984));
#54137=CARTESIAN_POINT('Ctrl Pts',(30.6785207267527,1.17523237272422,19.2083380103651));
#54138=CARTESIAN_POINT('Ctrl Pts',(30.,1.17523237272422,19.2500046770317));
#54139=CARTESIAN_POINT('Ctrl Pts',(29.3214792732473,1.17523237272422,19.2916713436984));
#54140=CARTESIAN_POINT('Ctrl Pts',(28.9822189098709,0.587616186362105,19.3333380103651));
#54141=CARTESIAN_POINT('Ctrl Pts',(28.6429585464946,-1.32141491426617E-14,
19.3750046770317));
#54142=CARTESIAN_POINT('Ctrl Pts',(28.9822189098709,-0.587616186362132,
19.4166713436984));
#54143=CARTESIAN_POINT('Ctrl Pts',(29.3214792732473,-1.17523237272425,19.4583380103651));
#54144=CARTESIAN_POINT('Ctrl Pts',(30.,-1.17523237272425,19.5000046770317));
#54145=CARTESIAN_POINT('Ctrl Pts',(30.6785207267527,-1.17523237272425,19.5416713436984));
#54146=CARTESIAN_POINT('Ctrl Pts',(31.017781090129,-0.587616186362132,19.5833380103651));
#54147=CARTESIAN_POINT('Ctrl Pts',(31.3570414535054,-1.35453513912972E-14,
19.6250046770317));
#54148=CARTESIAN_POINT('Ctrl Pts',(31.017781090129,0.587616186362104,19.6666713436984));
#54149=CARTESIAN_POINT('Ctrl Pts',(30.6785207267527,1.17523237272422,19.7083380103651));
#54150=CARTESIAN_POINT('Ctrl Pts',(30.,1.17523237272422,19.7500046770317));
#54151=CARTESIAN_POINT('Ctrl Pts',(29.3214792732473,1.17523237272422,19.7916713436984));
#54152=CARTESIAN_POINT('Ctrl Pts',(28.9822189098709,0.587616186362105,19.8333380103651));
#54153=CARTESIAN_POINT('Ctrl Pts',(28.6429585464946,-1.32141491426617E-14,
19.8750046770317));
#54154=CARTESIAN_POINT('Ctrl Pts',(28.9822189098709,-0.587616186362132,
19.9166713436984));
#54155=CARTESIAN_POINT('Ctrl Pts',(29.3214792732473,-1.17523237272425,19.9583380103651));
#54156=CARTESIAN_POINT('Ctrl Pts',(30.,-1.17523237272425,20.0000046770317));
#54157=CARTESIAN_POINT('Ctrl Pts',(30.6785207267527,-1.17523237272425,20.0416713436984));
#54158=CARTESIAN_POINT('Ctrl Pts',(31.017781090129,-0.587616186362132,20.0833380103651));
#54159=CARTESIAN_POINT('Ctrl Pts',(31.3570414535054,-1.35453513912972E-14,
20.1250046770317));
#54160=CARTESIAN_POINT('Ctrl Pts',(31.017781090129,0.587616186362104,20.1666713436984));
#54161=CARTESIAN_POINT('Ctrl Pts',(30.6785207267527,1.17523237272422,20.2083380103651));
#54162=CARTESIAN_POINT('Ctrl Pts',(30.,1.17523237272422,20.2500046770317));
#54163=CARTESIAN_POINT('Ctrl Pts',(29.3214792732473,1.17523237272422,20.2916713436984));
#54164=CARTESIAN_POINT('Ctrl Pts',(28.9822189098709,0.587616186362105,20.3333380103651));
#54165=CARTESIAN_POINT('Ctrl Pts',(28.6429585464946,-1.32141491426617E-14,
20.3750046770317));
#54166=CARTESIAN_POINT('Ctrl Pts',(28.9822189098709,-0.587616186362132,
20.4166713436984));
#54167=CARTESIAN_POINT('Ctrl Pts',(29.3214792732473,-1.17523237272425,20.4583380103651));
#54168=CARTESIAN_POINT('Ctrl Pts',(30.,-1.17523237272425,20.5000046770317));
#54169=CARTESIAN_POINT('Ctrl Pts',(30.6785207267527,-1.17523237272425,20.5416713436984));
#54170=CARTESIAN_POINT('Ctrl Pts',(31.017781090129,-0.587616186362132,20.5833380103651));
#54171=CARTESIAN_POINT('Ctrl Pts',(31.3570414535054,-1.35453513912972E-14,
20.6250046770317));
#54172=CARTESIAN_POINT('Ctrl Pts',(31.017781090129,0.587616186362104,20.6666713436984));
#54173=CARTESIAN_POINT('Ctrl Pts',(30.6785207267527,1.17523237272422,20.7083380103651));
#54174=CARTESIAN_POINT('Ctrl Pts',(30.,1.17523237272422,20.7500046770317));
#54175=CARTESIAN_POINT('Ctrl Pts',(29.3214792732473,1.17523237272422,20.7916713436984));
#54176=CARTESIAN_POINT('Ctrl Pts',(28.9822189098709,0.587616186362105,20.8333380103651));
#54177=CARTESIAN_POINT('Ctrl Pts',(28.6429585464946,-1.32141491426617E-14,
20.8750046770317));
#54178=CARTESIAN_POINT('Ctrl Pts',(28.9822189098709,-0.587616186362132,
20.9166713436984));
#54179=CARTESIAN_POINT('Ctrl Pts',(29.3214792732473,-1.17523237272425,20.9583380103651));
#54180=CARTESIAN_POINT('Ctrl Pts',(30.,-1.17523237272425,21.0000046770317));
#54181=CARTESIAN_POINT('Ctrl Pts',(30.6785207267527,-1.17523237272425,21.0416713436984));
#54182=CARTESIAN_POINT('Ctrl Pts',(31.017781090129,-0.587616186362132,21.0833380103651));
#54183=CARTESIAN_POINT('Ctrl Pts',(31.3570414535054,-1.35453513912972E-14,
21.1250046770317));
#54184=CARTESIAN_POINT('Ctrl Pts',(31.017781090129,0.587616186362104,21.1666713436984));
#54185=CARTESIAN_POINT('Ctrl Pts',(30.6785207267527,1.17523237272422,21.2083380103651));
#54186=CARTESIAN_POINT('Ctrl Pts',(30.,1.17523237272422,21.2500046770317));
#54187=CARTESIAN_POINT('Ctrl Pts',(29.3214792732473,1.17523237272422,21.2916713436984));
#54188=CARTESIAN_POINT('Ctrl Pts',(28.9822189098709,0.587616186362105,21.3333380103651));
#54189=CARTESIAN_POINT('Ctrl Pts',(28.6429585464946,-1.32141491426617E-14,
21.3750046770317));
#54190=CARTESIAN_POINT('Ctrl Pts',(28.9822189098709,-0.587616186362132,
21.4166713436984));
#54191=CARTESIAN_POINT('Ctrl Pts',(29.3214792732473,-1.17523237272425,21.4583380103651));
#54192=CARTESIAN_POINT('Ctrl Pts',(30.,-1.17523237272425,21.5000046770317));
#54193=CARTESIAN_POINT('Ctrl Pts',(30.6785207267527,-1.17523237272425,21.5416713436984));
#54194=CARTESIAN_POINT('Ctrl Pts',(31.017781090129,-0.587616186362132,21.5833380103651));
#54195=CARTESIAN_POINT('Ctrl Pts',(31.3570414535054,-1.35453513912972E-14,
21.6250046770317));
#54196=CARTESIAN_POINT('Ctrl Pts',(31.017781090129,0.587616186362104,21.6666713436984));
#54197=CARTESIAN_POINT('Ctrl Pts',(30.6785207267527,1.17523237272422,21.7083380103651));
#54198=CARTESIAN_POINT('Ctrl Pts',(30.,1.17523237272422,21.7500046770317));
#54199=CARTESIAN_POINT('Ctrl Pts',(29.3214792732473,1.17523237272422,21.7916713436984));
#54200=CARTESIAN_POINT('Ctrl Pts',(28.9822189098709,0.587616186362105,21.8333380103651));
#54201=CARTESIAN_POINT('Ctrl Pts',(28.6429585464946,-1.32141491426617E-14,
21.8750046770317));
#54202=CARTESIAN_POINT('Ctrl Pts',(28.9822189098709,-0.587616186362132,
21.9166713436984));
#54203=CARTESIAN_POINT('Ctrl Pts',(29.3214792732473,-1.17523237272425,21.9583380103651));
#54204=CARTESIAN_POINT('Ctrl Pts',(30.,-1.17523237272425,22.0000046770317));
#54205=CARTESIAN_POINT('Ctrl Pts',(30.6785207267527,-1.17523237272425,22.0416713436984));
#54206=CARTESIAN_POINT('Ctrl Pts',(31.017781090129,-0.587616186362132,22.0833380103651));
#54207=CARTESIAN_POINT('Ctrl Pts',(31.3570414535054,-1.35453513912972E-14,
22.1250046770317));
#54208=CARTESIAN_POINT('Ctrl Pts',(31.017781090129,0.587616186362104,22.1666713436984));
#54209=CARTESIAN_POINT('Ctrl Pts',(30.6785207267527,1.17523237272422,22.2083380103651));
#54210=CARTESIAN_POINT('Ctrl Pts',(30.,1.17523237272422,22.2500046770317));
#54211=CARTESIAN_POINT('Ctrl Pts',(29.3214792732473,1.17523237272422,22.2916713436984));
#54212=CARTESIAN_POINT('Ctrl Pts',(28.9822189098709,0.587616186362105,22.3333380103651));
#54213=CARTESIAN_POINT('Ctrl Pts',(28.6429585464946,-1.32141491426617E-14,
22.3750046770317));
#54214=CARTESIAN_POINT('Ctrl Pts',(28.9822189098709,-0.587616186362132,
22.4166713436984));
#54215=CARTESIAN_POINT('Ctrl Pts',(29.3214792732473,-1.17523237272425,22.4583380103651));
#54216=CARTESIAN_POINT('Ctrl Pts',(30.,-1.17523237272425,22.5000046770317));
#54217=CARTESIAN_POINT('Ctrl Pts',(30.6785207267527,-1.17523237272425,22.5416713436984));
#54218=CARTESIAN_POINT('Ctrl Pts',(31.017781090129,-0.587616186362132,22.5833380103651));
#54219=CARTESIAN_POINT('Ctrl Pts',(31.3570414535054,-1.35453513912972E-14,
22.6250046770317));
#54220=CARTESIAN_POINT('Ctrl Pts',(31.017781090129,0.587616186362104,22.6666713436984));
#54221=CARTESIAN_POINT('Ctrl Pts',(30.6785207267527,1.17523237272422,22.7083380103651));
#54222=CARTESIAN_POINT('Ctrl Pts',(30.,1.17523237272422,22.7500046770317));
#54223=CARTESIAN_POINT('Ctrl Pts',(29.3214792732473,1.17523237272422,22.7916713436984));
#54224=CARTESIAN_POINT('Ctrl Pts',(28.9822189098709,0.587616186362105,22.8333380103651));
#54225=CARTESIAN_POINT('Ctrl Pts',(28.6429585464946,-1.32141491426617E-14,
22.8750046770317));
#54226=CARTESIAN_POINT('Ctrl Pts',(28.9822189098709,-0.587616186362132,
22.9166713436984));
#54227=CARTESIAN_POINT('Ctrl Pts',(29.3214792732473,-1.17523237272425,22.9583380103651));
#54228=CARTESIAN_POINT('Ctrl Pts',(30.,-1.17523237272425,23.0000046770317));
#54229=CARTESIAN_POINT('Ctrl Pts',(30.6785207267527,-1.17523237272425,23.0416713436984));
#54230=CARTESIAN_POINT('Ctrl Pts',(31.017781090129,-0.587616186362132,23.0833380103651));
#54231=CARTESIAN_POINT('Ctrl Pts',(31.3570414535054,-1.35453513912972E-14,
23.1250046770317));
#54232=CARTESIAN_POINT('Ctrl Pts',(31.017781090129,0.587616186362104,23.1666713436984));
#54233=CARTESIAN_POINT('Ctrl Pts',(30.6785207267527,1.17523237272422,23.2083380103651));
#54234=CARTESIAN_POINT('Ctrl Pts',(30.,1.17523237272422,23.2500046770317));
#54235=CARTESIAN_POINT('Ctrl Pts',(29.3214792732473,1.17523237272422,23.2916713436984));
#54236=CARTESIAN_POINT('Ctrl Pts',(28.9822189098709,0.587616186362105,23.3333380103651));
#54237=CARTESIAN_POINT('Ctrl Pts',(28.6429585464946,-1.32141491426617E-14,
23.3750046770317));
#54238=CARTESIAN_POINT('Ctrl Pts',(28.9822189098709,-0.587616186362132,
23.4166713436984));
#54239=CARTESIAN_POINT('Ctrl Pts',(29.3214792732473,-1.17523237272425,23.4583380103651));
#54240=CARTESIAN_POINT('Ctrl Pts',(30.,-1.17523237272425,23.5000046770317));
#54241=CARTESIAN_POINT('Ctrl Pts',(30.6785207267527,-1.17523237272425,23.5416713436984));
#54242=CARTESIAN_POINT('Ctrl Pts',(31.017781090129,-0.587616186362132,23.5833380103651));
#54243=CARTESIAN_POINT('Ctrl Pts',(31.3570414535054,-1.35453513912972E-14,
23.6250046770317));
#54244=CARTESIAN_POINT('Ctrl Pts',(31.017781090129,0.587616186362104,23.6666713436984));
#54245=CARTESIAN_POINT('Ctrl Pts',(30.6785207267527,1.17523237272422,23.7083380103651));
#54246=CARTESIAN_POINT('Ctrl Pts',(30.,1.17523237272422,23.7500046770317));
#54247=CARTESIAN_POINT('Ctrl Pts',(29.3214792732473,1.17523237272422,23.7916713436984));
#54248=CARTESIAN_POINT('Ctrl Pts',(28.9822189098709,0.587616186362105,23.8333380103651));
#54249=CARTESIAN_POINT('Ctrl Pts',(28.6429585464946,-1.32141491426617E-14,
23.8750046770317));
#54250=CARTESIAN_POINT('Ctrl Pts',(28.9822189098709,-0.587616186362132,
23.9166713436984));
#54251=CARTESIAN_POINT('Ctrl Pts',(29.3214792732473,-1.17523237272425,23.9583380103651));
#54252=CARTESIAN_POINT('Ctrl Pts',(30.,-1.17523237272425,24.0000046770317));
#54253=CARTESIAN_POINT('Ctrl Pts',(30.6785207267527,-1.17523237272425,24.0416713436984));
#54254=CARTESIAN_POINT('Ctrl Pts',(31.017781090129,-0.587616186362132,24.0833380103651));
#54255=CARTESIAN_POINT('Ctrl Pts',(31.3570414535054,-1.35453513912972E-14,
24.1250046770317));
#54256=CARTESIAN_POINT('Ctrl Pts',(31.017781090129,0.587616186362104,24.1666713436984));
#54257=CARTESIAN_POINT('Ctrl Pts',(30.6785207267527,1.17523237272422,24.2083380103651));
#54258=CARTESIAN_POINT('Ctrl Pts',(30.,1.17523237272422,24.2500046770317));
#54259=CARTESIAN_POINT('Ctrl Pts',(29.3214792732473,1.17523237272422,24.2916713436984));
#54260=CARTESIAN_POINT('Ctrl Pts',(28.9822189098709,0.587616186362105,24.3333380103651));
#54261=CARTESIAN_POINT('Ctrl Pts',(28.6429585464946,-1.32141491426617E-14,
24.3750046770317));
#54262=CARTESIAN_POINT('Ctrl Pts',(28.9822189098709,-0.587616186362132,
24.4166713436984));
#54263=CARTESIAN_POINT('Ctrl Pts',(29.3214792732473,-1.17523237272425,24.4583380103651));
#54264=CARTESIAN_POINT('Ctrl Pts',(30.,-1.17523237272425,24.5000046770317));
#54265=CARTESIAN_POINT('Ctrl Pts',(30.6785207267527,-1.17523237272425,24.5416713436984));
#54266=CARTESIAN_POINT('Ctrl Pts',(31.017781090129,-0.587616186362132,24.5833380103651));
#54267=CARTESIAN_POINT('Ctrl Pts',(31.3570414535054,-1.35453513912972E-14,
24.6250046770317));
#54268=CARTESIAN_POINT('Ctrl Pts',(31.017781090129,0.587616186362104,24.6666713436984));
#54269=CARTESIAN_POINT('Ctrl Pts',(30.6785207267527,1.17523237272422,24.7083380103651));
#54270=CARTESIAN_POINT('Ctrl Pts',(30.,1.17523237272422,24.7500046770317));
#54271=CARTESIAN_POINT('Ctrl Pts',(29.3214792732473,1.17523237272422,24.7916713436984));
#54272=CARTESIAN_POINT('Ctrl Pts',(28.9822189098709,0.587616186362105,24.8333380103651));
#54273=CARTESIAN_POINT('Ctrl Pts',(28.6429585464946,-1.32141491426617E-14,
24.8750046770317));
#54274=CARTESIAN_POINT('Ctrl Pts',(28.9822189098709,-0.587616186362132,
24.9166713436984));
#54275=CARTESIAN_POINT('Ctrl Pts',(29.3214792732473,-1.17523237272425,24.9583380103651));
#54276=CARTESIAN_POINT('Ctrl Pts',(30.,-1.17523237272425,25.0000046770317));
#54277=CARTESIAN_POINT('Ctrl Pts',(30.6785207267527,-1.17523237272425,25.0416713436984));
#54278=CARTESIAN_POINT('Ctrl Pts',(31.017781090129,-0.587616186362132,25.0833380103651));
#54279=CARTESIAN_POINT('Ctrl Pts',(31.3570414535054,-1.35453513912972E-14,
25.1250046770317));
#54280=CARTESIAN_POINT('Ctrl Pts',(31.017781090129,0.587616186362104,25.1666713436984));
#54281=CARTESIAN_POINT('Ctrl Pts',(30.6785207267527,1.17523237272422,25.2083380103651));
#54282=CARTESIAN_POINT('Ctrl Pts',(30.,1.17523237272422,25.2500046770317));
#54283=CARTESIAN_POINT('Ctrl Pts',(29.3214792732473,1.17523237272422,25.2916713436984));
#54284=CARTESIAN_POINT('Ctrl Pts',(28.9822189098709,0.587616186362105,25.3333380103651));
#54285=CARTESIAN_POINT('Ctrl Pts',(28.6429585464946,-1.32141491426617E-14,
25.3750046770317));
#54286=CARTESIAN_POINT('Ctrl Pts',(28.9822189098709,-0.587616186362132,
25.4166713436984));
#54287=CARTESIAN_POINT('Ctrl Pts',(29.3214792732473,-1.17523237272425,25.4583380103651));
#54288=CARTESIAN_POINT('Ctrl Pts',(30.,-1.17523237272425,25.5000046770317));
#54289=CARTESIAN_POINT('Ctrl Pts',(30.6785207267527,-1.17523237272425,25.5416713436984));
#54290=CARTESIAN_POINT('Ctrl Pts',(31.017781090129,-0.587616186362132,25.5833380103651));
#54291=CARTESIAN_POINT('Ctrl Pts',(31.3570414535054,-1.35453513912972E-14,
25.6250046770317));
#54292=CARTESIAN_POINT('Ctrl Pts',(31.017781090129,0.587616186362104,25.6666713436984));
#54293=CARTESIAN_POINT('Ctrl Pts',(30.6785207267527,1.17523237272422,25.7083380103651));
#54294=CARTESIAN_POINT('Ctrl Pts',(30.,1.17523237272422,25.7500046770317));
#54295=CARTESIAN_POINT('Ctrl Pts',(29.3214792732473,1.17523237272422,25.7916713436984));
#54296=CARTESIAN_POINT('Ctrl Pts',(28.9822189098709,0.587616186362105,25.8333380103651));
#54297=CARTESIAN_POINT('Ctrl Pts',(28.6429585464946,-1.32141491426617E-14,
25.8750046770317));
#54298=CARTESIAN_POINT('Ctrl Pts',(28.9822189098709,-0.587616186362132,
25.9166713436984));
#54299=CARTESIAN_POINT('Ctrl Pts',(29.3214792732473,-1.17523237272425,25.9583380103651));
#54300=CARTESIAN_POINT('Ctrl Pts',(30.,-1.17523237272425,26.0000046770317));
#54301=CARTESIAN_POINT('Ctrl Pts',(30.6785207267527,-1.17523237272425,26.0416713436984));
#54302=CARTESIAN_POINT('Ctrl Pts',(31.017781090129,-0.587616186362132,26.0833380103651));
#54303=CARTESIAN_POINT('Ctrl Pts',(31.3570414535054,-1.35453513912972E-14,
26.1250046770317));
#54304=CARTESIAN_POINT('Ctrl Pts',(31.017781090129,0.587616186362104,26.1666713436984));
#54305=CARTESIAN_POINT('Ctrl Pts',(30.6785207267527,1.17523237272422,26.2083380103651));
#54306=CARTESIAN_POINT('Ctrl Pts',(30.,1.17523237272422,26.2500046770317));
#54307=CARTESIAN_POINT('Ctrl Pts',(29.3214792732473,1.17523237272422,26.2916713436984));
#54308=CARTESIAN_POINT('Ctrl Pts',(28.9822189098709,0.587616186362105,26.3333380103651));
#54309=CARTESIAN_POINT('Ctrl Pts',(28.6429585464946,-1.32141491426617E-14,
26.3750046770317));
#54310=CARTESIAN_POINT('Ctrl Pts',(28.9822189098709,-0.587616186362132,
26.4166713436984));
#54311=CARTESIAN_POINT('Ctrl Pts',(29.3214792732473,-1.17523237272425,26.4583380103651));
#54312=CARTESIAN_POINT('Ctrl Pts',(30.,-1.17523237272425,26.5000046770317));
#54313=CARTESIAN_POINT('Ctrl Pts',(30.6785207267527,-1.17523237272425,26.5416713436984));
#54314=CARTESIAN_POINT('Ctrl Pts',(31.017781090129,-0.587616186362132,26.5833380103651));
#54315=CARTESIAN_POINT('Ctrl Pts',(31.3570414535054,-1.35453513912972E-14,
26.6250046770317));
#54316=CARTESIAN_POINT('Ctrl Pts',(31.017781090129,0.587616186362104,26.6666713436984));
#54317=CARTESIAN_POINT('Ctrl Pts',(30.6785207267527,1.17523237272422,26.7083380103651));
#54318=CARTESIAN_POINT('Ctrl Pts',(30.,1.17523237272422,26.7500046770317));
#54319=CARTESIAN_POINT('Ctrl Pts',(29.3214792732473,1.17523237272422,26.7916713436984));
#54320=CARTESIAN_POINT('Ctrl Pts',(28.9822189098709,0.587616186362105,26.8333380103651));
#54321=CARTESIAN_POINT('Ctrl Pts',(28.6429585464946,-1.32141491426617E-14,
26.8750046770317));
#54322=CARTESIAN_POINT('Ctrl Pts',(28.9822189098709,-0.587616186362132,
26.9166713436984));
#54323=CARTESIAN_POINT('Ctrl Pts',(29.3214792732473,-1.17523237272425,26.9583380103651));
#54324=CARTESIAN_POINT('Ctrl Pts',(30.,-1.17523237272425,27.0000046770317));
#54325=CARTESIAN_POINT('Ctrl Pts',(30.6785207267527,-1.17523237272425,27.0416713436984));
#54326=CARTESIAN_POINT('Ctrl Pts',(31.017781090129,-0.587616186362132,27.0833380103651));
#54327=CARTESIAN_POINT('Ctrl Pts',(31.3570414535054,-1.35453513912972E-14,
27.1250046770317));
#54328=CARTESIAN_POINT('Ctrl Pts',(31.017781090129,0.587616186362104,27.1666713436984));
#54329=CARTESIAN_POINT('Ctrl Pts',(30.6785207267527,1.17523237272422,27.2083380103651));
#54330=CARTESIAN_POINT('Ctrl Pts',(30.,1.17523237272422,27.2500046770317));
#54331=CARTESIAN_POINT('Ctrl Pts',(29.3214792732473,1.17523237272422,27.2916713436984));
#54332=CARTESIAN_POINT('Ctrl Pts',(28.9822189098709,0.587616186362105,27.3333380103651));
#54333=CARTESIAN_POINT('Ctrl Pts',(28.6429585464946,-1.32141491426617E-14,
27.3750046770317));
#54334=CARTESIAN_POINT('Ctrl Pts',(28.9822189098709,-0.587616186362132,
27.4166713436984));
#54335=CARTESIAN_POINT('Ctrl Pts',(29.3214792732473,-1.17523237272425,27.4583380103651));
#54336=CARTESIAN_POINT('Ctrl Pts',(30.,-1.17523237272425,27.5000046770317));
#54337=CARTESIAN_POINT('Ctrl Pts',(30.6785207267527,-1.17523237272425,27.5416713436984));
#54338=CARTESIAN_POINT('Ctrl Pts',(31.017781090129,-0.587616186362132,27.5833380103651));
#54339=CARTESIAN_POINT('Ctrl Pts',(31.3570414535054,-1.35453513912972E-14,
27.6250046770317));
#54340=CARTESIAN_POINT('Ctrl Pts',(31.017781090129,0.587616186362104,27.6666713436984));
#54341=CARTESIAN_POINT('Ctrl Pts',(30.6785207267527,1.17523237272422,27.7083380103651));
#54342=CARTESIAN_POINT('Ctrl Pts',(30.,1.17523237272422,27.7500046770317));
#54343=CARTESIAN_POINT('Ctrl Pts',(29.3214792732473,1.17523237272422,27.7916713436984));
#54344=CARTESIAN_POINT('Ctrl Pts',(28.9822189098709,0.587616186362105,27.8333380103651));
#54345=CARTESIAN_POINT('Ctrl Pts',(28.6429585464946,-1.32141491426617E-14,
27.8750046770317));
#54346=CARTESIAN_POINT('Ctrl Pts',(28.9822189098709,-0.587616186362132,
27.9166713436984));
#54347=CARTESIAN_POINT('Ctrl Pts',(29.3214792732473,-1.17523237272425,27.9583380103651));
#54348=CARTESIAN_POINT('Ctrl Pts',(30.,-1.17523237272425,28.0000046770317));
#54349=CARTESIAN_POINT('Ctrl Pts',(30.6785207267527,-1.17523237272425,28.0416713436984));
#54350=CARTESIAN_POINT('Ctrl Pts',(31.017781090129,-0.587616186362132,28.0833380103651));
#54351=CARTESIAN_POINT('Ctrl Pts',(31.3570414535054,-1.35453513912972E-14,
28.1250046770317));
#54352=CARTESIAN_POINT('Ctrl Pts',(31.017781090129,0.587616186362104,28.1666713436984));
#54353=CARTESIAN_POINT('Ctrl Pts',(30.6785207267527,1.17523237272422,28.2083380103651));
#54354=CARTESIAN_POINT('Ctrl Pts',(30.,1.17523237272422,28.2500046770317));
#54355=CARTESIAN_POINT('Ctrl Pts',(29.3214792732473,1.17523237272422,28.2916713436984));
#54356=CARTESIAN_POINT('Ctrl Pts',(28.9822189098709,0.587616186362105,28.3333380103651));
#54357=CARTESIAN_POINT('Ctrl Pts',(28.6429585464946,-1.32141491426617E-14,
28.3750046770317));
#54358=CARTESIAN_POINT('Ctrl Pts',(28.9822189098709,-0.587616186362132,
28.4166713436984));
#54359=CARTESIAN_POINT('Ctrl Pts',(29.3214792732473,-1.17523237272425,28.4583380103651));
#54360=CARTESIAN_POINT('Ctrl Pts',(30.,-1.17523237272425,28.5000046770317));
#54361=CARTESIAN_POINT('Ctrl Pts',(30.6785207267527,-1.17523237272425,28.5416713436984));
#54362=CARTESIAN_POINT('Ctrl Pts',(31.017781090129,-0.587616186362132,28.5833380103651));
#54363=CARTESIAN_POINT('Ctrl Pts',(31.3570414535054,-1.35453513912972E-14,
28.6250046770317));
#54364=CARTESIAN_POINT('Ctrl Pts',(31.017781090129,0.587616186362104,28.6666713436984));
#54365=CARTESIAN_POINT('Ctrl Pts',(30.6785207267527,1.17523237272422,28.7083380103651));
#54366=CARTESIAN_POINT('Ctrl Pts',(30.,1.17523237272422,28.7500046770317));
#54367=CARTESIAN_POINT('Ctrl Pts',(29.3214792732473,1.17523237272422,28.7916713436984));
#54368=CARTESIAN_POINT('Ctrl Pts',(28.9822189098709,0.587616186362105,28.8333380103651));
#54369=CARTESIAN_POINT('Ctrl Pts',(28.6429585464946,-1.32141491426617E-14,
28.8750046770317));
#54370=CARTESIAN_POINT('Ctrl Pts',(28.9822189098709,-0.587616186362132,
28.9166713436984));
#54371=CARTESIAN_POINT('Ctrl Pts',(29.3214792732473,-1.17523237272425,28.9583380103651));
#54372=CARTESIAN_POINT('Ctrl Pts',(30.,-1.17523237272425,29.0000046770317));
#54373=CARTESIAN_POINT('Ctrl Pts',(30.6785207267527,-1.17523237272425,29.0416713436984));
#54374=CARTESIAN_POINT('Ctrl Pts',(31.017781090129,-0.587616186362132,29.0833380103651));
#54375=CARTESIAN_POINT('Ctrl Pts',(31.3570414535054,-1.35453513912972E-14,
29.1250046770317));
#54376=CARTESIAN_POINT('Ctrl Pts',(31.017781090129,0.587616186362104,29.1666713436984));
#54377=CARTESIAN_POINT('Ctrl Pts',(30.6785207267527,1.17523237272422,29.2083380103651));
#54378=CARTESIAN_POINT('Ctrl Pts',(30.,1.17523237272422,29.2500046770317));
#54379=CARTESIAN_POINT('Ctrl Pts',(29.3214792732473,1.17523237272422,29.2916713436984));
#54380=CARTESIAN_POINT('Ctrl Pts',(28.9822189098709,0.587616186362105,29.3333380103651));
#54381=CARTESIAN_POINT('Ctrl Pts',(28.6429585464946,-1.32141491426617E-14,
29.3750046770317));
#54382=CARTESIAN_POINT('Ctrl Pts',(28.9822189098709,-0.587616186362132,
29.4166713436984));
#54383=CARTESIAN_POINT('Ctrl Pts',(29.3214792732473,-1.17523237272425,29.4583380103651));
#54384=CARTESIAN_POINT('Ctrl Pts',(30.,-1.17523237272425,29.5000046770317));
#54385=CARTESIAN_POINT('Ctrl Pts',(30.6785207267527,-1.17523237272425,29.5416713436984));
#54386=CARTESIAN_POINT('Ctrl Pts',(31.017781090129,-0.587616186362132,29.5833380103651));
#54387=CARTESIAN_POINT('Ctrl Pts',(31.3570414535054,-1.35453513912972E-14,
29.6250046770317));
#54388=CARTESIAN_POINT('Ctrl Pts',(31.017781090129,0.587616186362104,29.6666713436984));
#54389=CARTESIAN_POINT('Ctrl Pts',(30.6785207267527,1.17523237272422,29.7083380103651));
#54390=CARTESIAN_POINT('Ctrl Pts',(30.,1.17523237272422,29.7500046770317));
#54391=CARTESIAN_POINT('Ctrl Pts',(29.3214792732473,1.17523237272422,29.7916713436984));
#54392=CARTESIAN_POINT('Ctrl Pts',(28.9822189098709,0.587616186362105,29.8333380103651));
#54393=CARTESIAN_POINT('Ctrl Pts',(28.6429585464946,-1.32141491426617E-14,
29.8750046770317));
#54394=CARTESIAN_POINT('Ctrl Pts',(28.9822189098709,-0.587616186362132,
29.9166713436984));
#54395=CARTESIAN_POINT('Ctrl Pts',(29.3214792732473,-1.17523237272425,29.9583380103651));
#54396=CARTESIAN_POINT('Ctrl Pts',(30.,-1.17523237272425,30.0000046770317));
#54397=CARTESIAN_POINT('Ctrl Pts',(30.6785207267527,-1.17523237272425,30.0416713436984));
#54398=CARTESIAN_POINT('Ctrl Pts',(31.017781090129,-0.587616186362132,30.0833380103651));
#54399=CARTESIAN_POINT('Ctrl Pts',(31.3570414535054,-1.35453513912972E-14,
30.1250046770317));
#54400=CARTESIAN_POINT('Ctrl Pts',(31.017781090129,0.587616186362104,30.1666713436984));
#54401=CARTESIAN_POINT('Ctrl Pts',(30.6785207267527,1.17523237272422,30.2083380103651));
#54402=CARTESIAN_POINT('Ctrl Pts',(30.,1.17523237272422,30.2500046770317));
#54403=CARTESIAN_POINT('Ctrl Pts',(29.3214792732473,1.17523237272422,30.2916713436984));
#54404=CARTESIAN_POINT('Ctrl Pts',(28.9822189098709,0.587616186362105,30.3333380103651));
#54405=CARTESIAN_POINT('Ctrl Pts',(28.6429585464946,-1.32141491426617E-14,
30.3750046770317));
#54406=CARTESIAN_POINT('Ctrl Pts',(28.9822189098709,-0.587616186362132,
30.4166713436984));
#54407=CARTESIAN_POINT('Ctrl Pts',(29.3214792732473,-1.17523237272425,30.4583380103651));
#54408=CARTESIAN_POINT('Ctrl Pts',(30.,-1.17523237272425,30.5000046770317));
#54409=CARTESIAN_POINT('Ctrl Pts',(30.6785207267527,-1.17523237272425,30.5416713436984));
#54410=CARTESIAN_POINT('Ctrl Pts',(31.017781090129,-0.587616186362132,30.5833380103651));
#54411=CARTESIAN_POINT('Ctrl Pts',(31.3570414535054,-1.35453513912972E-14,
30.6250046770317));
#54412=CARTESIAN_POINT('Ctrl Pts',(31.017781090129,0.587616186362104,30.6666713436984));
#54413=CARTESIAN_POINT('Ctrl Pts',(30.6785207267527,1.17523237272422,30.7083380103651));
#54414=CARTESIAN_POINT('Ctrl Pts',(30.,1.17523237272422,30.7500046770317));
#54415=CARTESIAN_POINT('Ctrl Pts',(29.3214792732473,1.17523237272422,30.7916713436984));
#54416=CARTESIAN_POINT('Ctrl Pts',(28.9822189098709,0.587616186362105,30.8333380103651));
#54417=CARTESIAN_POINT('Ctrl Pts',(28.6429585464946,-1.32141491426617E-14,
30.8750046770317));
#54418=CARTESIAN_POINT('Ctrl Pts',(28.9822189098709,-0.587616186362132,
30.9166713436984));
#54419=CARTESIAN_POINT('Ctrl Pts',(29.3214792732473,-1.17523237272425,30.9583380103651));
#54420=CARTESIAN_POINT('Ctrl Pts',(30.,-1.17523237272425,31.0000046770317));
#54421=CARTESIAN_POINT('Ctrl Pts',(30.6785207267527,-1.17523237272425,31.0416713436984));
#54422=CARTESIAN_POINT('Ctrl Pts',(31.017781090129,-0.587616186362132,31.0833380103651));
#54423=CARTESIAN_POINT('Ctrl Pts',(31.3570414535054,-1.35453513912972E-14,
31.1250046770317));
#54424=CARTESIAN_POINT('Ctrl Pts',(31.017781090129,0.587616186362104,31.1666713436984));
#54425=CARTESIAN_POINT('Ctrl Pts',(30.6785207267527,1.17523237272422,31.2083380103651));
#54426=CARTESIAN_POINT('Ctrl Pts',(30.,1.17523237272422,31.2500046770317));
#54427=CARTESIAN_POINT('Ctrl Pts',(30.,1.52706329386825,15.546875));
#54428=CARTESIAN_POINT('Ctrl Pts',(29.1183495962155,1.52706329386825,15.5885416666667));
#54429=CARTESIAN_POINT('Ctrl Pts',(28.6775243943233,0.76353164693412,15.6302083333334));
#54430=CARTESIAN_POINT('Ctrl Pts',(28.2366991924311,-1.31894491186926E-14,
15.671875));
#54431=CARTESIAN_POINT('Ctrl Pts',(28.6775243943233,-0.763531646934146,
15.7135416666667));
#54432=CARTESIAN_POINT('Ctrl Pts',(29.1183495962155,-1.52706329386828,15.7552083333334));
#54433=CARTESIAN_POINT('Ctrl Pts',(30.,-1.52706329386828,15.796875));
#54434=CARTESIAN_POINT('Ctrl Pts',(30.8816504037844,-1.52706329386828,15.8385416666667));
#54435=CARTESIAN_POINT('Ctrl Pts',(31.3224756056766,-0.763531646934147,
15.8802083333334));
#54436=CARTESIAN_POINT('Ctrl Pts',(31.7633008075689,-1.36198038370242E-14,
15.921875));
#54437=CARTESIAN_POINT('Ctrl Pts',(31.3224756056766,0.763531646934118,15.9635416666667));
#54438=CARTESIAN_POINT('Ctrl Pts',(30.8816504037844,1.52706329386825,16.0052083333334));
#54439=CARTESIAN_POINT('Ctrl Pts',(30.,1.52706329386825,16.046875));
#54440=CARTESIAN_POINT('Ctrl Pts',(29.1183495962155,1.52706329386825,16.0885416666667));
#54441=CARTESIAN_POINT('Ctrl Pts',(28.6775243943233,0.76353164693412,16.1302083333334));
#54442=CARTESIAN_POINT('Ctrl Pts',(28.2366991924311,-1.31894491186926E-14,
16.171875));
#54443=CARTESIAN_POINT('Ctrl Pts',(28.6775243943233,-0.763531646934146,
16.2135416666667));
#54444=CARTESIAN_POINT('Ctrl Pts',(29.1183495962155,-1.52706329386828,16.2552083333334));
#54445=CARTESIAN_POINT('Ctrl Pts',(30.,-1.52706329386828,16.296875));
#54446=CARTESIAN_POINT('Ctrl Pts',(30.8816504037844,-1.52706329386828,16.3385416666667));
#54447=CARTESIAN_POINT('Ctrl Pts',(31.3224756056766,-0.763531646934147,
16.3802083333334));
#54448=CARTESIAN_POINT('Ctrl Pts',(31.7633008075689,-1.36198038370242E-14,
16.421875));
#54449=CARTESIAN_POINT('Ctrl Pts',(31.3224756056766,0.763531646934118,16.4635416666667));
#54450=CARTESIAN_POINT('Ctrl Pts',(30.8816504037844,1.52706329386825,16.5052083333334));
#54451=CARTESIAN_POINT('Ctrl Pts',(30.,1.52706329386825,16.546875));
#54452=CARTESIAN_POINT('Ctrl Pts',(29.1183495962155,1.52706329386825,16.5885416666667));
#54453=CARTESIAN_POINT('Ctrl Pts',(28.6775243943233,0.76353164693412,16.6302083333334));
#54454=CARTESIAN_POINT('Ctrl Pts',(28.2366991924311,-1.31894491186926E-14,
16.671875));
#54455=CARTESIAN_POINT('Ctrl Pts',(28.6775243943233,-0.763531646934146,
16.7135416666667));
#54456=CARTESIAN_POINT('Ctrl Pts',(29.1183495962155,-1.52706329386828,16.7552083333334));
#54457=CARTESIAN_POINT('Ctrl Pts',(30.,-1.52706329386828,16.796875));
#54458=CARTESIAN_POINT('Ctrl Pts',(30.8816504037844,-1.52706329386828,16.8385416666667));
#54459=CARTESIAN_POINT('Ctrl Pts',(31.3224756056766,-0.763531646934147,
16.8802083333334));
#54460=CARTESIAN_POINT('Ctrl Pts',(31.7633008075689,-1.36198038370242E-14,
16.921875));
#54461=CARTESIAN_POINT('Ctrl Pts',(31.3224756056766,0.763531646934118,16.9635416666667));
#54462=CARTESIAN_POINT('Ctrl Pts',(30.8816504037844,1.52706329386825,17.0052083333334));
#54463=CARTESIAN_POINT('Ctrl Pts',(30.,1.52706329386825,17.046875));
#54464=CARTESIAN_POINT('Ctrl Pts',(29.1183495962155,1.52706329386825,17.0885416666667));
#54465=CARTESIAN_POINT('Ctrl Pts',(28.6775243943233,0.76353164693412,17.1302083333334));
#54466=CARTESIAN_POINT('Ctrl Pts',(28.2366991924311,-1.31894491186926E-14,
17.171875));
#54467=CARTESIAN_POINT('Ctrl Pts',(28.6775243943233,-0.763531646934146,
17.2135416666667));
#54468=CARTESIAN_POINT('Ctrl Pts',(29.1183495962155,-1.52706329386828,17.2552083333334));
#54469=CARTESIAN_POINT('Ctrl Pts',(30.,-1.52706329386828,17.296875));
#54470=CARTESIAN_POINT('Ctrl Pts',(30.8816504037844,-1.52706329386828,17.3385416666667));
#54471=CARTESIAN_POINT('Ctrl Pts',(31.3224756056766,-0.763531646934147,
17.3802083333334));
#54472=CARTESIAN_POINT('Ctrl Pts',(31.7633008075689,-1.36198038370242E-14,
17.421875));
#54473=CARTESIAN_POINT('Ctrl Pts',(31.3224756056766,0.763531646934118,17.4635416666667));
#54474=CARTESIAN_POINT('Ctrl Pts',(30.8816504037844,1.52706329386825,17.5052083333334));
#54475=CARTESIAN_POINT('Ctrl Pts',(30.,1.52706329386825,17.546875));
#54476=CARTESIAN_POINT('Ctrl Pts',(29.1183495962155,1.52706329386825,17.5885416666667));
#54477=CARTESIAN_POINT('Ctrl Pts',(28.6775243943233,0.76353164693412,17.6302083333334));
#54478=CARTESIAN_POINT('Ctrl Pts',(28.2366991924311,-1.31894491186926E-14,
17.671875));
#54479=CARTESIAN_POINT('Ctrl Pts',(28.6775243943233,-0.763531646934146,
17.7135416666667));
#54480=CARTESIAN_POINT('Ctrl Pts',(29.1183495962155,-1.52706329386828,17.7552083333334));
#54481=CARTESIAN_POINT('Ctrl Pts',(30.,-1.52706329386828,17.796875));
#54482=CARTESIAN_POINT('Ctrl Pts',(30.8816504037844,-1.52706329386828,17.8385416666667));
#54483=CARTESIAN_POINT('Ctrl Pts',(31.3224756056766,-0.763531646934147,
17.8802083333334));
#54484=CARTESIAN_POINT('Ctrl Pts',(31.7633008075689,-1.36198038370242E-14,
17.921875));
#54485=CARTESIAN_POINT('Ctrl Pts',(31.3224756056766,0.763531646934118,17.9635416666667));
#54486=CARTESIAN_POINT('Ctrl Pts',(30.8816504037844,1.52706329386825,18.0052083333334));
#54487=CARTESIAN_POINT('Ctrl Pts',(30.,1.52706329386825,18.046875));
#54488=CARTESIAN_POINT('Ctrl Pts',(29.1183495962155,1.52706329386825,18.0885416666667));
#54489=CARTESIAN_POINT('Ctrl Pts',(28.6775243943233,0.76353164693412,18.1302083333334));
#54490=CARTESIAN_POINT('Ctrl Pts',(28.2366991924311,-1.31894491186926E-14,
18.171875));
#54491=CARTESIAN_POINT('Ctrl Pts',(28.6775243943233,-0.763531646934146,
18.2135416666667));
#54492=CARTESIAN_POINT('Ctrl Pts',(29.1183495962155,-1.52706329386828,18.2552083333334));
#54493=CARTESIAN_POINT('Ctrl Pts',(30.,-1.52706329386828,18.296875));
#54494=CARTESIAN_POINT('Ctrl Pts',(30.8816504037844,-1.52706329386828,18.3385416666667));
#54495=CARTESIAN_POINT('Ctrl Pts',(31.3224756056766,-0.763531646934147,
18.3802083333334));
#54496=CARTESIAN_POINT('Ctrl Pts',(31.7633008075689,-1.36198038370242E-14,
18.421875));
#54497=CARTESIAN_POINT('Ctrl Pts',(31.3224756056766,0.763531646934118,18.4635416666667));
#54498=CARTESIAN_POINT('Ctrl Pts',(30.8816504037844,1.52706329386825,18.5052083333334));
#54499=CARTESIAN_POINT('Ctrl Pts',(30.,1.52706329386825,18.546875));
#54500=CARTESIAN_POINT('Ctrl Pts',(29.1183495962155,1.52706329386825,18.5885416666667));
#54501=CARTESIAN_POINT('Ctrl Pts',(28.6775243943233,0.76353164693412,18.6302083333334));
#54502=CARTESIAN_POINT('Ctrl Pts',(28.2366991924311,-1.31894491186926E-14,
18.671875));
#54503=CARTESIAN_POINT('Ctrl Pts',(28.6775243943233,-0.763531646934146,
18.7135416666667));
#54504=CARTESIAN_POINT('Ctrl Pts',(29.1183495962155,-1.52706329386828,18.7552083333334));
#54505=CARTESIAN_POINT('Ctrl Pts',(30.,-1.52706329386828,18.796875));
#54506=CARTESIAN_POINT('Ctrl Pts',(30.8816504037844,-1.52706329386828,18.8385416666667));
#54507=CARTESIAN_POINT('Ctrl Pts',(31.3224756056766,-0.763531646934147,
18.8802083333334));
#54508=CARTESIAN_POINT('Ctrl Pts',(31.7633008075689,-1.36198038370242E-14,
18.921875));
#54509=CARTESIAN_POINT('Ctrl Pts',(31.3224756056766,0.763531646934118,18.9635416666667));
#54510=CARTESIAN_POINT('Ctrl Pts',(30.8816504037844,1.52706329386825,19.0052083333334));
#54511=CARTESIAN_POINT('Ctrl Pts',(30.,1.52706329386825,19.046875));
#54512=CARTESIAN_POINT('Ctrl Pts',(29.1183495962155,1.52706329386825,19.0885416666667));
#54513=CARTESIAN_POINT('Ctrl Pts',(28.6775243943233,0.76353164693412,19.1302083333334));
#54514=CARTESIAN_POINT('Ctrl Pts',(28.2366991924311,-1.31894491186926E-14,
19.171875));
#54515=CARTESIAN_POINT('Ctrl Pts',(28.6775243943233,-0.763531646934146,
19.2135416666667));
#54516=CARTESIAN_POINT('Ctrl Pts',(29.1183495962155,-1.52706329386828,19.2552083333334));
#54517=CARTESIAN_POINT('Ctrl Pts',(30.,-1.52706329386828,19.296875));
#54518=CARTESIAN_POINT('Ctrl Pts',(30.8816504037844,-1.52706329386828,19.3385416666667));
#54519=CARTESIAN_POINT('Ctrl Pts',(31.3224756056766,-0.763531646934147,
19.3802083333334));
#54520=CARTESIAN_POINT('Ctrl Pts',(31.7633008075689,-1.36198038370242E-14,
19.421875));
#54521=CARTESIAN_POINT('Ctrl Pts',(31.3224756056766,0.763531646934118,19.4635416666667));
#54522=CARTESIAN_POINT('Ctrl Pts',(30.8816504037844,1.52706329386825,19.5052083333334));
#54523=CARTESIAN_POINT('Ctrl Pts',(30.,1.52706329386825,19.546875));
#54524=CARTESIAN_POINT('Ctrl Pts',(29.1183495962155,1.52706329386825,19.5885416666667));
#54525=CARTESIAN_POINT('Ctrl Pts',(28.6775243943233,0.76353164693412,19.6302083333334));
#54526=CARTESIAN_POINT('Ctrl Pts',(28.2366991924311,-1.31894491186926E-14,
19.671875));
#54527=CARTESIAN_POINT('Ctrl Pts',(28.6775243943233,-0.763531646934146,
19.7135416666667));
#54528=CARTESIAN_POINT('Ctrl Pts',(29.1183495962155,-1.52706329386828,19.7552083333334));
#54529=CARTESIAN_POINT('Ctrl Pts',(30.,-1.52706329386828,19.796875));
#54530=CARTESIAN_POINT('Ctrl Pts',(30.8816504037844,-1.52706329386828,19.8385416666667));
#54531=CARTESIAN_POINT('Ctrl Pts',(31.3224756056766,-0.763531646934147,
19.8802083333334));
#54532=CARTESIAN_POINT('Ctrl Pts',(31.7633008075689,-1.36198038370242E-14,
19.921875));
#54533=CARTESIAN_POINT('Ctrl Pts',(31.3224756056766,0.763531646934118,19.9635416666667));
#54534=CARTESIAN_POINT('Ctrl Pts',(30.8816504037844,1.52706329386825,20.0052083333334));
#54535=CARTESIAN_POINT('Ctrl Pts',(30.,1.52706329386825,20.046875));
#54536=CARTESIAN_POINT('Ctrl Pts',(29.1183495962155,1.52706329386825,20.0885416666667));
#54537=CARTESIAN_POINT('Ctrl Pts',(28.6775243943233,0.76353164693412,20.1302083333334));
#54538=CARTESIAN_POINT('Ctrl Pts',(28.2366991924311,-1.31894491186926E-14,
20.171875));
#54539=CARTESIAN_POINT('Ctrl Pts',(28.6775243943233,-0.763531646934146,
20.2135416666667));
#54540=CARTESIAN_POINT('Ctrl Pts',(29.1183495962155,-1.52706329386828,20.2552083333334));
#54541=CARTESIAN_POINT('Ctrl Pts',(30.,-1.52706329386828,20.296875));
#54542=CARTESIAN_POINT('Ctrl Pts',(30.8816504037844,-1.52706329386828,20.3385416666667));
#54543=CARTESIAN_POINT('Ctrl Pts',(31.3224756056766,-0.763531646934147,
20.3802083333334));
#54544=CARTESIAN_POINT('Ctrl Pts',(31.7633008075689,-1.36198038370242E-14,
20.421875));
#54545=CARTESIAN_POINT('Ctrl Pts',(31.3224756056766,0.763531646934118,20.4635416666667));
#54546=CARTESIAN_POINT('Ctrl Pts',(30.8816504037844,1.52706329386825,20.5052083333334));
#54547=CARTESIAN_POINT('Ctrl Pts',(30.,1.52706329386825,20.546875));
#54548=CARTESIAN_POINT('Ctrl Pts',(29.1183495962155,1.52706329386825,20.5885416666667));
#54549=CARTESIAN_POINT('Ctrl Pts',(28.6775243943233,0.76353164693412,20.6302083333334));
#54550=CARTESIAN_POINT('Ctrl Pts',(28.2366991924311,-1.31894491186926E-14,
20.671875));
#54551=CARTESIAN_POINT('Ctrl Pts',(28.6775243943233,-0.763531646934146,
20.7135416666667));
#54552=CARTESIAN_POINT('Ctrl Pts',(29.1183495962155,-1.52706329386828,20.7552083333334));
#54553=CARTESIAN_POINT('Ctrl Pts',(30.,-1.52706329386828,20.796875));
#54554=CARTESIAN_POINT('Ctrl Pts',(30.8816504037844,-1.52706329386828,20.8385416666667));
#54555=CARTESIAN_POINT('Ctrl Pts',(31.3224756056766,-0.763531646934147,
20.8802083333334));
#54556=CARTESIAN_POINT('Ctrl Pts',(31.7633008075689,-1.36198038370242E-14,
20.921875));
#54557=CARTESIAN_POINT('Ctrl Pts',(31.3224756056766,0.763531646934118,20.9635416666667));
#54558=CARTESIAN_POINT('Ctrl Pts',(30.8816504037844,1.52706329386825,21.0052083333334));
#54559=CARTESIAN_POINT('Ctrl Pts',(30.,1.52706329386825,21.046875));
#54560=CARTESIAN_POINT('Ctrl Pts',(29.1183495962155,1.52706329386825,21.0885416666667));
#54561=CARTESIAN_POINT('Ctrl Pts',(28.6775243943233,0.76353164693412,21.1302083333334));
#54562=CARTESIAN_POINT('Ctrl Pts',(28.2366991924311,-1.31894491186926E-14,
21.171875));
#54563=CARTESIAN_POINT('Ctrl Pts',(28.6775243943233,-0.763531646934146,
21.2135416666667));
#54564=CARTESIAN_POINT('Ctrl Pts',(29.1183495962155,-1.52706329386828,21.2552083333334));
#54565=CARTESIAN_POINT('Ctrl Pts',(30.,-1.52706329386828,21.296875));
#54566=CARTESIAN_POINT('Ctrl Pts',(30.8816504037844,-1.52706329386828,21.3385416666667));
#54567=CARTESIAN_POINT('Ctrl Pts',(31.3224756056766,-0.763531646934147,
21.3802083333334));
#54568=CARTESIAN_POINT('Ctrl Pts',(31.7633008075689,-1.36198038370242E-14,
21.421875));
#54569=CARTESIAN_POINT('Ctrl Pts',(31.3224756056766,0.763531646934118,21.4635416666667));
#54570=CARTESIAN_POINT('Ctrl Pts',(30.8816504037844,1.52706329386825,21.5052083333334));
#54571=CARTESIAN_POINT('Ctrl Pts',(30.,1.52706329386825,21.546875));
#54572=CARTESIAN_POINT('Ctrl Pts',(29.1183495962155,1.52706329386825,21.5885416666667));
#54573=CARTESIAN_POINT('Ctrl Pts',(28.6775243943233,0.76353164693412,21.6302083333334));
#54574=CARTESIAN_POINT('Ctrl Pts',(28.2366991924311,-1.31894491186926E-14,
21.671875));
#54575=CARTESIAN_POINT('Ctrl Pts',(28.6775243943233,-0.763531646934146,
21.7135416666667));
#54576=CARTESIAN_POINT('Ctrl Pts',(29.1183495962155,-1.52706329386828,21.7552083333334));
#54577=CARTESIAN_POINT('Ctrl Pts',(30.,-1.52706329386828,21.796875));
#54578=CARTESIAN_POINT('Ctrl Pts',(30.8816504037844,-1.52706329386828,21.8385416666667));
#54579=CARTESIAN_POINT('Ctrl Pts',(31.3224756056766,-0.763531646934147,
21.8802083333334));
#54580=CARTESIAN_POINT('Ctrl Pts',(31.7633008075689,-1.36198038370242E-14,
21.921875));
#54581=CARTESIAN_POINT('Ctrl Pts',(31.3224756056766,0.763531646934118,21.9635416666667));
#54582=CARTESIAN_POINT('Ctrl Pts',(30.8816504037844,1.52706329386825,22.0052083333334));
#54583=CARTESIAN_POINT('Ctrl Pts',(30.,1.52706329386825,22.046875));
#54584=CARTESIAN_POINT('Ctrl Pts',(29.1183495962155,1.52706329386825,22.0885416666667));
#54585=CARTESIAN_POINT('Ctrl Pts',(28.6775243943233,0.76353164693412,22.1302083333334));
#54586=CARTESIAN_POINT('Ctrl Pts',(28.2366991924311,-1.31894491186926E-14,
22.171875));
#54587=CARTESIAN_POINT('Ctrl Pts',(28.6775243943233,-0.763531646934146,
22.2135416666667));
#54588=CARTESIAN_POINT('Ctrl Pts',(29.1183495962155,-1.52706329386828,22.2552083333334));
#54589=CARTESIAN_POINT('Ctrl Pts',(30.,-1.52706329386828,22.296875));
#54590=CARTESIAN_POINT('Ctrl Pts',(30.8816504037844,-1.52706329386828,22.3385416666667));
#54591=CARTESIAN_POINT('Ctrl Pts',(31.3224756056766,-0.763531646934147,
22.3802083333334));
#54592=CARTESIAN_POINT('Ctrl Pts',(31.7633008075689,-1.36198038370242E-14,
22.421875));
#54593=CARTESIAN_POINT('Ctrl Pts',(31.3224756056766,0.763531646934118,22.4635416666667));
#54594=CARTESIAN_POINT('Ctrl Pts',(30.8816504037844,1.52706329386825,22.5052083333334));
#54595=CARTESIAN_POINT('Ctrl Pts',(30.,1.52706329386825,22.546875));
#54596=CARTESIAN_POINT('Ctrl Pts',(29.1183495962155,1.52706329386825,22.5885416666667));
#54597=CARTESIAN_POINT('Ctrl Pts',(28.6775243943233,0.76353164693412,22.6302083333334));
#54598=CARTESIAN_POINT('Ctrl Pts',(28.2366991924311,-1.31894491186926E-14,
22.671875));
#54599=CARTESIAN_POINT('Ctrl Pts',(28.6775243943233,-0.763531646934146,
22.7135416666667));
#54600=CARTESIAN_POINT('Ctrl Pts',(29.1183495962155,-1.52706329386828,22.7552083333334));
#54601=CARTESIAN_POINT('Ctrl Pts',(30.,-1.52706329386828,22.796875));
#54602=CARTESIAN_POINT('Ctrl Pts',(30.8816504037844,-1.52706329386828,22.8385416666667));
#54603=CARTESIAN_POINT('Ctrl Pts',(31.3224756056766,-0.763531646934147,
22.8802083333334));
#54604=CARTESIAN_POINT('Ctrl Pts',(31.7633008075689,-1.36198038370242E-14,
22.921875));
#54605=CARTESIAN_POINT('Ctrl Pts',(31.3224756056766,0.763531646934118,22.9635416666667));
#54606=CARTESIAN_POINT('Ctrl Pts',(30.8816504037844,1.52706329386825,23.0052083333334));
#54607=CARTESIAN_POINT('Ctrl Pts',(30.,1.52706329386825,23.046875));
#54608=CARTESIAN_POINT('Ctrl Pts',(29.1183495962155,1.52706329386825,23.0885416666667));
#54609=CARTESIAN_POINT('Ctrl Pts',(28.6775243943233,0.76353164693412,23.1302083333334));
#54610=CARTESIAN_POINT('Ctrl Pts',(28.2366991924311,-1.31894491186926E-14,
23.171875));
#54611=CARTESIAN_POINT('Ctrl Pts',(28.6775243943233,-0.763531646934146,
23.2135416666667));
#54612=CARTESIAN_POINT('Ctrl Pts',(29.1183495962155,-1.52706329386828,23.2552083333334));
#54613=CARTESIAN_POINT('Ctrl Pts',(30.,-1.52706329386828,23.296875));
#54614=CARTESIAN_POINT('Ctrl Pts',(30.8816504037844,-1.52706329386828,23.3385416666667));
#54615=CARTESIAN_POINT('Ctrl Pts',(31.3224756056766,-0.763531646934147,
23.3802083333334));
#54616=CARTESIAN_POINT('Ctrl Pts',(31.7633008075689,-1.36198038370242E-14,
23.421875));
#54617=CARTESIAN_POINT('Ctrl Pts',(31.3224756056766,0.763531646934118,23.4635416666667));
#54618=CARTESIAN_POINT('Ctrl Pts',(30.8816504037844,1.52706329386825,23.5052083333334));
#54619=CARTESIAN_POINT('Ctrl Pts',(30.,1.52706329386825,23.546875));
#54620=CARTESIAN_POINT('Ctrl Pts',(29.1183495962155,1.52706329386825,23.5885416666667));
#54621=CARTESIAN_POINT('Ctrl Pts',(28.6775243943233,0.76353164693412,23.6302083333334));
#54622=CARTESIAN_POINT('Ctrl Pts',(28.2366991924311,-1.31894491186926E-14,
23.671875));
#54623=CARTESIAN_POINT('Ctrl Pts',(28.6775243943233,-0.763531646934146,
23.7135416666667));
#54624=CARTESIAN_POINT('Ctrl Pts',(29.1183495962155,-1.52706329386828,23.7552083333334));
#54625=CARTESIAN_POINT('Ctrl Pts',(30.,-1.52706329386828,23.796875));
#54626=CARTESIAN_POINT('Ctrl Pts',(30.8816504037844,-1.52706329386828,23.8385416666667));
#54627=CARTESIAN_POINT('Ctrl Pts',(31.3224756056766,-0.763531646934147,
23.8802083333334));
#54628=CARTESIAN_POINT('Ctrl Pts',(31.7633008075689,-1.36198038370242E-14,
23.921875));
#54629=CARTESIAN_POINT('Ctrl Pts',(31.3224756056766,0.763531646934118,23.9635416666667));
#54630=CARTESIAN_POINT('Ctrl Pts',(30.8816504037844,1.52706329386825,24.0052083333334));
#54631=CARTESIAN_POINT('Ctrl Pts',(30.,1.52706329386825,24.046875));
#54632=CARTESIAN_POINT('Ctrl Pts',(29.1183495962155,1.52706329386825,24.0885416666667));
#54633=CARTESIAN_POINT('Ctrl Pts',(28.6775243943233,0.76353164693412,24.1302083333334));
#54634=CARTESIAN_POINT('Ctrl Pts',(28.2366991924311,-1.31894491186926E-14,
24.171875));
#54635=CARTESIAN_POINT('Ctrl Pts',(28.6775243943233,-0.763531646934146,
24.2135416666667));
#54636=CARTESIAN_POINT('Ctrl Pts',(29.1183495962155,-1.52706329386828,24.2552083333334));
#54637=CARTESIAN_POINT('Ctrl Pts',(30.,-1.52706329386828,24.296875));
#54638=CARTESIAN_POINT('Ctrl Pts',(30.8816504037844,-1.52706329386828,24.3385416666667));
#54639=CARTESIAN_POINT('Ctrl Pts',(31.3224756056766,-0.763531646934147,
24.3802083333334));
#54640=CARTESIAN_POINT('Ctrl Pts',(31.7633008075689,-1.36198038370242E-14,
24.421875));
#54641=CARTESIAN_POINT('Ctrl Pts',(31.3224756056766,0.763531646934118,24.4635416666667));
#54642=CARTESIAN_POINT('Ctrl Pts',(30.8816504037844,1.52706329386825,24.5052083333334));
#54643=CARTESIAN_POINT('Ctrl Pts',(30.,1.52706329386825,24.546875));
#54644=CARTESIAN_POINT('Ctrl Pts',(29.1183495962155,1.52706329386825,24.5885416666667));
#54645=CARTESIAN_POINT('Ctrl Pts',(28.6775243943233,0.76353164693412,24.6302083333334));
#54646=CARTESIAN_POINT('Ctrl Pts',(28.2366991924311,-1.31894491186926E-14,
24.671875));
#54647=CARTESIAN_POINT('Ctrl Pts',(28.6775243943233,-0.763531646934146,
24.7135416666667));
#54648=CARTESIAN_POINT('Ctrl Pts',(29.1183495962155,-1.52706329386828,24.7552083333334));
#54649=CARTESIAN_POINT('Ctrl Pts',(30.,-1.52706329386828,24.796875));
#54650=CARTESIAN_POINT('Ctrl Pts',(30.8816504037844,-1.52706329386828,24.8385416666667));
#54651=CARTESIAN_POINT('Ctrl Pts',(31.3224756056766,-0.763531646934147,
24.8802083333334));
#54652=CARTESIAN_POINT('Ctrl Pts',(31.7633008075689,-1.36198038370242E-14,
24.921875));
#54653=CARTESIAN_POINT('Ctrl Pts',(31.3224756056766,0.763531646934118,24.9635416666667));
#54654=CARTESIAN_POINT('Ctrl Pts',(30.8816504037844,1.52706329386825,25.0052083333334));
#54655=CARTESIAN_POINT('Ctrl Pts',(30.,1.52706329386825,25.046875));
#54656=CARTESIAN_POINT('Ctrl Pts',(29.1183495962155,1.52706329386825,25.0885416666667));
#54657=CARTESIAN_POINT('Ctrl Pts',(28.6775243943233,0.76353164693412,25.1302083333334));
#54658=CARTESIAN_POINT('Ctrl Pts',(28.2366991924311,-1.31894491186926E-14,
25.171875));
#54659=CARTESIAN_POINT('Ctrl Pts',(28.6775243943233,-0.763531646934146,
25.2135416666667));
#54660=CARTESIAN_POINT('Ctrl Pts',(29.1183495962155,-1.52706329386828,25.2552083333334));
#54661=CARTESIAN_POINT('Ctrl Pts',(30.,-1.52706329386828,25.296875));
#54662=CARTESIAN_POINT('Ctrl Pts',(30.8816504037844,-1.52706329386828,25.3385416666667));
#54663=CARTESIAN_POINT('Ctrl Pts',(31.3224756056766,-0.763531646934147,
25.3802083333334));
#54664=CARTESIAN_POINT('Ctrl Pts',(31.7633008075689,-1.36198038370242E-14,
25.421875));
#54665=CARTESIAN_POINT('Ctrl Pts',(31.3224756056766,0.763531646934118,25.4635416666667));
#54666=CARTESIAN_POINT('Ctrl Pts',(30.8816504037844,1.52706329386825,25.5052083333334));
#54667=CARTESIAN_POINT('Ctrl Pts',(30.,1.52706329386825,25.546875));
#54668=CARTESIAN_POINT('Ctrl Pts',(29.1183495962155,1.52706329386825,25.5885416666667));
#54669=CARTESIAN_POINT('Ctrl Pts',(28.6775243943233,0.76353164693412,25.6302083333334));
#54670=CARTESIAN_POINT('Ctrl Pts',(28.2366991924311,-1.31894491186926E-14,
25.671875));
#54671=CARTESIAN_POINT('Ctrl Pts',(28.6775243943233,-0.763531646934146,
25.7135416666667));
#54672=CARTESIAN_POINT('Ctrl Pts',(29.1183495962155,-1.52706329386828,25.7552083333334));
#54673=CARTESIAN_POINT('Ctrl Pts',(30.,-1.52706329386828,25.796875));
#54674=CARTESIAN_POINT('Ctrl Pts',(30.8816504037844,-1.52706329386828,25.8385416666667));
#54675=CARTESIAN_POINT('Ctrl Pts',(31.3224756056766,-0.763531646934147,
25.8802083333334));
#54676=CARTESIAN_POINT('Ctrl Pts',(31.7633008075689,-1.36198038370242E-14,
25.921875));
#54677=CARTESIAN_POINT('Ctrl Pts',(31.3224756056766,0.763531646934118,25.9635416666667));
#54678=CARTESIAN_POINT('Ctrl Pts',(30.8816504037844,1.52706329386825,26.0052083333334));
#54679=CARTESIAN_POINT('Ctrl Pts',(30.,1.52706329386825,26.046875));
#54680=CARTESIAN_POINT('Ctrl Pts',(29.1183495962155,1.52706329386825,26.0885416666667));
#54681=CARTESIAN_POINT('Ctrl Pts',(28.6775243943233,0.76353164693412,26.1302083333334));
#54682=CARTESIAN_POINT('Ctrl Pts',(28.2366991924311,-1.31894491186926E-14,
26.171875));
#54683=CARTESIAN_POINT('Ctrl Pts',(28.6775243943233,-0.763531646934146,
26.2135416666667));
#54684=CARTESIAN_POINT('Ctrl Pts',(29.1183495962155,-1.52706329386828,26.2552083333334));
#54685=CARTESIAN_POINT('Ctrl Pts',(30.,-1.52706329386828,26.296875));
#54686=CARTESIAN_POINT('Ctrl Pts',(30.8816504037844,-1.52706329386828,26.3385416666667));
#54687=CARTESIAN_POINT('Ctrl Pts',(31.3224756056766,-0.763531646934147,
26.3802083333334));
#54688=CARTESIAN_POINT('Ctrl Pts',(31.7633008075689,-1.36198038370242E-14,
26.421875));
#54689=CARTESIAN_POINT('Ctrl Pts',(31.3224756056766,0.763531646934118,26.4635416666667));
#54690=CARTESIAN_POINT('Ctrl Pts',(30.8816504037844,1.52706329386825,26.5052083333334));
#54691=CARTESIAN_POINT('Ctrl Pts',(30.,1.52706329386825,26.546875));
#54692=CARTESIAN_POINT('Ctrl Pts',(29.1183495962155,1.52706329386825,26.5885416666667));
#54693=CARTESIAN_POINT('Ctrl Pts',(28.6775243943233,0.76353164693412,26.6302083333334));
#54694=CARTESIAN_POINT('Ctrl Pts',(28.2366991924311,-1.31894491186926E-14,
26.671875));
#54695=CARTESIAN_POINT('Ctrl Pts',(28.6775243943233,-0.763531646934146,
26.7135416666667));
#54696=CARTESIAN_POINT('Ctrl Pts',(29.1183495962155,-1.52706329386828,26.7552083333334));
#54697=CARTESIAN_POINT('Ctrl Pts',(30.,-1.52706329386828,26.796875));
#54698=CARTESIAN_POINT('Ctrl Pts',(30.8816504037844,-1.52706329386828,26.8385416666667));
#54699=CARTESIAN_POINT('Ctrl Pts',(31.3224756056766,-0.763531646934147,
26.8802083333334));
#54700=CARTESIAN_POINT('Ctrl Pts',(31.7633008075689,-1.36198038370242E-14,
26.921875));
#54701=CARTESIAN_POINT('Ctrl Pts',(31.3224756056766,0.763531646934118,26.9635416666667));
#54702=CARTESIAN_POINT('Ctrl Pts',(30.8816504037844,1.52706329386825,27.0052083333334));
#54703=CARTESIAN_POINT('Ctrl Pts',(30.,1.52706329386825,27.046875));
#54704=CARTESIAN_POINT('Ctrl Pts',(29.1183495962155,1.52706329386825,27.0885416666667));
#54705=CARTESIAN_POINT('Ctrl Pts',(28.6775243943233,0.76353164693412,27.1302083333334));
#54706=CARTESIAN_POINT('Ctrl Pts',(28.2366991924311,-1.31894491186926E-14,
27.171875));
#54707=CARTESIAN_POINT('Ctrl Pts',(28.6775243943233,-0.763531646934146,
27.2135416666667));
#54708=CARTESIAN_POINT('Ctrl Pts',(29.1183495962155,-1.52706329386828,27.2552083333334));
#54709=CARTESIAN_POINT('Ctrl Pts',(30.,-1.52706329386828,27.296875));
#54710=CARTESIAN_POINT('Ctrl Pts',(30.8816504037844,-1.52706329386828,27.3385416666667));
#54711=CARTESIAN_POINT('Ctrl Pts',(31.3224756056766,-0.763531646934147,
27.3802083333334));
#54712=CARTESIAN_POINT('Ctrl Pts',(31.7633008075689,-1.36198038370242E-14,
27.421875));
#54713=CARTESIAN_POINT('Ctrl Pts',(31.3224756056766,0.763531646934118,27.4635416666667));
#54714=CARTESIAN_POINT('Ctrl Pts',(30.8816504037844,1.52706329386825,27.5052083333334));
#54715=CARTESIAN_POINT('Ctrl Pts',(30.,1.52706329386825,27.546875));
#54716=CARTESIAN_POINT('Ctrl Pts',(29.1183495962155,1.52706329386825,27.5885416666667));
#54717=CARTESIAN_POINT('Ctrl Pts',(28.6775243943233,0.76353164693412,27.6302083333334));
#54718=CARTESIAN_POINT('Ctrl Pts',(28.2366991924311,-1.31894491186926E-14,
27.671875));
#54719=CARTESIAN_POINT('Ctrl Pts',(28.6775243943233,-0.763531646934146,
27.7135416666667));
#54720=CARTESIAN_POINT('Ctrl Pts',(29.1183495962155,-1.52706329386828,27.7552083333334));
#54721=CARTESIAN_POINT('Ctrl Pts',(30.,-1.52706329386828,27.796875));
#54722=CARTESIAN_POINT('Ctrl Pts',(30.8816504037844,-1.52706329386828,27.8385416666667));
#54723=CARTESIAN_POINT('Ctrl Pts',(31.3224756056766,-0.763531646934147,
27.8802083333334));
#54724=CARTESIAN_POINT('Ctrl Pts',(31.7633008075689,-1.36198038370242E-14,
27.921875));
#54725=CARTESIAN_POINT('Ctrl Pts',(31.3224756056766,0.763531646934118,27.9635416666667));
#54726=CARTESIAN_POINT('Ctrl Pts',(30.8816504037844,1.52706329386825,28.0052083333334));
#54727=CARTESIAN_POINT('Ctrl Pts',(30.,1.52706329386825,28.046875));
#54728=CARTESIAN_POINT('Ctrl Pts',(29.1183495962155,1.52706329386825,28.0885416666667));
#54729=CARTESIAN_POINT('Ctrl Pts',(28.6775243943233,0.76353164693412,28.1302083333334));
#54730=CARTESIAN_POINT('Ctrl Pts',(28.2366991924311,-1.31894491186926E-14,
28.171875));
#54731=CARTESIAN_POINT('Ctrl Pts',(28.6775243943233,-0.763531646934146,
28.2135416666667));
#54732=CARTESIAN_POINT('Ctrl Pts',(29.1183495962155,-1.52706329386828,28.2552083333334));
#54733=CARTESIAN_POINT('Ctrl Pts',(30.,-1.52706329386828,28.296875));
#54734=CARTESIAN_POINT('Ctrl Pts',(30.8816504037844,-1.52706329386828,28.3385416666667));
#54735=CARTESIAN_POINT('Ctrl Pts',(31.3224756056766,-0.763531646934147,
28.3802083333334));
#54736=CARTESIAN_POINT('Ctrl Pts',(31.7633008075689,-1.36198038370242E-14,
28.421875));
#54737=CARTESIAN_POINT('Ctrl Pts',(31.3224756056766,0.763531646934118,28.4635416666667));
#54738=CARTESIAN_POINT('Ctrl Pts',(30.8816504037844,1.52706329386825,28.5052083333334));
#54739=CARTESIAN_POINT('Ctrl Pts',(30.,1.52706329386825,28.546875));
#54740=CARTESIAN_POINT('Ctrl Pts',(29.1183495962155,1.52706329386825,28.5885416666667));
#54741=CARTESIAN_POINT('Ctrl Pts',(28.6775243943233,0.76353164693412,28.6302083333334));
#54742=CARTESIAN_POINT('Ctrl Pts',(28.2366991924311,-1.31894491186926E-14,
28.671875));
#54743=CARTESIAN_POINT('Ctrl Pts',(28.6775243943233,-0.763531646934146,
28.7135416666667));
#54744=CARTESIAN_POINT('Ctrl Pts',(29.1183495962155,-1.52706329386828,28.7552083333334));
#54745=CARTESIAN_POINT('Ctrl Pts',(30.,-1.52706329386828,28.796875));
#54746=CARTESIAN_POINT('Ctrl Pts',(30.8816504037844,-1.52706329386828,28.8385416666667));
#54747=CARTESIAN_POINT('Ctrl Pts',(31.3224756056766,-0.763531646934147,
28.8802083333334));
#54748=CARTESIAN_POINT('Ctrl Pts',(31.7633008075689,-1.36198038370242E-14,
28.921875));
#54749=CARTESIAN_POINT('Ctrl Pts',(31.3224756056766,0.763531646934118,28.9635416666667));
#54750=CARTESIAN_POINT('Ctrl Pts',(30.8816504037844,1.52706329386825,29.0052083333334));
#54751=CARTESIAN_POINT('Ctrl Pts',(30.,1.52706329386825,29.046875));
#54752=CARTESIAN_POINT('Ctrl Pts',(29.1183495962155,1.52706329386825,29.0885416666667));
#54753=CARTESIAN_POINT('Ctrl Pts',(28.6775243943233,0.76353164693412,29.1302083333334));
#54754=CARTESIAN_POINT('Ctrl Pts',(28.2366991924311,-1.31894491186926E-14,
29.171875));
#54755=CARTESIAN_POINT('Ctrl Pts',(28.6775243943233,-0.763531646934146,
29.2135416666667));
#54756=CARTESIAN_POINT('Ctrl Pts',(29.1183495962155,-1.52706329386828,29.2552083333334));
#54757=CARTESIAN_POINT('Ctrl Pts',(30.,-1.52706329386828,29.296875));
#54758=CARTESIAN_POINT('Ctrl Pts',(30.8816504037844,-1.52706329386828,29.3385416666667));
#54759=CARTESIAN_POINT('Ctrl Pts',(31.3224756056766,-0.763531646934147,
29.3802083333334));
#54760=CARTESIAN_POINT('Ctrl Pts',(31.7633008075689,-1.36198038370242E-14,
29.421875));
#54761=CARTESIAN_POINT('Ctrl Pts',(31.3224756056766,0.763531646934118,29.4635416666667));
#54762=CARTESIAN_POINT('Ctrl Pts',(30.8816504037844,1.52706329386825,29.5052083333334));
#54763=CARTESIAN_POINT('Ctrl Pts',(30.,1.52706329386825,29.546875));
#54764=CARTESIAN_POINT('Ctrl Pts',(29.1183495962155,1.52706329386825,29.5885416666667));
#54765=CARTESIAN_POINT('Ctrl Pts',(28.6775243943233,0.76353164693412,29.6302083333334));
#54766=CARTESIAN_POINT('Ctrl Pts',(28.2366991924311,-1.31894491186926E-14,
29.671875));
#54767=CARTESIAN_POINT('Ctrl Pts',(28.6775243943233,-0.763531646934146,
29.7135416666667));
#54768=CARTESIAN_POINT('Ctrl Pts',(29.1183495962155,-1.52706329386828,29.7552083333334));
#54769=CARTESIAN_POINT('Ctrl Pts',(30.,-1.52706329386828,29.796875));
#54770=CARTESIAN_POINT('Ctrl Pts',(30.8816504037844,-1.52706329386828,29.8385416666667));
#54771=CARTESIAN_POINT('Ctrl Pts',(31.3224756056766,-0.763531646934147,
29.8802083333334));
#54772=CARTESIAN_POINT('Ctrl Pts',(31.7633008075689,-1.36198038370242E-14,
29.921875));
#54773=CARTESIAN_POINT('Ctrl Pts',(31.3224756056766,0.763531646934118,29.9635416666667));
#54774=CARTESIAN_POINT('Ctrl Pts',(30.8816504037844,1.52706329386825,30.0052083333334));
#54775=CARTESIAN_POINT('Ctrl Pts',(30.,1.52706329386825,30.046875));
#54776=CARTESIAN_POINT('Ctrl Pts',(29.1183495962155,1.52706329386825,30.0885416666667));
#54777=CARTESIAN_POINT('Ctrl Pts',(28.6775243943233,0.76353164693412,30.1302083333334));
#54778=CARTESIAN_POINT('Ctrl Pts',(28.2366991924311,-1.31894491186926E-14,
30.171875));
#54779=CARTESIAN_POINT('Ctrl Pts',(28.6775243943233,-0.763531646934146,
30.2135416666667));
#54780=CARTESIAN_POINT('Ctrl Pts',(29.1183495962155,-1.52706329386828,30.2552083333334));
#54781=CARTESIAN_POINT('Ctrl Pts',(30.,-1.52706329386828,30.296875));
#54782=CARTESIAN_POINT('Ctrl Pts',(30.8816504037844,-1.52706329386828,30.3385416666667));
#54783=CARTESIAN_POINT('Ctrl Pts',(31.3224756056766,-0.763531646934147,
30.3802083333334));
#54784=CARTESIAN_POINT('Ctrl Pts',(31.7633008075689,-1.36198038370242E-14,
30.421875));
#54785=CARTESIAN_POINT('Ctrl Pts',(31.3224756056766,0.763531646934118,30.4635416666667));
#54786=CARTESIAN_POINT('Ctrl Pts',(30.8816504037844,1.52706329386825,30.5052083333334));
#54787=CARTESIAN_POINT('Ctrl Pts',(30.,1.52706329386825,30.546875));
#54788=CARTESIAN_POINT('Ctrl Pts',(29.1183495962155,1.52706329386825,30.5885416666667));
#54789=CARTESIAN_POINT('Ctrl Pts',(28.6775243943233,0.76353164693412,30.6302083333334));
#54790=CARTESIAN_POINT('Ctrl Pts',(28.2366991924311,-1.31894491186926E-14,
30.671875));
#54791=CARTESIAN_POINT('Ctrl Pts',(28.6775243943233,-0.763531646934146,
30.7135416666667));
#54792=CARTESIAN_POINT('Ctrl Pts',(29.1183495962155,-1.52706329386828,30.7552083333334));
#54793=CARTESIAN_POINT('Ctrl Pts',(30.,-1.52706329386828,30.796875));
#54794=CARTESIAN_POINT('Ctrl Pts',(30.8816504037844,-1.52706329386828,30.8385416666667));
#54795=CARTESIAN_POINT('Ctrl Pts',(31.3224756056766,-0.763531646934147,
30.8802083333334));
#54796=CARTESIAN_POINT('Ctrl Pts',(31.7633008075689,-1.36198038370242E-14,
30.921875));
#54797=CARTESIAN_POINT('Ctrl Pts',(31.3224756056766,0.763531646934118,30.9635416666667));
#54798=CARTESIAN_POINT('Ctrl Pts',(30.8816504037844,1.52706329386825,31.0052083333334));
#54799=CARTESIAN_POINT('Ctrl Pts',(30.,1.52706329386825,31.046875));
#54800=CARTESIAN_POINT('Ctrl Pts',(30.8234003400376,-0.838570603170131,
30.5624996575278));
#54801=CARTESIAN_POINT('Ctrl Pts',(30.9252409219315,-0.749808119816165,
30.5671289662449));
#54802=CARTESIAN_POINT('Ctrl Pts',(31.0094069192668,-0.645130506686946,
30.571193014068));
#54803=CARTESIAN_POINT('Ctrl Pts',(31.1396529784097,-0.412074319923831,
30.5795221820465));
#54804=CARTESIAN_POINT('Ctrl Pts',(31.1849584507844,-0.287685440765051,
30.5838904393726));
#54805=CARTESIAN_POINT('Ctrl Pts',(31.2386945750578,-0.00655181811616603,
30.5935664195233));
#54806=CARTESIAN_POINT('Ctrl Pts',(31.2387490550162,0.149503133824081,30.5988162542928));
#54807=CARTESIAN_POINT('Ctrl Pts',(31.1719223736106,0.500568259068406,30.610386374166));
#54808=CARTESIAN_POINT('Ctrl Pts',(31.0923154827319,0.652496494934345,30.6150433766711));
#54809=CARTESIAN_POINT('Ctrl Pts',(30.9283336729762,0.900293879400657,30.6239504439807));
#54810=CARTESIAN_POINT('Ctrl Pts',(30.8055598520391,1.02369588322745,30.6294622341334));
#54811=CARTESIAN_POINT('Ctrl Pts',(30.5288337282237,1.20882504193349,30.6401101417162));
#54812=CARTESIAN_POINT('Ctrl Pts',(30.3799906896905,1.27260041719159,30.6451552807199));
#54813=CARTESIAN_POINT('Ctrl Pts',(30.0014927028803,1.35728019461807,30.6565651904367));
#54814=CARTESIAN_POINT('Ctrl Pts',(29.8132785668206,1.33887636851719,30.6613880776071));
#54815=CARTESIAN_POINT('Ctrl Pts',(29.5198061598154,1.28660005614596,30.6701589170659));
#54816=CARTESIAN_POINT('Ctrl Pts',(29.3521505621284,1.22147978200258,30.6756096035631));
#54817=CARTESIAN_POINT('Ctrl Pts',(29.0485837866741,1.02916361274227,30.6863949411503));
#54818=CARTESIAN_POINT('Ctrl Pts',(28.9162494293832,0.902843317652004,30.6916208752244));
#54819=CARTESIAN_POINT('Ctrl Pts',(28.7272437086822,0.633185410868888,30.7002552651022));
#54820=CARTESIAN_POINT('Ctrl Pts',(28.6461891944724,0.476094037694283,30.7048351996635));
#54821=CARTESIAN_POINT('Ctrl Pts',(28.551105022901,0.105569064666544,30.715730913862));
#54822=CARTESIAN_POINT('Ctrl Pts',(28.5402826505383,-0.0831493783931786,
30.7211721595761));
#54823=CARTESIAN_POINT('Ctrl Pts',(28.5859138822382,-0.415083694084825,
30.7305650693331));
#54824=CARTESIAN_POINT('Ctrl Pts',(28.6283908398168,-0.557537406078615,
30.7345346397522));
#54825=CARTESIAN_POINT('Ctrl Pts',(28.7447696187018,-0.802908073480822,
30.7412906353098));
#54826=CARTESIAN_POINT('Ctrl Pts',(28.8264704242263,-0.938163811130005,
30.7451577422722));
#54827=CARTESIAN_POINT('Ctrl Pts',(28.9490560961683,-1.07028823734174,30.7500000000014));
#54828=CARTESIAN_POINT('Ctrl Pts',(30.,1.52706329386825,16.015625));
#54829=CARTESIAN_POINT('Ctrl Pts',(29.1183495962155,1.52706329386825,16.0572916666666));
#54830=CARTESIAN_POINT('Ctrl Pts',(28.6775243943233,0.76353164693412,16.0989583333333));
#54831=CARTESIAN_POINT('Ctrl Pts',(28.2366991924311,-1.31894491186926E-14,
16.140625));
#54832=CARTESIAN_POINT('Ctrl Pts',(28.6775243943233,-0.763531646934146,
16.1822916666666));
#54833=CARTESIAN_POINT('Ctrl Pts',(29.1183495962155,-1.52706329386828,16.2239583333333));
#54834=CARTESIAN_POINT('Ctrl Pts',(30.,-1.52706329386828,16.265625));
#54835=CARTESIAN_POINT('Ctrl Pts',(30.8816504037844,-1.52706329386828,16.3072916666666));
#54836=CARTESIAN_POINT('Ctrl Pts',(31.3224756056766,-0.763531646934147,
16.3489583333333));
#54837=CARTESIAN_POINT('Ctrl Pts',(31.7633008075689,-1.36198038370242E-14,
16.390625));
#54838=CARTESIAN_POINT('Ctrl Pts',(31.3224756056766,0.763531646934118,16.4322916666666));
#54839=CARTESIAN_POINT('Ctrl Pts',(30.8816504037844,1.52706329386825,16.4739583333333));
#54840=CARTESIAN_POINT('Ctrl Pts',(30.,1.52706329386825,16.515625));
#54841=CARTESIAN_POINT('Ctrl Pts',(29.1183495962155,1.52706329386825,16.5572916666666));
#54842=CARTESIAN_POINT('Ctrl Pts',(28.6775243943233,0.76353164693412,16.5989583333333));
#54843=CARTESIAN_POINT('Ctrl Pts',(28.2366991924311,-1.31894491186926E-14,
16.640625));
#54844=CARTESIAN_POINT('Ctrl Pts',(28.6775243943233,-0.763531646934146,
16.6822916666666));
#54845=CARTESIAN_POINT('Ctrl Pts',(29.1183495962155,-1.52706329386828,16.7239583333333));
#54846=CARTESIAN_POINT('Ctrl Pts',(30.,-1.52706329386828,16.765625));
#54847=CARTESIAN_POINT('Ctrl Pts',(30.8816504037844,-1.52706329386828,16.8072916666666));
#54848=CARTESIAN_POINT('Ctrl Pts',(31.3224756056766,-0.763531646934147,
16.8489583333333));
#54849=CARTESIAN_POINT('Ctrl Pts',(31.7633008075689,-1.36198038370242E-14,
16.890625));
#54850=CARTESIAN_POINT('Ctrl Pts',(31.3224756056766,0.763531646934118,16.9322916666666));
#54851=CARTESIAN_POINT('Ctrl Pts',(30.8816504037844,1.52706329386825,16.9739583333333));
#54852=CARTESIAN_POINT('Ctrl Pts',(30.,1.52706329386825,17.015625));
#54853=CARTESIAN_POINT('Ctrl Pts',(29.1183495962155,1.52706329386825,17.0572916666666));
#54854=CARTESIAN_POINT('Ctrl Pts',(28.6775243943233,0.76353164693412,17.0989583333333));
#54855=CARTESIAN_POINT('Ctrl Pts',(28.2366991924311,-1.31894491186926E-14,
17.140625));
#54856=CARTESIAN_POINT('Ctrl Pts',(28.6775243943233,-0.763531646934146,
17.1822916666666));
#54857=CARTESIAN_POINT('Ctrl Pts',(29.1183495962155,-1.52706329386828,17.2239583333333));
#54858=CARTESIAN_POINT('Ctrl Pts',(30.,-1.52706329386828,17.265625));
#54859=CARTESIAN_POINT('Ctrl Pts',(30.8816504037844,-1.52706329386828,17.3072916666666));
#54860=CARTESIAN_POINT('Ctrl Pts',(31.3224756056766,-0.763531646934147,
17.3489583333333));
#54861=CARTESIAN_POINT('Ctrl Pts',(31.7633008075689,-1.36198038370242E-14,
17.390625));
#54862=CARTESIAN_POINT('Ctrl Pts',(31.3224756056766,0.763531646934118,17.4322916666666));
#54863=CARTESIAN_POINT('Ctrl Pts',(30.8816504037844,1.52706329386825,17.4739583333333));
#54864=CARTESIAN_POINT('Ctrl Pts',(30.,1.52706329386825,17.515625));
#54865=CARTESIAN_POINT('Ctrl Pts',(29.1183495962155,1.52706329386825,17.5572916666666));
#54866=CARTESIAN_POINT('Ctrl Pts',(28.6775243943233,0.76353164693412,17.5989583333333));
#54867=CARTESIAN_POINT('Ctrl Pts',(28.2366991924311,-1.31894491186926E-14,
17.640625));
#54868=CARTESIAN_POINT('Ctrl Pts',(28.6775243943233,-0.763531646934146,
17.6822916666666));
#54869=CARTESIAN_POINT('Ctrl Pts',(29.1183495962155,-1.52706329386828,17.7239583333333));
#54870=CARTESIAN_POINT('Ctrl Pts',(30.,-1.52706329386828,17.765625));
#54871=CARTESIAN_POINT('Ctrl Pts',(30.8816504037844,-1.52706329386828,17.8072916666666));
#54872=CARTESIAN_POINT('Ctrl Pts',(31.3224756056766,-0.763531646934147,
17.8489583333333));
#54873=CARTESIAN_POINT('Ctrl Pts',(31.7633008075689,-1.36198038370242E-14,
17.890625));
#54874=CARTESIAN_POINT('Ctrl Pts',(31.3224756056766,0.763531646934118,17.9322916666666));
#54875=CARTESIAN_POINT('Ctrl Pts',(30.8816504037844,1.52706329386825,17.9739583333333));
#54876=CARTESIAN_POINT('Ctrl Pts',(30.,1.52706329386825,18.015625));
#54877=CARTESIAN_POINT('Ctrl Pts',(29.1183495962155,1.52706329386825,18.0572916666666));
#54878=CARTESIAN_POINT('Ctrl Pts',(28.6775243943233,0.76353164693412,18.0989583333333));
#54879=CARTESIAN_POINT('Ctrl Pts',(28.2366991924311,-1.31894491186926E-14,
18.140625));
#54880=CARTESIAN_POINT('Ctrl Pts',(28.6775243943233,-0.763531646934146,
18.1822916666666));
#54881=CARTESIAN_POINT('Ctrl Pts',(29.1183495962155,-1.52706329386828,18.2239583333333));
#54882=CARTESIAN_POINT('Ctrl Pts',(30.,-1.52706329386828,18.265625));
#54883=CARTESIAN_POINT('Ctrl Pts',(30.8816504037844,-1.52706329386828,18.3072916666666));
#54884=CARTESIAN_POINT('Ctrl Pts',(31.3224756056766,-0.763531646934147,
18.3489583333333));
#54885=CARTESIAN_POINT('Ctrl Pts',(31.7633008075689,-1.36198038370242E-14,
18.390625));
#54886=CARTESIAN_POINT('Ctrl Pts',(31.3224756056766,0.763531646934118,18.4322916666666));
#54887=CARTESIAN_POINT('Ctrl Pts',(30.8816504037844,1.52706329386825,18.4739583333333));
#54888=CARTESIAN_POINT('Ctrl Pts',(30.,1.52706329386825,18.515625));
#54889=CARTESIAN_POINT('Ctrl Pts',(29.1183495962155,1.52706329386825,18.5572916666666));
#54890=CARTESIAN_POINT('Ctrl Pts',(28.6775243943233,0.76353164693412,18.5989583333333));
#54891=CARTESIAN_POINT('Ctrl Pts',(28.2366991924311,-1.31894491186926E-14,
18.640625));
#54892=CARTESIAN_POINT('Ctrl Pts',(28.6775243943233,-0.763531646934146,
18.6822916666666));
#54893=CARTESIAN_POINT('Ctrl Pts',(29.1183495962155,-1.52706329386828,18.7239583333333));
#54894=CARTESIAN_POINT('Ctrl Pts',(30.,-1.52706329386828,18.765625));
#54895=CARTESIAN_POINT('Ctrl Pts',(30.8816504037844,-1.52706329386828,18.8072916666666));
#54896=CARTESIAN_POINT('Ctrl Pts',(31.3224756056766,-0.763531646934147,
18.8489583333333));
#54897=CARTESIAN_POINT('Ctrl Pts',(31.7633008075689,-1.36198038370242E-14,
18.890625));
#54898=CARTESIAN_POINT('Ctrl Pts',(31.3224756056766,0.763531646934118,18.9322916666666));
#54899=CARTESIAN_POINT('Ctrl Pts',(30.8816504037844,1.52706329386825,18.9739583333333));
#54900=CARTESIAN_POINT('Ctrl Pts',(30.,1.52706329386825,19.015625));
#54901=CARTESIAN_POINT('Ctrl Pts',(29.1183495962155,1.52706329386825,19.0572916666666));
#54902=CARTESIAN_POINT('Ctrl Pts',(28.6775243943233,0.76353164693412,19.0989583333333));
#54903=CARTESIAN_POINT('Ctrl Pts',(28.2366991924311,-1.31894491186926E-14,
19.140625));
#54904=CARTESIAN_POINT('Ctrl Pts',(28.6775243943233,-0.763531646934146,
19.1822916666666));
#54905=CARTESIAN_POINT('Ctrl Pts',(29.1183495962155,-1.52706329386828,19.2239583333333));
#54906=CARTESIAN_POINT('Ctrl Pts',(30.,-1.52706329386828,19.265625));
#54907=CARTESIAN_POINT('Ctrl Pts',(30.8816504037844,-1.52706329386828,19.3072916666666));
#54908=CARTESIAN_POINT('Ctrl Pts',(31.3224756056766,-0.763531646934147,
19.3489583333333));
#54909=CARTESIAN_POINT('Ctrl Pts',(31.7633008075689,-1.36198038370242E-14,
19.390625));
#54910=CARTESIAN_POINT('Ctrl Pts',(31.3224756056766,0.763531646934118,19.4322916666666));
#54911=CARTESIAN_POINT('Ctrl Pts',(30.8816504037844,1.52706329386825,19.4739583333333));
#54912=CARTESIAN_POINT('Ctrl Pts',(30.,1.52706329386825,19.515625));
#54913=CARTESIAN_POINT('Ctrl Pts',(29.1183495962155,1.52706329386825,19.5572916666666));
#54914=CARTESIAN_POINT('Ctrl Pts',(28.6775243943233,0.76353164693412,19.5989583333333));
#54915=CARTESIAN_POINT('Ctrl Pts',(28.2366991924311,-1.31894491186926E-14,
19.640625));
#54916=CARTESIAN_POINT('Ctrl Pts',(28.6775243943233,-0.763531646934146,
19.6822916666666));
#54917=CARTESIAN_POINT('Ctrl Pts',(29.1183495962155,-1.52706329386828,19.7239583333333));
#54918=CARTESIAN_POINT('Ctrl Pts',(30.,-1.52706329386828,19.765625));
#54919=CARTESIAN_POINT('Ctrl Pts',(30.8816504037844,-1.52706329386828,19.8072916666666));
#54920=CARTESIAN_POINT('Ctrl Pts',(31.3224756056766,-0.763531646934147,
19.8489583333333));
#54921=CARTESIAN_POINT('Ctrl Pts',(31.7633008075689,-1.36198038370242E-14,
19.890625));
#54922=CARTESIAN_POINT('Ctrl Pts',(31.3224756056766,0.763531646934118,19.9322916666666));
#54923=CARTESIAN_POINT('Ctrl Pts',(30.8816504037844,1.52706329386825,19.9739583333333));
#54924=CARTESIAN_POINT('Ctrl Pts',(30.,1.52706329386825,20.015625));
#54925=CARTESIAN_POINT('Ctrl Pts',(29.1183495962155,1.52706329386825,20.0572916666666));
#54926=CARTESIAN_POINT('Ctrl Pts',(28.6775243943233,0.76353164693412,20.0989583333333));
#54927=CARTESIAN_POINT('Ctrl Pts',(28.2366991924311,-1.31894491186926E-14,
20.140625));
#54928=CARTESIAN_POINT('Ctrl Pts',(28.6775243943233,-0.763531646934146,
20.1822916666666));
#54929=CARTESIAN_POINT('Ctrl Pts',(29.1183495962155,-1.52706329386828,20.2239583333333));
#54930=CARTESIAN_POINT('Ctrl Pts',(30.,-1.52706329386828,20.265625));
#54931=CARTESIAN_POINT('Ctrl Pts',(30.8816504037844,-1.52706329386828,20.3072916666666));
#54932=CARTESIAN_POINT('Ctrl Pts',(31.3224756056766,-0.763531646934147,
20.3489583333333));
#54933=CARTESIAN_POINT('Ctrl Pts',(31.7633008075689,-1.36198038370242E-14,
20.390625));
#54934=CARTESIAN_POINT('Ctrl Pts',(31.3224756056766,0.763531646934118,20.4322916666666));
#54935=CARTESIAN_POINT('Ctrl Pts',(30.8816504037844,1.52706329386825,20.4739583333333));
#54936=CARTESIAN_POINT('Ctrl Pts',(30.,1.52706329386825,20.515625));
#54937=CARTESIAN_POINT('Ctrl Pts',(29.1183495962155,1.52706329386825,20.5572916666666));
#54938=CARTESIAN_POINT('Ctrl Pts',(28.6775243943233,0.76353164693412,20.5989583333333));
#54939=CARTESIAN_POINT('Ctrl Pts',(28.2366991924311,-1.31894491186926E-14,
20.640625));
#54940=CARTESIAN_POINT('Ctrl Pts',(28.6775243943233,-0.763531646934146,
20.6822916666666));
#54941=CARTESIAN_POINT('Ctrl Pts',(29.1183495962155,-1.52706329386828,20.7239583333333));
#54942=CARTESIAN_POINT('Ctrl Pts',(30.,-1.52706329386828,20.765625));
#54943=CARTESIAN_POINT('Ctrl Pts',(30.8816504037844,-1.52706329386828,20.8072916666666));
#54944=CARTESIAN_POINT('Ctrl Pts',(31.3224756056766,-0.763531646934147,
20.8489583333333));
#54945=CARTESIAN_POINT('Ctrl Pts',(31.7633008075689,-1.36198038370242E-14,
20.890625));
#54946=CARTESIAN_POINT('Ctrl Pts',(31.3224756056766,0.763531646934118,20.9322916666666));
#54947=CARTESIAN_POINT('Ctrl Pts',(30.8816504037844,1.52706329386825,20.9739583333333));
#54948=CARTESIAN_POINT('Ctrl Pts',(30.,1.52706329386825,21.015625));
#54949=CARTESIAN_POINT('Ctrl Pts',(29.1183495962155,1.52706329386825,21.0572916666666));
#54950=CARTESIAN_POINT('Ctrl Pts',(28.6775243943233,0.76353164693412,21.0989583333333));
#54951=CARTESIAN_POINT('Ctrl Pts',(28.2366991924311,-1.31894491186926E-14,
21.140625));
#54952=CARTESIAN_POINT('Ctrl Pts',(28.6775243943233,-0.763531646934146,
21.1822916666666));
#54953=CARTESIAN_POINT('Ctrl Pts',(29.1183495962155,-1.52706329386828,21.2239583333333));
#54954=CARTESIAN_POINT('Ctrl Pts',(30.,-1.52706329386828,21.265625));
#54955=CARTESIAN_POINT('Ctrl Pts',(30.8816504037844,-1.52706329386828,21.3072916666666));
#54956=CARTESIAN_POINT('Ctrl Pts',(31.3224756056766,-0.763531646934147,
21.3489583333333));
#54957=CARTESIAN_POINT('Ctrl Pts',(31.7633008075689,-1.36198038370242E-14,
21.390625));
#54958=CARTESIAN_POINT('Ctrl Pts',(31.3224756056766,0.763531646934118,21.4322916666666));
#54959=CARTESIAN_POINT('Ctrl Pts',(30.8816504037844,1.52706329386825,21.4739583333333));
#54960=CARTESIAN_POINT('Ctrl Pts',(30.,1.52706329386825,21.515625));
#54961=CARTESIAN_POINT('Ctrl Pts',(29.1183495962155,1.52706329386825,21.5572916666666));
#54962=CARTESIAN_POINT('Ctrl Pts',(28.6775243943233,0.76353164693412,21.5989583333333));
#54963=CARTESIAN_POINT('Ctrl Pts',(28.2366991924311,-1.31894491186926E-14,
21.640625));
#54964=CARTESIAN_POINT('Ctrl Pts',(28.6775243943233,-0.763531646934146,
21.6822916666666));
#54965=CARTESIAN_POINT('Ctrl Pts',(29.1183495962155,-1.52706329386828,21.7239583333333));
#54966=CARTESIAN_POINT('Ctrl Pts',(30.,-1.52706329386828,21.765625));
#54967=CARTESIAN_POINT('Ctrl Pts',(30.8816504037844,-1.52706329386828,21.8072916666666));
#54968=CARTESIAN_POINT('Ctrl Pts',(31.3224756056766,-0.763531646934147,
21.8489583333333));
#54969=CARTESIAN_POINT('Ctrl Pts',(31.7633008075689,-1.36198038370242E-14,
21.890625));
#54970=CARTESIAN_POINT('Ctrl Pts',(31.3224756056766,0.763531646934118,21.9322916666666));
#54971=CARTESIAN_POINT('Ctrl Pts',(30.8816504037844,1.52706329386825,21.9739583333333));
#54972=CARTESIAN_POINT('Ctrl Pts',(30.,1.52706329386825,22.015625));
#54973=CARTESIAN_POINT('Ctrl Pts',(29.1183495962155,1.52706329386825,22.0572916666666));
#54974=CARTESIAN_POINT('Ctrl Pts',(28.6775243943233,0.76353164693412,22.0989583333333));
#54975=CARTESIAN_POINT('Ctrl Pts',(28.2366991924311,-1.31894491186926E-14,
22.140625));
#54976=CARTESIAN_POINT('Ctrl Pts',(28.6775243943233,-0.763531646934146,
22.1822916666666));
#54977=CARTESIAN_POINT('Ctrl Pts',(29.1183495962155,-1.52706329386828,22.2239583333333));
#54978=CARTESIAN_POINT('Ctrl Pts',(30.,-1.52706329386828,22.265625));
#54979=CARTESIAN_POINT('Ctrl Pts',(30.8816504037844,-1.52706329386828,22.3072916666666));
#54980=CARTESIAN_POINT('Ctrl Pts',(31.3224756056766,-0.763531646934147,
22.3489583333333));
#54981=CARTESIAN_POINT('Ctrl Pts',(31.7633008075689,-1.36198038370242E-14,
22.390625));
#54982=CARTESIAN_POINT('Ctrl Pts',(31.3224756056766,0.763531646934118,22.4322916666666));
#54983=CARTESIAN_POINT('Ctrl Pts',(30.8816504037844,1.52706329386825,22.4739583333333));
#54984=CARTESIAN_POINT('Ctrl Pts',(30.,1.52706329386825,22.515625));
#54985=CARTESIAN_POINT('Ctrl Pts',(29.1183495962155,1.52706329386825,22.5572916666666));
#54986=CARTESIAN_POINT('Ctrl Pts',(28.6775243943233,0.76353164693412,22.5989583333333));
#54987=CARTESIAN_POINT('Ctrl Pts',(28.2366991924311,-1.31894491186926E-14,
22.640625));
#54988=CARTESIAN_POINT('Ctrl Pts',(28.6775243943233,-0.763531646934146,
22.6822916666666));
#54989=CARTESIAN_POINT('Ctrl Pts',(29.1183495962155,-1.52706329386828,22.7239583333333));
#54990=CARTESIAN_POINT('Ctrl Pts',(30.,-1.52706329386828,22.765625));
#54991=CARTESIAN_POINT('Ctrl Pts',(30.8816504037844,-1.52706329386828,22.8072916666666));
#54992=CARTESIAN_POINT('Ctrl Pts',(31.3224756056766,-0.763531646934147,
22.8489583333333));
#54993=CARTESIAN_POINT('Ctrl Pts',(31.7633008075689,-1.36198038370242E-14,
22.890625));
#54994=CARTESIAN_POINT('Ctrl Pts',(31.3224756056766,0.763531646934118,22.9322916666666));
#54995=CARTESIAN_POINT('Ctrl Pts',(30.8816504037844,1.52706329386825,22.9739583333333));
#54996=CARTESIAN_POINT('Ctrl Pts',(30.,1.52706329386825,23.015625));
#54997=CARTESIAN_POINT('Ctrl Pts',(29.1183495962155,1.52706329386825,23.0572916666666));
#54998=CARTESIAN_POINT('Ctrl Pts',(28.6775243943233,0.76353164693412,23.0989583333333));
#54999=CARTESIAN_POINT('Ctrl Pts',(28.2366991924311,-1.31894491186926E-14,
23.140625));
#55000=CARTESIAN_POINT('Ctrl Pts',(28.6775243943233,-0.763531646934146,
23.1822916666666));
#55001=CARTESIAN_POINT('Ctrl Pts',(29.1183495962155,-1.52706329386828,23.2239583333333));
#55002=CARTESIAN_POINT('Ctrl Pts',(30.,-1.52706329386828,23.265625));
#55003=CARTESIAN_POINT('Ctrl Pts',(30.8816504037844,-1.52706329386828,23.3072916666666));
#55004=CARTESIAN_POINT('Ctrl Pts',(31.3224756056766,-0.763531646934147,
23.3489583333333));
#55005=CARTESIAN_POINT('Ctrl Pts',(31.7633008075689,-1.36198038370242E-14,
23.390625));
#55006=CARTESIAN_POINT('Ctrl Pts',(31.3224756056766,0.763531646934118,23.4322916666666));
#55007=CARTESIAN_POINT('Ctrl Pts',(30.8816504037844,1.52706329386825,23.4739583333333));
#55008=CARTESIAN_POINT('Ctrl Pts',(30.,1.52706329386825,23.515625));
#55009=CARTESIAN_POINT('Ctrl Pts',(29.1183495962155,1.52706329386825,23.5572916666666));
#55010=CARTESIAN_POINT('Ctrl Pts',(28.6775243943233,0.76353164693412,23.5989583333333));
#55011=CARTESIAN_POINT('Ctrl Pts',(28.2366991924311,-1.31894491186926E-14,
23.640625));
#55012=CARTESIAN_POINT('Ctrl Pts',(28.6775243943233,-0.763531646934146,
23.6822916666666));
#55013=CARTESIAN_POINT('Ctrl Pts',(29.1183495962155,-1.52706329386828,23.7239583333333));
#55014=CARTESIAN_POINT('Ctrl Pts',(30.,-1.52706329386828,23.765625));
#55015=CARTESIAN_POINT('Ctrl Pts',(30.8816504037844,-1.52706329386828,23.8072916666666));
#55016=CARTESIAN_POINT('Ctrl Pts',(31.3224756056766,-0.763531646934147,
23.8489583333333));
#55017=CARTESIAN_POINT('Ctrl Pts',(31.7633008075689,-1.36198038370242E-14,
23.890625));
#55018=CARTESIAN_POINT('Ctrl Pts',(31.3224756056766,0.763531646934118,23.9322916666666));
#55019=CARTESIAN_POINT('Ctrl Pts',(30.8816504037844,1.52706329386825,23.9739583333333));
#55020=CARTESIAN_POINT('Ctrl Pts',(30.,1.52706329386825,24.015625));
#55021=CARTESIAN_POINT('Ctrl Pts',(29.1183495962155,1.52706329386825,24.0572916666666));
#55022=CARTESIAN_POINT('Ctrl Pts',(28.6775243943233,0.76353164693412,24.0989583333333));
#55023=CARTESIAN_POINT('Ctrl Pts',(28.2366991924311,-1.31894491186926E-14,
24.140625));
#55024=CARTESIAN_POINT('Ctrl Pts',(28.6775243943233,-0.763531646934146,
24.1822916666666));
#55025=CARTESIAN_POINT('Ctrl Pts',(29.1183495962155,-1.52706329386828,24.2239583333333));
#55026=CARTESIAN_POINT('Ctrl Pts',(30.,-1.52706329386828,24.265625));
#55027=CARTESIAN_POINT('Ctrl Pts',(30.8816504037844,-1.52706329386828,24.3072916666666));
#55028=CARTESIAN_POINT('Ctrl Pts',(31.3224756056766,-0.763531646934147,
24.3489583333333));
#55029=CARTESIAN_POINT('Ctrl Pts',(31.7633008075689,-1.36198038370242E-14,
24.390625));
#55030=CARTESIAN_POINT('Ctrl Pts',(31.3224756056766,0.763531646934118,24.4322916666666));
#55031=CARTESIAN_POINT('Ctrl Pts',(30.8816504037844,1.52706329386825,24.4739583333333));
#55032=CARTESIAN_POINT('Ctrl Pts',(30.,1.52706329386825,24.515625));
#55033=CARTESIAN_POINT('Ctrl Pts',(29.1183495962155,1.52706329386825,24.5572916666666));
#55034=CARTESIAN_POINT('Ctrl Pts',(28.6775243943233,0.76353164693412,24.5989583333333));
#55035=CARTESIAN_POINT('Ctrl Pts',(28.2366991924311,-1.31894491186926E-14,
24.640625));
#55036=CARTESIAN_POINT('Ctrl Pts',(28.6775243943233,-0.763531646934146,
24.6822916666666));
#55037=CARTESIAN_POINT('Ctrl Pts',(29.1183495962155,-1.52706329386828,24.7239583333333));
#55038=CARTESIAN_POINT('Ctrl Pts',(30.,-1.52706329386828,24.765625));
#55039=CARTESIAN_POINT('Ctrl Pts',(30.8816504037844,-1.52706329386828,24.8072916666666));
#55040=CARTESIAN_POINT('Ctrl Pts',(31.3224756056766,-0.763531646934147,
24.8489583333333));
#55041=CARTESIAN_POINT('Ctrl Pts',(31.7633008075689,-1.36198038370242E-14,
24.890625));
#55042=CARTESIAN_POINT('Ctrl Pts',(31.3224756056766,0.763531646934118,24.9322916666666));
#55043=CARTESIAN_POINT('Ctrl Pts',(30.8816504037844,1.52706329386825,24.9739583333333));
#55044=CARTESIAN_POINT('Ctrl Pts',(30.,1.52706329386825,25.015625));
#55045=CARTESIAN_POINT('Ctrl Pts',(29.1183495962155,1.52706329386825,25.0572916666666));
#55046=CARTESIAN_POINT('Ctrl Pts',(28.6775243943233,0.76353164693412,25.0989583333333));
#55047=CARTESIAN_POINT('Ctrl Pts',(28.2366991924311,-1.31894491186926E-14,
25.140625));
#55048=CARTESIAN_POINT('Ctrl Pts',(28.6775243943233,-0.763531646934146,
25.1822916666666));
#55049=CARTESIAN_POINT('Ctrl Pts',(29.1183495962155,-1.52706329386828,25.2239583333333));
#55050=CARTESIAN_POINT('Ctrl Pts',(30.,-1.52706329386828,25.265625));
#55051=CARTESIAN_POINT('Ctrl Pts',(30.8816504037844,-1.52706329386828,25.3072916666666));
#55052=CARTESIAN_POINT('Ctrl Pts',(31.3224756056766,-0.763531646934147,
25.3489583333333));
#55053=CARTESIAN_POINT('Ctrl Pts',(31.7633008075689,-1.36198038370242E-14,
25.390625));
#55054=CARTESIAN_POINT('Ctrl Pts',(31.3224756056766,0.763531646934118,25.4322916666666));
#55055=CARTESIAN_POINT('Ctrl Pts',(30.8816504037844,1.52706329386825,25.4739583333333));
#55056=CARTESIAN_POINT('Ctrl Pts',(30.,1.52706329386825,25.515625));
#55057=CARTESIAN_POINT('Ctrl Pts',(29.1183495962155,1.52706329386825,25.5572916666666));
#55058=CARTESIAN_POINT('Ctrl Pts',(28.6775243943233,0.76353164693412,25.5989583333333));
#55059=CARTESIAN_POINT('Ctrl Pts',(28.2366991924311,-1.31894491186926E-14,
25.640625));
#55060=CARTESIAN_POINT('Ctrl Pts',(28.6775243943233,-0.763531646934146,
25.6822916666666));
#55061=CARTESIAN_POINT('Ctrl Pts',(29.1183495962155,-1.52706329386828,25.7239583333333));
#55062=CARTESIAN_POINT('Ctrl Pts',(30.,-1.52706329386828,25.765625));
#55063=CARTESIAN_POINT('Ctrl Pts',(30.8816504037844,-1.52706329386828,25.8072916666666));
#55064=CARTESIAN_POINT('Ctrl Pts',(31.3224756056766,-0.763531646934147,
25.8489583333333));
#55065=CARTESIAN_POINT('Ctrl Pts',(31.7633008075689,-1.36198038370242E-14,
25.890625));
#55066=CARTESIAN_POINT('Ctrl Pts',(31.3224756056766,0.763531646934118,25.9322916666666));
#55067=CARTESIAN_POINT('Ctrl Pts',(30.8816504037844,1.52706329386825,25.9739583333333));
#55068=CARTESIAN_POINT('Ctrl Pts',(30.,1.52706329386825,26.015625));
#55069=CARTESIAN_POINT('Ctrl Pts',(29.1183495962155,1.52706329386825,26.0572916666666));
#55070=CARTESIAN_POINT('Ctrl Pts',(28.6775243943233,0.76353164693412,26.0989583333333));
#55071=CARTESIAN_POINT('Ctrl Pts',(28.2366991924311,-1.31894491186926E-14,
26.140625));
#55072=CARTESIAN_POINT('Ctrl Pts',(28.6775243943233,-0.763531646934146,
26.1822916666666));
#55073=CARTESIAN_POINT('Ctrl Pts',(29.1183495962155,-1.52706329386828,26.2239583333333));
#55074=CARTESIAN_POINT('Ctrl Pts',(30.,-1.52706329386828,26.265625));
#55075=CARTESIAN_POINT('Ctrl Pts',(30.8816504037844,-1.52706329386828,26.3072916666666));
#55076=CARTESIAN_POINT('Ctrl Pts',(31.3224756056766,-0.763531646934147,
26.3489583333333));
#55077=CARTESIAN_POINT('Ctrl Pts',(31.7633008075689,-1.36198038370242E-14,
26.390625));
#55078=CARTESIAN_POINT('Ctrl Pts',(31.3224756056766,0.763531646934118,26.4322916666666));
#55079=CARTESIAN_POINT('Ctrl Pts',(30.8816504037844,1.52706329386825,26.4739583333333));
#55080=CARTESIAN_POINT('Ctrl Pts',(30.,1.52706329386825,26.515625));
#55081=CARTESIAN_POINT('Ctrl Pts',(29.1183495962155,1.52706329386825,26.5572916666666));
#55082=CARTESIAN_POINT('Ctrl Pts',(28.6775243943233,0.76353164693412,26.5989583333333));
#55083=CARTESIAN_POINT('Ctrl Pts',(28.2366991924311,-1.31894491186926E-14,
26.640625));
#55084=CARTESIAN_POINT('Ctrl Pts',(28.6775243943233,-0.763531646934146,
26.6822916666666));
#55085=CARTESIAN_POINT('Ctrl Pts',(29.1183495962155,-1.52706329386828,26.7239583333333));
#55086=CARTESIAN_POINT('Ctrl Pts',(30.,-1.52706329386828,26.765625));
#55087=CARTESIAN_POINT('Ctrl Pts',(30.8816504037844,-1.52706329386828,26.8072916666666));
#55088=CARTESIAN_POINT('Ctrl Pts',(31.3224756056766,-0.763531646934147,
26.8489583333333));
#55089=CARTESIAN_POINT('Ctrl Pts',(31.7633008075689,-1.36198038370242E-14,
26.890625));
#55090=CARTESIAN_POINT('Ctrl Pts',(31.3224756056766,0.763531646934118,26.9322916666666));
#55091=CARTESIAN_POINT('Ctrl Pts',(30.8816504037844,1.52706329386825,26.9739583333333));
#55092=CARTESIAN_POINT('Ctrl Pts',(30.,1.52706329386825,27.015625));
#55093=CARTESIAN_POINT('Ctrl Pts',(29.1183495962155,1.52706329386825,27.0572916666666));
#55094=CARTESIAN_POINT('Ctrl Pts',(28.6775243943233,0.76353164693412,27.0989583333333));
#55095=CARTESIAN_POINT('Ctrl Pts',(28.2366991924311,-1.31894491186926E-14,
27.140625));
#55096=CARTESIAN_POINT('Ctrl Pts',(28.6775243943233,-0.763531646934146,
27.1822916666666));
#55097=CARTESIAN_POINT('Ctrl Pts',(29.1183495962155,-1.52706329386828,27.2239583333333));
#55098=CARTESIAN_POINT('Ctrl Pts',(30.,-1.52706329386828,27.265625));
#55099=CARTESIAN_POINT('Ctrl Pts',(30.8816504037844,-1.52706329386828,27.3072916666666));
#55100=CARTESIAN_POINT('Ctrl Pts',(31.3224756056766,-0.763531646934147,
27.3489583333333));
#55101=CARTESIAN_POINT('Ctrl Pts',(31.7633008075689,-1.36198038370242E-14,
27.390625));
#55102=CARTESIAN_POINT('Ctrl Pts',(31.3224756056766,0.763531646934118,27.4322916666666));
#55103=CARTESIAN_POINT('Ctrl Pts',(30.8816504037844,1.52706329386825,27.4739583333333));
#55104=CARTESIAN_POINT('Ctrl Pts',(30.,1.52706329386825,27.515625));
#55105=CARTESIAN_POINT('Ctrl Pts',(29.1183495962155,1.52706329386825,27.5572916666666));
#55106=CARTESIAN_POINT('Ctrl Pts',(28.6775243943233,0.76353164693412,27.5989583333333));
#55107=CARTESIAN_POINT('Ctrl Pts',(28.2366991924311,-1.31894491186926E-14,
27.640625));
#55108=CARTESIAN_POINT('Ctrl Pts',(28.6775243943233,-0.763531646934146,
27.6822916666666));
#55109=CARTESIAN_POINT('Ctrl Pts',(29.1183495962155,-1.52706329386828,27.7239583333333));
#55110=CARTESIAN_POINT('Ctrl Pts',(30.,-1.52706329386828,27.765625));
#55111=CARTESIAN_POINT('Ctrl Pts',(30.8816504037844,-1.52706329386828,27.8072916666666));
#55112=CARTESIAN_POINT('Ctrl Pts',(31.3224756056766,-0.763531646934147,
27.8489583333333));
#55113=CARTESIAN_POINT('Ctrl Pts',(31.7633008075689,-1.36198038370242E-14,
27.890625));
#55114=CARTESIAN_POINT('Ctrl Pts',(31.3224756056766,0.763531646934118,27.9322916666666));
#55115=CARTESIAN_POINT('Ctrl Pts',(30.8816504037844,1.52706329386825,27.9739583333333));
#55116=CARTESIAN_POINT('Ctrl Pts',(30.,1.52706329386825,28.015625));
#55117=CARTESIAN_POINT('Ctrl Pts',(29.1183495962155,1.52706329386825,28.0572916666666));
#55118=CARTESIAN_POINT('Ctrl Pts',(28.6775243943233,0.76353164693412,28.0989583333333));
#55119=CARTESIAN_POINT('Ctrl Pts',(28.2366991924311,-1.31894491186926E-14,
28.140625));
#55120=CARTESIAN_POINT('Ctrl Pts',(28.6775243943233,-0.763531646934146,
28.1822916666666));
#55121=CARTESIAN_POINT('Ctrl Pts',(29.1183495962155,-1.52706329386828,28.2239583333333));
#55122=CARTESIAN_POINT('Ctrl Pts',(30.,-1.52706329386828,28.265625));
#55123=CARTESIAN_POINT('Ctrl Pts',(30.8816504037844,-1.52706329386828,28.3072916666666));
#55124=CARTESIAN_POINT('Ctrl Pts',(31.3224756056766,-0.763531646934147,
28.3489583333333));
#55125=CARTESIAN_POINT('Ctrl Pts',(31.7633008075689,-1.36198038370242E-14,
28.390625));
#55126=CARTESIAN_POINT('Ctrl Pts',(31.3224756056766,0.763531646934118,28.4322916666666));
#55127=CARTESIAN_POINT('Ctrl Pts',(30.8816504037844,1.52706329386825,28.4739583333333));
#55128=CARTESIAN_POINT('Ctrl Pts',(30.,1.52706329386825,28.515625));
#55129=CARTESIAN_POINT('Ctrl Pts',(29.1183495962155,1.52706329386825,28.5572916666666));
#55130=CARTESIAN_POINT('Ctrl Pts',(28.6775243943233,0.76353164693412,28.5989583333333));
#55131=CARTESIAN_POINT('Ctrl Pts',(28.2366991924311,-1.31894491186926E-14,
28.640625));
#55132=CARTESIAN_POINT('Ctrl Pts',(28.6775243943233,-0.763531646934146,
28.6822916666666));
#55133=CARTESIAN_POINT('Ctrl Pts',(29.1183495962155,-1.52706329386828,28.7239583333333));
#55134=CARTESIAN_POINT('Ctrl Pts',(30.,-1.52706329386828,28.765625));
#55135=CARTESIAN_POINT('Ctrl Pts',(30.8816504037844,-1.52706329386828,28.8072916666666));
#55136=CARTESIAN_POINT('Ctrl Pts',(31.3224756056766,-0.763531646934147,
28.8489583333333));
#55137=CARTESIAN_POINT('Ctrl Pts',(31.7633008075689,-1.36198038370242E-14,
28.890625));
#55138=CARTESIAN_POINT('Ctrl Pts',(31.3224756056766,0.763531646934118,28.9322916666666));
#55139=CARTESIAN_POINT('Ctrl Pts',(30.8816504037844,1.52706329386825,28.9739583333333));
#55140=CARTESIAN_POINT('Ctrl Pts',(30.,1.52706329386825,29.015625));
#55141=CARTESIAN_POINT('Ctrl Pts',(29.1183495962155,1.52706329386825,29.0572916666666));
#55142=CARTESIAN_POINT('Ctrl Pts',(28.6775243943233,0.76353164693412,29.0989583333333));
#55143=CARTESIAN_POINT('Ctrl Pts',(28.2366991924311,-1.31894491186926E-14,
29.140625));
#55144=CARTESIAN_POINT('Ctrl Pts',(28.6775243943233,-0.763531646934146,
29.1822916666666));
#55145=CARTESIAN_POINT('Ctrl Pts',(29.1183495962155,-1.52706329386828,29.2239583333333));
#55146=CARTESIAN_POINT('Ctrl Pts',(30.,-1.52706329386828,29.265625));
#55147=CARTESIAN_POINT('Ctrl Pts',(30.8816504037844,-1.52706329386828,29.3072916666666));
#55148=CARTESIAN_POINT('Ctrl Pts',(31.3224756056766,-0.763531646934147,
29.3489583333333));
#55149=CARTESIAN_POINT('Ctrl Pts',(31.7633008075689,-1.36198038370242E-14,
29.390625));
#55150=CARTESIAN_POINT('Ctrl Pts',(31.3224756056766,0.763531646934118,29.4322916666666));
#55151=CARTESIAN_POINT('Ctrl Pts',(30.8816504037844,1.52706329386825,29.4739583333333));
#55152=CARTESIAN_POINT('Ctrl Pts',(30.,1.52706329386825,29.515625));
#55153=CARTESIAN_POINT('Ctrl Pts',(29.1183495962155,1.52706329386825,29.5572916666666));
#55154=CARTESIAN_POINT('Ctrl Pts',(28.6775243943233,0.76353164693412,29.5989583333333));
#55155=CARTESIAN_POINT('Ctrl Pts',(28.2366991924311,-1.31894491186926E-14,
29.640625));
#55156=CARTESIAN_POINT('Ctrl Pts',(28.6775243943233,-0.763531646934146,
29.6822916666666));
#55157=CARTESIAN_POINT('Ctrl Pts',(29.1183495962155,-1.52706329386828,29.7239583333333));
#55158=CARTESIAN_POINT('Ctrl Pts',(30.,-1.52706329386828,29.765625));
#55159=CARTESIAN_POINT('Ctrl Pts',(30.8816504037844,-1.52706329386828,29.8072916666666));
#55160=CARTESIAN_POINT('Ctrl Pts',(31.3224756056766,-0.763531646934147,
29.8489583333333));
#55161=CARTESIAN_POINT('Ctrl Pts',(31.7633008075689,-1.36198038370242E-14,
29.890625));
#55162=CARTESIAN_POINT('Ctrl Pts',(31.3224756056766,0.763531646934118,29.9322916666666));
#55163=CARTESIAN_POINT('Ctrl Pts',(30.8816504037844,1.52706329386825,29.9739583333333));
#55164=CARTESIAN_POINT('Ctrl Pts',(30.,1.52706329386825,30.015625));
#55165=CARTESIAN_POINT('Ctrl Pts',(29.1183495962155,1.52706329386825,30.0572916666666));
#55166=CARTESIAN_POINT('Ctrl Pts',(28.6775243943233,0.76353164693412,30.0989583333333));
#55167=CARTESIAN_POINT('Ctrl Pts',(28.2366991924311,-1.31894491186926E-14,
30.140625));
#55168=CARTESIAN_POINT('Ctrl Pts',(28.6775243943233,-0.763531646934146,
30.1822916666666));
#55169=CARTESIAN_POINT('Ctrl Pts',(29.1183495962155,-1.52706329386828,30.2239583333333));
#55170=CARTESIAN_POINT('Ctrl Pts',(30.,-1.52706329386828,30.265625));
#55171=CARTESIAN_POINT('Ctrl Pts',(30.8816504037844,-1.52706329386828,30.3072916666666));
#55172=CARTESIAN_POINT('Ctrl Pts',(31.3224756056766,-0.763531646934147,
30.3489583333333));
#55173=CARTESIAN_POINT('Ctrl Pts',(31.7633008075689,-1.36198038370242E-14,
30.390625));
#55174=CARTESIAN_POINT('Ctrl Pts',(31.3224756056766,0.763531646934118,30.4322916666666));
#55175=CARTESIAN_POINT('Ctrl Pts',(30.8816504037844,1.52706329386825,30.4739583333333));
#55176=CARTESIAN_POINT('Ctrl Pts',(30.,1.52706329386825,30.515625));
#55177=CARTESIAN_POINT('Ctrl Pts',(29.1183495962155,1.52706329386825,30.5572916666666));
#55178=CARTESIAN_POINT('Ctrl Pts',(28.6775243943233,0.76353164693412,30.5989583333333));
#55179=CARTESIAN_POINT('Ctrl Pts',(28.2366991924311,-1.31894491186926E-14,
30.640625));
#55180=CARTESIAN_POINT('Ctrl Pts',(28.6775243943233,-0.763531646934146,
30.6822916666666));
#55181=CARTESIAN_POINT('Ctrl Pts',(29.1183495962155,-1.52706329386828,30.7239583333333));
#55182=CARTESIAN_POINT('Ctrl Pts',(30.,-1.52706329386828,30.765625));
#55183=CARTESIAN_POINT('Ctrl Pts',(30.8816504037844,-1.52706329386828,30.8072916666666));
#55184=CARTESIAN_POINT('Ctrl Pts',(31.3224756056766,-0.763531646934147,
30.8489583333333));
#55185=CARTESIAN_POINT('Ctrl Pts',(31.7633008075689,-1.36198038370242E-14,
30.890625));
#55186=CARTESIAN_POINT('Ctrl Pts',(31.3224756056766,0.763531646934118,30.9322916666666));
#55187=CARTESIAN_POINT('Ctrl Pts',(30.8816504037844,1.52706329386825,30.9739583333333));
#55188=CARTESIAN_POINT('Ctrl Pts',(30.,1.52706329386825,31.015625));
#55189=CARTESIAN_POINT('Ctrl Pts',(29.1183495962155,1.52706329386825,31.0572916666666));
#55190=CARTESIAN_POINT('Ctrl Pts',(28.6775243943233,0.76353164693412,31.0989583333333));
#55191=CARTESIAN_POINT('Ctrl Pts',(28.2366991924311,-1.31894491186926E-14,
31.140625));
#55192=CARTESIAN_POINT('Ctrl Pts',(28.6775243943233,-0.763531646934146,
31.1822916666666));
#55193=CARTESIAN_POINT('Ctrl Pts',(29.1183495962155,-1.52706329386828,31.2239583333333));
#55194=CARTESIAN_POINT('Ctrl Pts',(30.,-1.52706329386828,31.265625));
#55195=CARTESIAN_POINT('Ctrl Pts',(30.8816504037844,-1.52706329386828,31.3072916666666));
#55196=CARTESIAN_POINT('Ctrl Pts',(31.3224756056766,-0.763531646934147,
31.3489583333333));
#55197=CARTESIAN_POINT('Ctrl Pts',(31.7633008075689,-1.36198038370242E-14,
31.390625));
#55198=CARTESIAN_POINT('Ctrl Pts',(31.3224756056766,0.763531646934118,31.4322916666666));
#55199=CARTESIAN_POINT('Ctrl Pts',(30.8816504037844,1.52706329386825,31.4739583333333));
#55200=CARTESIAN_POINT('Ctrl Pts',(30.,1.52706329386825,31.515625));
#55201=CARTESIAN_POINT('Ctrl Pts',(30.,1.17523507120987,15.8124968809397));
#55202=CARTESIAN_POINT('Ctrl Pts',(29.3214777152758,1.17523507120987,15.8541635476064));
#55203=CARTESIAN_POINT('Ctrl Pts',(28.9822165729138,0.587617535604928,15.895830214273));
#55204=CARTESIAN_POINT('Ctrl Pts',(28.6429554305518,-1.32141489532166E-14,
15.9374968809397));
#55205=CARTESIAN_POINT('Ctrl Pts',(28.9822165729138,-0.587617535604954,
15.9791635476064));
#55206=CARTESIAN_POINT('Ctrl Pts',(29.3214777152758,-1.17523507120989,16.020830214273));
#55207=CARTESIAN_POINT('Ctrl Pts',(30.,-1.17523507120989,16.0624968809397));
#55208=CARTESIAN_POINT('Ctrl Pts',(30.6785222847241,-1.17523507120989,16.1041635476064));
#55209=CARTESIAN_POINT('Ctrl Pts',(31.0177834270861,-0.587617535604955,
16.145830214273));
#55210=CARTESIAN_POINT('Ctrl Pts',(31.3570445694482,-1.35453519623354E-14,
16.1874968809397));
#55211=CARTESIAN_POINT('Ctrl Pts',(31.0177834270861,0.587617535604927,16.2291635476064));
#55212=CARTESIAN_POINT('Ctrl Pts',(30.6785222847241,1.17523507120987,16.270830214273));
#55213=CARTESIAN_POINT('Ctrl Pts',(30.,1.17523507120987,16.3124968809397));
#55214=CARTESIAN_POINT('Ctrl Pts',(29.3214777152758,1.17523507120987,16.3541635476064));
#55215=CARTESIAN_POINT('Ctrl Pts',(28.9822165729138,0.587617535604928,16.395830214273));
#55216=CARTESIAN_POINT('Ctrl Pts',(28.6429554305518,-1.32141489532166E-14,
16.4374968809397));
#55217=CARTESIAN_POINT('Ctrl Pts',(28.9822165729138,-0.587617535604954,
16.4791635476064));
#55218=CARTESIAN_POINT('Ctrl Pts',(29.3214777152758,-1.17523507120989,16.520830214273));
#55219=CARTESIAN_POINT('Ctrl Pts',(30.,-1.17523507120989,16.5624968809397));
#55220=CARTESIAN_POINT('Ctrl Pts',(30.6785222847241,-1.17523507120989,16.6041635476064));
#55221=CARTESIAN_POINT('Ctrl Pts',(31.0177834270861,-0.587617535604955,
16.645830214273));
#55222=CARTESIAN_POINT('Ctrl Pts',(31.3570445694482,-1.35453519623354E-14,
16.6874968809397));
#55223=CARTESIAN_POINT('Ctrl Pts',(31.0177834270861,0.587617535604927,16.7291635476064));
#55224=CARTESIAN_POINT('Ctrl Pts',(30.6785222847241,1.17523507120987,16.770830214273));
#55225=CARTESIAN_POINT('Ctrl Pts',(30.,1.17523507120987,16.8124968809397));
#55226=CARTESIAN_POINT('Ctrl Pts',(29.3214777152758,1.17523507120987,16.8541635476064));
#55227=CARTESIAN_POINT('Ctrl Pts',(28.9822165729138,0.587617535604928,16.895830214273));
#55228=CARTESIAN_POINT('Ctrl Pts',(28.6429554305518,-1.32141489532166E-14,
16.9374968809397));
#55229=CARTESIAN_POINT('Ctrl Pts',(28.9822165729138,-0.587617535604954,
16.9791635476064));
#55230=CARTESIAN_POINT('Ctrl Pts',(29.3214777152758,-1.17523507120989,17.020830214273));
#55231=CARTESIAN_POINT('Ctrl Pts',(30.,-1.17523507120989,17.0624968809397));
#55232=CARTESIAN_POINT('Ctrl Pts',(30.6785222847241,-1.17523507120989,17.1041635476064));
#55233=CARTESIAN_POINT('Ctrl Pts',(31.0177834270861,-0.587617535604955,
17.145830214273));
#55234=CARTESIAN_POINT('Ctrl Pts',(31.3570445694482,-1.35453519623354E-14,
17.1874968809397));
#55235=CARTESIAN_POINT('Ctrl Pts',(31.0177834270861,0.587617535604927,17.2291635476064));
#55236=CARTESIAN_POINT('Ctrl Pts',(30.6785222847241,1.17523507120987,17.270830214273));
#55237=CARTESIAN_POINT('Ctrl Pts',(30.,1.17523507120987,17.3124968809397));
#55238=CARTESIAN_POINT('Ctrl Pts',(29.3214777152758,1.17523507120987,17.3541635476064));
#55239=CARTESIAN_POINT('Ctrl Pts',(28.9822165729138,0.587617535604928,17.395830214273));
#55240=CARTESIAN_POINT('Ctrl Pts',(28.6429554305518,-1.32141489532166E-14,
17.4374968809397));
#55241=CARTESIAN_POINT('Ctrl Pts',(28.9822165729138,-0.587617535604954,
17.4791635476064));
#55242=CARTESIAN_POINT('Ctrl Pts',(29.3214777152758,-1.17523507120989,17.520830214273));
#55243=CARTESIAN_POINT('Ctrl Pts',(30.,-1.17523507120989,17.5624968809397));
#55244=CARTESIAN_POINT('Ctrl Pts',(30.6785222847241,-1.17523507120989,17.6041635476064));
#55245=CARTESIAN_POINT('Ctrl Pts',(31.0177834270861,-0.587617535604955,
17.645830214273));
#55246=CARTESIAN_POINT('Ctrl Pts',(31.3570445694482,-1.35453519623354E-14,
17.6874968809397));
#55247=CARTESIAN_POINT('Ctrl Pts',(31.0177834270861,0.587617535604927,17.7291635476064));
#55248=CARTESIAN_POINT('Ctrl Pts',(30.6785222847241,1.17523507120987,17.770830214273));
#55249=CARTESIAN_POINT('Ctrl Pts',(30.,1.17523507120987,17.8124968809397));
#55250=CARTESIAN_POINT('Ctrl Pts',(29.3214777152758,1.17523507120987,17.8541635476064));
#55251=CARTESIAN_POINT('Ctrl Pts',(28.9822165729138,0.587617535604928,17.895830214273));
#55252=CARTESIAN_POINT('Ctrl Pts',(28.6429554305518,-1.32141489532166E-14,
17.9374968809397));
#55253=CARTESIAN_POINT('Ctrl Pts',(28.9822165729138,-0.587617535604954,
17.9791635476064));
#55254=CARTESIAN_POINT('Ctrl Pts',(29.3214777152758,-1.17523507120989,18.020830214273));
#55255=CARTESIAN_POINT('Ctrl Pts',(30.,-1.17523507120989,18.0624968809397));
#55256=CARTESIAN_POINT('Ctrl Pts',(30.6785222847241,-1.17523507120989,18.1041635476064));
#55257=CARTESIAN_POINT('Ctrl Pts',(31.0177834270861,-0.587617535604955,
18.145830214273));
#55258=CARTESIAN_POINT('Ctrl Pts',(31.3570445694482,-1.35453519623354E-14,
18.1874968809397));
#55259=CARTESIAN_POINT('Ctrl Pts',(31.0177834270861,0.587617535604927,18.2291635476064));
#55260=CARTESIAN_POINT('Ctrl Pts',(30.6785222847241,1.17523507120987,18.270830214273));
#55261=CARTESIAN_POINT('Ctrl Pts',(30.,1.17523507120987,18.3124968809397));
#55262=CARTESIAN_POINT('Ctrl Pts',(29.3214777152758,1.17523507120987,18.3541635476064));
#55263=CARTESIAN_POINT('Ctrl Pts',(28.9822165729138,0.587617535604928,18.395830214273));
#55264=CARTESIAN_POINT('Ctrl Pts',(28.6429554305518,-1.32141489532166E-14,
18.4374968809397));
#55265=CARTESIAN_POINT('Ctrl Pts',(28.9822165729138,-0.587617535604954,
18.4791635476064));
#55266=CARTESIAN_POINT('Ctrl Pts',(29.3214777152758,-1.17523507120989,18.520830214273));
#55267=CARTESIAN_POINT('Ctrl Pts',(30.,-1.17523507120989,18.5624968809397));
#55268=CARTESIAN_POINT('Ctrl Pts',(30.6785222847241,-1.17523507120989,18.6041635476064));
#55269=CARTESIAN_POINT('Ctrl Pts',(31.0177834270861,-0.587617535604955,
18.645830214273));
#55270=CARTESIAN_POINT('Ctrl Pts',(31.3570445694482,-1.35453519623354E-14,
18.6874968809397));
#55271=CARTESIAN_POINT('Ctrl Pts',(31.0177834270861,0.587617535604927,18.7291635476064));
#55272=CARTESIAN_POINT('Ctrl Pts',(30.6785222847241,1.17523507120987,18.770830214273));
#55273=CARTESIAN_POINT('Ctrl Pts',(30.,1.17523507120987,18.8124968809397));
#55274=CARTESIAN_POINT('Ctrl Pts',(29.3214777152758,1.17523507120987,18.8541635476064));
#55275=CARTESIAN_POINT('Ctrl Pts',(28.9822165729138,0.587617535604928,18.895830214273));
#55276=CARTESIAN_POINT('Ctrl Pts',(28.6429554305518,-1.32141489532166E-14,
18.9374968809397));
#55277=CARTESIAN_POINT('Ctrl Pts',(28.9822165729138,-0.587617535604954,
18.9791635476064));
#55278=CARTESIAN_POINT('Ctrl Pts',(29.3214777152758,-1.17523507120989,19.020830214273));
#55279=CARTESIAN_POINT('Ctrl Pts',(30.,-1.17523507120989,19.0624968809397));
#55280=CARTESIAN_POINT('Ctrl Pts',(30.6785222847241,-1.17523507120989,19.1041635476064));
#55281=CARTESIAN_POINT('Ctrl Pts',(31.0177834270861,-0.587617535604955,
19.145830214273));
#55282=CARTESIAN_POINT('Ctrl Pts',(31.3570445694482,-1.35453519623354E-14,
19.1874968809397));
#55283=CARTESIAN_POINT('Ctrl Pts',(31.0177834270861,0.587617535604927,19.2291635476064));
#55284=CARTESIAN_POINT('Ctrl Pts',(30.6785222847241,1.17523507120987,19.270830214273));
#55285=CARTESIAN_POINT('Ctrl Pts',(30.,1.17523507120987,19.3124968809397));
#55286=CARTESIAN_POINT('Ctrl Pts',(29.3214777152758,1.17523507120987,19.3541635476064));
#55287=CARTESIAN_POINT('Ctrl Pts',(28.9822165729138,0.587617535604928,19.395830214273));
#55288=CARTESIAN_POINT('Ctrl Pts',(28.6429554305518,-1.32141489532166E-14,
19.4374968809397));
#55289=CARTESIAN_POINT('Ctrl Pts',(28.9822165729138,-0.587617535604954,
19.4791635476064));
#55290=CARTESIAN_POINT('Ctrl Pts',(29.3214777152758,-1.17523507120989,19.520830214273));
#55291=CARTESIAN_POINT('Ctrl Pts',(30.,-1.17523507120989,19.5624968809397));
#55292=CARTESIAN_POINT('Ctrl Pts',(30.6785222847241,-1.17523507120989,19.6041635476064));
#55293=CARTESIAN_POINT('Ctrl Pts',(31.0177834270861,-0.587617535604955,
19.645830214273));
#55294=CARTESIAN_POINT('Ctrl Pts',(31.3570445694482,-1.35453519623354E-14,
19.6874968809397));
#55295=CARTESIAN_POINT('Ctrl Pts',(31.0177834270861,0.587617535604927,19.7291635476064));
#55296=CARTESIAN_POINT('Ctrl Pts',(30.6785222847241,1.17523507120987,19.770830214273));
#55297=CARTESIAN_POINT('Ctrl Pts',(30.,1.17523507120987,19.8124968809397));
#55298=CARTESIAN_POINT('Ctrl Pts',(29.3214777152758,1.17523507120987,19.8541635476064));
#55299=CARTESIAN_POINT('Ctrl Pts',(28.9822165729138,0.587617535604928,19.895830214273));
#55300=CARTESIAN_POINT('Ctrl Pts',(28.6429554305518,-1.32141489532166E-14,
19.9374968809397));
#55301=CARTESIAN_POINT('Ctrl Pts',(28.9822165729138,-0.587617535604954,
19.9791635476064));
#55302=CARTESIAN_POINT('Ctrl Pts',(29.3214777152758,-1.17523507120989,20.020830214273));
#55303=CARTESIAN_POINT('Ctrl Pts',(30.,-1.17523507120989,20.0624968809397));
#55304=CARTESIAN_POINT('Ctrl Pts',(30.6785222847241,-1.17523507120989,20.1041635476064));
#55305=CARTESIAN_POINT('Ctrl Pts',(31.0177834270861,-0.587617535604955,
20.145830214273));
#55306=CARTESIAN_POINT('Ctrl Pts',(31.3570445694482,-1.35453519623354E-14,
20.1874968809397));
#55307=CARTESIAN_POINT('Ctrl Pts',(31.0177834270861,0.587617535604927,20.2291635476064));
#55308=CARTESIAN_POINT('Ctrl Pts',(30.6785222847241,1.17523507120987,20.270830214273));
#55309=CARTESIAN_POINT('Ctrl Pts',(30.,1.17523507120987,20.3124968809397));
#55310=CARTESIAN_POINT('Ctrl Pts',(29.3214777152758,1.17523507120987,20.3541635476064));
#55311=CARTESIAN_POINT('Ctrl Pts',(28.9822165729138,0.587617535604928,20.395830214273));
#55312=CARTESIAN_POINT('Ctrl Pts',(28.6429554305518,-1.32141489532166E-14,
20.4374968809397));
#55313=CARTESIAN_POINT('Ctrl Pts',(28.9822165729138,-0.587617535604954,
20.4791635476064));
#55314=CARTESIAN_POINT('Ctrl Pts',(29.3214777152758,-1.17523507120989,20.520830214273));
#55315=CARTESIAN_POINT('Ctrl Pts',(30.,-1.17523507120989,20.5624968809397));
#55316=CARTESIAN_POINT('Ctrl Pts',(30.6785222847241,-1.17523507120989,20.6041635476064));
#55317=CARTESIAN_POINT('Ctrl Pts',(31.0177834270861,-0.587617535604955,
20.645830214273));
#55318=CARTESIAN_POINT('Ctrl Pts',(31.3570445694482,-1.35453519623354E-14,
20.6874968809397));
#55319=CARTESIAN_POINT('Ctrl Pts',(31.0177834270861,0.587617535604927,20.7291635476064));
#55320=CARTESIAN_POINT('Ctrl Pts',(30.6785222847241,1.17523507120987,20.770830214273));
#55321=CARTESIAN_POINT('Ctrl Pts',(30.,1.17523507120987,20.8124968809397));
#55322=CARTESIAN_POINT('Ctrl Pts',(29.3214777152758,1.17523507120987,20.8541635476064));
#55323=CARTESIAN_POINT('Ctrl Pts',(28.9822165729138,0.587617535604928,20.895830214273));
#55324=CARTESIAN_POINT('Ctrl Pts',(28.6429554305518,-1.32141489532166E-14,
20.9374968809397));
#55325=CARTESIAN_POINT('Ctrl Pts',(28.9822165729138,-0.587617535604954,
20.9791635476064));
#55326=CARTESIAN_POINT('Ctrl Pts',(29.3214777152758,-1.17523507120989,21.020830214273));
#55327=CARTESIAN_POINT('Ctrl Pts',(30.,-1.17523507120989,21.0624968809397));
#55328=CARTESIAN_POINT('Ctrl Pts',(30.6785222847241,-1.17523507120989,21.1041635476064));
#55329=CARTESIAN_POINT('Ctrl Pts',(31.0177834270861,-0.587617535604955,
21.145830214273));
#55330=CARTESIAN_POINT('Ctrl Pts',(31.3570445694482,-1.35453519623354E-14,
21.1874968809397));
#55331=CARTESIAN_POINT('Ctrl Pts',(31.0177834270861,0.587617535604927,21.2291635476064));
#55332=CARTESIAN_POINT('Ctrl Pts',(30.6785222847241,1.17523507120987,21.270830214273));
#55333=CARTESIAN_POINT('Ctrl Pts',(30.,1.17523507120987,21.3124968809397));
#55334=CARTESIAN_POINT('Ctrl Pts',(29.3214777152758,1.17523507120987,21.3541635476064));
#55335=CARTESIAN_POINT('Ctrl Pts',(28.9822165729138,0.587617535604928,21.395830214273));
#55336=CARTESIAN_POINT('Ctrl Pts',(28.6429554305518,-1.32141489532166E-14,
21.4374968809397));
#55337=CARTESIAN_POINT('Ctrl Pts',(28.9822165729138,-0.587617535604954,
21.4791635476064));
#55338=CARTESIAN_POINT('Ctrl Pts',(29.3214777152758,-1.17523507120989,21.520830214273));
#55339=CARTESIAN_POINT('Ctrl Pts',(30.,-1.17523507120989,21.5624968809397));
#55340=CARTESIAN_POINT('Ctrl Pts',(30.6785222847241,-1.17523507120989,21.6041635476064));
#55341=CARTESIAN_POINT('Ctrl Pts',(31.0177834270861,-0.587617535604955,
21.645830214273));
#55342=CARTESIAN_POINT('Ctrl Pts',(31.3570445694482,-1.35453519623354E-14,
21.6874968809397));
#55343=CARTESIAN_POINT('Ctrl Pts',(31.0177834270861,0.587617535604927,21.7291635476064));
#55344=CARTESIAN_POINT('Ctrl Pts',(30.6785222847241,1.17523507120987,21.770830214273));
#55345=CARTESIAN_POINT('Ctrl Pts',(30.,1.17523507120987,21.8124968809397));
#55346=CARTESIAN_POINT('Ctrl Pts',(29.3214777152758,1.17523507120987,21.8541635476064));
#55347=CARTESIAN_POINT('Ctrl Pts',(28.9822165729138,0.587617535604928,21.895830214273));
#55348=CARTESIAN_POINT('Ctrl Pts',(28.6429554305518,-1.32141489532166E-14,
21.9374968809397));
#55349=CARTESIAN_POINT('Ctrl Pts',(28.9822165729138,-0.587617535604954,
21.9791635476064));
#55350=CARTESIAN_POINT('Ctrl Pts',(29.3214777152758,-1.17523507120989,22.020830214273));
#55351=CARTESIAN_POINT('Ctrl Pts',(30.,-1.17523507120989,22.0624968809397));
#55352=CARTESIAN_POINT('Ctrl Pts',(30.6785222847241,-1.17523507120989,22.1041635476064));
#55353=CARTESIAN_POINT('Ctrl Pts',(31.0177834270861,-0.587617535604955,
22.145830214273));
#55354=CARTESIAN_POINT('Ctrl Pts',(31.3570445694482,-1.35453519623354E-14,
22.1874968809397));
#55355=CARTESIAN_POINT('Ctrl Pts',(31.0177834270861,0.587617535604927,22.2291635476064));
#55356=CARTESIAN_POINT('Ctrl Pts',(30.6785222847241,1.17523507120987,22.270830214273));
#55357=CARTESIAN_POINT('Ctrl Pts',(30.,1.17523507120987,22.3124968809397));
#55358=CARTESIAN_POINT('Ctrl Pts',(29.3214777152758,1.17523507120987,22.3541635476064));
#55359=CARTESIAN_POINT('Ctrl Pts',(28.9822165729138,0.587617535604928,22.395830214273));
#55360=CARTESIAN_POINT('Ctrl Pts',(28.6429554305518,-1.32141489532166E-14,
22.4374968809397));
#55361=CARTESIAN_POINT('Ctrl Pts',(28.9822165729138,-0.587617535604954,
22.4791635476064));
#55362=CARTESIAN_POINT('Ctrl Pts',(29.3214777152758,-1.17523507120989,22.520830214273));
#55363=CARTESIAN_POINT('Ctrl Pts',(30.,-1.17523507120989,22.5624968809397));
#55364=CARTESIAN_POINT('Ctrl Pts',(30.6785222847241,-1.17523507120989,22.6041635476064));
#55365=CARTESIAN_POINT('Ctrl Pts',(31.0177834270861,-0.587617535604955,
22.645830214273));
#55366=CARTESIAN_POINT('Ctrl Pts',(31.3570445694482,-1.35453519623354E-14,
22.6874968809397));
#55367=CARTESIAN_POINT('Ctrl Pts',(31.0177834270861,0.587617535604927,22.7291635476064));
#55368=CARTESIAN_POINT('Ctrl Pts',(30.6785222847241,1.17523507120987,22.770830214273));
#55369=CARTESIAN_POINT('Ctrl Pts',(30.,1.17523507120987,22.8124968809397));
#55370=CARTESIAN_POINT('Ctrl Pts',(29.3214777152758,1.17523507120987,22.8541635476064));
#55371=CARTESIAN_POINT('Ctrl Pts',(28.9822165729138,0.587617535604928,22.895830214273));
#55372=CARTESIAN_POINT('Ctrl Pts',(28.6429554305518,-1.32141489532166E-14,
22.9374968809397));
#55373=CARTESIAN_POINT('Ctrl Pts',(28.9822165729138,-0.587617535604954,
22.9791635476064));
#55374=CARTESIAN_POINT('Ctrl Pts',(29.3214777152758,-1.17523507120989,23.020830214273));
#55375=CARTESIAN_POINT('Ctrl Pts',(30.,-1.17523507120989,23.0624968809397));
#55376=CARTESIAN_POINT('Ctrl Pts',(30.6785222847241,-1.17523507120989,23.1041635476064));
#55377=CARTESIAN_POINT('Ctrl Pts',(31.0177834270861,-0.587617535604955,
23.145830214273));
#55378=CARTESIAN_POINT('Ctrl Pts',(31.3570445694482,-1.35453519623354E-14,
23.1874968809397));
#55379=CARTESIAN_POINT('Ctrl Pts',(31.0177834270861,0.587617535604927,23.2291635476064));
#55380=CARTESIAN_POINT('Ctrl Pts',(30.6785222847241,1.17523507120987,23.270830214273));
#55381=CARTESIAN_POINT('Ctrl Pts',(30.,1.17523507120987,23.3124968809397));
#55382=CARTESIAN_POINT('Ctrl Pts',(29.3214777152758,1.17523507120987,23.3541635476064));
#55383=CARTESIAN_POINT('Ctrl Pts',(28.9822165729138,0.587617535604928,23.395830214273));
#55384=CARTESIAN_POINT('Ctrl Pts',(28.6429554305518,-1.32141489532166E-14,
23.4374968809397));
#55385=CARTESIAN_POINT('Ctrl Pts',(28.9822165729138,-0.587617535604954,
23.4791635476064));
#55386=CARTESIAN_POINT('Ctrl Pts',(29.3214777152758,-1.17523507120989,23.520830214273));
#55387=CARTESIAN_POINT('Ctrl Pts',(30.,-1.17523507120989,23.5624968809397));
#55388=CARTESIAN_POINT('Ctrl Pts',(30.6785222847241,-1.17523507120989,23.6041635476064));
#55389=CARTESIAN_POINT('Ctrl Pts',(31.0177834270861,-0.587617535604955,
23.645830214273));
#55390=CARTESIAN_POINT('Ctrl Pts',(31.3570445694482,-1.35453519623354E-14,
23.6874968809397));
#55391=CARTESIAN_POINT('Ctrl Pts',(31.0177834270861,0.587617535604927,23.7291635476064));
#55392=CARTESIAN_POINT('Ctrl Pts',(30.6785222847241,1.17523507120987,23.770830214273));
#55393=CARTESIAN_POINT('Ctrl Pts',(30.,1.17523507120987,23.8124968809397));
#55394=CARTESIAN_POINT('Ctrl Pts',(29.3214777152758,1.17523507120987,23.8541635476064));
#55395=CARTESIAN_POINT('Ctrl Pts',(28.9822165729138,0.587617535604928,23.895830214273));
#55396=CARTESIAN_POINT('Ctrl Pts',(28.6429554305518,-1.32141489532166E-14,
23.9374968809397));
#55397=CARTESIAN_POINT('Ctrl Pts',(28.9822165729138,-0.587617535604954,
23.9791635476064));
#55398=CARTESIAN_POINT('Ctrl Pts',(29.3214777152758,-1.17523507120989,24.020830214273));
#55399=CARTESIAN_POINT('Ctrl Pts',(30.,-1.17523507120989,24.0624968809397));
#55400=CARTESIAN_POINT('Ctrl Pts',(30.6785222847241,-1.17523507120989,24.1041635476064));
#55401=CARTESIAN_POINT('Ctrl Pts',(31.0177834270861,-0.587617535604955,
24.145830214273));
#55402=CARTESIAN_POINT('Ctrl Pts',(31.3570445694482,-1.35453519623354E-14,
24.1874968809397));
#55403=CARTESIAN_POINT('Ctrl Pts',(31.0177834270861,0.587617535604927,24.2291635476064));
#55404=CARTESIAN_POINT('Ctrl Pts',(30.6785222847241,1.17523507120987,24.270830214273));
#55405=CARTESIAN_POINT('Ctrl Pts',(30.,1.17523507120987,24.3124968809397));
#55406=CARTESIAN_POINT('Ctrl Pts',(29.3214777152758,1.17523507120987,24.3541635476064));
#55407=CARTESIAN_POINT('Ctrl Pts',(28.9822165729138,0.587617535604928,24.395830214273));
#55408=CARTESIAN_POINT('Ctrl Pts',(28.6429554305518,-1.32141489532166E-14,
24.4374968809397));
#55409=CARTESIAN_POINT('Ctrl Pts',(28.9822165729138,-0.587617535604954,
24.4791635476064));
#55410=CARTESIAN_POINT('Ctrl Pts',(29.3214777152758,-1.17523507120989,24.520830214273));
#55411=CARTESIAN_POINT('Ctrl Pts',(30.,-1.17523507120989,24.5624968809397));
#55412=CARTESIAN_POINT('Ctrl Pts',(30.6785222847241,-1.17523507120989,24.6041635476064));
#55413=CARTESIAN_POINT('Ctrl Pts',(31.0177834270861,-0.587617535604955,
24.645830214273));
#55414=CARTESIAN_POINT('Ctrl Pts',(31.3570445694482,-1.35453519623354E-14,
24.6874968809397));
#55415=CARTESIAN_POINT('Ctrl Pts',(31.0177834270861,0.587617535604927,24.7291635476064));
#55416=CARTESIAN_POINT('Ctrl Pts',(30.6785222847241,1.17523507120987,24.770830214273));
#55417=CARTESIAN_POINT('Ctrl Pts',(30.,1.17523507120987,24.8124968809397));
#55418=CARTESIAN_POINT('Ctrl Pts',(29.3214777152758,1.17523507120987,24.8541635476064));
#55419=CARTESIAN_POINT('Ctrl Pts',(28.9822165729138,0.587617535604928,24.895830214273));
#55420=CARTESIAN_POINT('Ctrl Pts',(28.6429554305518,-1.32141489532166E-14,
24.9374968809397));
#55421=CARTESIAN_POINT('Ctrl Pts',(28.9822165729138,-0.587617535604954,
24.9791635476064));
#55422=CARTESIAN_POINT('Ctrl Pts',(29.3214777152758,-1.17523507120989,25.020830214273));
#55423=CARTESIAN_POINT('Ctrl Pts',(30.,-1.17523507120989,25.0624968809397));
#55424=CARTESIAN_POINT('Ctrl Pts',(30.6785222847241,-1.17523507120989,25.1041635476064));
#55425=CARTESIAN_POINT('Ctrl Pts',(31.0177834270861,-0.587617535604955,
25.145830214273));
#55426=CARTESIAN_POINT('Ctrl Pts',(31.3570445694482,-1.35453519623354E-14,
25.1874968809397));
#55427=CARTESIAN_POINT('Ctrl Pts',(31.0177834270861,0.587617535604927,25.2291635476064));
#55428=CARTESIAN_POINT('Ctrl Pts',(30.6785222847241,1.17523507120987,25.270830214273));
#55429=CARTESIAN_POINT('Ctrl Pts',(30.,1.17523507120987,25.3124968809397));
#55430=CARTESIAN_POINT('Ctrl Pts',(29.3214777152758,1.17523507120987,25.3541635476064));
#55431=CARTESIAN_POINT('Ctrl Pts',(28.9822165729138,0.587617535604928,25.395830214273));
#55432=CARTESIAN_POINT('Ctrl Pts',(28.6429554305518,-1.32141489532166E-14,
25.4374968809397));
#55433=CARTESIAN_POINT('Ctrl Pts',(28.9822165729138,-0.587617535604954,
25.4791635476064));
#55434=CARTESIAN_POINT('Ctrl Pts',(29.3214777152758,-1.17523507120989,25.520830214273));
#55435=CARTESIAN_POINT('Ctrl Pts',(30.,-1.17523507120989,25.5624968809397));
#55436=CARTESIAN_POINT('Ctrl Pts',(30.6785222847241,-1.17523507120989,25.6041635476064));
#55437=CARTESIAN_POINT('Ctrl Pts',(31.0177834270861,-0.587617535604955,
25.645830214273));
#55438=CARTESIAN_POINT('Ctrl Pts',(31.3570445694482,-1.35453519623354E-14,
25.6874968809397));
#55439=CARTESIAN_POINT('Ctrl Pts',(31.0177834270861,0.587617535604927,25.7291635476064));
#55440=CARTESIAN_POINT('Ctrl Pts',(30.6785222847241,1.17523507120987,25.770830214273));
#55441=CARTESIAN_POINT('Ctrl Pts',(30.,1.17523507120987,25.8124968809397));
#55442=CARTESIAN_POINT('Ctrl Pts',(29.3214777152758,1.17523507120987,25.8541635476064));
#55443=CARTESIAN_POINT('Ctrl Pts',(28.9822165729138,0.587617535604928,25.895830214273));
#55444=CARTESIAN_POINT('Ctrl Pts',(28.6429554305518,-1.32141489532166E-14,
25.9374968809397));
#55445=CARTESIAN_POINT('Ctrl Pts',(28.9822165729138,-0.587617535604954,
25.9791635476064));
#55446=CARTESIAN_POINT('Ctrl Pts',(29.3214777152758,-1.17523507120989,26.020830214273));
#55447=CARTESIAN_POINT('Ctrl Pts',(30.,-1.17523507120989,26.0624968809397));
#55448=CARTESIAN_POINT('Ctrl Pts',(30.6785222847241,-1.17523507120989,26.1041635476064));
#55449=CARTESIAN_POINT('Ctrl Pts',(31.0177834270861,-0.587617535604955,
26.145830214273));
#55450=CARTESIAN_POINT('Ctrl Pts',(31.3570445694482,-1.35453519623354E-14,
26.1874968809397));
#55451=CARTESIAN_POINT('Ctrl Pts',(31.0177834270861,0.587617535604927,26.2291635476064));
#55452=CARTESIAN_POINT('Ctrl Pts',(30.6785222847241,1.17523507120987,26.270830214273));
#55453=CARTESIAN_POINT('Ctrl Pts',(30.,1.17523507120987,26.3124968809397));
#55454=CARTESIAN_POINT('Ctrl Pts',(29.3214777152758,1.17523507120987,26.3541635476064));
#55455=CARTESIAN_POINT('Ctrl Pts',(28.9822165729138,0.587617535604928,26.395830214273));
#55456=CARTESIAN_POINT('Ctrl Pts',(28.6429554305518,-1.32141489532166E-14,
26.4374968809397));
#55457=CARTESIAN_POINT('Ctrl Pts',(28.9822165729138,-0.587617535604954,
26.4791635476064));
#55458=CARTESIAN_POINT('Ctrl Pts',(29.3214777152758,-1.17523507120989,26.520830214273));
#55459=CARTESIAN_POINT('Ctrl Pts',(30.,-1.17523507120989,26.5624968809397));
#55460=CARTESIAN_POINT('Ctrl Pts',(30.6785222847241,-1.17523507120989,26.6041635476064));
#55461=CARTESIAN_POINT('Ctrl Pts',(31.0177834270861,-0.587617535604955,
26.645830214273));
#55462=CARTESIAN_POINT('Ctrl Pts',(31.3570445694482,-1.35453519623354E-14,
26.6874968809397));
#55463=CARTESIAN_POINT('Ctrl Pts',(31.0177834270861,0.587617535604927,26.7291635476064));
#55464=CARTESIAN_POINT('Ctrl Pts',(30.6785222847241,1.17523507120987,26.770830214273));
#55465=CARTESIAN_POINT('Ctrl Pts',(30.,1.17523507120987,26.8124968809397));
#55466=CARTESIAN_POINT('Ctrl Pts',(29.3214777152758,1.17523507120987,26.8541635476064));
#55467=CARTESIAN_POINT('Ctrl Pts',(28.9822165729138,0.587617535604928,26.895830214273));
#55468=CARTESIAN_POINT('Ctrl Pts',(28.6429554305518,-1.32141489532166E-14,
26.9374968809397));
#55469=CARTESIAN_POINT('Ctrl Pts',(28.9822165729138,-0.587617535604954,
26.9791635476064));
#55470=CARTESIAN_POINT('Ctrl Pts',(29.3214777152758,-1.17523507120989,27.020830214273));
#55471=CARTESIAN_POINT('Ctrl Pts',(30.,-1.17523507120989,27.0624968809397));
#55472=CARTESIAN_POINT('Ctrl Pts',(30.6785222847241,-1.17523507120989,27.1041635476064));
#55473=CARTESIAN_POINT('Ctrl Pts',(31.0177834270861,-0.587617535604955,
27.145830214273));
#55474=CARTESIAN_POINT('Ctrl Pts',(31.3570445694482,-1.35453519623354E-14,
27.1874968809397));
#55475=CARTESIAN_POINT('Ctrl Pts',(31.0177834270861,0.587617535604927,27.2291635476064));
#55476=CARTESIAN_POINT('Ctrl Pts',(30.6785222847241,1.17523507120987,27.270830214273));
#55477=CARTESIAN_POINT('Ctrl Pts',(30.,1.17523507120987,27.3124968809397));
#55478=CARTESIAN_POINT('Ctrl Pts',(29.3214777152758,1.17523507120987,27.3541635476064));
#55479=CARTESIAN_POINT('Ctrl Pts',(28.9822165729138,0.587617535604928,27.395830214273));
#55480=CARTESIAN_POINT('Ctrl Pts',(28.6429554305518,-1.32141489532166E-14,
27.4374968809397));
#55481=CARTESIAN_POINT('Ctrl Pts',(28.9822165729138,-0.587617535604954,
27.4791635476064));
#55482=CARTESIAN_POINT('Ctrl Pts',(29.3214777152758,-1.17523507120989,27.520830214273));
#55483=CARTESIAN_POINT('Ctrl Pts',(30.,-1.17523507120989,27.5624968809397));
#55484=CARTESIAN_POINT('Ctrl Pts',(30.6785222847241,-1.17523507120989,27.6041635476064));
#55485=CARTESIAN_POINT('Ctrl Pts',(31.0177834270861,-0.587617535604955,
27.645830214273));
#55486=CARTESIAN_POINT('Ctrl Pts',(31.3570445694482,-1.35453519623354E-14,
27.6874968809397));
#55487=CARTESIAN_POINT('Ctrl Pts',(31.0177834270861,0.587617535604927,27.7291635476064));
#55488=CARTESIAN_POINT('Ctrl Pts',(30.6785222847241,1.17523507120987,27.770830214273));
#55489=CARTESIAN_POINT('Ctrl Pts',(30.,1.17523507120987,27.8124968809397));
#55490=CARTESIAN_POINT('Ctrl Pts',(29.3214777152758,1.17523507120987,27.8541635476064));
#55491=CARTESIAN_POINT('Ctrl Pts',(28.9822165729138,0.587617535604928,27.895830214273));
#55492=CARTESIAN_POINT('Ctrl Pts',(28.6429554305518,-1.32141489532166E-14,
27.9374968809397));
#55493=CARTESIAN_POINT('Ctrl Pts',(28.9822165729138,-0.587617535604954,
27.9791635476064));
#55494=CARTESIAN_POINT('Ctrl Pts',(29.3214777152758,-1.17523507120989,28.020830214273));
#55495=CARTESIAN_POINT('Ctrl Pts',(30.,-1.17523507120989,28.0624968809397));
#55496=CARTESIAN_POINT('Ctrl Pts',(30.6785222847241,-1.17523507120989,28.1041635476064));
#55497=CARTESIAN_POINT('Ctrl Pts',(31.0177834270861,-0.587617535604955,
28.145830214273));
#55498=CARTESIAN_POINT('Ctrl Pts',(31.3570445694482,-1.35453519623354E-14,
28.1874968809397));
#55499=CARTESIAN_POINT('Ctrl Pts',(31.0177834270861,0.587617535604927,28.2291635476064));
#55500=CARTESIAN_POINT('Ctrl Pts',(30.6785222847241,1.17523507120987,28.270830214273));
#55501=CARTESIAN_POINT('Ctrl Pts',(30.,1.17523507120987,28.3124968809397));
#55502=CARTESIAN_POINT('Ctrl Pts',(29.3214777152758,1.17523507120987,28.3541635476064));
#55503=CARTESIAN_POINT('Ctrl Pts',(28.9822165729138,0.587617535604928,28.395830214273));
#55504=CARTESIAN_POINT('Ctrl Pts',(28.6429554305518,-1.32141489532166E-14,
28.4374968809397));
#55505=CARTESIAN_POINT('Ctrl Pts',(28.9822165729138,-0.587617535604954,
28.4791635476064));
#55506=CARTESIAN_POINT('Ctrl Pts',(29.3214777152758,-1.17523507120989,28.520830214273));
#55507=CARTESIAN_POINT('Ctrl Pts',(30.,-1.17523507120989,28.5624968809397));
#55508=CARTESIAN_POINT('Ctrl Pts',(30.6785222847241,-1.17523507120989,28.6041635476064));
#55509=CARTESIAN_POINT('Ctrl Pts',(31.0177834270861,-0.587617535604955,
28.645830214273));
#55510=CARTESIAN_POINT('Ctrl Pts',(31.3570445694482,-1.35453519623354E-14,
28.6874968809397));
#55511=CARTESIAN_POINT('Ctrl Pts',(31.0177834270861,0.587617535604927,28.7291635476064));
#55512=CARTESIAN_POINT('Ctrl Pts',(30.6785222847241,1.17523507120987,28.770830214273));
#55513=CARTESIAN_POINT('Ctrl Pts',(30.,1.17523507120987,28.8124968809397));
#55514=CARTESIAN_POINT('Ctrl Pts',(29.3214777152758,1.17523507120987,28.8541635476064));
#55515=CARTESIAN_POINT('Ctrl Pts',(28.9822165729138,0.587617535604928,28.895830214273));
#55516=CARTESIAN_POINT('Ctrl Pts',(28.6429554305518,-1.32141489532166E-14,
28.9374968809397));
#55517=CARTESIAN_POINT('Ctrl Pts',(28.9822165729138,-0.587617535604954,
28.9791635476064));
#55518=CARTESIAN_POINT('Ctrl Pts',(29.3214777152758,-1.17523507120989,29.020830214273));
#55519=CARTESIAN_POINT('Ctrl Pts',(30.,-1.17523507120989,29.0624968809397));
#55520=CARTESIAN_POINT('Ctrl Pts',(30.6785222847241,-1.17523507120989,29.1041635476064));
#55521=CARTESIAN_POINT('Ctrl Pts',(31.0177834270861,-0.587617535604955,
29.145830214273));
#55522=CARTESIAN_POINT('Ctrl Pts',(31.3570445694482,-1.35453519623354E-14,
29.1874968809397));
#55523=CARTESIAN_POINT('Ctrl Pts',(31.0177834270861,0.587617535604927,29.2291635476064));
#55524=CARTESIAN_POINT('Ctrl Pts',(30.6785222847241,1.17523507120987,29.270830214273));
#55525=CARTESIAN_POINT('Ctrl Pts',(30.,1.17523507120987,29.3124968809397));
#55526=CARTESIAN_POINT('Ctrl Pts',(29.3214777152758,1.17523507120987,29.3541635476064));
#55527=CARTESIAN_POINT('Ctrl Pts',(28.9822165729138,0.587617535604928,29.395830214273));
#55528=CARTESIAN_POINT('Ctrl Pts',(28.6429554305518,-1.32141489532166E-14,
29.4374968809397));
#55529=CARTESIAN_POINT('Ctrl Pts',(28.9822165729138,-0.587617535604954,
29.4791635476064));
#55530=CARTESIAN_POINT('Ctrl Pts',(29.3214777152758,-1.17523507120989,29.520830214273));
#55531=CARTESIAN_POINT('Ctrl Pts',(30.,-1.17523507120989,29.5624968809397));
#55532=CARTESIAN_POINT('Ctrl Pts',(30.6785222847241,-1.17523507120989,29.6041635476064));
#55533=CARTESIAN_POINT('Ctrl Pts',(31.0177834270861,-0.587617535604955,
29.645830214273));
#55534=CARTESIAN_POINT('Ctrl Pts',(31.3570445694482,-1.35453519623354E-14,
29.6874968809397));
#55535=CARTESIAN_POINT('Ctrl Pts',(31.0177834270861,0.587617535604927,29.7291635476064));
#55536=CARTESIAN_POINT('Ctrl Pts',(30.6785222847241,1.17523507120987,29.770830214273));
#55537=CARTESIAN_POINT('Ctrl Pts',(30.,1.17523507120987,29.8124968809397));
#55538=CARTESIAN_POINT('Ctrl Pts',(29.3214777152758,1.17523507120987,29.8541635476064));
#55539=CARTESIAN_POINT('Ctrl Pts',(28.9822165729138,0.587617535604928,29.895830214273));
#55540=CARTESIAN_POINT('Ctrl Pts',(28.6429554305518,-1.32141489532166E-14,
29.9374968809397));
#55541=CARTESIAN_POINT('Ctrl Pts',(28.9822165729138,-0.587617535604954,
29.9791635476064));
#55542=CARTESIAN_POINT('Ctrl Pts',(29.3214777152758,-1.17523507120989,30.020830214273));
#55543=CARTESIAN_POINT('Ctrl Pts',(30.,-1.17523507120989,30.0624968809397));
#55544=CARTESIAN_POINT('Ctrl Pts',(30.6785222847241,-1.17523507120989,30.1041635476064));
#55545=CARTESIAN_POINT('Ctrl Pts',(31.0177834270861,-0.587617535604955,
30.145830214273));
#55546=CARTESIAN_POINT('Ctrl Pts',(31.3570445694482,-1.35453519623354E-14,
30.1874968809397));
#55547=CARTESIAN_POINT('Ctrl Pts',(31.0177834270861,0.587617535604927,30.2291635476064));
#55548=CARTESIAN_POINT('Ctrl Pts',(30.6785222847241,1.17523507120987,30.270830214273));
#55549=CARTESIAN_POINT('Ctrl Pts',(30.,1.17523507120987,30.3124968809397));
#55550=CARTESIAN_POINT('Ctrl Pts',(29.3214777152758,1.17523507120987,30.3541635476064));
#55551=CARTESIAN_POINT('Ctrl Pts',(28.9822165729138,0.587617535604928,30.395830214273));
#55552=CARTESIAN_POINT('Ctrl Pts',(28.6429554305518,-1.32141489532166E-14,
30.4374968809397));
#55553=CARTESIAN_POINT('Ctrl Pts',(28.9822165729138,-0.587617535604954,
30.4791635476064));
#55554=CARTESIAN_POINT('Ctrl Pts',(29.3214777152758,-1.17523507120989,30.520830214273));
#55555=CARTESIAN_POINT('Ctrl Pts',(30.,-1.17523507120989,30.5624968809397));
#55556=CARTESIAN_POINT('Ctrl Pts',(30.6785222847241,-1.17523507120989,30.6041635476064));
#55557=CARTESIAN_POINT('Ctrl Pts',(31.0177834270861,-0.587617535604955,
30.645830214273));
#55558=CARTESIAN_POINT('Ctrl Pts',(31.3570445694482,-1.35453519623354E-14,
30.6874968809397));
#55559=CARTESIAN_POINT('Ctrl Pts',(31.0177834270861,0.587617535604927,30.7291635476064));
#55560=CARTESIAN_POINT('Ctrl Pts',(30.6785222847241,1.17523507120987,30.770830214273));
#55561=CARTESIAN_POINT('Ctrl Pts',(30.,1.17523507120987,30.8124968809397));
#55562=CARTESIAN_POINT('Ctrl Pts',(29.3214777152758,1.17523507120987,30.8541635476064));
#55563=CARTESIAN_POINT('Ctrl Pts',(28.9822165729138,0.587617535604928,30.895830214273));
#55564=CARTESIAN_POINT('Ctrl Pts',(28.6429554305518,-1.32141489532166E-14,
30.9374968809397));
#55565=CARTESIAN_POINT('Ctrl Pts',(28.9822165729138,-0.587617535604954,
30.9791635476064));
#55566=CARTESIAN_POINT('Ctrl Pts',(29.3214777152758,-1.17523507120989,31.020830214273));
#55567=CARTESIAN_POINT('Ctrl Pts',(30.,-1.17523507120989,31.0624968809397));
#55568=CARTESIAN_POINT('Ctrl Pts',(30.6785222847241,-1.17523507120989,31.1041635476064));
#55569=CARTESIAN_POINT('Ctrl Pts',(31.0177834270861,-0.587617535604955,
31.145830214273));
#55570=CARTESIAN_POINT('Ctrl Pts',(31.3570445694482,-1.35453519623354E-14,
31.1874968809397));
#55571=CARTESIAN_POINT('Ctrl Pts',(31.0177834270861,0.587617535604927,31.2291635476064));
#55572=CARTESIAN_POINT('Ctrl Pts',(30.6785222847241,1.17523507120987,31.270830214273));
#55573=CARTESIAN_POINT('Ctrl Pts',(30.,1.17523507120987,31.3124968809397));
#55574=CARTESIAN_POINT('',(30.,-1.50000000000002,30.75));
#55575=CARTESIAN_POINT('Origin',(30.,-1.24258096838242E-13,1029.88397459622));
#55576=CARTESIAN_POINT('Origin',(30.06875,2.82851012598683,15.7235432561772));
#55577=CARTESIAN_POINT('',(30.012548982272,2.70302030326666,15.7235432561772));
#55578=CARTESIAN_POINT('Origin',(30.,2.70864040503946,15.7235432561772));
#55579=CARTESIAN_POINT('',(29.987451017728,2.70302030326666,15.7235432561772));
#55580=CARTESIAN_POINT('Origin',(29.987451017728,2.70302030326666,15.7235432561772));
#55581=CARTESIAN_POINT('Origin',(30.2904604134361,2.81439671040465,15.7235432561772));
#55582=CARTESIAN_POINT('',(30.224586826676,2.69370321195774,15.7235432561772));
#55583=CARTESIAN_POINT('Origin',(30.2125174768313,2.70029057063376,15.7235432561772));
#55584=CARTESIAN_POINT('',(30.1995662307806,2.69567237556048,15.7235432561772));
#55585=CARTESIAN_POINT('Origin',(30.1995662307806,2.69567237556048,15.7235432561772));
#55586=CARTESIAN_POINT('Origin',(29.8466157199522,2.82518483606723,15.7235432561772));
#55587=CARTESIAN_POINT('',(29.8004337692194,2.69567237556048,15.7235432561772));
#55588=CARTESIAN_POINT('Origin',(29.7874825231687,2.70029057063376,15.7235432561772));
#55589=CARTESIAN_POINT('',(29.775413173324,2.69370321195775,15.7235432561772));
#55590=CARTESIAN_POINT('Origin',(29.775413173324,2.69370321195775,15.7235432561772));
#55591=CARTESIAN_POINT('Origin',(29.6254271049963,2.804441342164,15.7235432561772));
#55592=CARTESIAN_POINT('',(29.589548948342,2.67170473125694,15.7235432561772));
#55593=CARTESIAN_POINT('Origin',(29.5762752872513,2.67529254692237,15.7235432561772));
#55594=CARTESIAN_POINT('',(29.5647599813892,2.6677785445999,15.7235432561772));
#55595=CARTESIAN_POINT('Origin',(29.5647599813892,2.6677785445999,15.7235432561772));
#55596=CARTESIAN_POINT('Origin',(29.4065478564962,2.76640753481494,15.7235432561772));
#55597=CARTESIAN_POINT('',(29.3811946946869,2.63126513885323,15.7235432561772));
#55598=CARTESIAN_POINT('Origin',(29.3676804550908,2.63380045503416,15.7235432561772));
#55599=CARTESIAN_POINT('',(29.3567901889011,2.6254061353882,15.7235432561772));
#55600=CARTESIAN_POINT('Origin',(29.3567901889011,2.6254061353882,15.7235432561772));
#55601=CARTESIAN_POINT('Origin',(29.1913274378037,2.71131790508989,15.7235432561772));
#55602=CARTESIAN_POINT('',(29.1766555815128,2.57460292188403,15.7235432561772));
#55603=CARTESIAN_POINT('Origin',(29.1629840831922,2.57607010751313,15.7235432561772));
#55604=CARTESIAN_POINT('',(29.1527859987874,2.56684722431571,15.7235432561772));
#55605=CARTESIAN_POINT('Origin',(29.1527859987874,2.56684722431571,15.7235432561772));
#55606=CARTESIAN_POINT('Origin',(28.9810927543681,2.63951209887526,15.7235432561772));
#55607=CARTESIAN_POINT('',(28.9771926604684,2.50206742175908,15.7235432561772));
#55608=CARTESIAN_POINT('Origin',(28.9634481927567,2.50245743114905,15.7235432561772));
#55609=CARTESIAN_POINT('',(28.9540051647184,2.49246284654199,15.7235432561772));
#55610=CARTESIAN_POINT('Origin',(28.9540051647184,2.49246284654199,15.7235432561772));
#55611=CARTESIAN_POINT('Origin',(28.7771399729228,2.55143282284423,15.7235432561772));
#55612=CARTESIAN_POINT('Origin',(28.7616732366375,2.40271160649133,15.7235432561772));
#55613=CARTESIAN_POINT('Origin',(28.5807265301867,2.44762311502286,15.7235432561772));
#55614=CARTESIAN_POINT('Origin',(28.5769760048382,2.29814685040398,15.7235432561772));
#55615=CARTESIAN_POINT('Origin',(28.3930633803483,2.32872299678009,15.7235432561772));
#55616=CARTESIAN_POINT('Origin',(28.4010521891726,2.1794132547725,15.7235432561772));
#55617=CARTESIAN_POINT('Origin',(28.2153075291307,2.1954655268832,15.7235432561772));
#55618=CARTESIAN_POINT('Origin',(28.2349864184648,2.0472428516969,15.7235432561772));
#55619=CARTESIAN_POINT('Origin',(28.0485549004665,2.0486722819467,15.7235432561772));
#55620=CARTESIAN_POINT('Origin',(28.0798025434137,1.90245051566326,15.7235432561772));
#55621=CARTESIAN_POINT('Origin',(27.8938335797622,1.88924829113933,15.7235432561772));
#55622=CARTESIAN_POINT('Origin',(27.9364573242129,1.74592893957157,15.7235432561772));
#55623=CARTESIAN_POINT('Origin',(27.7520974754101,1.71817645637828,15.7235432561772));
#55624=CARTESIAN_POINT('Origin',(27.805834531806,1.57864313098712,15.7235432561772));
#55625=CARTESIAN_POINT('Origin',(27.6242204376256,1.53651149241201,15.7235432561772));
#55626=CARTESIAN_POINT('Origin',(27.6887394991445,1.40162446254803,15.7235432561772));
#55627=CARTESIAN_POINT('Origin',(27.5109908708699,1.3453734241531,15.7235432561772));
#55628=CARTESIAN_POINT('Origin',(27.5858941560429,1.2159643132099,15.7235432561772));
#55629=CARTESIAN_POINT('Origin',(30.5103800418355,2.78293160322096,15.7235432561772));
#55630=CARTESIAN_POINT('',(30.4352400186108,2.66777854459989,15.7235432561772));
#55631=CARTESIAN_POINT('Origin',(30.4237247127487,2.67529254692237,15.7235432561772));
#55632=CARTESIAN_POINT('',(30.410451051658,2.67170473125694,15.7235432561772));
#55633=CARTESIAN_POINT('Origin',(30.410451051658,2.67170473125694,15.7235432561772));
#55634=CARTESIAN_POINT('Origin',(30.7271530075584,2.73430879728474,15.7235432561772));
#55635=CARTESIAN_POINT('',(30.6432098110989,2.62540613538819,15.7235432561772));
#55636=CARTESIAN_POINT('Origin',(30.6323195449092,2.63380045503415,15.7235432561772));
#55637=CARTESIAN_POINT('',(30.6188053053131,2.63126513885322,15.7235432561772));
#55638=CARTESIAN_POINT('Origin',(30.6188053053131,2.63126513885322,15.7235432561772));
#55639=CARTESIAN_POINT('Origin',(30.9394428331868,2.66882806836332,15.7235432561772));
#55640=CARTESIAN_POINT('',(30.8472140012126,2.5668472243157,15.7235432561772));
#55641=CARTESIAN_POINT('Origin',(30.8370159168078,2.57607010751312,15.7235432561772));
#55642=CARTESIAN_POINT('',(30.8233444184872,2.57460292188402,15.7235432561772));
#55643=CARTESIAN_POINT('Origin',(30.8233444184872,2.57460292188402,15.7235432561772));
#55644=CARTESIAN_POINT('Origin',(31.1459406813522,2.58689312692505,15.7235432561772));
#55645=CARTESIAN_POINT('',(31.0459948352816,2.49246284654197,15.7235432561772));
#55646=CARTESIAN_POINT('Origin',(31.0365518072432,2.50245743114904,15.7235432561772));
#55647=CARTESIAN_POINT('',(31.0228073395316,2.50206742175906,15.7235432561772));
#55648=CARTESIAN_POINT('Origin',(31.0228073395316,2.50206742175906,15.7235432561772));
#55649=CARTESIAN_POINT('Origin',(31.3453734241531,2.48900912913003,15.7235432561772));
#55650=CARTESIAN_POINT('',(31.2383267633625,2.40271160649132,15.7235432561772));
#55651=CARTESIAN_POINT('Origin',(31.2296970110986,2.41341627257038,15.7235432561772));
#55652=CARTESIAN_POINT('',(31.2159643132099,2.41410584395711,15.7235432561772));
#55653=CARTESIAN_POINT('Origin',(31.2159643132099,2.41410584395711,15.7235432561772));
#55654=CARTESIAN_POINT('Origin',(31.536511492412,2.3757795623744,15.7235432561772));
#55655=CARTESIAN_POINT('',(31.4230239951618,2.29814685040396,15.7235432561772));
#55656=CARTESIAN_POINT('Origin',(31.4152607239647,2.30949560012898,15.7235432561772));
#55657=CARTESIAN_POINT('',(31.401624462548,2.3112605008555,15.7235432561772));
#55658=CARTESIAN_POINT('Origin',(31.401624462548,2.3112605008555,15.7235432561772));
#55659=CARTESIAN_POINT('Origin',(31.7181764563782,2.24790252458986,15.7235432561772));
#55660=CARTESIAN_POINT('',(31.5989478108274,2.17941325477248,15.7235432561772));
#55661=CARTESIAN_POINT('Origin',(31.5920988838457,2.19133611932756,15.7235432561772));
#55662=CARTESIAN_POINT('',(31.5786431309871,2.19416546819402,15.7235432561772));
#55663=CARTESIAN_POINT('Origin',(31.5786431309871,2.19416546819402,15.7235432561772));
#55664=CARTESIAN_POINT('Origin',(31.8892482911393,2.10616642023777,15.7235432561772));
#55665=CARTESIAN_POINT('',(31.7650135815352,2.04724285169688,15.7235432561772));
#55666=CARTESIAN_POINT('Origin',(31.7591212246811,2.05966632265728,15.7235432561772));
#55667=CARTESIAN_POINT('',(31.7459289395715,2.06354267578706,15.7235432561772));
#55668=CARTESIAN_POINT('Origin',(31.7459289395715,2.06354267578706,15.7235432561772));
#55669=CARTESIAN_POINT('Origin',(32.0486722819467,1.95144509953352,15.7235432561772));
#55670=CARTESIAN_POINT('',(31.9201974565863,1.90245051566323,15.7235432561772));
#55671=CARTESIAN_POINT('Origin',(31.9152979981993,1.91529799819927,15.7235432561772));
#55672=CARTESIAN_POINT('',(31.9024505156632,1.9201974565863,15.7235432561772));
#55673=CARTESIAN_POINT('Origin',(31.9024505156632,1.9201974565863,15.7235432561772));
#55674=CARTESIAN_POINT('Origin',(32.1954655268832,1.7846924708693,15.7235432561772));
#55675=CARTESIAN_POINT('',(32.0635426757871,1.74592893957153,15.7235432561772));
#55676=CARTESIAN_POINT('Origin',(32.0596663226573,1.75912122468115,15.7235432561772));
#55677=CARTESIAN_POINT('',(32.0472428516969,1.76501358153524,15.7235432561772));
#55678=CARTESIAN_POINT('Origin',(32.0472428516969,1.76501358153524,15.7235432561772));
#55679=CARTESIAN_POINT('Origin',(32.3287229967801,1.6069366196517,15.7235432561772));
#55680=CARTESIAN_POINT('',(32.194165468194,1.57864313098709,15.7235432561772));
#55681=CARTESIAN_POINT('Origin',(32.1913361193276,1.59209888384569,15.7235432561772));
#55682=CARTESIAN_POINT('',(32.1794132547725,1.59894781082743,15.7235432561772));
#55683=CARTESIAN_POINT('Origin',(32.1794132547725,1.59894781082743,15.7235432561772));
#55684=CARTESIAN_POINT('Origin',(32.4476231150228,1.41927346981329,15.7235432561772));
#55685=CARTESIAN_POINT('',(32.3112605008555,1.401624462548,15.7235432561772));
#55686=CARTESIAN_POINT('Origin',(32.309495600129,1.41526072396473,15.7235432561772));
#55687=CARTESIAN_POINT('',(32.298146850404,1.42302399516178,15.7235432561772));
#55688=CARTESIAN_POINT('Origin',(32.298146850404,1.42302399516178,15.7235432561772));
#55689=CARTESIAN_POINT('Origin',(32.5514328228442,1.22286002707717,15.7235432561772));
#55690=CARTESIAN_POINT('',(32.4141058439571,1.21596431320987,15.7235432561772));
#55691=CARTESIAN_POINT('Origin',(32.4134162725704,1.22969701109858,15.7235432561772));
#55692=CARTESIAN_POINT('',(32.4027116064913,1.23832676336245,15.7235432561772));
#55693=CARTESIAN_POINT('Origin',(32.4027116064913,1.23832676336245,15.7235432561772));
#55694=CARTESIAN_POINT('Origin',(32.6395120988752,1.01890724563189,15.7235432561772));
#55695=CARTESIAN_POINT('',(32.5020674217591,1.02280733953163,15.7235432561772));
#55696=CARTESIAN_POINT('Origin',(32.502457431149,1.03655180724325,15.7235432561772));
#55697=CARTESIAN_POINT('',(32.492462846542,1.04599483528156,15.7235432561772));
#55698=CARTESIAN_POINT('Origin',(32.492462846542,1.04599483528156,15.7235432561772));
#55699=CARTESIAN_POINT('Origin',(32.7113179050899,0.808672562196245,15.7235432561772));
#55700=CARTESIAN_POINT('',(32.574602921884,0.823344418487232,15.7235432561772));
#55701=CARTESIAN_POINT('Origin',(32.5760701075131,0.837015916807817,15.7235432561772));
#55702=CARTESIAN_POINT('',(32.5668472243157,0.84721400121258,15.7235432561772));
#55703=CARTESIAN_POINT('Origin',(32.5668472243157,0.84721400121258,15.7235432561772));
#55704=CARTESIAN_POINT('Origin',(32.7664075348149,0.593452143503749,15.7235432561772));
#55705=CARTESIAN_POINT('',(32.6312651388532,0.618805305313054,15.7235432561772));
#55706=CARTESIAN_POINT('Origin',(32.6338004550341,0.632319544909225,15.7235432561772));
#55707=CARTESIAN_POINT('',(32.6254061353882,0.64320981109888,15.7235432561772));
#55708=CARTESIAN_POINT('Origin',(32.6254061353882,0.64320981109888,15.7235432561772));
#55709=CARTESIAN_POINT('Origin',(32.804441342164,0.37457289500369,15.7235432561772));
#55710=CARTESIAN_POINT('',(32.6717047312569,0.410451051657977,15.7235432561772));
#55711=CARTESIAN_POINT('Origin',(32.6752925469224,0.423724712748682,15.7235432561772));
#55712=CARTESIAN_POINT('',(32.6677785445999,0.435240018610789,15.7235432561772));
#55713=CARTESIAN_POINT('Origin',(32.6677785445999,0.435240018610789,15.7235432561772));
#55714=CARTESIAN_POINT('Origin',(32.8251848360672,0.153384280047806,15.7235432561772));
#55715=CARTESIAN_POINT('',(32.6956723755605,0.199566230780603,15.7235432561772));
#55716=CARTESIAN_POINT('Origin',(32.7002905706337,0.212517476831278,15.7235432561772));
#55717=CARTESIAN_POINT('',(32.6937032119577,0.224586826675969,15.7235432561772));
#55718=CARTESIAN_POINT('Origin',(32.6937032119577,0.224586826675969,15.7235432561772));
#55719=CARTESIAN_POINT('Origin',(32.8285101259868,-0.0687500000000229,15.7235432561772));
#55720=CARTESIAN_POINT('',(32.7030203032667,-0.0125489822720396,15.7235432561772));
#55721=CARTESIAN_POINT('Origin',(32.7086404050395,-2.31188656783185E-14,
15.7235432561772));
#55722=CARTESIAN_POINT('',(32.7030203032667,0.0125489822719939,15.7235432561772));
#55723=CARTESIAN_POINT('Origin',(32.7030203032667,0.0125489822719939,15.7235432561772));
#55724=CARTESIAN_POINT('Origin',(32.8143967104046,-0.290460413436156,15.7235432561772));
#55725=CARTESIAN_POINT('',(32.6937032119577,-0.224586826676015,15.7235432561772));
#55726=CARTESIAN_POINT('Origin',(32.7002905706337,-0.212517476831324,15.7235432561772));
#55727=CARTESIAN_POINT('',(32.6956723755605,-0.199566230780649,15.7235432561772));
#55728=CARTESIAN_POINT('Origin',(32.6956723755605,-0.199566230780649,15.7235432561772));
#55729=CARTESIAN_POINT('Origin',(32.7829316032209,-0.510380041835567,15.7235432561772));
#55730=CARTESIAN_POINT('',(32.6677785445999,-0.435240018610835,15.7235432561772));
#55731=CARTESIAN_POINT('Origin',(32.6752925469224,-0.423724712748728,15.7235432561772));
#55732=CARTESIAN_POINT('',(32.6717047312569,-0.410451051658023,15.7235432561772));
#55733=CARTESIAN_POINT('Origin',(32.6717047312569,-0.410451051658023,15.7235432561772));
#55734=CARTESIAN_POINT('Origin',(32.7343087972847,-0.727153007558476,15.7235432561772));
#55735=CARTESIAN_POINT('',(32.6254061353882,-0.643209811098926,15.7235432561772));
#55736=CARTESIAN_POINT('Origin',(32.6338004550341,-0.632319544909271,15.7235432561772));
#55737=CARTESIAN_POINT('',(32.6312651388532,-0.6188053053131,15.7235432561772));
#55738=CARTESIAN_POINT('Origin',(32.6312651388532,-0.6188053053131,15.7235432561772));
#55739=CARTESIAN_POINT('Origin',(32.6688280683633,-0.939442833186874,15.7235432561772));
#55740=CARTESIAN_POINT('',(32.5668472243157,-0.847214001212625,15.7235432561772));
#55741=CARTESIAN_POINT('Origin',(32.5760701075131,-0.837015916807863,15.7235432561772));
#55742=CARTESIAN_POINT('',(32.574602921884,-0.823344418487278,15.7235432561772));
#55743=CARTESIAN_POINT('Origin',(32.574602921884,-0.823344418487278,15.7235432561772));
#55744=CARTESIAN_POINT('Origin',(32.586893126925,-1.14594068135223,15.7235432561772));
#55745=CARTESIAN_POINT('',(32.492462846542,-1.0459948352816,15.7235432561772));
#55746=CARTESIAN_POINT('Origin',(32.502457431149,-1.0365518072433,15.7235432561772));
#55747=CARTESIAN_POINT('',(32.5020674217591,-1.02280733953168,15.7235432561772));
#55748=CARTESIAN_POINT('Origin',(32.5020674217591,-1.02280733953168,15.7235432561772));
#55749=CARTESIAN_POINT('Origin',(32.48900912913,-1.34537342415311,15.7235432561772));
#55750=CARTESIAN_POINT('',(32.4027116064913,-1.2383267633625,15.7235432561772));
#55751=CARTESIAN_POINT('Origin',(32.4134162725704,-1.22969701109862,15.7235432561772));
#55752=CARTESIAN_POINT('',(32.4141058439571,-1.21596431320991,15.7235432561772));
#55753=CARTESIAN_POINT('Origin',(32.4141058439571,-1.21596431320991,15.7235432561772));
#55754=CARTESIAN_POINT('Origin',(32.3757795623744,-1.53651149241202,15.7235432561772));
#55755=CARTESIAN_POINT('',(32.2981468504039,-1.42302399516182,15.7235432561772));
#55756=CARTESIAN_POINT('Origin',(32.309495600129,-1.41526072396478,15.7235432561772));
#55757=CARTESIAN_POINT('',(32.3112605008555,-1.40162446254804,15.7235432561772));
#55758=CARTESIAN_POINT('Origin',(32.3112605008555,-1.40162446254804,15.7235432561772));
#55759=CARTESIAN_POINT('Origin',(32.2479025245898,-1.71817645637829,15.7235432561772));
#55760=CARTESIAN_POINT('',(32.1794132547725,-1.59894781082747,15.7235432561772));
#55761=CARTESIAN_POINT('Origin',(32.1913361193275,-1.59209888384574,15.7235432561772));
#55762=CARTESIAN_POINT('',(32.194165468194,-1.57864313098713,15.7235432561772));
#55763=CARTESIAN_POINT('Origin',(32.194165468194,-1.57864313098713,15.7235432561772));
#55764=CARTESIAN_POINT('Origin',(32.1061664202378,-1.88924829113934,15.7235432561772));
#55765=CARTESIAN_POINT('',(32.0472428516969,-1.76501358153528,15.7235432561772));
#55766=CARTESIAN_POINT('Origin',(32.0596663226573,-1.75912122468119,15.7235432561772));
#55767=CARTESIAN_POINT('',(32.063542675787,-1.74592893957158,15.7235432561772));
#55768=CARTESIAN_POINT('Origin',(32.063542675787,-1.74592893957158,15.7235432561772));
#55769=CARTESIAN_POINT('Origin',(31.9514450995335,-2.04867228194671,15.7235432561772));
#55770=CARTESIAN_POINT('',(31.9024505156632,-1.92019745658634,15.7235432561772));
#55771=CARTESIAN_POINT('Origin',(31.9152979981993,-1.91529799819931,15.7235432561772));
#55772=CARTESIAN_POINT('',(31.9201974565863,-1.90245051566327,15.7235432561772));
#55773=CARTESIAN_POINT('Origin',(31.9201974565863,-1.90245051566327,15.7235432561772));
#55774=CARTESIAN_POINT('Origin',(31.7846924708693,-2.19546552688321,15.7235432561772));
#55775=CARTESIAN_POINT('',(31.7459289395715,-2.0635426757871,15.7235432561772));
#55776=CARTESIAN_POINT('Origin',(31.7591212246811,-2.05966632265732,15.7235432561772));
#55777=CARTESIAN_POINT('',(31.7650135815352,-2.04724285169692,15.7235432561772));
#55778=CARTESIAN_POINT('Origin',(31.7650135815352,-2.04724285169692,15.7235432561772));
#55779=CARTESIAN_POINT('Origin',(31.6069366196517,-2.32872299678011,15.7235432561772));
#55780=CARTESIAN_POINT('',(31.5786431309871,-2.19416546819406,15.7235432561772));
#55781=CARTESIAN_POINT('Origin',(31.5920988838457,-2.1913361193276,15.7235432561772));
#55782=CARTESIAN_POINT('',(31.5989478108274,-2.17941325477251,15.7235432561772));
#55783=CARTESIAN_POINT('Origin',(31.5989478108274,-2.17941325477251,15.7235432561772));
#55784=CARTESIAN_POINT('Origin',(31.4192734698133,-2.44762311502288,15.7235432561772));
#55785=CARTESIAN_POINT('',(31.401624462548,-2.31126050085554,15.7235432561772));
#55786=CARTESIAN_POINT('Origin',(31.4152607239647,-2.30949560012901,15.7235432561772));
#55787=CARTESIAN_POINT('',(31.4230239951618,-2.29814685040399,15.7235432561772));
#55788=CARTESIAN_POINT('Origin',(31.4230239951618,-2.29814685040399,15.7235432561772));
#55789=CARTESIAN_POINT('Origin',(31.2228600270771,-2.55143282284425,15.7235432561772));
#55790=CARTESIAN_POINT('',(31.2159643132098,-2.41410584395714,15.7235432561772));
#55791=CARTESIAN_POINT('Origin',(31.2296970110986,-2.41341627257041,15.7235432561772));
#55792=CARTESIAN_POINT('',(31.2383267633624,-2.40271160649135,15.7235432561772));
#55793=CARTESIAN_POINT('Origin',(31.2383267633624,-2.40271160649135,15.7235432561772));
#55794=CARTESIAN_POINT('Origin',(31.0189072456319,-2.63951209887528,15.7235432561772));
#55795=CARTESIAN_POINT('',(31.0228073395316,-2.5020674217591,15.7235432561772));
#55796=CARTESIAN_POINT('Origin',(31.0365518072432,-2.50245743114907,15.7235432561772));
#55797=CARTESIAN_POINT('',(31.0459948352815,-2.49246284654201,15.7235432561772));
#55798=CARTESIAN_POINT('Origin',(31.0459948352815,-2.49246284654201,15.7235432561772));
#55799=CARTESIAN_POINT('Origin',(30.8086725621962,-2.71131790508991,15.7235432561772));
#55800=CARTESIAN_POINT('',(30.8233444184872,-2.57460292188405,15.7235432561772));
#55801=CARTESIAN_POINT('Origin',(30.8370159168078,-2.57607010751315,15.7235432561772));
#55802=CARTESIAN_POINT('',(30.8472140012126,-2.56684722431573,15.7235432561772));
#55803=CARTESIAN_POINT('Origin',(30.8472140012126,-2.56684722431573,15.7235432561772));
#55804=CARTESIAN_POINT('Origin',(30.5934521435037,-2.76640753481496,15.7235432561772));
#55805=CARTESIAN_POINT('',(30.618805305313,-2.63126513885325,15.7235432561772));
#55806=CARTESIAN_POINT('Origin',(30.6323195449092,-2.63380045503418,15.7235432561772));
#55807=CARTESIAN_POINT('',(30.6432098110989,-2.62540613538822,15.7235432561772));
#55808=CARTESIAN_POINT('Origin',(30.6432098110989,-2.62540613538822,15.7235432561772));
#55809=CARTESIAN_POINT('Origin',(30.3745728950037,-2.80444134216402,15.7235432561772));
#55810=CARTESIAN_POINT('',(30.410451051658,-2.67170473125697,15.7235432561772));
#55811=CARTESIAN_POINT('Origin',(30.4237247127487,-2.67529254692239,15.7235432561772));
#55812=CARTESIAN_POINT('',(30.4352400186108,-2.66777854459992,15.7235432561772));
#55813=CARTESIAN_POINT('Origin',(30.4352400186108,-2.66777854459992,15.7235432561772));
#55814=CARTESIAN_POINT('Origin',(30.1533842800478,-2.82518483606726,15.7235432561772));
#55815=CARTESIAN_POINT('',(30.1995662307806,-2.69567237556051,15.7235432561772));
#55816=CARTESIAN_POINT('Origin',(30.2125174768313,-2.70029057063379,15.7235432561772));
#55817=CARTESIAN_POINT('',(30.224586826676,-2.69370321195777,15.7235432561772));
#55818=CARTESIAN_POINT('Origin',(30.224586826676,-2.69370321195777,15.7235432561772));
#55819=CARTESIAN_POINT('Origin',(29.93125,-2.82851012598686,15.7235432561772));
#55820=CARTESIAN_POINT('',(29.987451017728,-2.70302030326669,15.7235432561772));
#55821=CARTESIAN_POINT('Origin',(30.,-2.70864040503949,15.7235432561772));
#55822=CARTESIAN_POINT('',(30.012548982272,-2.70302030326669,15.7235432561772));
#55823=CARTESIAN_POINT('Origin',(30.012548982272,-2.70302030326669,15.7235432561772));
#55824=CARTESIAN_POINT('Origin',(29.7095395865638,-2.81439671040468,15.7235432561772));
#55825=CARTESIAN_POINT('',(29.775413173324,-2.69370321195777,15.7235432561772));
#55826=CARTESIAN_POINT('Origin',(29.7874825231687,-2.70029057063378,15.7235432561772));
#55827=CARTESIAN_POINT('',(29.8004337692193,-2.6956723755605,15.7235432561772));
#55828=CARTESIAN_POINT('Origin',(29.8004337692193,-2.6956723755605,15.7235432561772));
#55829=CARTESIAN_POINT('Origin',(29.4896199581644,-2.78293160322098,15.7235432561772));
#55830=CARTESIAN_POINT('',(29.5647599813891,-2.66777854459992,15.7235432561772));
#55831=CARTESIAN_POINT('Origin',(29.5762752872513,-2.67529254692239,15.7235432561772));
#55832=CARTESIAN_POINT('',(29.589548948342,-2.67170473125696,15.7235432561772));
#55833=CARTESIAN_POINT('Origin',(29.589548948342,-2.67170473125696,15.7235432561772));
#55834=CARTESIAN_POINT('Origin',(29.2728469924415,-2.73430879728476,15.7235432561772));
#55835=CARTESIAN_POINT('',(29.3567901889011,-2.62540613538822,15.7235432561772));
#55836=CARTESIAN_POINT('Origin',(29.3676804550907,-2.63380045503417,15.7235432561772));
#55837=CARTESIAN_POINT('',(29.3811946946869,-2.63126513885324,15.7235432561772));
#55838=CARTESIAN_POINT('Origin',(29.3811946946869,-2.63126513885324,15.7235432561772));
#55839=CARTESIAN_POINT('Origin',(29.0605571668131,-2.66882806836334,15.7235432561772));
#55840=CARTESIAN_POINT('',(29.1527859987874,-2.56684722431572,15.7235432561772));
#55841=CARTESIAN_POINT('Origin',(29.1629840831921,-2.57607010751314,15.7235432561772));
#55842=CARTESIAN_POINT('',(29.1766555815127,-2.57460292188404,15.7235432561772));
#55843=CARTESIAN_POINT('Origin',(29.1766555815127,-2.57460292188404,15.7235432561772));
#55844=CARTESIAN_POINT('Origin',(28.8540593186477,-2.58689312692507,15.7235432561772));
#55845=CARTESIAN_POINT('',(28.9540051647184,-2.49246284654199,15.7235432561772));
#55846=CARTESIAN_POINT('Origin',(28.9634481927567,-2.50245743114906,15.7235432561772));
#55847=CARTESIAN_POINT('',(28.9771926604683,-2.50206742175908,15.7235432561772));
#55848=CARTESIAN_POINT('Origin',(28.9771926604683,-2.50206742175908,15.7235432561772));
#55849=CARTESIAN_POINT('Origin',(28.6546265758469,-2.48900912913005,15.7235432561772));
#55850=CARTESIAN_POINT('',(28.7616732366375,-2.40271160649133,15.7235432561772));
#55851=CARTESIAN_POINT('Origin',(28.7703029889014,-2.4134162725704,15.7235432561772));
#55852=CARTESIAN_POINT('',(28.7840356867901,-2.41410584395713,15.7235432561772));
#55853=CARTESIAN_POINT('Origin',(28.7840356867901,-2.41410584395713,15.7235432561772));
#55854=CARTESIAN_POINT('Origin',(28.463488507588,-2.37577956237441,15.7235432561772));
#55855=CARTESIAN_POINT('',(28.5769760048382,-2.29814685040397,15.7235432561772));
#55856=CARTESIAN_POINT('Origin',(28.5847392760352,-2.30949560012899,15.7235432561772));
#55857=CARTESIAN_POINT('',(28.5983755374519,-2.31126050085552,15.7235432561772));
#55858=CARTESIAN_POINT('Origin',(28.5983755374519,-2.31126050085552,15.7235432561772));
#55859=CARTESIAN_POINT('Origin',(28.2818235436217,-2.24790252458987,15.7235432561772));
#55860=CARTESIAN_POINT('',(28.4010521891725,-2.17941325477249,15.7235432561772));
#55861=CARTESIAN_POINT('Origin',(28.4079011161542,-2.19133611932757,15.7235432561772));
#55862=CARTESIAN_POINT('',(28.4213568690129,-2.19416546819403,15.7235432561772));
#55863=CARTESIAN_POINT('Origin',(28.4213568690129,-2.19416546819403,15.7235432561772));
#55864=CARTESIAN_POINT('Origin',(28.1107517088606,-2.10616642023779,15.7235432561772));
#55865=CARTESIAN_POINT('',(28.2349864184647,-2.04724285169689,15.7235432561772));
#55866=CARTESIAN_POINT('Origin',(28.2408787753188,-2.0596663226573,15.7235432561772));
#55867=CARTESIAN_POINT('',(28.2540710604284,-2.06354267578707,15.7235432561772));
#55868=CARTESIAN_POINT('Origin',(28.2540710604284,-2.06354267578707,15.7235432561772));
#55869=CARTESIAN_POINT('Origin',(27.9513277180533,-1.95144509953353,15.7235432561772));
#55870=CARTESIAN_POINT('',(28.0798025434136,-1.90245051566325,15.7235432561772));
#55871=CARTESIAN_POINT('Origin',(28.0847020018007,-1.91529799819928,15.7235432561772));
#55872=CARTESIAN_POINT('',(28.0975494843367,-1.92019745658631,15.7235432561772));
#55873=CARTESIAN_POINT('Origin',(28.0975494843367,-1.92019745658631,15.7235432561772));
#55874=CARTESIAN_POINT('Origin',(27.8045344731168,-1.78469247086931,15.7235432561772));
#55875=CARTESIAN_POINT('',(27.9364573242129,-1.74592893957155,15.7235432561772));
#55876=CARTESIAN_POINT('Origin',(27.9403336773427,-1.75912122468116,15.7235432561772));
#55877=CARTESIAN_POINT('',(27.9527571483031,-1.76501358153525,15.7235432561772));
#55878=CARTESIAN_POINT('Origin',(27.9527571483031,-1.76501358153525,15.7235432561772));
#55879=CARTESIAN_POINT('Origin',(27.6712770032199,-1.6069366196517,15.7235432561772));
#55880=CARTESIAN_POINT('',(27.8058345318059,-1.5786431309871,15.7235432561772));
#55881=CARTESIAN_POINT('Origin',(27.8086638806724,-1.59209888384571,15.7235432561772));
#55882=CARTESIAN_POINT('',(27.8205867452275,-1.59894781082744,15.7235432561772));
#55883=CARTESIAN_POINT('Origin',(27.8205867452275,-1.59894781082744,15.7235432561772));
#55884=CARTESIAN_POINT('Origin',(27.5523768849771,-1.4192734698133,15.7235432561772));
#55885=CARTESIAN_POINT('',(27.6887394991444,-1.40162446254801,15.7235432561772));
#55886=CARTESIAN_POINT('Origin',(27.690504399871,-1.41526072396474,15.7235432561772));
#55887=CARTESIAN_POINT('',(27.701853149596,-1.42302399516179,15.7235432561772));
#55888=CARTESIAN_POINT('Origin',(27.701853149596,-1.42302399516179,15.7235432561772));
#55889=CARTESIAN_POINT('Origin',(27.4485671771557,-1.22286002707717,15.7235432561772));
#55890=CARTESIAN_POINT('',(27.5858941560428,-1.21596431320988,15.7235432561772));
#55891=CARTESIAN_POINT('Origin',(27.5865837274296,-1.22969701109859,15.7235432561772));
#55892=CARTESIAN_POINT('',(27.5972883935086,-1.23832676336246,15.7235432561772));
#55893=CARTESIAN_POINT('Origin',(27.5972883935086,-1.23832676336246,15.7235432561772));
#55894=CARTESIAN_POINT('Origin',(27.3604879011247,-1.01890724563189,15.7235432561772));
#55895=CARTESIAN_POINT('',(27.4979325782409,-1.02280733953164,15.7235432561772));
#55896=CARTESIAN_POINT('Origin',(27.4975425688509,-1.03655180724326,15.7235432561772));
#55897=CARTESIAN_POINT('',(27.507537153458,-1.04599483528157,15.7235432561772));
#55898=CARTESIAN_POINT('Origin',(27.507537153458,-1.04599483528157,15.7235432561772));
#55899=CARTESIAN_POINT('Origin',(27.2886820949101,-0.808672562196254,15.7235432561772));
#55900=CARTESIAN_POINT('',(27.4253970781159,-0.823344418487241,15.7235432561772));
#55901=CARTESIAN_POINT('Origin',(27.4239298924868,-0.837015916807826,15.7235432561772));
#55902=CARTESIAN_POINT('',(27.4331527756843,-0.847214001212589,15.7235432561772));
#55903=CARTESIAN_POINT('Origin',(27.4331527756843,-0.847214001212589,15.7235432561772));
#55904=CARTESIAN_POINT('Origin',(27.233592465185,-0.593452143503757,15.7235432561772));
#55905=CARTESIAN_POINT('',(27.3687348611467,-0.618805305313063,15.7235432561772));
#55906=CARTESIAN_POINT('Origin',(27.3661995449658,-0.632319544909233,15.7235432561772));
#55907=CARTESIAN_POINT('',(27.3745938646118,-0.643209811098888,15.7235432561772));
#55908=CARTESIAN_POINT('Origin',(27.3745938646118,-0.643209811098888,15.7235432561772));
#55909=CARTESIAN_POINT('Origin',(27.195558657836,-0.374572895003696,15.7235432561772));
#55910=CARTESIAN_POINT('',(27.328295268743,-0.410451051657984,15.7235432561772));
#55911=CARTESIAN_POINT('Origin',(27.3247074530776,-0.423724712748689,15.7235432561772));
#55912=CARTESIAN_POINT('',(27.3322214554001,-0.435240018610796,15.7235432561772));
#55913=CARTESIAN_POINT('Origin',(27.3322214554001,-0.435240018610796,15.7235432561772));
#55914=CARTESIAN_POINT('Origin',(27.1748151639327,-0.153384280047813,15.7235432561772));
#55915=CARTESIAN_POINT('',(27.3043276244395,-0.199566230780611,15.7235432561772));
#55916=CARTESIAN_POINT('Origin',(27.2997094293662,-0.212517476831286,15.7235432561772));
#55917=CARTESIAN_POINT('',(27.3062967880422,-0.224586826675978,15.7235432561772));
#55918=CARTESIAN_POINT('Origin',(27.3062967880422,-0.224586826675978,15.7235432561772));
#55919=CARTESIAN_POINT('Origin',(27.1714898740131,0.068750000000016,15.7235432561772));
#55920=CARTESIAN_POINT('Origin',(27.2969796967333,-0.0125489822720016,15.7235432561772));
#55921=CARTESIAN_POINT('Origin',(27.1856032895953,0.29046041343615,15.7235432561772));
#55922=CARTESIAN_POINT('Origin',(27.3043276244395,0.199566230780642,15.7235432561772));
#55923=CARTESIAN_POINT('Origin',(27.217068396779,0.510380041835561,15.7235432561772));
#55924=CARTESIAN_POINT('Origin',(27.328295268743,0.410451051658016,15.7235432561772));
#55925=CARTESIAN_POINT('Origin',(27.2656912027152,0.727153007558468,15.7235432561772));
#55926=CARTESIAN_POINT('Origin',(27.3687348611468,0.618805305313091,15.7235432561772));
#55927=CARTESIAN_POINT('Origin',(27.3311719316367,0.939442833186866,15.7235432561772));
#55928=CARTESIAN_POINT('Origin',(27.4253970781159,0.823344418487269,15.7235432561772));
#55929=CARTESIAN_POINT('Origin',(27.4131068730749,1.14594068135223,15.7235432561772));
#55930=CARTESIAN_POINT('Origin',(27.4979325782409,1.02280733953167,15.7235432561772));
#55931=CARTESIAN_POINT('',(0.,0.,0.));
#55932=CARTESIAN_POINT('Origin',(30.,-1.32966554433622E-14,16.));
#55933=CARTESIAN_POINT('',(29.9999999999999,-1.50000000000001,30.25));
#55934=CARTESIAN_POINT('',(30.,-1.50000000000001,30.3125));
#55935=CARTESIAN_POINT('',(30.,-1.50000000000001,16.));
#55936=CARTESIAN_POINT('',(30.,-1.50000000000002,30.75));
#55937=CARTESIAN_POINT('Ctrl Pts',(29.9999999999999,-1.50000000000001,30.25));
#55938=CARTESIAN_POINT('Ctrl Pts',(30.1658036138247,-1.50000000000003,30.2579772300895));
#55939=CARTESIAN_POINT('Ctrl Pts',(30.3306771390814,-1.47251502213024,30.2666731828795));
#55940=CARTESIAN_POINT('Ctrl Pts',(30.6740051197163,-1.35441705513551,30.2864720571327));
#55941=CARTESIAN_POINT('Ctrl Pts',(30.8456956760641,-1.25440329321601,30.2975106829297));
#55942=CARTESIAN_POINT('Ctrl Pts',(31.1355371924707,-0.998320157723232,
30.31856910982));
#55943=CARTESIAN_POINT('Ctrl Pts',(31.2526807741055,-0.846671576374736,
30.3279626902015));
#55944=CARTESIAN_POINT('Ctrl Pts',(31.4282014939959,-0.499786966349004,
30.3472340574251));
#55945=CARTESIAN_POINT('Ctrl Pts',(31.4817951924464,-0.306278304449559,
30.3579845386417));
#55946=CARTESIAN_POINT('Ctrl Pts',(31.5101111597472,0.0860175204635018,
30.3797787511369));
#55947=CARTESIAN_POINT('Ctrl Pts',(31.4862462216493,0.280921846793951,30.3906067692664));
#55948=CARTESIAN_POINT('Ctrl Pts',(31.3664146176937,0.647698903970874,30.4109832724428));
#55949=CARTESIAN_POINT('Ctrl Pts',(31.2727727808063,0.816486916731949,30.4197772164968));
#55950=CARTESIAN_POINT('Ctrl Pts',(31.0215777110749,1.11639419547156,30.440193602667));
#55951=CARTESIAN_POINT('Ctrl Pts',(30.8638920671928,1.2424306705166,30.4512812699412));
#55952=CARTESIAN_POINT('Ctrl Pts',(30.51519869364,1.4218077371841,30.4730404839947));
#55953=CARTESIAN_POINT('Ctrl Pts',(30.3288784064271,1.47608428096084,30.4835125047644));
#55954=CARTESIAN_POINT('Ctrl Pts',(29.9417076474062,1.51169090841865,30.5031293395779));
#55955=CARTESIAN_POINT('Ctrl Pts',(29.7444133180912,1.49107258678014,30.5125449036674));
#55956=CARTESIAN_POINT('Ctrl Pts',(29.3680874803138,1.37464650826943,30.5338849467157));
#55957=CARTESIAN_POINT('Ctrl Pts',(29.192868275455,1.27964935682832,30.5449539944024));
#55958=CARTESIAN_POINT('Ctrl Pts',(28.8948089362382,1.03185947909864,30.5661774332058));
#55959=CARTESIAN_POINT('Ctrl Pts',(28.7730426891403,0.883581363472215,30.5759121464738));
#55960=CARTESIAN_POINT('Ctrl Pts',(28.5872420086988,0.541893735862482,30.5948947924521));
#55961=CARTESIAN_POINT('Ctrl Pts',(28.5279457886126,0.350092848014275,30.6055503973326));
#55962=CARTESIAN_POINT('Ctrl Pts',(28.4879441501424,-0.0417086531130522,
30.6273171473952));
#55963=CARTESIAN_POINT('Ctrl Pts',(28.5061747163527,-0.237794814766365,
30.6382108230426));
#55964=CARTESIAN_POINT('Ctrl Pts',(28.6154381406337,-0.60772707143957,30.65876261508));
#55965=CARTESIAN_POINT('Ctrl Pts',(28.7037802077497,-0.77855877037785,30.6675955620118));
#55966=CARTESIAN_POINT('Ctrl Pts',(28.9458348287961,-1.08578773838532,30.687775558397));
#55967=CARTESIAN_POINT('Ctrl Pts',(29.1002278810903,-1.21679626071423,30.6988429232091));
#55968=CARTESIAN_POINT('Ctrl Pts',(29.3881527190005,-1.37554036843891,30.7171052719799));
#55969=CARTESIAN_POINT('Ctrl Pts',(29.5080276522,-1.42282651307167,30.7241862614101));
#55970=CARTESIAN_POINT('Ctrl Pts',(29.7526687702711,-1.48465507368766,30.7376740227083));
#55971=CARTESIAN_POINT('Ctrl Pts',(29.8761199631302,-1.50000000000009,30.7440398189472));
#55972=CARTESIAN_POINT('Ctrl Pts',(30.0000000000009,-1.50000000000001,30.75));
#55973=CARTESIAN_POINT('',(30.,-1.50000000000001,30.85));
#55974=CARTESIAN_POINT('',(30.,-1.50000000000001,16.));
#55975=CARTESIAN_POINT('Origin',(30.,-1.32966554433622E-14,30.85));
#55976=CARTESIAN_POINT('',(28.9490560961666,-1.07028823734334,30.75));
#55977=CARTESIAN_POINT('Origin',(30.,-1.5916987375435E-14,30.75));
#55978=CARTESIAN_POINT('Ctrl Pts',(28.9490560961666,-1.07028823734332,30.75));
#55979=CARTESIAN_POINT('Ctrl Pts',(28.8761609488349,-0.998710593084209,
30.7445045626927));
#55980=CARTESIAN_POINT('Ctrl Pts',(28.8107674297946,-0.919873442584925,
30.7391683946938));
#55981=CARTESIAN_POINT('Ctrl Pts',(28.6983154051604,-0.752052754529888,
30.7290963583567));
#55982=CARTESIAN_POINT('Ctrl Pts',(28.6511686993163,-0.663795554008335,
30.7243775307781));
#55983=CARTESIAN_POINT('Ctrl Pts',(28.5395598759442,-0.392939439769756,
30.709329968876));
#55984=CARTESIAN_POINT('Ctrl Pts',(28.5011631241701,-0.201888114570883,
30.6987160063649));
#55985=CARTESIAN_POINT('Ctrl Pts',(28.4988436150777,0.191908857459164,30.6768383968077));
#55986=CARTESIAN_POINT('Ctrl Pts',(28.5379718270057,0.390884408078152,30.6657841995511));
#55987=CARTESIAN_POINT('Ctrl Pts',(28.6882496652404,0.752033457565058,30.6457203634686));
#55988=CARTESIAN_POINT('Ctrl Pts',(28.7941652988744,0.912256576314666,30.6368419553212));
#55989=CARTESIAN_POINT('Ctrl Pts',(29.0637866570552,1.18813740110581,30.6162064354332));
#55990=CARTESIAN_POINT('Ctrl Pts',(29.2263162356668,1.29983562680085,30.6052839989448));
#55991=CARTESIAN_POINT('Ctrl Pts',(29.5881540142218,1.45598200117754,30.5835376714189));
#55992=CARTESIAN_POINT('Ctrl Pts',(29.7845106480132,1.49769538170803,30.5729317534561));
#55993=CARTESIAN_POINT('Ctrl Pts',(30.1735918421599,1.5020241460186,30.5540918323215));
#55994=CARTESIAN_POINT('Ctrl Pts',(30.3626153088868,1.46791385953203,30.544162381137));
#55995=CARTESIAN_POINT('Ctrl Pts',(30.7246797057952,1.32812661690519,30.5228595707569));
#55996=CARTESIAN_POINT('Ctrl Pts',(30.8932233177541,1.2211620663456,30.5117792749302));
#55997=CARTESIAN_POINT('Ctrl Pts',(31.1776737025205,0.949411483501645,30.4905450221109));
#55998=CARTESIAN_POINT('Ctrl Pts',(31.2913339229655,0.787872571372875,30.4812706984095));
#55999=CARTESIAN_POINT('Ctrl Pts',(31.4489779041399,0.433069950768308,30.4615594417092));
#56000=CARTESIAN_POINT('Ctrl Pts',(31.4925441992832,0.243681023738972,30.451037834652));
#56001=CARTESIAN_POINT('Ctrl Pts',(31.5059639907605,-0.148777135728896,
30.4292346035705));
#56002=CARTESIAN_POINT('Ctrl Pts',(31.4726973264507,-0.348194823891665,
30.418155843117));
#56003=CARTESIAN_POINT('Ctrl Pts',(31.3331360295961,-0.713588890875335,
30.3978561727291));
#56004=CARTESIAN_POINT('Ctrl Pts',(31.2315888806866,-0.877298264710928,
30.3890521180742));
#56005=CARTESIAN_POINT('Ctrl Pts',(30.969887909143,-1.16071911064266,30.3685882229343));
#56006=CARTESIAN_POINT('Ctrl Pts',(30.8111118646049,-1.27673016594729,30.3577265776157));
#56007=CARTESIAN_POINT('Ctrl Pts',(30.4544959445291,-1.44324278722566,30.3359435355702));
#56008=CARTESIAN_POINT('Ctrl Pts',(30.2594138454525,-1.49071962728781,30.3252388425894));
#56009=CARTESIAN_POINT('Ctrl Pts',(30.0404799678322,-1.49959063127059,30.3144589647139));
#56010=CARTESIAN_POINT('Ctrl Pts',(30.0202329450965,-1.50000000000001,30.3134734580248));
#56011=CARTESIAN_POINT('Ctrl Pts',(30.,-1.50000000000001,30.3125));
#56012=CARTESIAN_POINT('Origin',(30.,-1.32966554433622E-14,16.));
#56013=CARTESIAN_POINT('',(30.0000000422953,-1.50000000000001,29.7500000040699));
#56014=CARTESIAN_POINT('',(30.0000000000001,-1.50000000000001,29.8125));
#56015=CARTESIAN_POINT('',(30.,-1.50000000000001,16.));
#56016=CARTESIAN_POINT('Ctrl Pts',(30.0000000423936,-1.50000000000001,29.7500000020397));
#56017=CARTESIAN_POINT('Ctrl Pts',(30.195284159332,-1.49999999448081,29.7593956136499));
#56018=CARTESIAN_POINT('Ctrl Pts',(30.3888046451199,-1.46186371850976,29.7697657133627));
#56019=CARTESIAN_POINT('Ctrl Pts',(30.7506676874449,-1.3133124636612,29.7913022808498));
#56020=CARTESIAN_POINT('Ctrl Pts',(30.9154176613495,-1.20428706546983,29.8022573009481));
#56021=CARTESIAN_POINT('Ctrl Pts',(31.18981388205,-0.933008136594988,29.8229947210741));
#56022=CARTESIAN_POINT('Ctrl Pts',(31.2983679232815,-0.774850228387389,
29.8319527650896));
#56023=CARTESIAN_POINT('Ctrl Pts',(31.4541476549185,-0.418353419581691,
29.8517581433566));
#56024=CARTESIAN_POINT('Ctrl Pts',(31.4967395542031,-0.22207441884915,29.8626625322862));
#56025=CARTESIAN_POINT('Ctrl Pts',(31.5028167108854,0.170195075492689,29.8844552819718));
#56026=CARTESIAN_POINT('Ctrl Pts',(31.4683656451658,0.362410265994727,29.8951339036664));
#56027=CARTESIAN_POINT('Ctrl Pts',(31.3284167977355,0.722950513431523,29.9151639174129));
#56028=CARTESIAN_POINT('Ctrl Pts',(31.2243440361084,0.887881539566768,29.9240904295301));
#56029=CARTESIAN_POINT('Ctrl Pts',(30.9555499935672,1.17320843290826,29.9449485359688));
#56030=CARTESIAN_POINT('Ctrl Pts',(30.7918896841479,1.28933944326239,29.9560485076758));
#56031=CARTESIAN_POINT('Ctrl Pts',(30.4356884609645,1.44801470954154,29.9775938933022));
#56032=CARTESIAN_POINT('Ctrl Pts',(30.24769400318,1.49172420709908,29.9878529335795));
#56033=CARTESIAN_POINT('Ctrl Pts',(29.8564383086953,1.50648133745832,30.007087152245));
#56034=CARTESIAN_POINT('Ctrl Pts',(29.6568006042803,1.4738887523207,30.0172375010609));
#56035=CARTESIAN_POINT('Ctrl Pts',(29.2858871639067,1.33362042993594,30.0389794245699));
#56036=CARTESIAN_POINT('Ctrl Pts',(29.1177424716204,1.22887149382963,30.049978982519));
#56037=CARTESIAN_POINT('Ctrl Pts',(28.8358984689122,0.964859074366596,30.0708728867402));
#56038=CARTESIAN_POINT('Ctrl Pts',(28.7232154667205,0.809870978335536,30.0800071678703));
#56039=CARTESIAN_POINT('Ctrl Pts',(28.5578456280088,0.457982195266601,30.0995565447074));
#56040=CARTESIAN_POINT('Ctrl Pts',(28.5099042682065,0.262965364708001,30.1103908130718));
#56041=CARTESIAN_POINT('Ctrl Pts',(28.4930631778567,-0.129475272168894,
30.1321930706761));
#56042=CARTESIAN_POINT('Ctrl Pts',(28.5224126203679,-0.323064053208287,
30.142948002956));
#56043=CARTESIAN_POINT('Ctrl Pts',(28.6526173206986,-0.686662322858743,
30.1631479068255));
#56044=CARTESIAN_POINT('Ctrl Pts',(28.7515795011674,-0.85345907766542,30.1719758706799));
#56045=CARTESIAN_POINT('Ctrl Pts',(29.0118186458561,-1.14595641051804,30.1926215582791));
#56046=CARTESIAN_POINT('Ctrl Pts',(29.172636650331,-1.26695599442051,30.2037200176798));
#56047=CARTESIAN_POINT('Ctrl Pts',(29.5253217759949,-1.43577307549295,30.2253779520631));
#56048=CARTESIAN_POINT('Ctrl Pts',(29.7125728326969,-1.48464476779679,30.2357446197376));
#56049=CARTESIAN_POINT('Ctrl Pts',(29.9359811243456,-1.49897644179293,30.2468914582366));
#56050=CARTESIAN_POINT('Ctrl Pts',(29.9680065223165,-1.50000000000001,30.2484607130873));
#56051=CARTESIAN_POINT('Ctrl Pts',(29.9999999999999,-1.50000000000001,30.25));
#56052=CARTESIAN_POINT('Ctrl Pts',(30.,-1.50000000000001,30.3125));
#56053=CARTESIAN_POINT('Ctrl Pts',(29.8305649734084,-1.50000000000001,30.3043480534823));
#56054=CARTESIAN_POINT('Ctrl Pts',(29.6621927434306,-1.471296371185,30.2954499177677));
#56055=CARTESIAN_POINT('Ctrl Pts',(29.3161242189391,-1.34950305066004,30.2754165403276));
#56056=CARTESIAN_POINT('Ctrl Pts',(29.1449154106261,-1.2480688680691,30.264361636514));
#56057=CARTESIAN_POINT('Ctrl Pts',(28.8512754656375,-0.984586302069753,
30.242914917907));
#56058=CARTESIAN_POINT('Ctrl Pts',(28.7318299827785,-0.825047829175388,
30.2333359905097));
#56059=CARTESIAN_POINT('Ctrl Pts',(28.5638630976012,-0.47370253085421,30.2138168072696));
#56060=CARTESIAN_POINT('Ctrl Pts',(28.5150825240157,-0.286153024679847,
30.2033973902599));
#56061=CARTESIAN_POINT('Ctrl Pts',(28.4904050702493,0.104624550291977,30.1816875249837));
#56062=CARTESIAN_POINT('Ctrl Pts',(28.5176966903753,0.304322584656878,30.1705931897412));
#56063=CARTESIAN_POINT('Ctrl Pts',(28.6462704703314,0.673930577459572,30.1500594123633));
#56064=CARTESIAN_POINT('Ctrl Pts',(28.7433931121189,0.841252262459088,30.141257075347));
#56065=CARTESIAN_POINT('Ctrl Pts',(28.9970706151381,1.13219704351489,30.1209702113185));
#56066=CARTESIAN_POINT('Ctrl Pts',(29.1519620886259,1.25242080149054,30.1101784429931));
#56067=CARTESIAN_POINT('Ctrl Pts',(29.5030294160994,1.42917820121841,30.0883777805545));
#56068=CARTESIAN_POINT('Ctrl Pts',(29.696654967539,1.48240812812318,30.0775833577866));
#56069=CARTESIAN_POINT('Ctrl Pts',(30.0844620336651,1.50960977413546,30.0581693803401));
#56070=CARTESIAN_POINT('Ctrl Pts',(30.2746950762916,1.48681483093204,30.0489174722834));
#56071=CARTESIAN_POINT('Ctrl Pts',(30.642872277816,1.3694262764412,30.0279427452356));
#56072=CARTESIAN_POINT('Ctrl Pts',(30.8165454300566,1.27352463490858,30.0169229573155));
#56073=CARTESIAN_POINT('Ctrl Pts',(31.1192034235311,1.01839257572982,29.9952743161713));
#56074=CARTESIAN_POINT('Ctrl Pts',(31.2444516003803,0.860842115189833,29.9853245619549));
#56075=CARTESIAN_POINT('Ctrl Pts',(31.4225185229473,0.51295924874081,29.9659977360411));
#56076=CARTESIAN_POINT('Ctrl Pts',(31.476317491186,0.327339595503408,29.9556855330835));
#56077=CARTESIAN_POINT('Ctrl Pts',(31.5118899575654,-0.0614966036299657,
29.9340835220205));
#56078=CARTESIAN_POINT('Ctrl Pts',(31.49041063713,-0.261302093346022,29.9229832170363));
#56079=CARTESIAN_POINT('Ctrl Pts',(31.3726040951777,-0.63490434793495,29.9022275362258));
#56080=CARTESIAN_POINT('Ctrl Pts',(31.2797800327084,-0.805795593106099,
29.8933569012793));
#56081=CARTESIAN_POINT('Ctrl Pts',(31.0338687856651,-1.10392432463312,29.873244137236));
#56082=CARTESIAN_POINT('Ctrl Pts',(30.8828092373533,-1.22807490132932,29.8625276541988));
#56083=CARTESIAN_POINT('Ctrl Pts',(30.5373473005298,-1.41449618106684,29.8407282401322));
#56084=CARTESIAN_POINT('Ctrl Pts',(30.3452845785499,-1.47320733373471,29.8298567527606));
#56085=CARTESIAN_POINT('Ctrl Pts',(30.0982962322989,-1.49758712755237,29.8172963039161));
#56086=CARTESIAN_POINT('Ctrl Pts',(30.0491225084885,-1.50000000000001,29.8148634077916));
#56087=CARTESIAN_POINT('Ctrl Pts',(30.0000000000002,-1.50000000000001,29.8125));
#56088=CARTESIAN_POINT('Origin',(30.,-1.32966554433622E-14,16.));
#56089=CARTESIAN_POINT('',(30.,-1.50000000000001,29.25));
#56090=CARTESIAN_POINT('',(30.,-1.50000000000001,29.3125));
#56091=CARTESIAN_POINT('',(30.,-1.50000000000001,16.));
#56092=CARTESIAN_POINT('Ctrl Pts',(30.0000000000001,-1.50000000000001,29.25));
#56093=CARTESIAN_POINT('Ctrl Pts',(30.0257058009192,-1.50000000000001,29.2512367709234));
#56094=CARTESIAN_POINT('Ctrl Pts',(30.0514327409082,-1.49933922123128,29.2524929138666));
#56095=CARTESIAN_POINT('Ctrl Pts',(30.2757518694164,-1.4877855903611,29.2636064071598));
#56096=CARTESIAN_POINT('Ctrl Pts',(30.4703136581261,-1.43816783024051,29.2743455366981));
#56097=CARTESIAN_POINT('Ctrl Pts',(30.8249043497727,-1.26783071251083,29.2961373759079));
#56098=CARTESIAN_POINT('Ctrl Pts',(30.9822510518058,-1.15024113589767,29.3069740997672));
#56099=CARTESIAN_POINT('Ctrl Pts',(31.2409808029183,-0.864020908483806,
29.3273728025942));
#56100=CARTESIAN_POINT('Ctrl Pts',(31.3408899715229,-0.698983488656709,
29.3361675839636));
#56101=CARTESIAN_POINT('Ctrl Pts',(31.4763980403227,-0.332018378933428,
29.3565545345038));
#56102=CARTESIAN_POINT('Ctrl Pts',(31.5074559153656,-0.132477013527386,
29.3676401659153));
#56103=CARTESIAN_POINT('Ctrl Pts',(31.4898677318573,0.259397054955175,29.3894109474976));
#56104=CARTESIAN_POINT('Ctrl Pts',(31.444367356687,0.448123046557066,29.3998957248088));
#56105=CARTESIAN_POINT('Ctrl Pts',(31.2829132867175,0.801659109129801,29.419536617174));
#56106=CARTESIAN_POINT('Ctrl Pts',(31.1671346623852,0.962462537199801,29.4289146111855));
#56107=CARTESIAN_POINT('Ctrl Pts',(30.8792964511142,1.23119218867364,29.4502279461232));
#56108=CARTESIAN_POINT('Ctrl Pts',(30.7097525390342,1.33613064071083,29.4613000883974));
#56109=CARTESIAN_POINT('Ctrl Pts',(30.346523773562,1.47177468007876,29.4825438305068));
#56110=CARTESIAN_POINT('Ctrl Pts',(30.1572989096959,1.50379960302192,29.4923264081504));
#56111=CARTESIAN_POINT('Ctrl Pts',(29.7684168962525,1.49529312487305,29.5112727938055));
#56112=CARTESIAN_POINT('Ctrl Pts',(29.5725063077327,1.45146676708809,29.5219159452176));
#56113=CARTESIAN_POINT('Ctrl Pts',(29.2125442219205,1.29150806105852,29.5436779265358));
#56114=CARTESIAN_POINT('Ctrl Pts',(29.051374885103,1.17821798386326,29.5545791364576));
#56115=CARTESIAN_POINT('Ctrl Pts',(28.784644635234,0.899571593555892,29.5751523790963));
#56116=CARTESIAN_POINT('Ctrl Pts',(28.6803243600253,0.738084850822973,29.5839952860653));
#56117=CARTESIAN_POINT('Ctrl Pts',(28.5339435846744,0.375376943196454,29.6041457253779));
#56118=CARTESIAN_POINT('Ctrl Pts',(28.4969501646145,0.176221200716502,29.6152099332935));
#56119=CARTESIAN_POINT('Ctrl Pts',(28.5033188891713,-0.217123692718195,
29.6370624273732));
#56120=CARTESIAN_POINT('Ctrl Pts',(28.5436046203998,-0.407585858885439,
29.6476436588269));
#56121=CARTESIAN_POINT('Ctrl Pts',(28.6948329707667,-0.764496194056087,
29.6674720107808));
#56122=CARTESIAN_POINT('Ctrl Pts',(28.8049699824855,-0.927268122072015,
29.6765948726435));
#56123=CARTESIAN_POINT('Ctrl Pts',(29.0837280295094,-1.20402609540407,29.6976943469156));
#56124=CARTESIAN_POINT('Ctrl Pts',(29.2505451199729,-1.31436112105669,29.7087851997463));
#56125=CARTESIAN_POINT('Ctrl Pts',(29.6105129505334,-1.46104267840857,29.7301786477734));
#56126=CARTESIAN_POINT('Ctrl Pts',(29.799201008928,-1.49868271487424,29.7403024627842));
#56127=CARTESIAN_POINT('Ctrl Pts',(29.9932712661576,-1.49998868274459,29.7496759492739));
#56128=CARTESIAN_POINT('Ctrl Pts',(29.9966359009771,-1.50000000009509,29.7498381447076));
#56129=CARTESIAN_POINT('Ctrl Pts',(30.0000000423936,-1.50000000000001,29.7500000020397));
#56130=CARTESIAN_POINT('Ctrl Pts',(30.0000000000002,-1.50000000000001,29.8125));
#56131=CARTESIAN_POINT('Ctrl Pts',(29.8597537134085,-1.50000000000001,29.8057523973903));
#56132=CARTESIAN_POINT('Ctrl Pts',(29.7199776172616,-1.48033650865739,29.798481208736));
#56133=CARTESIAN_POINT('Ctrl Pts',(29.396444095828,-1.38712528602054,29.7803259942996));
#56134=CARTESIAN_POINT('Ctrl Pts',(29.2206000446906,-1.29650603057681,29.7693484919046));
#56135=CARTESIAN_POINT('Ctrl Pts',(28.911420128637,-1.05097346611518,29.747652717245));
#56136=CARTESIAN_POINT('Ctrl Pts',(28.7818724475201,-0.897590413872414,
29.737366134104));
#56137=CARTESIAN_POINT('Ctrl Pts',(28.5939020851709,-0.556198210295242,
29.7183999005719));
#56138=CARTESIAN_POINT('Ctrl Pts',(28.5345980064858,-0.372882477899534,
29.7082156932166));
#56139=CARTESIAN_POINT('Ctrl Pts',(28.4870031451474,0.0134445146485481,
29.6867530825195));
#56140=CARTESIAN_POINT('Ctrl Pts',(28.502033993864,0.213177772539474,29.6756567904145));
#56141=CARTESIAN_POINT('Ctrl Pts',(28.6077791980133,0.591085049341038,29.6546619417033));
#56142=CARTESIAN_POINT('Ctrl Pts',(28.6958240597398,0.766015662165753,29.6456356480104));
#56143=CARTESIAN_POINT('Ctrl Pts',(28.9331445661562,1.07197536298372,29.6257186792435));
#56144=CARTESIAN_POINT('Ctrl Pts',(29.079894739921,1.20029258347643,29.6150937909803));
#56145=CARTESIAN_POINT('Ctrl Pts',(29.4205899711736,1.39807482372058,29.5932081329061));
#56146=CARTESIAN_POINT('Ctrl Pts',(29.6127784235583,1.46301280498413,29.5821576288666));
#56147=CARTESIAN_POINT('Ctrl Pts',(30.000882127086,1.51202551870596,29.5621235164545));
#56148=CARTESIAN_POINT('Ctrl Pts',(30.1924980276144,1.49972435337029,29.5532307774773));
#56149=CARTESIAN_POINT('Ctrl Pts',(30.565900986819,1.40283604422102,29.5325740773055));
#56150=CARTESIAN_POINT('Ctrl Pts',(30.7436552900603,1.31725598082702,29.5216446454201));
#56151=CARTESIAN_POINT('Ctrl Pts',(31.0589827795059,1.08076551025951,29.4999042647726));
#56152=CARTESIAN_POINT('Ctrl Pts',(31.1927323157941,0.931082658468895,29.4893113802134));
#56153=CARTESIAN_POINT('Ctrl Pts',(31.3898152208091,0.595521362119493,29.470508077404));
#56154=CARTESIAN_POINT('Ctrl Pts',(31.454132752542,0.414466978649508,29.4605259432583));
#56155=CARTESIAN_POINT('Ctrl Pts',(31.5126702779257,0.0306540870738048,
29.4392030048374));
#56156=CARTESIAN_POINT('Ctrl Pts',(31.5035323460368,-0.168835937693657,
29.4281202256837));
#56157=CARTESIAN_POINT('Ctrl Pts',(31.4089367798935,-0.550558804938134,
29.4069133997257));
#56158=CARTESIAN_POINT('Ctrl Pts',(31.3252882833553,-0.729258932876967,
29.3976724363492));
#56159=CARTESIAN_POINT('Ctrl Pts',(31.095809753143,-1.04226364925314,29.3779370699617));
#56160=CARTESIAN_POINT('Ctrl Pts',(30.9530486497371,-1.17422022183269,29.3674030128222));
#56161=CARTESIAN_POINT('Ctrl Pts',(30.6189939852,-1.38091973480463,29.3455891471428));
#56162=CARTESIAN_POINT('Ctrl Pts',(30.429320489981,-1.45113472826307,29.3345130603643));
#56163=CARTESIAN_POINT('Ctrl Pts',(30.1547092959792,-1.49402062264703,29.3201095482887));
#56164=CARTESIAN_POINT('Ctrl Pts',(30.0773321028638,-1.50000000000001,29.3162206425338));
#56165=CARTESIAN_POINT('Ctrl Pts',(30.,-1.50000000000001,29.3125));
#56166=CARTESIAN_POINT('Origin',(30.,-1.32966554433622E-14,16.));
#56167=CARTESIAN_POINT('',(30.0000000000001,-1.50000000000001,28.75));
#56168=CARTESIAN_POINT('',(30.,-1.50000000000001,28.8125));
#56169=CARTESIAN_POINT('',(30.,-1.50000000000001,16.));
#56170=CARTESIAN_POINT('Ctrl Pts',(30.0000000000002,-1.50000000000001,28.75));
#56171=CARTESIAN_POINT('Ctrl Pts',(30.0540853804301,-1.50000000000001,28.7526021840792));
#56172=CARTESIAN_POINT('Ctrl Pts',(30.1082259230801,-1.49707499170992,28.7552882723823));
#56173=CARTESIAN_POINT('Ctrl Pts',(30.3599293953789,-1.46969892581938,28.7681588076143));
#56174=CARTESIAN_POINT('Ctrl Pts',(30.551406195325,-1.40907643365525,28.7790551975627));
#56175=CARTESIAN_POINT('Ctrl Pts',(30.8948389562126,-1.21930777033508,28.8008499657338));
#56176=CARTESIAN_POINT('Ctrl Pts',(31.0445316684251,-1.09380802186036,28.8115381638324));
#56177=CARTESIAN_POINT('Ctrl Pts',(31.2877030940359,-0.793168713090864,
28.8315888464123));
#56178=CARTESIAN_POINT('Ctrl Pts',(31.379006293082,-0.620999590881335,28.8405000227289));
#56179=CARTESIAN_POINT('Ctrl Pts',(31.4929834420294,-0.246010850263539,
28.861332730541));
#56180=CARTESIAN_POINT('Ctrl Pts',(31.5124077516471,-0.0462064671363202,
28.872432974048));
#56181=CARTESIAN_POINT('Ctrl Pts',(31.472996504913,0.34187077296362,28.8939928207202));
#56182=CARTESIAN_POINT('Ctrl Pts',(31.4174359900152,0.526774847879437,28.9042652693267));
#56183=CARTESIAN_POINT('Ctrl Pts',(31.2357811865968,0.873408443354475,28.9235226912975));
#56184=CARTESIAN_POINT('Ctrl Pts',(31.1084372252019,1.03024288184359,28.9336214802999));
#56185=CARTESIAN_POINT('Ctrl Pts',(30.8025714917792,1.28234443647017,28.9553402732223));
#56186=CARTESIAN_POINT('Ctrl Pts',(30.6280587815183,1.37625325113107,28.9663450980946));
#56187=CARTESIAN_POINT('Ctrl Pts',(30.2588396849677,1.48965870484553,28.9872593116519));
#56188=CARTESIAN_POINT('Ctrl Pts',(30.068359262301,1.51042753130005,28.996421409812));
#56189=CARTESIAN_POINT('Ctrl Pts',(29.6808324457,1.4790834395187,29.015936971685));
#56190=CARTESIAN_POINT('Ctrl Pts',(29.4877765738488,1.42378431516532,29.0267614634377));
#56191=CARTESIAN_POINT('Ctrl Pts',(29.1387883585853,1.24336756773843,29.0485637430906));
#56192=CARTESIAN_POINT('Ctrl Pts',(28.9853282851658,1.12165139698337,29.0593280990587));
#56193=CARTESIAN_POINT('Ctrl Pts',(28.7345675292747,0.827996981331758,29.0795498986531));
#56194=CARTESIAN_POINT('Ctrl Pts',(28.6390572969471,0.659343561113025,29.0883698021604));
#56195=CARTESIAN_POINT('Ctrl Pts',(28.5145121329283,0.288224890453508,29.108987506086));
#56196=CARTESIAN_POINT('Ctrl Pts',(28.4894007489509,0.0884674237606763,
29.1200851431244));
#56197=CARTESIAN_POINT('Ctrl Pts',(28.5181714945435,-0.301617414497863,
29.1417565230277));
#56198=CARTESIAN_POINT('Ctrl Pts',(28.5688407456957,-0.488459284239858,
29.1521366269022));
#56199=CARTESIAN_POINT('Ctrl Pts',(28.7405885892344,-0.838517734954907,
29.1715843186086));
#56200=CARTESIAN_POINT('Ctrl Pts',(28.8621896492638,-0.99731625641509,29.1812936366545));
#56201=CARTESIAN_POINT('Ctrl Pts',(29.1592029920166,-1.25770358504828,29.2028166791214));
#56202=CARTESIAN_POINT('Ctrl Pts',(29.3313514615525,-1.35708034159287,29.2138596416832));
#56203=CARTESIAN_POINT('Ctrl Pts',(29.6732716198879,-1.47316539526991,29.2335348677957));
#56204=CARTESIAN_POINT('Ctrl Pts',(29.836171069295,-1.50000000000001,29.2421177768964));
#56205=CARTESIAN_POINT('Ctrl Pts',(30.0000000000001,-1.50000000000001,29.25));
#56206=CARTESIAN_POINT('Ctrl Pts',(30.,-1.50000000000001,29.3125));
#56207=CARTESIAN_POINT('Ctrl Pts',(29.8873008443269,-1.50000000000001,29.3070777593446));
#56208=CARTESIAN_POINT('Ctrl Pts',(29.7747317592542,-1.48730209620256,29.3013090571639));
#56209=CARTESIAN_POINT('Ctrl Pts',(29.4744632015876,-1.41837586794508,29.2849477619958));
#56210=CARTESIAN_POINT('Ctrl Pts',(29.294837753903,-1.33817655775596,29.2740777699983));
#56211=CARTESIAN_POINT('Ctrl Pts',(28.9731315511867,-1.11133054751215,29.2522983950411));
#56212=CARTESIAN_POINT('Ctrl Pts',(28.8350302040853,-0.965600487241644,
29.241605933651));
#56213=CARTESIAN_POINT('Ctrl Pts',(28.6283822605559,-0.636211572057215,
29.2225138877439));
#56214=CARTESIAN_POINT('Ctrl Pts',(28.5588803689078,-0.457503373167084,
29.2129168540649));
#56215=CARTESIAN_POINT('Ctrl Pts',(28.4890373687744,-0.0765943370343735,
29.1917552409464));
#56216=CARTESIAN_POINT('Ctrl Pts',(28.4920613555339,0.122462822378066,29.1806965098678));
#56217=CARTESIAN_POINT('Ctrl Pts',(28.5749385187676,0.508021327520356,29.1592765929154));
#56218=CARTESIAN_POINT('Ctrl Pts',(28.6539760022703,0.690715131611738,29.1497407450183));
#56219=CARTESIAN_POINT('Ctrl Pts',(28.8753117279029,1.01093295253508,29.1301967854836));
#56220=CARTESIAN_POINT('Ctrl Pts',(29.0138845897616,1.14650161502305,29.1197638993787));
#56221=CARTESIAN_POINT('Ctrl Pts',(29.3408853293963,1.36213850199283,29.0980411554306));
#56222=CARTESIAN_POINT('Ctrl Pts',(29.5278326261113,1.43768005817386,29.0869482728631));
#56223=CARTESIAN_POINT('Ctrl Pts',(29.9124519842907,1.50965487695232,29.0664439648431));
#56224=CARTESIAN_POINT('Ctrl Pts',(30.1057978761999,1.50848592114141,29.0576455173396));
#56225=CARTESIAN_POINT('Ctrl Pts',(30.4842893221004,1.43290905070853,29.0373359816462));
#56226=CARTESIAN_POINT('Ctrl Pts',(30.6656448486515,1.3581864320247,29.02653488151));
#56227=CARTESIAN_POINT('Ctrl Pts',(30.9934995933557,1.14126552935963,29.0047353821212));
#56228=CARTESIAN_POINT('Ctrl Pts',(31.1358790692293,0.999664672511309,28.9939517892597));
#56229=CARTESIAN_POINT('Ctrl Pts',(31.3521306759684,0.67660748989115,28.974573568351));
#56230=CARTESIAN_POINT('Ctrl Pts',(31.426848104494,0.500181082019829,28.9652878378899));
#56231=CARTESIAN_POINT('Ctrl Pts',(31.5078778462889,0.122255781263764,28.9442919878479));
#56232=CARTESIAN_POINT('Ctrl Pts',(31.5109056485428,-0.0761896933508503,
28.9332672392582));
#56233=CARTESIAN_POINT('Ctrl Pts',(31.4398008862795,-0.46541654048851,28.9116435255283));
#56234=CARTESIAN_POINT('Ctrl Pts',(31.3653977766762,-0.65214948337147,28.9017441343992));
#56235=CARTESIAN_POINT('Ctrl Pts',(31.1521444486118,-0.979425287841449,
28.8823929843003));
#56236=CARTESIAN_POINT('Ctrl Pts',(31.0177656624447,-1.1184106596764,28.8720669771632));
#56237=CARTESIAN_POINT('Ctrl Pts',(30.6979072153004,-1.34258973369453,28.8504505839492));
#56238=CARTESIAN_POINT('Ctrl Pts',(30.5137720633169,-1.42326028628083,28.8393505286358));
#56239=CARTESIAN_POINT('Ctrl Pts',(30.2141280739392,-1.48853135114915,28.8231208153399));
#56240=CARTESIAN_POINT('Ctrl Pts',(30.107104215103,-1.50000000000001,28.8176530539518));
#56241=CARTESIAN_POINT('Ctrl Pts',(30.,-1.50000000000001,28.8125));
#56242=CARTESIAN_POINT('Origin',(30.,-1.32966554433622E-14,16.));
#56243=CARTESIAN_POINT('',(30.,-1.50000000000001,28.25));
#56244=CARTESIAN_POINT('',(29.9999999999999,-1.50000000000001,28.3125));
#56245=CARTESIAN_POINT('',(30.,-1.50000000000001,16.));
#56246=CARTESIAN_POINT('Ctrl Pts',(30.,-1.50000000000001,28.25));
#56247=CARTESIAN_POINT('Ctrl Pts',(30.0829658981124,-1.50000000000001,28.2539916986341));
#56248=CARTESIAN_POINT('Ctrl Pts',(30.1659646402018,-1.49311778203419,28.258176150196));
#56249=CARTESIAN_POINT('Ctrl Pts',(30.4454386189069,-1.44623695759697,28.272924593389));
#56250=CARTESIAN_POINT('Ctrl Pts',(30.6341065114148,-1.37401296366571,28.2840081036532));
#56251=CARTESIAN_POINT('Ctrl Pts',(30.9655430066945,-1.16393488515826,28.305789851648));
#56252=CARTESIAN_POINT('Ctrl Pts',(31.1067439460802,-1.03060853555517,28.3162868947229));
#56253=CARTESIAN_POINT('Ctrl Pts',(31.3331794991128,-0.714896180931114,
28.3359510679762));
#56254=CARTESIAN_POINT('Ctrl Pts',(31.4151109522262,-0.5347128589249,28.3452937300598));
#56255=CARTESIAN_POINT('Ctrl Pts',(31.5053441166005,-0.151540941191815,
28.3665810588227));
#56256=CARTESIAN_POINT('Ctrl Pts',(31.5121960357138,0.047808853319833,28.3776560474067));
#56257=CARTESIAN_POINT('Ctrl Pts',(31.4494295470438,0.430548940590616,28.3989193855884));
#56258=CARTESIAN_POINT('Ctrl Pts',(31.3831821322801,0.610720967506089,28.4087494232854));
#56259=CARTESIAN_POINT('Ctrl Pts',(31.1825379493516,0.943999251999173,28.4276606511623));
#56260=CARTESIAN_POINT('Ctrl Pts',(31.047158086339,1.09222920702457,28.4382916166091));
#56261=CARTESIAN_POINT('Ctrl Pts',(30.7294268326579,1.32515752881874,28.4600486998403));
#56262=CARTESIAN_POINT('Ctrl Pts',(30.550958922042,1.4087432384851,28.4709570664618));
#56263=CARTESIAN_POINT('Ctrl Pts',(30.1765920486677,1.5017020595339,28.4915509905286));
#56264=CARTESIAN_POINT('Ctrl Pts',(29.9846796160604,1.51197023290498,28.5004045958464));
#56265=CARTESIAN_POINT('Ctrl Pts',(29.5971747277955,1.45876321333926,28.5205264062414));
#56266=CARTESIAN_POINT('Ctrl Pts',(29.4058997547266,1.39186434368365,28.5315874296089));
#56267=CARTESIAN_POINT('Ctrl Pts',(29.0676327101079,1.19076140439435,28.5534485031393));
#56268=CARTESIAN_POINT('Ctrl Pts',(28.9223466869136,1.06108495094317,28.5640407038963));
#56269=CARTESIAN_POINT('Ctrl Pts',(28.6879155980949,0.752518131365587,28.5838910754598));
#56270=CARTESIAN_POINT('Ctrl Pts',(28.6014862328755,0.576207606788701,28.5929884662895));
#56271=CARTESIAN_POINT('Ctrl Pts',(28.499833643426,0.196881228217823,28.6140621539879));
#56272=CARTESIAN_POINT('Ctrl Pts',(28.4869739372834,-0.00278217893022192,
28.6251545654961));
#56273=CARTESIAN_POINT('Ctrl Pts',(28.5386011115484,-0.388179803466622,
28.646565544637));
#56274=CARTESIAN_POINT('Ctrl Pts',(28.5997438056181,-0.57068109411198,28.6567045052284));
#56275=CARTESIAN_POINT('Ctrl Pts',(28.7910752661536,-0.909939730661663,
28.6755522072589));
#56276=CARTESIAN_POINT('Ctrl Pts',(28.9221594106395,-1.06198129449833,28.6859751842018));
#56277=CARTESIAN_POINT('Ctrl Pts',(29.2336502066539,-1.30423330232361,28.7076910145522));
#56278=CARTESIAN_POINT('Ctrl Pts',(29.4102115046891,-1.39300789458955,28.7186517848609));
#56279=CARTESIAN_POINT('Ctrl Pts',(29.7297304238973,-1.48169043732429,28.7364880499937));
#56280=CARTESIAN_POINT('Ctrl Pts',(29.8646679236608,-1.50000000000001,28.7434888324413));
#56281=CARTESIAN_POINT('Ctrl Pts',(30.0000000000002,-1.50000000000001,28.75));
#56282=CARTESIAN_POINT('Ctrl Pts',(30.,-1.50000000000001,28.8125));
#56283=CARTESIAN_POINT('Ctrl Pts',(29.915383015882,-1.50000000000001,28.8084288634535));
#56284=CARTESIAN_POINT('Ctrl Pts',(29.8307352254749,-1.4928411598692,28.8041573880682));
#56285=CARTESIAN_POINT('Ctrl Pts',(29.5559284168413,-1.44580747389306,28.7896292480462));
#56286=CARTESIAN_POINT('Ctrl Pts',(29.3730572440495,-1.37640415455312,28.7789029846613));
#56287=CARTESIAN_POINT('Ctrl Pts',(29.0395563050654,-1.16922544646275,28.7571024491396));
#56288=CARTESIAN_POINT('Ctrl Pts',(28.8931654598463,-1.03173520870096,28.7462400430439));
#56289=CARTESIAN_POINT('Ctrl Pts',(28.6676984257239,-0.714888535897263,
28.7265909588401));
#56290=CARTESIAN_POINT('Ctrl Pts',(28.5879546245725,-0.540586509645268,
28.7175325838691));
#56291=CARTESIAN_POINT('Ctrl Pts',(28.4963360655409,-0.165582907317607,
28.6966990504065));
#56292=CARTESIAN_POINT('Ctrl Pts',(28.4875887561367,0.032114568158461,28.6857158573245));
#56293=CARTESIAN_POINT('Ctrl Pts',(28.5470557852483,0.422500942588754,28.6640277254117));
#56294=CARTESIAN_POINT('Ctrl Pts',(28.6157998677826,0.611145026803925,28.6537877758344));
#56295=CARTESIAN_POINT('Ctrl Pts',(28.8187186237447,0.943964110383672,28.6347798680923));
#56296=CARTESIAN_POINT('Ctrl Pts',(28.9483973542157,1.08655537048085,28.6245798289275));
#56297=CARTESIAN_POINT('Ctrl Pts',(29.2601643471919,1.31985362966521,28.6030994252846));
#56298=CARTESIAN_POINT('Ctrl Pts',(29.4410566887989,1.40604402433623,28.5920020608114));
#56299=CARTESIAN_POINT('Ctrl Pts',(29.8214920682634,1.50190823479761,28.5710354603478));
#56300=CARTESIAN_POINT('Ctrl Pts',(30.0168727428654,1.5123834847247,28.5620321954671));
#56301=CARTESIAN_POINT('Ctrl Pts',(30.4002098002625,1.45848214178997,28.5420916231679));
#56302=CARTESIAN_POINT('Ctrl Pts',(30.5845472296663,1.39485738401663,28.531455330078));
#56303=CARTESIAN_POINT('Ctrl Pts',(30.9255768985555,1.19735876148644,28.5095614596354));
#56304=CARTESIAN_POINT('Ctrl Pts',(31.0774615143075,1.06275841541511,28.4985150091509));
#56305=CARTESIAN_POINT('Ctrl Pts',(31.3127681711381,0.750226996476014,28.4785123840417));
#56306=CARTESIAN_POINT('Ctrl Pts',(31.3972426471779,0.57785906771898,28.4696032815399));
#56307=CARTESIAN_POINT('Ctrl Pts',(31.4986444188222,0.205636520695856,28.4489242511497));
#56308=CARTESIAN_POINT('Ctrl Pts',(31.5126593744967,0.00877624847217685,
28.4379875693595));
#56309=CARTESIAN_POINT('Ctrl Pts',(31.4639817400215,-0.38243148199871,28.4162538065556));
#56310=CARTESIAN_POINT('Ctrl Pts',(31.4004868863224,-0.572852347631721,
28.405674869576));
#56311=CARTESIAN_POINT('Ctrl Pts',(31.2070793636249,-0.910612756316215,
28.3869104024268));
#56312=CARTESIAN_POINT('Ctrl Pts',(31.0818178721223,-1.05640050494828,28.3768711948362));
#56313=CARTESIAN_POINT('Ctrl Pts',(30.7776023551779,-1.29787423387296,28.3555270153716));
#56314=CARTESIAN_POINT('Ctrl Pts',(30.5998203088742,-1.38901510440857,28.3444417818325));
#56315=CARTESIAN_POINT('Ctrl Pts',(30.2759956104928,-1.48090471471267,28.3263092695923));
#56316=CARTESIAN_POINT('Ctrl Pts',(30.1382050521625,-1.50000000000003,28.3191493936725));
#56317=CARTESIAN_POINT('Ctrl Pts',(29.9999999999998,-1.50000000000001,28.3125));
#56318=CARTESIAN_POINT('Origin',(30.,-1.32966554433622E-14,16.));
#56319=CARTESIAN_POINT('',(30.,-1.50000000000001,27.75));
#56320=CARTESIAN_POINT('',(29.9999999999999,-1.50000000000001,27.8125));
#56321=CARTESIAN_POINT('',(30.,-1.50000000000001,16.));
#56322=CARTESIAN_POINT('Ctrl Pts',(30.,-1.50000000000001,27.75));
#56323=CARTESIAN_POINT('Ctrl Pts',(30.1124415068704,-1.50000000000002,27.7554098445216));
#56324=CARTESIAN_POINT('Ctrl Pts',(30.2247618661566,-1.48736003703784,27.7611649704098));
#56325=CARTESIAN_POINT('Ctrl Pts',(30.5287085515254,-1.41774990238772,27.7777222269793));
#56326=CARTESIAN_POINT('Ctrl Pts',(30.7117935692984,-1.3352484713228,27.7888226154224));
#56327=CARTESIAN_POINT('Ctrl Pts',(31.0290158327245,-1.10803593258209,27.810396438097));
#56328=CARTESIAN_POINT('Ctrl Pts',(31.1618575965723,-0.967846133863366,
27.8206819515156));
#56329=CARTESIAN_POINT('Ctrl Pts',(31.3721629460689,-0.6380210664967,27.8399620797878));
#56330=CARTESIAN_POINT('Ctrl Pts',(31.4448593309443,-0.449797513993593,
27.8500112492227));
#56331=CARTESIAN_POINT('Ctrl Pts',(31.5116357099559,-0.0592694964018678,
27.8717072502));
#56332=CARTESIAN_POINT('Ctrl Pts',(31.5064070816201,0.138907825669745,27.8827171014262));
#56333=CARTESIAN_POINT('Ctrl Pts',(31.4213057895144,0.515720730899333,27.9036511517167));
#56334=CARTESIAN_POINT('Ctrl Pts',(31.3446665574137,0.691326301909506,27.9128415418121));
#56335=CARTESIAN_POINT('Ctrl Pts',(31.1248857141117,1.01202109760975,27.9323239413351));
#56336=CARTESIAN_POINT('Ctrl Pts',(30.9809587395189,1.15206471718701,27.9431387316727));
#56337=CARTESIAN_POINT('Ctrl Pts',(30.6509116511972,1.36527940308072,27.964940759777));
#56338=CARTESIAN_POINT('Ctrl Pts',(30.4689587309927,1.43797198007731,27.9757142119819));
#56339=CARTESIAN_POINT('Ctrl Pts',(30.0895559298121,1.50958056680736,27.9959573651739));
#56340=CARTESIAN_POINT('Ctrl Pts',(29.8958570870542,1.50864454830606,28.0047704518936));
#56341=CARTESIAN_POINT('Ctrl Pts',(29.5119529197823,1.43233602869983,28.0253607308535));
#56342=CARTESIAN_POINT('Ctrl Pts',(29.326059536573,1.35483178794297,28.0364574259998));
#56343=CARTESIAN_POINT('Ctrl Pts',(29.0017503691465,1.13591853977073,28.058141681653));
#56344=CARTESIAN_POINT('Ctrl Pts',(28.8647633102306,0.999035130825837,28.0685347915132));
#56345=CARTESIAN_POINT('Ctrl Pts',(28.6464909172802,0.676130375169667,28.0880060034614));
#56346=CARTESIAN_POINT('Ctrl Pts',(28.5692025798653,0.491914163630282,28.097671435354));
#56347=CARTESIAN_POINT('Ctrl Pts',(28.4907708909632,0.10494838810591,28.1191695339942));
#56348=CARTESIAN_POINT('Ctrl Pts',(28.4900432259905,-0.0938982867387415,
28.1302165714856));
#56349=CARTESIAN_POINT('Ctrl Pts',(28.5641302538219,-0.473688030944453,
28.1513160017192));
#56350=CARTESIAN_POINT('Ctrl Pts',(28.6356001259049,-0.65152593371875,28.1607865563875));
#56351=CARTESIAN_POINT('Ctrl Pts',(28.845875335272,-0.978539657712538,28.1799871416705));
#56352=CARTESIAN_POINT('Ctrl Pts',(28.9856037255401,-1.12272886979256,28.1907150828729));
#56353=CARTESIAN_POINT('Ctrl Pts',(29.3096631032409,-1.34585412683097,28.2125043207586));
#56354=CARTESIAN_POINT('Ctrl Pts',(29.4899597666947,-1.42399330666579,28.2233493807965));
#56355=CARTESIAN_POINT('Ctrl Pts',(29.7854687062271,-1.48848755634025,28.2393585682142));
#56356=CARTESIAN_POINT('Ctrl Pts',(29.8926913234913,-1.50000000000001,28.2448371088943));
#56357=CARTESIAN_POINT('Ctrl Pts',(30.,-1.50000000000001,28.25));
#56358=CARTESIAN_POINT('Ctrl Pts',(29.9999999999998,-1.50000000000001,28.3125));
#56359=CARTESIAN_POINT('Ctrl Pts',(29.9436942937174,-1.50000000000001,28.3097909904434));
#56360=CARTESIAN_POINT('Ctrl Pts',(29.8873283119117,-1.49682992210333,28.3069910231599));
#56361=CARTESIAN_POINT('Ctrl Pts',(29.6396724584349,-1.46877643215582,28.2942964117443));
#56362=CARTESIAN_POINT('Ctrl Pts',(29.4541661443778,-1.41038581308707,28.2837492734071));
#56363=CARTESIAN_POINT('Ctrl Pts',(29.1087260311914,-1.22301113475657,28.2619244260365));
#56364=CARTESIAN_POINT('Ctrl Pts',(28.9535330490943,-1.09318251992373,28.250851349792));
#56365=CARTESIAN_POINT('Ctrl Pts',(28.7092889328235,-0.787692454984111,
28.2306143141317));
#56366=CARTESIAN_POINT('Ctrl Pts',(28.6196840987504,-0.61735395437333,28.2217974419096));
#56367=CARTESIAN_POINT('Ctrl Pts',(28.5078809954767,-0.248171981043882,
28.2012873322802));
#56368=CARTESIAN_POINT('Ctrl Pts',(28.4882926923279,-0.0523550997824531,
28.1904086166545));
#56369=CARTESIAN_POINT('Ctrl Pts',(28.5254878247544,0.339597077669009,28.168633495685));
#56370=CARTESIAN_POINT('Ctrl Pts',(28.5834194437059,0.531823926835376,28.1579542262869));
#56371=CARTESIAN_POINT('Ctrl Pts',(28.7667554264755,0.874769226053054,28.1389017096637));
#56372=CARTESIAN_POINT('Ctrl Pts',(28.8874031082008,1.02385470321529,28.129256101159));
#56373=CARTESIAN_POINT('Ctrl Pts',(29.1834814070674,1.27365788399194,28.1080720501192));
#56374=CARTESIAN_POINT('Ctrl Pts',(29.3578610118793,1.36987818467188,28.0970094213409));
#56375=CARTESIAN_POINT('Ctrl Pts',(29.7335617480327,1.48922788034193,28.0756182419206));
#56376=CARTESIAN_POINT('Ctrl Pts',(29.9311376367095,1.51130087803589,28.0661270552772));
#56377=CARTESIAN_POINT('Ctrl Pts',(30.3188296259211,1.47827076732948,28.0465567126743));
#56378=CARTESIAN_POINT('Ctrl Pts',(30.5053902810264,1.4253063260919,28.0361095744917));
#56379=CARTESIAN_POINT('Ctrl Pts',(30.8550820522802,1.24848731142734,28.0143733820065));
#56380=CARTESIAN_POINT('Ctrl Pts',(31.0135429189334,1.12366789185429,28.0032822239058));
#56381=CARTESIAN_POINT('Ctrl Pts',(31.2669421658592,0.825551327222966,27.9828095312695));
#56382=CARTESIAN_POINT('Ctrl Pts',(31.3618736710286,0.657250577679458,27.9740139209821));
#56383=CARTESIAN_POINT('Ctrl Pts',(31.4842407851538,0.291243414392501,27.9536801896884));
#56384=CARTESIAN_POINT('Ctrl Pts',(31.509450941646,0.0966465287303217,27.9428692515961));
#56385=CARTESIAN_POINT('Ctrl Pts',(31.4839402912682,-0.295715862316101,
27.9210713409824));
#56386=CARTESIAN_POINT('Ctrl Pts',(31.4317236332783,-0.489608696036187,
27.9102995168868));
#56387=CARTESIAN_POINT('Ctrl Pts',(31.2586786377253,-0.837725609348495,
27.8909596883695));
#56388=CARTESIAN_POINT('Ctrl Pts',(31.1426320784322,-0.99018742000189,27.8816363720611));
#56389=CARTESIAN_POINT('Ctrl Pts',(30.8547518896528,-1.24822771259633,27.8606179441152));
#56390=CARTESIAN_POINT('Ctrl Pts',(30.683921012954,-1.3494162779034,27.8495880462471));
#56391=CARTESIAN_POINT('Ctrl Pts',(30.3380948295812,-1.47125624803439,27.8295650326271));
#56392=CARTESIAN_POINT('Ctrl Pts',(30.1695563642114,-1.50000000000003,27.8206577843767));
#56393=CARTESIAN_POINT('Ctrl Pts',(29.9999999999999,-1.50000000000001,27.8125));
#56394=CARTESIAN_POINT('Origin',(30.,-1.32966554433622E-14,16.));
#56395=CARTESIAN_POINT('',(29.9999999999999,-1.50000000000001,27.25));
#56396=CARTESIAN_POINT('',(30.0000000001561,-1.50000000000001,27.312500000015));
#56397=CARTESIAN_POINT('',(30.,-1.50000000000001,16.));
#56398=CARTESIAN_POINT('Ctrl Pts',(29.9999999999998,-1.50000000000001,27.25));
#56399=CARTESIAN_POINT('Ctrl Pts',(30.1442714687728,-1.50000000000004,27.2569412642777));
#56400=CARTESIAN_POINT('Ctrl Pts',(30.2880340149987,-1.4791914741294,27.2644360576155));
#56401=CARTESIAN_POINT('Ctrl Pts',(30.6163114314673,-1.38174334274362,27.2829372047179));
#56402=CARTESIAN_POINT('Ctrl Pts',(30.7927900386128,-1.28861749288707,27.2940148648257));
#56403=CARTESIAN_POINT('Ctrl Pts',(31.0938533402203,-1.04389816914467,27.3152975386708));
#56404=CARTESIAN_POINT('Ctrl Pts',(31.2173213404585,-0.896838599044721,
27.3251756333865));
#56405=CARTESIAN_POINT('Ctrl Pts',(31.4068435879888,-0.557063752560209,
27.3440520137467));
#56406=CARTESIAN_POINT('Ctrl Pts',(31.4681965573585,-0.365925712559008,
27.3546707937468));
#56407=CARTESIAN_POINT('Ctrl Pts',(31.5124404667227,0.0256096349450533,
27.376422757497));
#56408=CARTESIAN_POINT('Ctrl Pts',(31.4962677243898,0.222085336897189,27.3873380742721));
#56409=CARTESIAN_POINT('Ctrl Pts',(31.3908461160845,0.593142920619804,27.4079523844789));
#56410=CARTESIAN_POINT('Ctrl Pts',(31.304401721973,0.764723471695272,27.4168175948822));
#56411=CARTESIAN_POINT('Ctrl Pts',(31.0656503667188,1.07455866625052,27.4369110579998));
#56412=CARTESIAN_POINT('Ctrl Pts',(30.9124772117446,1.20733392111332,27.4479688063785));
#56413=CARTESIAN_POINT('Ctrl Pts',(30.5697179509117,1.40095220523075,27.4698381046742));
#56414=CARTESIAN_POINT('Ctrl Pts',(30.3849139570494,1.46256729268532,27.4804410211816));
#56415=CARTESIAN_POINT('Ctrl Pts',(30.0007344874447,1.51254230178002,27.5003130592281));
#56416=CARTESIAN_POINT('Ctrl Pts',(29.8049569216954,1.49991645600797,27.5093863351468));
#56417=CARTESIAN_POINT('Ctrl Pts',(29.4253565109394,1.3996692288739,27.5304345136228));
#56418=CARTESIAN_POINT('Ctrl Pts',(29.245638701995,1.31157237616612,27.5415283255346));
#56419=CARTESIAN_POINT('Ctrl Pts',(28.9367683949736,1.07514318986943,27.562956332507));
#56420=CARTESIAN_POINT('Ctrl Pts',(28.8087599369318,0.93132448347984,27.5731101063824));
#56421=CARTESIAN_POINT('Ctrl Pts',(28.6094708234815,0.596592375009914,27.591996522448));
#56422=CARTESIAN_POINT('Ctrl Pts',(28.5427132787644,0.407261741609369,27.6023743476884));
#56423=CARTESIAN_POINT('Ctrl Pts',(28.4873635075659,0.0164898797776363,
27.624083895568));
#56424=CARTESIAN_POINT('Ctrl Pts',(28.4981279946982,-0.180903932406258,
27.6350502184671));
#56425=CARTESIAN_POINT('Ctrl Pts',(28.5934885065557,-0.554852956622451,
27.6558251642568));
#56426=CARTESIAN_POINT('Ctrl Pts',(28.6750314181996,-0.72841210507679,27.6648194223046));
#56427=CARTESIAN_POINT('Ctrl Pts',(28.9037835277885,-1.04301134033857,27.6845641309549));
#56428=CARTESIAN_POINT('Ctrl Pts',(29.0515807305306,-1.17900166318454,27.6954525361552));
#56429=CARTESIAN_POINT('Ctrl Pts',(29.3870321030576,-1.38265756586298,27.7172490562487));
#56430=CARTESIAN_POINT('Ctrl Pts',(29.570408592882,-1.45015060314336,27.7279465683201));
#56431=CARTESIAN_POINT('Ctrl Pts',(29.8405845073873,-1.49365112485936,27.7421537608929));
#56432=CARTESIAN_POINT('Ctrl Pts',(29.920314098353,-1.50000000000001,27.7461661102695));
#56433=CARTESIAN_POINT('Ctrl Pts',(30.,-1.50000000000001,27.75));
#56434=CARTESIAN_POINT('Ctrl Pts',(29.9999999999999,-1.50000000000001,27.8125));
#56435=CARTESIAN_POINT('Ctrl Pts',(29.9712572824709,-1.50000000000001,27.8111171153581));
#56436=CARTESIAN_POINT('Ctrl Pts',(29.9424874969812,-1.49917387170699,27.8097099804002));
#56437=CARTESIAN_POINT('Ctrl Pts',(29.7223735770152,-1.48649276547853,27.7987674915373));
#56438=CARTESIAN_POINT('Ctrl Pts',(29.5349257292356,-1.43889608772887,27.7884267728186));
#56439=CARTESIAN_POINT('Ctrl Pts',(29.1813453265204,-1.27257887490163,27.7667952051828));
#56440=CARTESIAN_POINT('Ctrl Pts',(29.0198117779222,-1.15277654761383,27.7556955762776));
#56441=CARTESIAN_POINT('Ctrl Pts',(28.7574522908629,-0.862041024530384,
27.7349968128188));
#56442=CARTESIAN_POINT('Ctrl Pts',(28.6572312223829,-0.695708343276581,
27.7261504635153));
#56443=CARTESIAN_POINT('Ctrl Pts',(28.524605736016,-0.332863036208749,27.7059923909005));
#56444=CARTESIAN_POINT('Ctrl Pts',(28.4939840388333,-0.139603136099824,
27.6952557297833));
#56445=CARTESIAN_POINT('Ctrl Pts',(28.508148989394,0.25282273238934,27.673454292645));
#56446=CARTESIAN_POINT('Ctrl Pts',(28.5547646373704,0.44816718663467,27.6626018229647));
#56447=CARTESIAN_POINT('Ctrl Pts',(28.7177569938957,0.801209312950165,27.6429883715028));
#56448=CARTESIAN_POINT('Ctrl Pts',(28.8294090431484,0.956981758536969,27.6339039237114));
#56449=CARTESIAN_POINT('Ctrl Pts',(29.1093968787388,1.22281551664853,27.6130487316321));
#56450=CARTESIAN_POINT('Ctrl Pts',(29.2767036270498,1.32864238149993,27.6020595468161));
#56451=CARTESIAN_POINT('Ctrl Pts',(29.6469534397504,1.47162694755714,27.5802741008953));
#56452=CARTESIAN_POINT('Ctrl Pts',(29.8468632228895,1.50560128622732,27.570023387908));
#56453=CARTESIAN_POINT('Ctrl Pts',(30.2385607914922,1.49319741260661,27.5508332778069));
#56454=CARTESIAN_POINT('Ctrl Pts',(30.4267058309758,1.45067195878526,27.540599882768));
#56455=CARTESIAN_POINT('Ctrl Pts',(30.7836729511717,1.29433057010809,27.5190824778378));
#56456=CARTESIAN_POINT('Ctrl Pts',(30.9479647504538,1.17932417828325,27.5079833629642));
#56457=CARTESIAN_POINT('Ctrl Pts',(31.2187102492265,0.89565657574078,27.4870774584548));
#56458=CARTESIAN_POINT('Ctrl Pts',(31.3239608540741,0.731149127851972,27.4781193959917));
#56459=CARTESIAN_POINT('Ctrl Pts',(31.4661242989034,0.37131396030254,27.4581285533501));
#56460=CARTESIAN_POINT('Ctrl Pts',(31.5017272578984,0.179429293592902,27.4474682940885));
#56461=CARTESIAN_POINT('Ctrl Pts',(31.4980926781097,-0.21275991516766,27.4256800047129));
#56462=CARTESIAN_POINT('Ctrl Pts',(31.4567210643059,-0.409304691427262,
27.4147608504762));
#56463=CARTESIAN_POINT('Ctrl Pts',(31.3031284414201,-0.766835781066652,
27.394898012163));
#56464=CARTESIAN_POINT('Ctrl Pts',(31.1955054411838,-0.925718941221814,
27.3859710339898));
#56465=CARTESIAN_POINT('Ctrl Pts',(30.9227930606553,-1.19862566676885,27.3652694110877));
#56466=CARTESIAN_POINT('Ctrl Pts',(30.75882230211,-1.30859982122977,27.354325526665));
#56467=CARTESIAN_POINT('Ctrl Pts',(30.3950972752779,-1.46060207029247,27.3326035134561));
#56468=CARTESIAN_POINT('Ctrl Pts',(30.198484714314,-1.4999999999587,27.3220496002711));
#56469=CARTESIAN_POINT('Ctrl Pts',(30.0000000003122,-1.50000000000001,27.312500000015));
#56470=CARTESIAN_POINT('Origin',(30.,-1.32966554433622E-14,16.));
#56471=CARTESIAN_POINT('',(30.,-1.50000000000001,26.75));
#56472=CARTESIAN_POINT('',(30.0000000000001,-1.50000000000001,26.8125));
#56473=CARTESIAN_POINT('',(30.,-1.50000000000001,16.));
#56474=CARTESIAN_POINT('Ctrl Pts',(29.9999999999999,-1.50000000000002,26.75));
#56475=CARTESIAN_POINT('Ctrl Pts',(30.1755630845093,-1.50000000000003,26.7584467828418));
#56476=CARTESIAN_POINT('Ctrl Pts',(30.3499584064833,-1.46918259215549,26.7676934207892));
#56477=CARTESIAN_POINT('Ctrl Pts',(30.6997034276012,-1.3412672085792,26.7880737410627));
#56478=CARTESIAN_POINT('Ctrl Pts',(30.8691431470038,-1.23821435243508,26.7990884927007));
#56479=CARTESIAN_POINT('Ctrl Pts',(31.1538803669515,-0.977054933639417,
26.8200423468827));
#56480=CARTESIAN_POINT('Ctrl Pts',(31.2681733329846,-0.823282264050392,
26.8292620964417));
#56481=CARTESIAN_POINT('Ctrl Pts',(31.4372326110993,-0.473197410553428,
26.8487112549693));
#56482=CARTESIAN_POINT('Ctrl Pts',(31.4872301101415,-0.278708237309613,
26.8595162090384));
#56483=CARTESIAN_POINT('Ctrl Pts',(31.5082331683214,0.113718878171538,26.881317715454));
#56484=CARTESIAN_POINT('Ctrl Pts',(31.4808674747884,0.307802550913579,26.8921001417175));
#56485=CARTESIAN_POINT('Ctrl Pts',(31.3544261384598,0.67256246632588,26.9123645814626));
#56486=CARTESIAN_POINT('Ctrl Pts',(31.2574072539999,0.840081862517357,26.9211719059107));
#56487=CARTESIAN_POINT('Ctrl Pts',(31.0004574791989,1.1352928844589,26.9417347138799));
#56488=CARTESIAN_POINT('Ctrl Pts',(30.8407636896231,1.25813738072432,26.9528303320317));
#56489=CARTESIAN_POINT('Ctrl Pts',(30.4894980147219,1.43081423936239,26.9745271891017));
#56490=CARTESIAN_POINT('Ctrl Pts',(30.302568408204,1.48165789304525,26.984933167702));
#56491=CARTESIAN_POINT('Ctrl Pts',(29.9140424353861,1.51051713966446,27.0044277780243));
#56492=CARTESIAN_POINT('Ctrl Pts',(29.7160053760103,1.48607476032932,27.0140505099305));
#56493=CARTESIAN_POINT('Ctrl Pts',(29.3413420123945,1.36197834203437,27.0355236321475));
#56494=CARTESIAN_POINT('Ctrl Pts',(29.1683424827117,1.26378814603618,27.0465745813446));
#56495=CARTESIAN_POINT('Ctrl Pts',(28.87548492057,1.01073104588063,27.0676940612658));
#56496=CARTESIAN_POINT('Ctrl Pts',(28.7566499301147,0.860326156686485,27.0772041024063));
#56497=CARTESIAN_POINT('Ctrl Pts',(28.5773390955292,0.515342682333064,27.0963698509815));
#56498=CARTESIAN_POINT('Ctrl Pts',(28.5216397715234,0.322442560698391,27.1070865244057));
#56499=CARTESIAN_POINT('Ctrl Pts',(28.4890218615652,-0.0697120082430973,
27.1288728893469));
#56500=CARTESIAN_POINT('Ctrl Pts',(28.510818362855,-0.265069960572926,27.1397261089208));
#56501=CARTESIAN_POINT('Ctrl Pts',(28.6267610927498,-0.633018179794785,
27.1601676766553));
#56502=CARTESIAN_POINT('Ctrl Pts',(28.7184387624141,-0.802555681667626,
27.1689674029211));
#56503=CARTESIAN_POINT('Ctrl Pts',(28.9662614123549,-1.10518359683465,27.1892971067025));
#56504=CARTESIAN_POINT('Ctrl Pts',(29.1227466839353,-1.23306866661795,27.2003783708913));
#56505=CARTESIAN_POINT('Ctrl Pts',(29.4698813680168,-1.416339226716,27.2221707450579));
#56506=CARTESIAN_POINT('Ctrl Pts',(29.6558172836666,-1.47261637710131,27.232679845148));
#56507=CARTESIAN_POINT('Ctrl Pts',(29.8981460836565,-1.49740948534734,27.2450275924248));
#56508=CARTESIAN_POINT('Ctrl Pts',(29.9491012405249,-1.5,27.247551132293));
#56509=CARTESIAN_POINT('Ctrl Pts',(29.9999999999998,-1.50000000000001,27.25));
#56510=CARTESIAN_POINT('Ctrl Pts',(30.0000000003122,-1.50000000000001,27.312500000015));
#56511=CARTESIAN_POINT('Ctrl Pts',(29.9998020603292,-1.50000000000005,27.3124904766232));
#56512=CARTESIAN_POINT('Ctrl Pts',(29.9996041185888,-1.49999996081992,27.3124809520584));
#56513=CARTESIAN_POINT('Ctrl Pts',(29.8088160951652,-1.49992443102837,27.3032995609518));
#56514=CARTESIAN_POINT('Ctrl Pts',(29.6200100906951,-1.46352575850992,27.2932045535897));
#56515=CARTESIAN_POINT('Ctrl Pts',(29.2593205849108,-1.31930644298838,27.2718447795537));
#56516=CARTESIAN_POINT('Ctrl Pts',(29.0918823606668,-1.21016636340677,27.2607572353565));
#56517=CARTESIAN_POINT('Ctrl Pts',(28.8110979291704,-0.935181294724627,
27.2396095139674));
#56518=CARTESIAN_POINT('Ctrl Pts',(28.6997118002275,-0.772848068745042,
27.2304360038192));
#56519=CARTESIAN_POINT('Ctrl Pts',(28.5461974612702,-0.416685157506792,
27.210649175417));
#56520=CARTESIAN_POINT('Ctrl Pts',(28.5047394765833,-0.226599155889903,
27.2000888419939));
#56521=CARTESIAN_POINT('Ctrl Pts',(28.4958539389935,0.166443777601294,27.1782531234666));
#56522=CARTESIAN_POINT('Ctrl Pts',(28.5315184967694,0.365700597221805,27.1671833001544));
#56523=CARTESIAN_POINT('Ctrl Pts',(28.6754701753172,0.729371435414476,27.1469793646992));
#56524=CARTESIAN_POINT('Ctrl Pts',(28.7788000491734,0.891648198610453,27.1381536711784));
#56525=CARTESIAN_POINT('Ctrl Pts',(29.0437345128306,1.17200464814443,27.1176193266989));
#56526=CARTESIAN_POINT('Ctrl Pts',(29.2040531543845,1.2862733419873,27.1067318620762));
#56527=CARTESIAN_POINT('Ctrl Pts',(29.5628324377282,1.44858368838945,27.0849614650246));
#56528=CARTESIAN_POINT('Ctrl Pts',(29.7584548095726,1.49371725552991,27.0742958690726));
#56529=CARTESIAN_POINT('Ctrl Pts',(30.1472060622831,1.50481186242553,27.055283882181));
#56530=CARTESIAN_POINT('Ctrl Pts',(30.3365600149074,1.47407427722924,27.045587089767));
#56531=CARTESIAN_POINT('Ctrl Pts',(30.7004989886168,1.34098519143669,27.0243801486806));
#56532=CARTESIAN_POINT('Ctrl Pts',(30.8706482413977,1.23730103012925,27.0133137233474));
#56533=CARTESIAN_POINT('Ctrl Pts',(31.1605713571455,0.970446090199086,26.991952153717));
#56534=CARTESIAN_POINT('Ctrl Pts',(31.2776619344983,0.810096307036669,26.9825053503909));
#56535=CARTESIAN_POINT('Ctrl Pts',(31.4414580755822,0.457344311316898,26.9629080172954));
#56536=CARTESIAN_POINT('Ctrl Pts',(31.4881418689773,0.269035150966863,26.9524463972759));
#56537=CARTESIAN_POINT('Ctrl Pts',(31.508284818313,-0.122458793694974,26.9306967336836));
#56538=CARTESIAN_POINT('Ctrl Pts',(31.478582774639,-0.322064434897177,26.9196075313946));
#56539=CARTESIAN_POINT('Ctrl Pts',(31.3455674834561,-0.689986184900448,
26.8991674341722));
#56540=CARTESIAN_POINT('Ctrl Pts',(31.246662212612,-0.855842984261559,26.8903733141072));
#56541=CARTESIAN_POINT('Ctrl Pts',(30.9897531567272,-1.14377092738595,26.8700147729728));
#56542=CARTESIAN_POINT('Ctrl Pts',(30.8332877383797,-1.26231706455743,26.8591938787678));
#56543=CARTESIAN_POINT('Ctrl Pts',(30.4799553603842,-1.43498001100993,26.8373979738484));
#56544=CARTESIAN_POINT('Ctrl Pts',(30.2857235516143,-1.48590367409306,26.8266384453951));
#56545=CARTESIAN_POINT('Ctrl Pts',(30.0581276265954,-1.49915605873645,26.8153201095514));
#56546=CARTESIAN_POINT('Ctrl Pts',(30.0290509426437,-1.50000000000001,26.8138977141296));
#56547=CARTESIAN_POINT('Ctrl Pts',(30.0000000000001,-1.50000000000001,26.8125));
#56548=CARTESIAN_POINT('Origin',(30.,-1.32966554433622E-14,16.));
#56549=CARTESIAN_POINT('',(30.,-1.50000000000001,26.25));
#56550=CARTESIAN_POINT('',(30.0000000000001,-1.50000000000001,26.3125));
#56551=CARTESIAN_POINT('',(30.,-1.50000000000001,16.));
#56552=CARTESIAN_POINT('Ctrl Pts',(30.,-1.50000000000001,26.25));
#56553=CARTESIAN_POINT('Ctrl Pts',(30.0056194401817,-1.50000000000001,26.2502703654418));
#56554=CARTESIAN_POINT('Ctrl Pts',(30.0112401600052,-1.49996842190559,26.2505416696197));
#56555=CARTESIAN_POINT('Ctrl Pts',(30.2156637559459,-1.49767029707552,26.2604408412659));
#56556=CARTESIAN_POINT('Ctrl Pts',(30.4120156853044,-1.45593401100177,26.2710471691517));
#56557=CARTESIAN_POINT('Ctrl Pts',(30.7738333695248,-1.29974623576057,26.2927936799124));
#56558=CARTESIAN_POINT('Ctrl Pts',(30.9363483004055,-1.18803068750778,26.3037158928437));
#56559=CARTESIAN_POINT('Ctrl Pts',(31.2059383925193,-0.91211987124096,26.3243507415389));
#56560=CARTESIAN_POINT('Ctrl Pts',(31.3118367658411,-0.751883140819906,
26.3332287143989));
#56561=CARTESIAN_POINT('Ctrl Pts',(31.4620725484111,-0.390717177178761,
26.3532934901568));
#56562=CARTESIAN_POINT('Ctrl Pts',(31.5011777050095,-0.191739563198423,
26.3643478020445));
#56563=CARTESIAN_POINT('Ctrl Pts',(31.4988144256802,0.202052743889533,26.3862251524383));
#56564=CARTESIAN_POINT('Ctrl Pts',(31.4603972352794,0.393097806012914,26.3968387670007));
#56565=CARTESIAN_POINT('Ctrl Pts',(31.3127984325509,0.751186708707084,26.4167325949282));
#56566=CARTESIAN_POINT('Ctrl Pts',(31.2046306350456,0.914654115967526,26.4257825736587));
#56567=CARTESIAN_POINT('Ctrl Pts',(30.929085340333,1.1942016269637,26.4468049614706));
#56568=CARTESIAN_POINT('Ctrl Pts',(30.763267624326,1.30642002708729,26.4579000478329));
#56569=CARTESIAN_POINT('Ctrl Pts',(30.4044749371868,1.4569895622401,26.479344956129));
#56570=CARTESIAN_POINT('Ctrl Pts',(30.2159899848526,1.49659297949806,26.4895135375502));
#56571=CARTESIAN_POINT('Ctrl Pts',(29.8264040657205,1.50311771775866,26.5084387415533));
#56572=CARTESIAN_POINT('Ctrl Pts',(29.6289313228251,1.46692091172634,26.5187719136178));
#56573=CARTESIAN_POINT('Ctrl Pts',(29.2622864534942,1.32066065000658,26.5404749081659));
#56574=CARTESIAN_POINT('Ctrl Pts',(29.0963152488665,1.21314636529189,26.5514467093804));
#56575=CARTESIAN_POINT('Ctrl Pts',(28.8192613253014,0.944447852152411,26.5722403200802));
#56576=CARTESIAN_POINT('Ctrl Pts',(28.7092361098565,0.787428080615722,26.5812539955214));
#56577=CARTESIAN_POINT('Ctrl Pts',(28.5500186537103,0.4325695152731,26.6009683602626));
#56578=CARTESIAN_POINT('Ctrl Pts',(28.5055087117716,0.236724815037938,26.6118486213868));
#56579=CARTESIAN_POINT('Ctrl Pts',(28.4955827399852,-0.155640049113208,
26.6336466693952));
#56580=CARTESIAN_POINT('Ctrl Pts',(28.5282144121142,-0.348361913823613,
26.6443534396569));
#56581=CARTESIAN_POINT('Ctrl Pts',(28.6646766132005,-0.710004687419899,
26.6644447048566));
#56582=CARTESIAN_POINT('Ctrl Pts',(28.7669073789545,-0.875602741749661,
26.6733284353239));
#56583=CARTESIAN_POINT('Ctrl Pts',(29.0326342692594,-1.16351957915387,26.6941109162225));
#56584=CARTESIAN_POINT('Ctrl Pts',(29.1952892767769,-1.28140768888904,26.7052113286353));
#56585=CARTESIAN_POINT('Ctrl Pts',(29.5502593863542,-1.44373597574174,26.7267989550745));
#56586=CARTESIAN_POINT('Ctrl Pts',(29.7380028348229,-1.48930167419739,26.7370974797965));
#56587=CARTESIAN_POINT('Ctrl Pts',(29.9528487018704,-1.49944465692866,26.7477160059146));
#56588=CARTESIAN_POINT('Ctrl Pts',(29.9764341399413,-1.50000000000001,26.7488661870293));
#56589=CARTESIAN_POINT('Ctrl Pts',(29.9999999999999,-1.50000000000001,26.75));
#56590=CARTESIAN_POINT('Ctrl Pts',(30.0000000000001,-1.50000000000001,26.8125));
#56591=CARTESIAN_POINT('Ctrl Pts',(29.8395800016776,-1.50000000000002,26.8047817892321));
#56592=CARTESIAN_POINT('Ctrl Pts',(29.6800130120943,-1.4742710204936,26.7963899249912));
#56593=CARTESIAN_POINT('Ctrl Pts',(29.3406580591605,-1.36160698346738,26.7769331456215));
#56594=CARTESIAN_POINT('Ctrl Pts',(29.1679496395237,-1.26348603655748,26.7658981260489));
#56595=CARTESIAN_POINT('Ctrl Pts',(28.8688888773426,-1.00499369846698,26.744329215695));
#56596=CARTESIAN_POINT('Ctrl Pts',(28.7459708502921,-0.846646295408431,
26.7345359053005));
#56597=CARTESIAN_POINT('Ctrl Pts',(28.5719299961441,-0.497373685523865,
26.7151318714181));
#56598=CARTESIAN_POINT('Ctrl Pts',(28.5201211210885,-0.310969647956289,
26.7047760915532));
#56599=CARTESIAN_POINT('Ctrl Pts',(28.4888763927518,0.078675171393689,26.6831291571448));
#56600=CARTESIAN_POINT('Ctrl Pts',(28.5126680280148,0.27845746343119,26.6720301409206));
#56601=CARTESIAN_POINT('Ctrl Pts',(28.6347687943924,0.650483449918004,26.6513620305602));
#56602=CARTESIAN_POINT('Ctrl Pts',(28.7293030467267,0.819946999855557,26.6425267967844));
#56603=CARTESIAN_POINT('Ctrl Pts',(28.9783004894773,1.11523286685495,26.62234451654));
#56604=CARTESIAN_POINT('Ctrl Pts',(29.1308905878018,1.23784103842587,26.6115972394678));
#56605=CARTESIAN_POINT('Ctrl Pts',(29.4786064716065,1.42045274911996,26.5897952036888));
#56606=CARTESIAN_POINT('Ctrl Pts',(29.671307799161,1.47699671076135,26.5789531911429));
#56607=CARTESIAN_POINT('Ctrl Pts',(30.058657983757,1.51083891985875,26.5593767353335));
#56608=CARTESIAN_POINT('Ctrl Pts',(30.2492918070221,1.49128918840572,26.5502639753537));
#56609=CARTESIAN_POINT('Ctrl Pts',(30.6191301716824,1.38027512961514,26.5293863948823));
#56610=CARTESIAN_POINT('Ctrl Pts',(30.7941362196709,1.2875659668366,26.518391157951));
#56611=CARTESIAN_POINT('Ctrl Pts',(31.1019229551517,1.03729505553015,26.4966307919773));
#56612=CARTESIAN_POINT('Ctrl Pts',(31.2305302882388,0.880892156398053,26.4864384531331));
#56613=CARTESIAN_POINT('Ctrl Pts',(31.4143329938993,0.535011347738905,26.467222852652));
#56614=CARTESIAN_POINT('Ctrl Pts',(31.4709425533457,0.350543024469619,26.4569746124704));
#56615=CARTESIAN_POINT('Ctrl Pts',(31.5126435249117,-0.0370627264893054,
26.4354409596394));
#56616=CARTESIAN_POINT('Ctrl Pts',(31.4944467514533,-0.236856679751601,
26.4243412955692));
#56617=CARTESIAN_POINT('Ctrl Pts',(31.382763240843,-0.612667143007661,26.4034629364995));
#56618=CARTESIAN_POINT('Ctrl Pts',(31.2923692914564,-0.785603738087747,
26.3945234871348));
#56619=CARTESIAN_POINT('Ctrl Pts',(31.0508333839059,-1.08773585408316,26.3745100265869));
#56620=CARTESIAN_POINT('Ctrl Pts',(30.9019600520426,-1.21403192877114,26.3638391307711));
#56621=CARTESIAN_POINT('Ctrl Pts',(30.559750929656,-1.4057831061822,26.3420481650989));
#56622=CARTESIAN_POINT('Ctrl Pts',(30.3686322762759,-1.46754077280931,26.3311374738613));
#56623=CARTESIAN_POINT('Ctrl Pts',(30.1141378164167,-1.49674664949133,26.3180818291001));
#56624=CARTESIAN_POINT('Ctrl Pts',(30.0570405412872,-1.50000000000001,26.3152443643222));
#56625=CARTESIAN_POINT('Ctrl Pts',(30.0000000000002,-1.50000000000001,26.3125));
#56626=CARTESIAN_POINT('Origin',(30.,-1.32966554433622E-14,16.));
#56627=CARTESIAN_POINT('',(30.0000000000001,-1.50000000000001,25.75));
#56628=CARTESIAN_POINT('',(30.,-1.50000000000001,25.8125));
#56629=CARTESIAN_POINT('',(30.,-1.50000000000001,16.));
#56630=CARTESIAN_POINT('Ctrl Pts',(30.0000000000002,-1.50000000000001,25.75));
#56631=CARTESIAN_POINT('Ctrl Pts',(30.0350308469701,-1.50000000000001,25.7516854224107));
#56632=CARTESIAN_POINT('Ctrl Pts',(30.0700958017757,-1.49877287551864,25.7534065726266));
#56633=CARTESIAN_POINT('Ctrl Pts',(30.3035194655511,-1.48237243734734,25.7650927416133));
#56634=CARTESIAN_POINT('Ctrl Pts',(30.4971388675202,-1.42911969045028,25.7758875024032));
#56635=CARTESIAN_POINT('Ctrl Pts',(30.848183508266,-1.2523218603483,25.7976881963921));
#56636=CARTESIAN_POINT('Ctrl Pts',(31.0030592952475,-1.13208157746957,25.8084796690252));
#56637=CARTESIAN_POINT('Ctrl Pts',(31.2567047166631,-0.841106936698577,
25.8287658189633));
#56638=CARTESIAN_POINT('Ctrl Pts',(31.3538096540821,-0.673770640691784,
25.8375682977395));
#56639=CARTESIAN_POINT('Ctrl Pts',(31.4823392304013,-0.304145984064151,
25.8581030008855));
#56640=CARTESIAN_POINT('Ctrl Pts',(31.5096068971125,-0.104447172132542,
25.8691973793261));
#56641=CARTESIAN_POINT('Ctrl Pts',(31.4848844296652,0.286323023183646,25.8909068346215));
#56642=CARTESIAN_POINT('Ctrl Pts',(31.4360830652788,0.473864860798067,25.9013258256));
#56643=CARTESIAN_POINT('Ctrl Pts',(31.2680746858178,0.825196096656156,25.9208442275921));
#56644=CARTESIAN_POINT('Ctrl Pts',(31.1486056539627,0.984726473310249,25.9304245311885));
#56645=CARTESIAN_POINT('Ctrl Pts',(30.8549287066094,1.24817526789042,25.9518720919776));
#56646=CARTESIAN_POINT('Ctrl Pts',(30.6837094772403,1.34958696185865,25.9629268724906));
#56647=CARTESIAN_POINT('Ctrl Pts',(30.3185036845909,1.47806545582453,25.9840666914365));
#56648=CARTESIAN_POINT('Ctrl Pts',(30.1289070957048,1.50647679352315,25.993618043535));
#56649=CARTESIAN_POINT('Ctrl Pts',(29.7404075656125,1.49068855536224,26.0127482980627));
#56650=CARTESIAN_POINT('Ctrl Pts',(29.545331017818,1.44318830470102,26.0234533742517));
#56651=CARTESIAN_POINT('Ctrl Pts',(29.188736991222,1.27663378618483,26.0452365267588));
#56652=CARTESIAN_POINT('Ctrl Pts',(29.0299764729631,1.16060540084053,26.056097906459));
#56653=CARTESIAN_POINT('Ctrl Pts',(28.7683079019703,0.877153943717209,26.0765610930375));
#56654=CARTESIAN_POINT('Ctrl Pts',(28.6667786145465,0.713430148276809,26.0853649917623));
#56655=CARTESIAN_POINT('Ctrl Pts',(28.5272614190292,0.348018884480366,26.1056656175288));
#56656=CARTESIAN_POINT('Ctrl Pts',(28.4940188142116,0.14859972255689,26.1167444598579));
#56657=CARTESIAN_POINT('Ctrl Pts',(28.5074840531687,-0.243852309362615,
26.1385473505201));
#56658=CARTESIAN_POINT('Ctrl Pts',(28.5510714566589,-0.433234122923729,
26.1490685623846));
#56659=CARTESIAN_POINT('Ctrl Pts',(28.7087569062828,-0.788023018123922,
26.1687790565624));
#56660=CARTESIAN_POINT('Ctrl Pts',(28.8224400778707,-0.949553940205162,
26.1780544535033));
#56661=CARTESIAN_POINT('Ctrl Pts',(29.1069273076436,-1.22127183449108,26.1992895710132));
#56662=CARTESIAN_POINT('Ctrl Pts',(29.2754819087647,-1.32821443027861,26.2103697857015));
#56663=CARTESIAN_POINT('Ctrl Pts',(29.6323103908041,-1.46593097223903,26.2313631635471));
#56664=CARTESIAN_POINT('Ctrl Pts',(29.8154198943914,-1.50000000000001,26.2411193855283));
#56665=CARTESIAN_POINT('Ctrl Pts',(30.,-1.50000000000001,26.25));
#56666=CARTESIAN_POINT('Ctrl Pts',(30.0000000000002,-1.50000000000001,26.3125));
#56667=CARTESIAN_POINT('Ctrl Pts',(29.867580258195,-1.50000000000001,26.3061289522019));
#56668=CARTESIAN_POINT('Ctrl Pts',(29.7355134428156,-1.48246999719879,26.299287940062));
#56669=CARTESIAN_POINT('Ctrl Pts',(29.4184023489971,-1.39643165750255,26.2816409715667));
#56670=CARTESIAN_POINT('Ctrl Pts',(29.2414246745114,-1.30875331188796,26.2706906196325));
#56671=CARTESIAN_POINT('Ctrl Pts',(28.9285790709285,-1.068455989113,26.2489639028796));
#56672=CARTESIAN_POINT('Ctrl Pts',(28.7965902868422,-0.917216536990246,
26.2384564742772));
#56673=CARTESIAN_POINT('Ctrl Pts',(28.6032774267936,-0.57923818308581,26.2196798990602));
#56674=CARTESIAN_POINT('Ctrl Pts',(28.5410496718181,-0.397228347537677,
26.2095682415298));
#56675=CARTESIAN_POINT('Ctrl Pts',(28.4870387262231,-0.0124011503103316,
26.1881889527949));
#56676=CARTESIAN_POINT('Ctrl Pts',(28.4986129287161,0.187210043596071,26.1770994420224));
#56677=CARTESIAN_POINT('Ctrl Pts',(28.5978341126594,0.567369358609899,26.1559794800772));
#56678=CARTESIAN_POINT('Ctrl Pts',(28.6833047820777,0.744501773375072,26.1468355900596));
#56679=CARTESIAN_POINT('Ctrl Pts',(28.9160253075989,1.05460577600707,26.1270248184819));
#56680=CARTESIAN_POINT('Ctrl Pts',(29.060441358732,1.18507685788338,26.1164524012633));
#56681=CARTESIAN_POINT('Ctrl Pts',(29.3972605323865,1.3881264388998,26.0946069150758));
#56682=CARTESIAN_POINT('Ctrl Pts',(29.5879874006837,1.45617711323181,26.0835402678372));
#56683=CARTESIAN_POINT('Ctrl Pts',(29.9751313819113,1.51185807000195,26.0633671011121));
#56684=CARTESIAN_POINT('Ctrl Pts',(30.1672228871666,1.50278877622694,26.0545319510962));
#56685=CARTESIAN_POINT('Ctrl Pts',(30.5421508905102,1.41213985662164,26.0339751935801));
#56686=CARTESIAN_POINT('Ctrl Pts',(30.7210278648892,1.32972839399854,26.0230797638426));
#56687=CARTESIAN_POINT('Ctrl Pts',(31.0401525812529,1.09890434445495,26.0013140896138));
#56688=CARTESIAN_POINT('Ctrl Pts',(31.1764827770535,0.951536572108244,25.9906613507783));
#56689=CARTESIAN_POINT('Ctrl Pts',(31.3792148041551,0.619604996410003,25.9716870800294));
#56690=CARTESIAN_POINT('Ctrl Pts',(31.4465937278795,0.439945368358781,25.9619414093531));
#56691=CARTESIAN_POINT('Ctrl Pts',(31.5118285637272,0.0578389075257285,
25.9407132726402));
#56692=CARTESIAN_POINT('Ctrl Pts',(31.5063115855957,-0.141417075009879,
25.9296434958327));
#56693=CARTESIAN_POINT('Ctrl Pts',(31.4186362556573,-0.525426994647723,
25.9083096114084));
#56694=CARTESIAN_POINT('Ctrl Pts',(31.3377111820022,-0.706481965554299,
25.8989028268757));
#56695=CARTESIAN_POINT('Ctrl Pts',(31.1130533652913,-1.0237694591265,25.8792804311414));
#56696=CARTESIAN_POINT('Ctrl Pts',(30.972766729538,-1.15788504149396,25.8688054543882));
#56697=CARTESIAN_POINT('Ctrl Pts',(30.6428698469895,-1.36991560346518,25.8470435453937));
#56698=CARTESIAN_POINT('Ctrl Pts',(30.4547968017865,-1.44330311864552,25.835956334699));
#56699=CARTESIAN_POINT('Ctrl Pts',(30.1725168697432,-1.4925627888959,25.8210068109627));
#56700=CARTESIAN_POINT('Ctrl Pts',(30.0862466800351,-1.50000000000001,25.8166495453279));
#56701=CARTESIAN_POINT('Ctrl Pts',(30.,-1.50000000000001,25.8125));
#56702=CARTESIAN_POINT('Origin',(30.,-1.32966554433622E-14,16.));
#56703=CARTESIAN_POINT('',(30.0000000000001,-1.50000000000001,25.25));
#56704=CARTESIAN_POINT('',(30.,-1.50000000000001,25.3125));
#56705=CARTESIAN_POINT('',(30.,-1.50000000000001,16.));
#56706=CARTESIAN_POINT('Ctrl Pts',(30.0000000000001,-1.50000000000001,25.25));
#56707=CARTESIAN_POINT('Ctrl Pts',(30.0627700539087,-1.50000000000001,25.2530200256268));
#56708=CARTESIAN_POINT('Ctrl Pts',(30.1255978857231,-1.49606031931736,25.2561522666689));
#56709=CARTESIAN_POINT('Ctrl Pts',(30.387395972516,-1.46296629655124,25.2696673114027));
#56710=CARTESIAN_POINT('Ctrl Pts',(30.5795743359629,-1.39800636679879,25.2807179397182));
#56711=CARTESIAN_POINT('Ctrl Pts',(30.9202426421314,-1.20018691165606,25.3026033361058));
#56712=CARTESIAN_POINT('Ctrl Pts',(31.0669765445057,-1.07185443274338,25.3132278653563));
#56713=CARTESIAN_POINT('Ctrl Pts',(31.3042648643842,-0.765865616588927,
25.3331440943071));
#56714=CARTESIAN_POINT('Ctrl Pts',(31.3922917557281,-0.59091969078094,25.3421711282901));
#56715=CARTESIAN_POINT('Ctrl Pts',(31.4979914701149,-0.212996523390812,
25.3631668598117));
#56716=CARTESIAN_POINT('Ctrl Pts',(31.5129981369395,-0.0132639168507718,
25.3742631157306));
#56717=CARTESIAN_POINT('Ctrl Pts',(31.4653583210385,0.373052959697002,25.3957251644277));
#56718=CARTESIAN_POINT('Ctrl Pts',(31.4060337226141,0.556359728684241,25.4059088738159));
#56719=CARTESIAN_POINT('Ctrl Pts',(31.2180258231604,0.89772836856045,25.4248737982534));
#56720=CARTESIAN_POINT('Ctrl Pts',(31.088460968798,1.05109657163312,25.4351618575451));
#56721=CARTESIAN_POINT('Ctrl Pts',(30.7792551558925,1.29659274113508,25.4568578671965));
#56722=CARTESIAN_POINT('Ctrl Pts',(30.6034030192283,1.3871914976091,25.4678351891908));
#56723=CARTESIAN_POINT('Ctrl Pts',(30.2324892526205,1.49400946706811,25.4886479519256));
#56724=CARTESIAN_POINT('Ctrl Pts',(30.0415773273281,1.51141487828139,25.4976825299541));
#56725=CARTESIAN_POINT('Ctrl Pts',(29.6545526771042,1.47316919187237,25.5173656422979));
#56726=CARTESIAN_POINT('Ctrl Pts',(29.4624963512885,1.41443679130397,25.5282374121534));
#56727=CARTESIAN_POINT('Ctrl Pts',(29.1170567587378,1.22797823527613,25.5500367866331));
#56728=CARTESIAN_POINT('Ctrl Pts',(28.9660123174462,1.10381260264269,25.560752961054));
#56729=CARTESIAN_POINT('Ctrl Pts',(28.7201314342041,0.805655980053721,25.5808650389699));
#56730=CARTESIAN_POINT('Ctrl Pts',(28.627324212077,0.634750626561539,25.5897360763022));
#56731=CARTESIAN_POINT('Ctrl Pts',(28.5095600205757,0.261132939276874,25.6104926144847));
#56732=CARTESIAN_POINT('Ctrl Pts',(28.4881034640454,0.0613273497745445,
25.6215929250126));
#56733=CARTESIAN_POINT('Ctrl Pts',(28.5237184917358,-0.327500650137204,
25.6431944805633));
#56734=CARTESIAN_POINT('Ctrl Pts',(28.57753700972,-0.513112472024964,25.6535062484459));
#56735=CARTESIAN_POINT('Ctrl Pts',(28.7556436240904,-0.860981573894074,
25.6728323096608));
#56736=CARTESIAN_POINT('Ctrl Pts',(28.8809148866478,-1.0185241445112,25.6827836630609));
#56737=CARTESIAN_POINT('Ctrl Pts',(29.1836083572217,-1.27362286430434,25.7044330850039));
#56738=CARTESIAN_POINT('Ctrl Pts',(29.357290902101,-1.3695025366285,25.7154527145718));
#56739=CARTESIAN_POINT('Ctrl Pts',(29.6920067607584,-1.47617903100382,25.7345199747848));
#56740=CARTESIAN_POINT('Ctrl Pts',(29.8456406050883,-1.50000000000001,25.7425733801496));
#56741=CARTESIAN_POINT('Ctrl Pts',(30.0000000000002,-1.50000000000001,25.75));
#56742=CARTESIAN_POINT('Ctrl Pts',(30.,-1.50000000000001,25.8125));
#56743=CARTESIAN_POINT('Ctrl Pts',(29.8958136711151,-1.50000000000001,25.8074873329144));
#56744=CARTESIAN_POINT('Ctrl Pts',(29.7916909834384,-1.4891476478018,25.80217627354));
#56745=CARTESIAN_POINT('Ctrl Pts',(29.4989680289332,-1.42717135574301,25.7863710701566));
#56746=CARTESIAN_POINT('Ctrl Pts',(29.3182929815531,-1.3502283271827,25.7755410315376));
#56747=CARTESIAN_POINT('Ctrl Pts',(28.9928896773701,-1.12927046795383,25.7537473394536));
#56748=CARTESIAN_POINT('Ctrl Pts',(28.8522264483536,-0.985982788210688,
25.7429994633659));
#56749=CARTESIAN_POINT('Ctrl Pts',(28.639853465626,-0.660351661724937,25.7237363544014));
#56750=CARTESIAN_POINT('Ctrl Pts',(28.5672444995779,-0.483012345456745,
25.714334019192));
#56751=CARTESIAN_POINT('Ctrl Pts',(28.4907135279836,-0.103874220197911,
25.6932707900109));
#56752=CARTESIAN_POINT('Ctrl Pts',(28.4901189594842,0.0948392876888842,
25.6822311506839));
#56753=CARTESIAN_POINT('Ctrl Pts',(28.5659791907661,0.482606924381713,25.660688504201));
#56754=CARTESIAN_POINT('Ctrl Pts',(28.6422553573453,0.667705397375409,25.6509438140946));
#56755=CARTESIAN_POINT('Ctrl Pts',(28.8587620723286,0.992152292410515,25.6315147161622));
#56756=CARTESIAN_POINT('Ctrl Pts',(28.9948328944551,1.12978254443193,25.6211449431241));
#56757=CARTESIAN_POINT('Ctrl Pts',(29.3175819275344,1.35056278988812,25.599483888434));
#56758=CARTESIAN_POINT('Ctrl Pts',(29.5028611462505,1.42918794783786,25.5883856057019));
#56759=CARTESIAN_POINT('Ctrl Pts',(29.8863465577115,1.507984767606,25.5677463546914));
#56760=CARTESIAN_POINT('Ctrl Pts',(30.0802506039983,1.51013051078303,25.5589203440921));
#56761=CARTESIAN_POINT('Ctrl Pts',(30.4601704571654,1.44079280620514,25.5387153942847));
#56762=CARTESIAN_POINT('Ctrl Pts',(30.6424548754516,1.36926262641685,25.5279582816823));
#56763=CARTESIAN_POINT('Ctrl Pts',(30.9737363815272,1.15817666999724,25.5061559940003));
#56764=CARTESIAN_POINT('Ctrl Pts',(31.118540202541,1.01903114337744,25.4953239633962));
#56765=CARTESIAN_POINT('Ctrl Pts',(31.3403349350297,0.699693252907024,25.4757823623965));
#56766=CARTESIAN_POINT('Ctrl Pts',(31.418072458882,0.524551989157358,25.4666417771753));
#56767=CARTESIAN_POINT('Ctrl Pts',(31.5054879258866,0.148377517280613,25.4457431954044));
#56768=CARTESIAN_POINT('Ctrl Pts',(31.5119666548414,-0.0496365545101339,
25.4347424136382));
#56769=CARTESIAN_POINT('Ctrl Pts',(31.4476607795272,-0.440895614279282,
25.4130057992066));
#56770=CARTESIAN_POINT('Ctrl Pts',(31.3759395541655,-0.629971074835861,
25.4028673928089));
#56771=CARTESIAN_POINT('Ctrl Pts',(31.1673112734267,-0.961240411187918,
25.383627833962));
#56772=CARTESIAN_POINT('Ctrl Pts',(31.0353453440586,-1.10210544227651,25.3733657026948));
#56773=CARTESIAN_POINT('Ctrl Pts',(30.7196295943324,-1.33102399282861,25.3518169729773));
#56774=CARTESIAN_POINT('Ctrl Pts',(30.5371475111052,-1.41455738295539,25.3407169277066));
#56775=CARTESIAN_POINT('Ctrl Pts',(30.2307882933611,-1.48667060842925,25.3239740678184));
#56776=CARTESIAN_POINT('Ctrl Pts',(30.1154677152456,-1.50000000000002,25.31805544304));
#56777=CARTESIAN_POINT('Ctrl Pts',(29.9999999999999,-1.50000000000001,25.3125));
#56778=CARTESIAN_POINT('Origin',(30.,-1.32966554433622E-14,16.));
#56779=CARTESIAN_POINT('',(30.,-1.50000000000001,24.75));
#56780=CARTESIAN_POINT('',(29.9999999999999,-1.50000000000001,24.8125));
#56781=CARTESIAN_POINT('',(30.,-1.50000000000001,16.));
#56782=CARTESIAN_POINT('Ctrl Pts',(30.,-1.50000000000001,24.75));
#56783=CARTESIAN_POINT('Ctrl Pts',(30.0924202028298,-1.50000000000002,24.7544465690819));
#56784=CARTESIAN_POINT('Ctrl Pts',(30.1848415762481,-1.49146009950343,24.759130413942));
#56785=CARTESIAN_POINT('Ctrl Pts',(30.4723479931102,-1.43762037173554,24.7744586208663));
#56786=CARTESIAN_POINT('Ctrl Pts',(30.6592834359903,-1.36205645668747,24.7855515541955));
#56787=CARTESIAN_POINT('Ctrl Pts',(30.9862537983022,-1.14638219357722,24.80727387484));
#56788=CARTESIAN_POINT('Ctrl Pts',(31.1248087259681,-1.01079850350159,24.8177063155187));
#56789=CARTESIAN_POINT('Ctrl Pts',(31.346109752526,-0.69055016576277,24.8372494532827));
#56790=CARTESIAN_POINT('Ctrl Pts',(31.4251274703691,-0.50783917665878,24.8467867124079));
#56791=CARTESIAN_POINT('Ctrl Pts',(31.5079543915197,-0.122264618516638,
24.8682075211936));
#56792=CARTESIAN_POINT('Ctrl Pts',(31.5109523526148,0.0767903025210503,
24.8792661279179));
#56793=CARTESIAN_POINT('Ctrl Pts',(31.441061251381,0.457686740875712,24.9004270411598));
#56794=CARTESIAN_POINT('Ctrl Pts',(31.3715371249325,0.636385044039808,24.9100225849775));
#56795=CARTESIAN_POINT('Ctrl Pts',(31.1648481820269,0.965747220324715,24.9291158607209));
#56796=CARTESIAN_POINT('Ctrl Pts',(31.0267283705006,1.11145999209774,24.939808730245));
#56797=CARTESIAN_POINT('Ctrl Pts',(30.7049953637051,1.33826413832451,24.9615882319247));
#56798=CARTESIAN_POINT('Ctrl Pts',(30.525362209954,1.41844022126688,24.9724579494792));
#56799=CARTESIAN_POINT('Ctrl Pts',(30.1493787440764,1.50469862427576,24.9929435291658));
#56800=CARTESIAN_POINT('Ctrl Pts',(29.9569371691124,1.5114809139774,25.00175294714));
#56801=CARTESIAN_POINT('Ctrl Pts',(29.5704977811955,1.45108059660786,25.0220233074535));
#56802=CARTESIAN_POINT('Ctrl Pts',(29.3808354910635,1.38084291684638,25.0330994853021));
#56803=CARTESIAN_POINT('Ctrl Pts',(29.0468101101847,1.17410520091496,25.0549130032641));
#56804=CARTESIAN_POINT('Ctrl Pts',(28.9040664949486,1.04213311105638,25.0654466500392));
#56805=CARTESIAN_POINT('Ctrl Pts',(28.6746221434491,0.72909790198446,25.0851812190219));
#56806=CARTESIAN_POINT('Ctrl Pts',(28.5909928953227,0.55038117737188,25.0944232679238));
#56807=CARTESIAN_POINT('Ctrl Pts',(28.496446216206,0.168641933616187,25.115631003688));
#56808=CARTESIAN_POINT('Ctrl Pts',(28.4873339658181,-0.0308466586561953,
25.1267137032587));
#56809=CARTESIAN_POINT('Ctrl Pts',(28.5459190178277,-0.414647584032544,
25.1480359768907));
#56810=CARTESIAN_POINT('Ctrl Pts',(28.6102581790788,-0.595692019972521,
25.1580163493537));
#56811=CARTESIAN_POINT('Ctrl Pts',(28.8073809961852,-0.931227827424643,
25.1768208644096));
#56812=CARTESIAN_POINT('Ctrl Pts',(28.9411488677475,-1.08089452062442,25.1874141822753));
#56813=CARTESIAN_POINT('Ctrl Pts',(29.2565034825196,-1.31734526046784,25.2091547643595));
#56814=CARTESIAN_POINT('Ctrl Pts',(29.4342658933141,-1.40290303357365,25.220083967145));
#56815=CARTESIAN_POINT('Ctrl Pts',(29.7466738861071,-1.48392560477994,25.2373653306843));
#56816=CARTESIAN_POINT('Ctrl Pts',(29.8731973879732,-1.50000000000001,25.2438992064844));
#56817=CARTESIAN_POINT('Ctrl Pts',(30.0000000000001,-1.50000000000001,25.25));
#56818=CARTESIAN_POINT('Ctrl Pts',(29.9999999999999,-1.50000000000001,25.3125));
#56819=CARTESIAN_POINT('Ctrl Pts',(29.9230963675565,-1.50000000000001,25.3087999722589));
#56820=CARTESIAN_POINT('Ctrl Pts',(29.8461434428577,-1.49408668250554,25.3049333141238));
#56821=CARTESIAN_POINT('Ctrl Pts',(29.5785997947569,-1.4525378268213,25.2909069794727));
#56822=CARTESIAN_POINT('Ctrl Pts',(29.394946779968,-1.38612426885289,25.2802261486243));
#56823=CARTESIAN_POINT('Ctrl Pts',(29.0584111434883,-1.1844646483524,25.2584329141398));
#56824=CARTESIAN_POINT('Ctrl Pts',(28.9098271705268,-1.04932739740415,25.2475303518813));
#56825=CARTESIAN_POINT('Ctrl Pts',(28.679224033866,-0.736002543967933,25.2277319851447));
#56826=CARTESIAN_POINT('Ctrl Pts',(28.5966653608253,-0.562858820299269,
25.218769934461));
#56827=CARTESIAN_POINT('Ctrl Pts',(28.4992036771274,-0.189506940379824,
25.1980281633544));
#56828=CARTESIAN_POINT('Ctrl Pts',(28.4873077258157,0.00770736323463039,
25.1870718131536));
#56829=CARTESIAN_POINT('Ctrl Pts',(28.5403428741226,0.398677937032776,25.1653512257204));
#56830=CARTESIAN_POINT('Ctrl Pts',(28.6059812891417,0.588385613614782,25.1548923783415));
#56831=CARTESIAN_POINT('Ctrl Pts',(28.8032229731553,0.924175534219124,25.1360750856002));
#56832=CARTESIAN_POINT('Ctrl Pts',(28.9302878616598,1.06867554049118,25.1259477842385));
#56833=CARTESIAN_POINT('Ctrl Pts',(29.2375170160562,1.30684882772379,25.1045502900104));
#56834=CARTESIAN_POINT('Ctrl Pts',(29.416566346389,1.39601031268743,25.0934590671725));
#56835=CARTESIAN_POINT('Ctrl Pts',(29.7956879290814,1.49872079338579,25.0723655026123));
#56836=CARTESIAN_POINT('Ctrl Pts',(29.9916913791595,1.51255777708596,25.0632485758478));
#56837=CARTESIAN_POINT('Ctrl Pts',(30.376338186137,1.46478286918679,25.0434151669436));
#56838=CARTESIAN_POINT('Ctrl Pts',(30.5613937867408,1.40429329778983,25.0328314093361));
#56839=CARTESIAN_POINT('Ctrl Pts',(30.9051019650582,1.2128519030953,25.0109769253773));
#56840=CARTESIAN_POINT('Ctrl Pts',(31.0589867932662,1.08110262857348,24.9999134360581));
#56841=CARTESIAN_POINT('Ctrl Pts',(31.2996601001576,0.7727813254929,24.9797695555402));
#56842=CARTESIAN_POINT('Ctrl Pts',(31.3872075591177,0.601637196257516,24.9709242886809));
#56843=CARTESIAN_POINT('Ctrl Pts',(31.4948659823167,0.231233394936456,24.9503462997187));
#56844=CARTESIAN_POINT('Ctrl Pts',(31.5122374051454,0.0349818838105959,
24.9394434379894));
#56845=CARTESIAN_POINT('Ctrl Pts',(31.4704629549247,-0.356714017311379,
24.9176825545938));
#56846=CARTESIAN_POINT('Ctrl Pts',(31.410306361987,-0.548240683911054,24.9070421842271));
#56847=CARTESIAN_POINT('Ctrl Pts',(31.2229499202263,-0.889130700933294,
24.8881038499482));
#56848=CARTESIAN_POINT('Ctrl Pts',(31.1004741653132,-1.03689935475768,24.8783104947773));
#56849=CARTESIAN_POINT('Ctrl Pts',(30.8011609016804,-1.28341012707365,24.8570622572132));
#56850=CARTESIAN_POINT('Ctrl Pts',(30.6254139659021,-1.37762857486559,24.8459894497178));
#56851=CARTESIAN_POINT('Ctrl Pts',(30.2947063232275,-1.4782094919839,24.8272843564766));
#56852=CARTESIAN_POINT('Ctrl Pts',(30.1476360382517,-1.50000000000004,24.8196031422022));
#56853=CARTESIAN_POINT('Ctrl Pts',(29.9999999999998,-1.50000000000001,24.8125));
#56854=CARTESIAN_POINT('Origin',(30.,-1.32966554433622E-14,16.));
#56855=CARTESIAN_POINT('',(30.,-1.50000000000001,24.25));
#56856=CARTESIAN_POINT('',(30.,-1.50000000000001,24.3125));
#56857=CARTESIAN_POINT('',(30.,-1.50000000000001,16.));
#56858=CARTESIAN_POINT('Ctrl Pts',(29.9999999999999,-1.50000000000001,24.25));
#56859=CARTESIAN_POINT('Ctrl Pts',(30.1233865336442,-1.50000000000002,24.2559364373678));
#56860=CARTESIAN_POINT('Ctrl Pts',(30.2465476489323,-1.48477988594364,24.2622848102359));
#56861=CARTESIAN_POINT('Ctrl Pts',(30.5591244259704,-1.40597165010196,24.2795127850953));
#56862=CARTESIAN_POINT('Ctrl Pts',(30.7400033595231,-1.31975922707827,24.2906101163719));
#56863=CARTESIAN_POINT('Ctrl Pts',(31.0517371878966,-1.08642473531537,24.3120899308425));
#56864=CARTESIAN_POINT('Ctrl Pts',(31.181396759577,-0.943819238764671,24.3222894436867));
#56865=CARTESIAN_POINT('Ctrl Pts',(31.3842738432636,-0.610977913754327,
24.341295964288));
#56866=CARTESIAN_POINT('Ctrl Pts',(31.4529950991553,-0.422325812949031,
24.3515374548362));
#56867=CARTESIAN_POINT('Ctrl Pts',(31.5124147536636,-0.0319347678693356,
24.3732258462295));
#56868=CARTESIAN_POINT('Ctrl Pts',(31.5036442008573,0.165759327603677,24.3842088515336));
#56869=CARTESIAN_POINT('Ctrl Pts',(31.4119825510711,0.540750850840327,24.4050417139356));
#56870=CARTESIAN_POINT('Ctrl Pts',(31.3322181025457,0.715044299742208,24.4140993016492));
#56871=CARTESIAN_POINT('Ctrl Pts',(31.106713322535,1.03186525150623,24.4337494874295));
#56872=CARTESIAN_POINT('Ctrl Pts',(30.9603062459911,1.1693383575936,24.4446121985753));
#56873=CARTESIAN_POINT('Ctrl Pts',(30.6267827077052,1.37647673516795,24.4664127011144));
#56874=CARTESIAN_POINT('Ctrl Pts',(30.4439056234701,1.4458581458551,24.47713864034));
#56875=CARTESIAN_POINT('Ctrl Pts',(30.0630400763872,1.51099956140736,24.4972725262831));
#56876=CARTESIAN_POINT('Ctrl Pts',(29.8687484810349,1.50660828894347,24.5061312780688));
#56877=CARTESIAN_POINT('Ctrl Pts',(29.4860566158504,1.4231980920111,24.526860498932));
#56878=CARTESIAN_POINT('Ctrl Pts',(29.3019333862064,1.34250650777999,24.5379605648438));
#56879=CARTESIAN_POINT('Ctrl Pts',(28.9821049580114,1.11829253966791,24.5595764830508));
#56880=CARTESIAN_POINT('Ctrl Pts',(28.8477437066725,0.979293286040407,24.5699020321484));
#56881=CARTESIAN_POINT('Ctrl Pts',(28.6345240475922,0.651988290747904,24.5892523732038));
#56882=CARTESIAN_POINT('Ctrl Pts',(28.5601403785395,0.465238374198666,24.5991534236556));
#56883=CARTESIAN_POINT('Ctrl Pts',(28.489084947481,0.0759965520384366,24.6207779693312));
#56884=CARTESIAN_POINT('Ctrl Pts',(28.4921379080883,-0.122445995567395,
24.6318025553093));
#56885=CARTESIAN_POINT('Ctrl Pts',(28.5732141775453,-0.500358663169468,
24.6527977035094));
#56886=CARTESIAN_POINT('Ctrl Pts',(28.6479534934179,-0.676775662247645,
24.662082289407));
#56887=CARTESIAN_POINT('Ctrl Pts',(28.8642453292122,-0.999806026462223,
24.6814617008812));
#56888=CARTESIAN_POINT('Ctrl Pts',(29.0066425215227,-1.1413892524153,24.6922456563782));
#56889=CARTESIAN_POINT('Ctrl Pts',(29.3345224631394,-1.35826808429126,24.7140451994209));
#56890=CARTESIAN_POINT('Ctrl Pts',(29.515884916708,-1.43296761407463,24.7248459914751));
#56891=CARTESIAN_POINT('Ctrl Pts',(29.8033393621129,-1.4903304156034,24.7402695610815));
#56892=CARTESIAN_POINT('Ctrl Pts',(29.901655948172,-1.50000000000001,24.7452684196003));
#56893=CARTESIAN_POINT('Ctrl Pts',(30.,-1.50000000000001,24.75));
#56894=CARTESIAN_POINT('Ctrl Pts',(29.9999999999998,-1.50000000000001,24.8125));
#56895=CARTESIAN_POINT('Ctrl Pts',(29.9520844763832,-1.50000000000001,24.8101946632951));
#56896=CARTESIAN_POINT('Ctrl Pts',(29.9041155058213,-1.49770423456202,24.8078229838607));
#56897=CARTESIAN_POINT('Ctrl Pts',(29.6647429412583,-1.47465918202179,24.7956660256301));
#56898=CARTESIAN_POINT('Ctrl Pts',(29.4785801635781,-1.4195491435244,24.7851784304102));
#56899=CARTESIAN_POINT('Ctrl Pts',(29.1305308217309,-1.23854895841351,24.7634051157232));
#56900=CARTESIAN_POINT('Ctrl Pts',(28.9733425780824,-1.11174127780071,24.752319957252));
#56901=CARTESIAN_POINT('Ctrl Pts',(28.7235507953419,-0.81069913235786,24.7319395626836));
#56902=CARTESIAN_POINT('Ctrl Pts',(28.6307275649839,-0.641599855569549,
24.7231444364205));
#56903=CARTESIAN_POINT('Ctrl Pts',(28.5125127288929,-0.274334472746556,
24.7027408040415));
#56904=CARTESIAN_POINT('Ctrl Pts',(28.4895069858667,-0.0792389156648355,
24.6919021619814));
#56905=CARTESIAN_POINT('Ctrl Pts',(28.5196116095794,0.313003938746328,24.6701108922919));
#56906=CARTESIAN_POINT('Ctrl Pts',(28.5740816740222,0.506262436197778,24.6593743091001));
#56907=CARTESIAN_POINT('Ctrl Pts',(28.7511791399573,0.852358280491469,24.640146762195));
#56908=CARTESIAN_POINT('Ctrl Pts',(28.8690245914396,1.00348928998653,24.630706043882));
#56909=CARTESIAN_POINT('Ctrl Pts',(29.1601188576535,1.25831795738381,24.6096221903744));
#56910=CARTESIAN_POINT('Ctrl Pts',(29.3323550489326,1.35757677634782,24.5985782833421));
#56911=CARTESIAN_POINT('Ctrl Pts',(29.7064392762191,1.4842685830248,24.577060930713));
#56912=CARTESIAN_POINT('Ctrl Pts',(29.9047304118308,1.51001063736079,24.5673617334579));
#56913=CARTESIAN_POINT('Ctrl Pts',(30.2937060245362,1.48342562743484,24.547908663068));
#56914=CARTESIAN_POINT('Ctrl Pts',(30.4808263548115,1.43373651283452,24.5375255787967));
#56915=CARTESIAN_POINT('Ctrl Pts',(30.8329282215013,1.26331849859809,24.5158512361083));
#56916=CARTESIAN_POINT('Ctrl Pts',(30.9932828024692,1.14155315563778,24.5047538020966));
#56917=CARTESIAN_POINT('Ctrl Pts',(31.2521599269974,0.847929325410954,24.4841423531291));
#56918=CARTESIAN_POINT('Ctrl Pts',(31.3503160471837,0.680833771104865,24.4753240983947));
#56919=CARTESIAN_POINT('Ctrl Pts',(31.4789636487266,0.316753550496772,24.455097419472));
#56920=CARTESIAN_POINT('Ctrl Pts',(31.5074931621648,0.122957581810777,24.4443309767673));
#56921=CARTESIAN_POINT('Ctrl Pts',(31.4889302469637,-0.269482846800126,
24.4225287307333));
#56922=CARTESIAN_POINT('Ctrl Pts',(31.4401374224707,-0.464284058469581,
24.4117064411961));
#56923=CARTESIAN_POINT('Ctrl Pts',(31.2732400969951,-0.815428064678723,
24.3921984408512));
#56924=CARTESIAN_POINT('Ctrl Pts',(31.1598920572171,-0.96991270557316,24.3830299796895));
#56925=CARTESIAN_POINT('Ctrl Pts',(30.8768520990815,-1.23274788918355,24.3621112360319));
#56926=CARTESIAN_POINT('Ctrl Pts',(30.7081704356177,-1.33679806788068,24.351105252973));
#56927=CARTESIAN_POINT('Ctrl Pts',(30.3563528915165,-1.46803396077468,24.330532982021));
#56928=CARTESIAN_POINT('Ctrl Pts',(30.1788031709794,-1.50000000000002,24.3211026715747));
#56929=CARTESIAN_POINT('Ctrl Pts',(29.9999999999999,-1.50000000000001,24.3125));
#56930=CARTESIAN_POINT('Origin',(30.,-1.32966554433622E-14,16.));
#56931=CARTESIAN_POINT('',(29.9999999999999,-1.50000000000001,23.75));
#56932=CARTESIAN_POINT('',(30.,-1.50000000000001,23.8125));
#56933=CARTESIAN_POINT('',(30.,-1.50000000000001,16.));
#56934=CARTESIAN_POINT('Ctrl Pts',(29.9999999999998,-1.50000000000001,23.75));
#56935=CARTESIAN_POINT('Ctrl Pts',(30.1539214445734,-1.50000000000004,23.7574055489549));
#56936=CARTESIAN_POINT('Ctrl Pts',(30.3071622224275,-1.47631426128188,23.7654362865035));
#56937=CARTESIAN_POINT('Ctrl Pts',(30.6423330661034,-1.36978679250727,23.7845212975935));
#56938=CARTESIAN_POINT('Ctrl Pts',(30.8166966283757,-1.27354330571266,23.7955837985834));
#56939=CARTESIAN_POINT('Ctrl Pts',(31.1127372375018,-1.02370190976136,23.8167670978074));
#56940=CARTESIAN_POINT('Ctrl Pts',(31.2333636655921,-0.874601042154043,
23.8264110532137));
#56941=CARTESIAN_POINT('Ctrl Pts',(31.4166526755054,-0.531631844802988,
23.8454648975109));
#56942=CARTESIAN_POINT('Ctrl Pts',(31.4745582697856,-0.339396978512901,
23.8561446123048));
#56943=CARTESIAN_POINT('Ctrl Pts',(31.511699941184,0.0525578729813968,23.8779198818323));
#56944=CARTESIAN_POINT('Ctrl Pts',(31.4920858025539,0.248369535334408,23.8887983075186));
#56945=CARTESIAN_POINT('Ctrl Pts',(31.3802343334373,0.617537171179423,23.909307620621));
#56946=CARTESIAN_POINT('Ctrl Pts',(31.2906053859832,0.78786629286171,23.9181242275504));
#56947=CARTESIAN_POINT('Ctrl Pts',(31.0463195284336,1.0933231170364,23.9383623481344));
#56948=CARTESIAN_POINT('Ctrl Pts',(30.8911113639651,1.22312916938911,23.9494355281055));
#56949=CARTESIAN_POINT('Ctrl Pts',(30.5456512461468,1.41045613992281,23.9712600127329));
#56950=CARTESIAN_POINT('Ctrl Pts',(30.3601397930707,1.4688221637187,23.9818067151192));
#56951=CARTESIAN_POINT('Ctrl Pts',(29.9746198000426,1.51244309002935,24.0015667468295));
#56952=CARTESIAN_POINT('Ctrl Pts',(29.7781833324316,1.4963071428617,24.0107747387592));
#56953=CARTESIAN_POINT('Ctrl Pts',(29.3999877237922,1.38893180194388,24.0319533318226));
#56954=CARTESIAN_POINT('Ctrl Pts',(29.222220687541,1.29776778429998,24.0430384861654));
#56955=CARTESIAN_POINT('Ctrl Pts',(28.9180417312452,1.05625627096343,24.0643819561719));
#56956=CARTESIAN_POINT('Ctrl Pts',(28.7928010889864,0.910453809129913,24.0744192328261));
#56957=CARTESIAN_POINT('Ctrl Pts',(28.5994385143727,0.572669994103534,24.0931850003275));
#56958=CARTESIAN_POINT('Ctrl Pts',(28.5359684061524,0.382240685005912,24.1037644063885));
#56959=CARTESIAN_POINT('Ctrl Pts',(28.4873420883061,-0.00897112678811804,
24.1254983959326));
#56960=CARTESIAN_POINT('Ctrl Pts',(28.5013820601517,-0.205827079960202,
24.1364348377755));
#56961=CARTESIAN_POINT('Ctrl Pts',(28.6028303892674,-0.578036208077185,
24.1571131226709));
#56962=CARTESIAN_POINT('Ctrl Pts',(28.6873275910153,-0.750394994115161,
24.1660216580016));
#56963=CARTESIAN_POINT('Ctrl Pts',(28.922674074919,-1.0628953635868,24.1860253368065));
#56964=CARTESIAN_POINT('Ctrl Pts',(29.0745736829203,-1.19747470970914,24.197071925274));
#56965=CARTESIAN_POINT('Ctrl Pts',(29.4156235588556,-1.39492862582615,24.2189655260838));
#56966=CARTESIAN_POINT('Ctrl Pts',(29.5999664963488,-1.45853020454807,24.2296014403193));
#56967=CARTESIAN_POINT('Ctrl Pts',(29.8606029709014,-1.49514680076604,24.2431584462207));
#56968=CARTESIAN_POINT('Ctrl Pts',(29.9303308703141,-1.50000000000001,24.2466480424351));
#56969=CARTESIAN_POINT('Ctrl Pts',(29.9999999999999,-1.50000000000001,24.25));
#56970=CARTESIAN_POINT('Ctrl Pts',(29.9999999999999,-1.50000000000001,24.3125));
#56971=CARTESIAN_POINT('Ctrl Pts',(29.9792133017942,-1.50000000000001,24.3114998995163));
#56972=CARTESIAN_POINT('Ctrl Pts',(29.9584107993835,-1.49956791710601,24.3104870363498));
#56973=CARTESIAN_POINT('Ctrl Pts',(29.7464034347025,-1.4907415866322,24.3000416514142));
#56974=CARTESIAN_POINT('Ctrl Pts',(29.5585103106211,-1.44626636462019,24.2897662164333));
#56975=CARTESIAN_POINT('Ctrl Pts',(29.2028124426411,-1.28608329400307,24.2682031650416));
#56976=CARTESIAN_POINT('Ctrl Pts',(29.0395645726164,-1.16922656097766,24.2571028778712));
#56977=CARTESIAN_POINT('Ctrl Pts',(28.7720346147835,-0.882829614311603,
24.2362758660328));
#56978=CARTESIAN_POINT('Ctrl Pts',(28.6687223598358,-0.717623891574991,
24.2273679939764));
#56979=CARTESIAN_POINT('Ctrl Pts',(28.5302095932634,-0.356628416668571,
24.2073126898149));
#56980=CARTESIAN_POINT('Ctrl Pts',(28.4965070465723,-0.164202501526158,
24.1966223611959));
#56981=CARTESIAN_POINT('Ctrl Pts',(28.504169008249,0.22811087427228,24.1748271736516));
#56982=CARTESIAN_POINT('Ctrl Pts',(28.547551398078,0.424213342298486,24.1639325920946));
#56983=CARTESIAN_POINT('Ctrl Pts',(28.7047478969298,0.780036844220854,24.1441646197656));
#56984=CARTESIAN_POINT('Ctrl Pts',(28.8139070776359,0.937725434330763,24.1351846602695));
#56985=CARTESIAN_POINT('Ctrl Pts',(29.089396967151,1.20794416549895,24.1144240709145));
#56986=CARTESIAN_POINT('Ctrl Pts',(29.2546507832928,1.31634974323744,24.10346202693));
#56987=CARTESIAN_POINT('Ctrl Pts',(29.6203184116569,1.46471395475137,24.0817476068599));
#56988=CARTESIAN_POINT('Ctrl Pts',(29.817562104219,1.50206749812624,24.0713349778568));
#56989=CARTESIAN_POINT('Ctrl Pts',(30.2070481745296,1.49784204922514,24.0524784469813));
#56990=CARTESIAN_POINT('Ctrl Pts',(30.3956551706626,1.45939464529562,24.0423361052064));
#56991=CARTESIAN_POINT('Ctrl Pts',(30.7551447714595,1.31111335433136,24.0209212289748));
#56992=CARTESIAN_POINT('Ctrl Pts',(30.9215534250012,1.20000288285394,24.0098284869129));
#56993=CARTESIAN_POINT('Ctrl Pts',(31.1989915137811,0.922095691461922,23.9887605964375));
#56994=CARTESIAN_POINT('Ctrl Pts',(31.3083178283937,0.759038041694919,23.9796687800942));
#56995=CARTESIAN_POINT('Ctrl Pts',(31.4580557742773,0.401642541393168,23.9598134745218));
#56996=CARTESIAN_POINT('Ctrl Pts',(31.4975752946798,0.210938880716583,23.9492188267065));
#56997=CARTESIAN_POINT('Ctrl Pts',(31.5023006219625,-0.182594498957542,
23.927355861169));
#56998=CARTESIAN_POINT('Ctrl Pts',(31.4644403140633,-0.381679718202,23.916295571211));
#56999=CARTESIAN_POINT('Ctrl Pts',(31.3164762945118,-0.74375638752885,23.8961802006929));
#57000=CARTESIAN_POINT('Ctrl Pts',(31.2115088567194,-0.904729197971778,
23.8873240471024));
#57001=CARTESIAN_POINT('Ctrl Pts',(30.9436055459159,-1.18225533242814,23.8667254837612));
#57002=CARTESIAN_POINT('Ctrl Pts',(30.7818828902994,-1.29490194314203,23.8558155263452));
#57003=CARTESIAN_POINT('Ctrl Pts',(30.4211554702292,-1.45331769745592,23.8340595826352));
#57004=CARTESIAN_POINT('Ctrl Pts',(30.225061216149,-1.49628795964726,23.8234313750427));
#57005=CARTESIAN_POINT('Ctrl Pts',(30.01751075903,-1.49992336974507,23.8133446154048));
#57006=CARTESIAN_POINT('Ctrl Pts',(30.0087538759465,-1.50000000000001,23.8129211710528));
#57007=CARTESIAN_POINT('Ctrl Pts',(30.,-1.50000000000001,23.8125));
#57008=CARTESIAN_POINT('Origin',(30.,-1.32966554433622E-14,16.));
#57009=CARTESIAN_POINT('',(30.,-1.50000000000001,23.25));
#57010=CARTESIAN_POINT('',(30.0000000000001,-1.50000000000001,23.3125));
#57011=CARTESIAN_POINT('',(30.,-1.50000000000001,16.));
#57012=CARTESIAN_POINT('Ctrl Pts',(30.,-1.50000000000001,23.25));
#57013=CARTESIAN_POINT('Ctrl Pts',(30.1848807806478,-1.50000000000001,23.2588950807062));
#57014=CARTESIAN_POINT('Ctrl Pts',(30.3682821495602,-1.46581977714696,23.268668433817));
#57015=CARTESIAN_POINT('Ctrl Pts',(30.7253175152828,-1.32777981441322,23.2896807492688));
#57016=CARTESIAN_POINT('Ctrl Pts',(30.8938177244611,-1.22072861570022,23.3007613637715));
#57017=CARTESIAN_POINT('Ctrl Pts',(31.17812266521,-0.948849031570725,23.3219922022812));
#57018=CARTESIAN_POINT('Ctrl Pts',(31.2916923057403,-0.787278580688064,
23.3312623010729));
#57019=CARTESIAN_POINT('Ctrl Pts',(31.4491725851422,-0.432421790169133,
23.3509765672128));
#57020=CARTESIAN_POINT('Ctrl Pts',(31.4926555401856,-0.243004803835009,
23.3614997331203));
#57021=CARTESIAN_POINT('Ctrl Pts',(31.5058959055076,0.149477495401521,23.3833043053001));
#57022=CARTESIAN_POINT('Ctrl Pts',(31.4725342594551,0.348889338242185,23.3943827410135));
#57023=CARTESIAN_POINT('Ctrl Pts',(31.3327988700423,0.714215497781599,23.4146786387656));
#57024=CARTESIAN_POINT('Ctrl Pts',(31.2311812032015,0.877867947558743,23.4234833208414));
#57025=CARTESIAN_POINT('Ctrl Pts',(30.9693523131294,1.16116792111582,23.4439500128983));
#57026=CARTESIAN_POINT('Ctrl Pts',(30.8105149834806,1.27711053175663,23.4548127055575));
#57027=CARTESIAN_POINT('Ctrl Pts',(30.4538126686857,1.44345770015622,23.4765953083576));
#57028=CARTESIAN_POINT('Ctrl Pts',(30.2587086794859,1.49084210066152,23.487298486762));
#57029=CARTESIAN_POINT('Ctrl Pts',(29.8701963712835,1.50640033026212,23.5064229669502));
#57030=CARTESIAN_POINT('Ctrl Pts',(29.6806119299331,1.47787523708767,23.5159811423084));
#57031=CARTESIAN_POINT('Ctrl Pts',(29.3158918902727,1.34932104216597,23.5370996932649));
#57032=CARTESIAN_POINT('Ctrl Pts',(29.1450773397405,1.24811033609704,23.5481294207781));
#57033=CARTESIAN_POINT('Ctrl Pts',(28.8572342555358,0.990033097118328,23.5691470898178));
#57034=CARTESIAN_POINT('Ctrl Pts',(28.741208429162,0.837555866674711,23.578469118518));
#57035=CARTESIAN_POINT('Ctrl Pts',(28.5682103547001,0.489415671302002,23.5978102404832));
#57036=CARTESIAN_POINT('Ctrl Pts',(28.5160198061383,0.295515658346084,23.6085824634252));
#57037=CARTESIAN_POINT('Ctrl Pts',(28.4905622848027,-0.0968477988030621,
23.6303804332668));
#57038=CARTESIAN_POINT('Ctrl Pts',(28.5157978904665,-0.291438773395986,
23.6411910429664));
#57039=CARTESIAN_POINT('Ctrl Pts',(28.6382130227664,-0.657431308298791,
23.6615239615721));
#57040=CARTESIAN_POINT('Ctrl Pts',(28.733169022031,-0.825722839750627,23.6703196450362));
#57041=CARTESIAN_POINT('Ctrl Pts',(28.9866100524997,-1.12380536152502,23.6907934023492));
#57042=CARTESIAN_POINT('Ctrl Pts',(29.1450855427347,-1.24860164286396,23.7018846212987));
#57043=CARTESIAN_POINT('Ctrl Pts',(29.4947960835532,-1.42537206508902,23.723620367045));
#57044=CARTESIAN_POINT('Ctrl Pts',(29.6813612118254,-1.47831159941945,23.7340670285844));
#57045=CARTESIAN_POINT('Ctrl Pts',(29.9152096611065,-1.49820471212254,23.7458706538102));
#57046=CARTESIAN_POINT('Ctrl Pts',(29.957628226374,-1.50000000000001,23.7479613870909));
#57047=CARTESIAN_POINT('Ctrl Pts',(29.9999999999998,-1.50000000000001,23.75));
#57048=CARTESIAN_POINT('Ctrl Pts',(30.,-1.50000000000001,23.8125));
#57049=CARTESIAN_POINT('Ctrl Pts',(29.8186899108673,-1.50000000000001,23.8037767142694));
#57050=CARTESIAN_POINT('Ctrl Pts',(29.6387564217711,-1.46712852254306,23.7942065636429));
#57051=CARTESIAN_POINT('Ctrl Pts',(29.284195027604,-1.33291119731626,23.7734194615783));
#57052=CARTESIAN_POINT('Ctrl Pts',(29.1150531352934,-1.22715164870581,23.762343853251));
#57053=CARTESIAN_POINT('Ctrl Pts',(28.8285848658366,-0.957196675383623,
23.7410623929517));
#57054=CARTESIAN_POINT('Ctrl Pts',(28.713664846415,-0.796095622176884,23.7317275345654));
#57055=CARTESIAN_POINT('Ctrl Pts',(28.5537507892143,-0.442046290271719,
23.7120581272374));
#57056=CARTESIAN_POINT('Ctrl Pts',(28.50903084701,-0.253050072432249,23.7015583373574));
#57057=CARTESIAN_POINT('Ctrl Pts',(28.493125704307,0.139065210502765,23.6797741549721));
#57058=CARTESIAN_POINT('Ctrl Pts',(28.5250759127101,0.338559440554235,23.6686911421915));
#57059=CARTESIAN_POINT('Ctrl Pts',(28.6622225705316,0.704891738980156,23.6483393478345));
#57060=CARTESIAN_POINT('Ctrl Pts',(28.7627930544851,0.869391639366899,23.6395420458263));
#57061=CARTESIAN_POINT('Ctrl Pts',(29.0227223626785,1.15448356589741,23.6191169709735));
#57062=CARTESIAN_POINT('Ctrl Pts',(29.1806474642266,1.27143845898823,23.6082700489523));
#57063=CARTESIAN_POINT('Ctrl Pts',(29.5360600403599,1.4402358268239,23.5864814376371));
#57064=CARTESIAN_POINT('Ctrl Pts',(29.7308346201,1.48899068833401,23.5757560395914));
#57065=CARTESIAN_POINT('Ctrl Pts',(30.1191927262396,1.50727161649964,23.5565633479378));
#57066=CARTESIAN_POINT('Ctrl Pts',(30.3089226794933,1.48009155403507,23.5470839383266));
#57067=CARTESIAN_POINT('Ctrl Pts',(30.6746275130695,1.35410584970156,23.5259893534154));
#57068=CARTESIAN_POINT('Ctrl Pts',(30.8462644331352,1.25401826984556,23.5149512576394));
#57069=CARTESIAN_POINT('Ctrl Pts',(31.1359831388577,0.997812339501797,23.4938953285128));
#57070=CARTESIAN_POINT('Ctrl Pts',(31.2530579642409,0.846112941875841,23.4845062745487));
#57071=CARTESIAN_POINT('Ctrl Pts',(31.4284239202414,0.499151075957345,23.465230615331));
#57072=CARTESIAN_POINT('Ctrl Pts',(31.4819315716114,0.305618089705,23.4544787827614));
#57073=CARTESIAN_POINT('Ctrl Pts',(31.5100720569101,-0.086682490418841,
23.4326843060879));
#57074=CARTESIAN_POINT('Ctrl Pts',(31.4861228872238,-0.281567854400411,
23.4218573414222));
#57075=CARTESIAN_POINT('Ctrl Pts',(31.3661326726942,-0.648296896097567,
23.4014835057724));
#57076=CARTESIAN_POINT('Ctrl Pts',(31.2724103712455,-0.817054396960877,
23.3926895837254));
#57077=CARTESIAN_POINT('Ctrl Pts',(31.0210775409326,-1.11685004948265,23.3722696702745));
#57078=CARTESIAN_POINT('Ctrl Pts',(30.8633432283804,-1.24281066274781,23.3611817686994));
#57079=CARTESIAN_POINT('Ctrl Pts',(30.5145869816219,-1.42202815813894,23.3394239621929));
#57080=CARTESIAN_POINT('Ctrl Pts',(30.3282514191413,-1.47622279958149,23.3289534815563));
#57081=CARTESIAN_POINT('Ctrl Pts',(30.0912045055574,-1.4979228580024,23.3169457772084));
#57082=CARTESIAN_POINT('Ctrl Pts',(30.0455768509778,-1.50000000000001,23.3146928172651));
#57083=CARTESIAN_POINT('Ctrl Pts',(30.0000000000002,-1.50000000000001,23.3125));
#57084=CARTESIAN_POINT('Origin',(30.,-1.32966554433622E-14,16.));
#57085=CARTESIAN_POINT('',(30.0000000000001,-1.50000000000001,22.75));
#57086=CARTESIAN_POINT('',(30.,-1.50000000000001,22.8125));
#57087=CARTESIAN_POINT('',(30.,-1.50000000000001,16.));
#57088=CARTESIAN_POINT('Ctrl Pts',(30.0000000000001,-1.50000000000001,22.75));
#57089=CARTESIAN_POINT('Ctrl Pts',(30.0238190927805,-1.50000000000001,22.7511459966357));
#57090=CARTESIAN_POINT('Ctrl Pts',(30.0476581179369,-1.49943265781826,22.7523087117734));
#57091=CARTESIAN_POINT('Ctrl Pts',(30.2627622738244,-1.48916810759789,22.7629430416939));
#57092=CARTESIAN_POINT('Ctrl Pts',(30.4504917710081,-1.44350305068679,22.7732436551414));
#57093=CARTESIAN_POINT('Ctrl Pts',(30.8053949324493,-1.28097942369943,22.7948334866517));
#57094=CARTESIAN_POINT('Ctrl Pts',(30.9679955997388,-1.16299746502374,22.8059338915341));
#57095=CARTESIAN_POINT('Ctrl Pts',(31.2335580340327,-0.874942371993705,
22.8267123004732));
#57096=CARTESIAN_POINT('Ctrl Pts',(31.3356903480274,-0.709308500806453,
22.8355939721774));
#57097=CARTESIAN_POINT('Ctrl Pts',(31.4719653898389,-0.347606806174152,
22.8556885107681));
#57098=CARTESIAN_POINT('Ctrl Pts',(31.5044992018676,-0.154858219876142,
22.8663967655625));
#57099=CARTESIAN_POINT('Ctrl Pts',(31.4943665307067,0.237510688978279,22.8881950382766));
#57100=CARTESIAN_POINT('Ctrl Pts',(31.4497537465181,0.433331528903234,22.899073973828));
#57101=CARTESIAN_POINT('Ctrl Pts',(31.2903519524536,0.78810181728577,22.9187834342937));
#57102=CARTESIAN_POINT('Ctrl Pts',(31.1802475750943,0.945060620681391,22.9278003293086));
#57103=CARTESIAN_POINT('Ctrl Pts',(30.9030507590494,1.21362000516214,22.948596950241));
#57104=CARTESIAN_POINT('Ctrl Pts',(30.7370141991215,1.32105257322674,22.9595696259569));
#57105=CARTESIAN_POINT('Ctrl Pts',(30.3702805499944,1.46712017353723,22.9812715402192));
#57106=CARTESIAN_POINT('Ctrl Pts',(30.1727871861063,1.50321114583692,22.991597574137));
#57107=CARTESIAN_POINT('Ctrl Pts',(29.7831928098337,1.49647610979574,23.0105290266394));
#57108=CARTESIAN_POINT('Ctrl Pts',(29.5947193673977,1.45676699750561,23.0206999902635));
#57109=CARTESIAN_POINT('Ctrl Pts',(29.2359911149794,1.30598838211349,23.0421476062271));
#57110=CARTESIAN_POINT('Ctrl Pts',(29.0702277888966,1.19366882317697,23.05324288572));
#57111=CARTESIAN_POINT('Ctrl Pts',(28.7948557226535,0.913971635465609,23.0742610967597));
#57112=CARTESIAN_POINT('Ctrl Pts',(28.686793719435,0.750466721324838,23.0833074043708));
#57113=CARTESIAN_POINT('Ctrl Pts',(28.5393908078851,0.39231449396832,23.1032047503351));
#57114=CARTESIAN_POINT('Ctrl Pts',(28.50107471408,0.201238476218244,23.1138200846545));
#57115=CARTESIAN_POINT('Ctrl Pts',(28.4989279287216,-0.192576857122968,
23.1356987142846));
#57116=CARTESIAN_POINT('Ctrl Pts',(28.5381471159066,-0.391544240809387,
23.1467524578227));
#57117=CARTESIAN_POINT('Ctrl Pts',(28.6885908974138,-0.752626531003943,
23.1668125850557));
#57118=CARTESIAN_POINT('Ctrl Pts',(28.7945746463293,-0.912795946069086,
23.1756927219105));
#57119=CARTESIAN_POINT('Ctrl Pts',(29.0643193882896,-1.1885583990927,23.1963308899987));
#57120=CARTESIAN_POINT('Ctrl Pts',(29.2269067570048,-1.30018824275338,23.2072542074138));
#57121=CARTESIAN_POINT('Ctrl Pts',(29.5888237919401,-1.45617120236401,23.228999808865));
#57122=CARTESIAN_POINT('Ctrl Pts',(29.7851989650319,-1.49779418034797,23.2396041076185));
#57123=CARTESIAN_POINT('Ctrl Pts',(29.9893352495882,-1.49997157194577,23.2494861022884));
#57124=CARTESIAN_POINT('Ctrl Pts',(29.9946682024469,-1.50000000000001,23.2497434737706));
#57125=CARTESIAN_POINT('Ctrl Pts',(30.,-1.50000000000001,23.25));
#57126=CARTESIAN_POINT('Ctrl Pts',(30.0000000000003,-1.50000000000001,23.3125));
#57127=CARTESIAN_POINT('Ctrl Pts',(29.8497176527518,-1.50000000000002,23.3052695371968));
#57128=CARTESIAN_POINT('Ctrl Pts',(29.7000480379928,-1.47742120454004,23.2974413657365));
#57129=CARTESIAN_POINT('Ctrl Pts',(29.3674490033452,-1.37435151569836,23.2785761403087));
#57130=CARTESIAN_POINT('Ctrl Pts',(29.1922818901849,-1.27927791742795,23.2675074753621));
#57131=CARTESIAN_POINT('Ctrl Pts',(28.8943459539799,-1.03136235914611,23.2462864826624));
#57132=CARTESIAN_POINT('Ctrl Pts',(28.7726494682524,-0.883034040962408,
23.2365574467202));
#57133=CARTESIAN_POINT('Ctrl Pts',(28.5870020748245,-0.541267982453404,
23.2175704434697));
#57134=CARTESIAN_POINT('Ctrl Pts',(28.5277906685824,-0.349440299767995,
23.2069133499871));
#57135=CARTESIAN_POINT('Ctrl Pts',(28.487963650694,0.0423711662580389,23.185146046319));
#57136=CARTESIAN_POINT('Ctrl Pts',(28.5062787794266,0.238440842104816,23.1742532865498));
#57137=CARTESIAN_POINT('Ctrl Pts',(28.6157002622386,0.608326552071247,23.1537040804405));
#57138=CARTESIAN_POINT('Ctrl Pts',(28.704120723826,0.779127514930934,23.1448722564411));
#57139=CARTESIAN_POINT('Ctrl Pts',(28.9463114752997,1.08624863564316,23.1246887062359));
#57140=CARTESIAN_POINT('Ctrl Pts',(29.100754465216,1.21718400346422,23.1136209708684));
#57141=CARTESIAN_POINT('Ctrl Pts',(29.4452036060534,1.40690072974557,23.0917787447896));
#57142=CARTESIAN_POINT('Ctrl Pts',(29.630453412942,1.46649956876065,23.0812103859941));
#57143=CARTESIAN_POINT('Ctrl Pts',(30.0154678344856,1.51253258675255,23.0614076760565));
#57144=CARTESIAN_POINT('Ctrl Pts',(30.2116518417758,1.49773354664468,23.052253938977));
#57145=CARTESIAN_POINT('Ctrl Pts',(30.5903886500576,1.39306917025536,23.031124612004));
#57146=CARTESIAN_POINT('Ctrl Pts',(30.7689034771477,1.3030667277533,23.0200357455338));
#57147=CARTESIAN_POINT('Ctrl Pts',(31.0748241700176,1.06351798971685,22.9986629977234));
#57148=CARTESIAN_POINT('Ctrl Pts',(31.2011381587389,0.918481956232081,22.9885569343996));
#57149=CARTESIAN_POINT('Ctrl Pts',(31.3967520547264,0.581861797904625,22.9697948964873));
#57150=CARTESIAN_POINT('Ctrl Pts',(31.4615014415134,0.391859484339943,22.9592699713522));
#57151=CARTESIAN_POINT('Ctrl Pts',(31.5127002734739,0.000740375396987882,
22.9375411319665));
#57152=CARTESIAN_POINT('Ctrl Pts',(31.4999079686113,-0.196327016676456,
22.9265929435179));
#57153=CARTESIAN_POINT('Ctrl Pts',(31.4007804390091,-0.569202940848263,
22.9058776143973));
#57154=CARTESIAN_POINT('Ctrl Pts',(31.3174135571943,-0.742018160934012,
22.8969391404085));
#57155=CARTESIAN_POINT('Ctrl Pts',(31.0853396535684,-1.05432624095891,22.8770982550692));
#57156=CARTESIAN_POINT('Ctrl Pts',(30.9361334950341,-1.18878161757634,22.8661846988469));
#57157=CARTESIAN_POINT('Ctrl Pts',(30.5987439832112,-1.38884930936682,22.8443946025078));
#57158=CARTESIAN_POINT('Ctrl Pts',(30.4148754905707,-1.45440359104526,22.8337272732621));
#57159=CARTESIAN_POINT('Ctrl Pts',(30.1494349053273,-1.49442202191131,22.8198446340705));
#57160=CARTESIAN_POINT('Ctrl Pts',(30.0746909808563,-1.50000000000001,22.816093571492));
#57161=CARTESIAN_POINT('Ctrl Pts',(30.0000000000001,-1.50000000000001,22.8125));
#57162=CARTESIAN_POINT('Origin',(30.,-1.32966554433622E-14,16.));
#57163=CARTESIAN_POINT('',(30.0000000000001,-1.50000000000001,22.25));
#57164=CARTESIAN_POINT('',(30.,-1.50000000000001,22.3125));
#57165=CARTESIAN_POINT('',(30.,-1.50000000000001,16.));
#57166=CARTESIAN_POINT('Ctrl Pts',(30.0000000000002,-1.50000000000001,22.25));
#57167=CARTESIAN_POINT('Ctrl Pts',(30.0511677444063,-1.50000000000001,22.2524618092506));
#57168=CARTESIAN_POINT('Ctrl Pts',(30.1023921263505,-1.49738203467576,22.254999064735));
#57169=CARTESIAN_POINT('Ctrl Pts',(30.3449868915282,-1.47242953219059,22.2673640358856));
#57170=CARTESIAN_POINT('Ctrl Pts',(30.5309019965201,-1.41604718249647,22.2778750569255));
#57171=CARTESIAN_POINT('Ctrl Pts',(30.8779534991821,-1.23257211766357,22.2996691097112));
#57172=CARTESIAN_POINT('Ctrl Pts',(31.0343750352224,-1.10459007945506,22.3107500009898));
#57173=CARTESIAN_POINT('Ctrl Pts',(31.2820199524192,-0.801819415517196,
22.3310751188442));
#57174=CARTESIAN_POINT('Ctrl Pts',(31.3735944009353,-0.632242273686504,
22.3398754292397));
#57175=CARTESIAN_POINT('Ctrl Pts',(31.4893318529591,-0.264232559817084,
22.3603204133435));
#57176=CARTESIAN_POINT('Ctrl Pts',(31.511019003439,-0.0688512669519718,
22.3711749296138));
#57177=CARTESIAN_POINT('Ctrl Pts',(31.4781740542578,0.32329452926424,22.3929608071814));
#57178=CARTESIAN_POINT('Ctrl Pts',(31.422363807823,0.516161881943181,22.403675660108));
#57179=CARTESIAN_POINT('Ctrl Pts',(31.2428531453717,0.861044634974944,22.4228358130542));
#57180=CARTESIAN_POINT('Ctrl Pts',(31.1239285676202,1.01138399102137,22.4323522946618));
#57181=CARTESIAN_POINT('Ctrl Pts',(30.8309115401787,1.26428053578999,22.4534749869891));
#57182=CARTESIAN_POINT('Ctrl Pts',(30.6578432463629,1.3623737449238,22.4645265505225));
#57183=CARTESIAN_POINT('Ctrl Pts',(30.2831279004866,1.48623532989505,22.4859956505893));
#57184=CARTESIAN_POINT('Ctrl Pts',(30.0851137662052,1.5105602610331,22.49561162143));
#57185=CARTESIAN_POINT('Ctrl Pts',(29.6966286981958,1.48149502237994,22.5151099857196));
#57186=CARTESIAN_POINT('Ctrl Pts',(29.5097167303907,1.43054672747056,22.5255180223776));
#57187=CARTESIAN_POINT('Ctrl Pts',(29.1585275612845,1.25766527467259,22.547216881732));
#57188=CARTESIAN_POINT('Ctrl Pts',(28.9988940242273,1.13472310971196,22.5583123140024));
#57189=CARTESIAN_POINT('Ctrl Pts',(28.7421191463059,0.839368453848379,22.5788706970727));
#57190=CARTESIAN_POINT('Ctrl Pts',(28.6452032661271,0.671810533827306,22.5876771925652));
#57191=CARTESIAN_POINT('Ctrl Pts',(28.5189623058816,0.306989072921277,22.6079450515044));
#57192=CARTESIAN_POINT('Ctrl Pts',(28.4917024287485,0.112879611784448,22.6187289104564));
#57193=CARTESIAN_POINT('Ctrl Pts',(28.5129271256702,-0.27954553838217,22.6405303076879));
#57194=CARTESIAN_POINT('Ctrl Pts',(28.5630339289139,-0.474005993650327,
22.6513336663139));
#57195=CARTESIAN_POINT('Ctrl Pts',(28.7322894218787,-0.823994430176359,
22.6707774683431));
#57196=CARTESIAN_POINT('Ctrl Pts',(28.8466683628132,-0.977702516203741,
22.680002042295));
#57197=CARTESIAN_POINT('Ctrl Pts',(29.1315598866997,-1.23870928805523,22.7009590802358));
#57198=CARTESIAN_POINT('Ctrl Pts',(29.301068288962,-1.34167114530826,22.7119746086325));
#57199=CARTESIAN_POINT('Ctrl Pts',(29.6506233621551,-1.46928601783117,22.732337442503));
#57200=CARTESIAN_POINT('Ctrl Pts',(29.8247316115896,-1.50000000000001,22.7415673957309));
#57201=CARTESIAN_POINT('Ctrl Pts',(30.0000000000001,-1.50000000000001,22.75));
#57202=CARTESIAN_POINT('Ctrl Pts',(30.0000000000001,-1.50000000000001,22.8125));
#57203=CARTESIAN_POINT('Ctrl Pts',(29.8821180181442,-1.50000000000001,22.8068284005036));
#57204=CARTESIAN_POINT('Ctrl Pts',(29.7644054408515,-1.48610745961779,22.8007790475884));
#57205=CARTESIAN_POINT('Ctrl Pts',(29.4561358619788,-1.41197523055228,22.7838881919746));
#57206=CARTESIAN_POINT('Ctrl Pts',(29.2741386603191,-1.32762177587115,22.7727886960081));
#57207=CARTESIAN_POINT('Ctrl Pts',(28.9596308471203,-1.09734948081223,22.7512604791499));
#57208=CARTESIAN_POINT('Ctrl Pts',(28.8283658665089,-0.955949757636784,
22.7410172197375));
#57209=CARTESIAN_POINT('Ctrl Pts',(28.6210784753189,-0.623528783846783,
22.7218101845402));
#57210=CARTESIAN_POINT('Ctrl Pts',(28.550139211662,-0.43377020073728,22.7115983444854));
#57211=CARTESIAN_POINT('Ctrl Pts',(28.4878128315539,-0.0419315259951405,
22.6898295292219));
#57212=CARTESIAN_POINT('Ctrl Pts',(28.4952899772074,0.155946448584049,22.678836308412));
#57213=CARTESIAN_POINT('Ctrl Pts',(28.5845546436209,0.531607574681399,22.657966245851));
#57214=CARTESIAN_POINT('Ctrl Pts',(28.6631729955745,0.706378968214403,22.6488631478995));
#57215=CARTESIAN_POINT('Ctrl Pts',(28.886581089556,1.02462509962909,22.6292742506491));
#57216=CARTESIAN_POINT('Ctrl Pts',(29.0320840520478,1.16304620087307,22.6184287055121));
#57217=CARTESIAN_POINT('Ctrl Pts',(29.3643456686259,1.37241961531272,22.5966268328521));
#57218=CARTESIAN_POINT('Ctrl Pts',(29.5468906971467,1.44301653433814,22.585883105544));
#57219=CARTESIAN_POINT('Ctrl Pts',(29.9272228832809,1.51053148619831,22.5657089493774));
#57220=CARTESIAN_POINT('Ctrl Pts',(30.1212939503538,1.50741198602448,22.5568701305933));
#57221=CARTESIAN_POINT('Ctrl Pts',(30.5044378408363,1.42661367919911,22.5361917141558));
#57222=CARTESIAN_POINT('Ctrl Pts',(30.6892182911204,1.34709011542225,22.5250924727137));
#57223=CARTESIAN_POINT('Ctrl Pts',(31.0107046879826,1.12481571216727,22.5034506622537));
#57224=CARTESIAN_POINT('Ctrl Pts',(31.1460355364563,0.986589014961116,22.4930999232927));
#57225=CARTESIAN_POINT('Ctrl Pts',(31.3611183370781,0.66090197936205,22.473704885123));
#57226=CARTESIAN_POINT('Ctrl Pts',(31.4365760335144,0.475089538086611,22.463893863227));
#57227=CARTESIAN_POINT('Ctrl Pts',(31.5103576978905,0.0866802952431828,
22.4423155719579));
#57228=CARTESIAN_POINT('Ctrl Pts',(31.5086976507443,-0.111919508747406,
22.431282249514));
#57229=CARTESIAN_POINT('Ctrl Pts',(31.4301969979147,-0.490528747223499,
22.410248402932));
#57230=CARTESIAN_POINT('Ctrl Pts',(31.3566667795852,-0.667467593155736,
22.4008985610562));
#57231=CARTESIAN_POINT('Ctrl Pts',(31.1425983489439,-0.991976419659515,
22.3815850548154));
#57232=CARTESIAN_POINT('Ctrl Pts',(31.0011829334274,-1.13452992378446,22.370821382905));
#57233=CARTESIAN_POINT('Ctrl Pts',(30.6747026750166,-1.35372782384191,22.3490247635913));
#57234=CARTESIAN_POINT('Ctrl Pts',(30.4937271061129,-1.42970164427305,22.3382071885718));
#57235=CARTESIAN_POINT('Ctrl Pts',(30.2032733713701,-1.48966742655325,22.322567010569));
#57236=CARTESIAN_POINT('Ctrl Pts',(30.1016602333963,-1.50000000000001,22.3173911302598));
#57237=CARTESIAN_POINT('Ctrl Pts',(30.,-1.50000000000001,22.3125));
#57238=CARTESIAN_POINT('Origin',(30.,-1.32966554433622E-14,16.));
#57239=CARTESIAN_POINT('',(30.,-1.50000000000001,21.75));
#57240=CARTESIAN_POINT('',(29.9999999999999,-1.50000000000001,21.8125));
#57241=CARTESIAN_POINT('',(30.,-1.50000000000001,16.));
#57242=CARTESIAN_POINT('Ctrl Pts',(30.,-1.50000000000001,21.75));
#57243=CARTESIAN_POINT('Ctrl Pts',(30.0799345840677,-1.50000000000001,21.7538458544691));
#57244=CARTESIAN_POINT('Ctrl Pts',(30.1599122998412,-1.4936114408734,21.7578712440892));
#57245=CARTESIAN_POINT('Ctrl Pts',(30.4303228176761,-1.44993500309235,21.7720946105773));
#57246=CARTESIAN_POINT('Ctrl Pts',(30.6136742893428,-1.38234553687229,21.7827935975436));
#57247=CARTESIAN_POINT('Ctrl Pts',(30.9490281775211,-1.17851150378185,21.8045903754862));
#57248=CARTESIAN_POINT('Ctrl Pts',(31.096754819913,-1.04244516916321,21.8154774972882));
#57249=CARTESIAN_POINT('Ctrl Pts',(31.3253413942278,-0.727732251316939,
21.8352173994684));
#57250=CARTESIAN_POINT('Ctrl Pts',(31.4067935410376,-0.554135842314364,
21.8442146754271));
#57251=CARTESIAN_POINT('Ctrl Pts',(31.5019658936778,-0.180133518226551,
21.8649925823208));
#57252=CARTESIAN_POINT('Ctrl Pts',(31.5126290136531,0.0172760533687308,
21.8759597807428));
#57253=CARTESIAN_POINT('Ctrl Pts',(31.457072059222,0.408029499969523,21.8976683055539));
#57254=CARTESIAN_POINT('Ctrl Pts',(31.3902144216195,0.597326073407902,21.9080390017153));
#57255=CARTESIAN_POINT('Ctrl Pts',(31.1907422817111,0.931962878929858,21.9269315763413));
#57256=CARTESIAN_POINT('Ctrl Pts',(31.0626495240423,1.07572029471252,21.9370877035676));
#57257=CARTESIAN_POINT('Ctrl Pts',(30.7536327605205,1.31199280194067,21.9585184047354));
#57258=CARTESIAN_POINT('Ctrl Pts',(30.5738554020277,1.39999410781883,21.9696124276475));
#57259=CARTESIAN_POINT('Ctrl Pts',(30.1942124641512,1.50002082255712,21.9906565268663));
#57260=CARTESIAN_POINT('Ctrl Pts',(29.9984550225415,1.51253833676667,21.9997260456303));
#57261=CARTESIAN_POINT('Ctrl Pts',(29.6143176021754,1.46236614670513,22.0196015378309));
#57262=CARTESIAN_POINT('Ctrl Pts',(29.4295365026789,1.40065016331119,22.0302061554976));
#57263=CARTESIAN_POINT('Ctrl Pts',(29.0868629977602,1.20683686352092,22.052076744962));
#57264=CARTESIAN_POINT('Ctrl Pts',(28.9337539891966,1.07396976987892,22.0631339581722));
#57265=CARTESIAN_POINT('Ctrl Pts',(28.6951751765203,0.763999003449345,22.0832228857165));
#57266=CARTESIAN_POINT('Ctrl Pts',(28.60882966791,0.592379173375639,22.0920900459236));
#57267=CARTESIAN_POINT('Ctrl Pts',(28.5036090779159,0.221263029136351,22.1127076094925));
#57268=CARTESIAN_POINT('Ctrl Pts',(28.4875441317865,0.0247675363524192,
22.1236240257582));
#57269=CARTESIAN_POINT('Ctrl Pts',(28.5320098906898,-0.36675262012417,22.1453751455625));
#57270=CARTESIAN_POINT('Ctrl Pts',(28.593470220051,-0.557855368091198,22.155991964894));
#57271=CARTESIAN_POINT('Ctrl Pts',(28.7831869687067,-0.897529793649072,
22.1748627663138));
#57272=CARTESIAN_POINT('Ctrl Pts',(28.9067443386156,-1.04452569047662,22.1847486483138));
#57273=CARTESIAN_POINT('Ctrl Pts',(29.2079650540828,-1.28908351396432,22.2060344096185));
#57274=CARTESIAN_POINT('Ctrl Pts',(29.3845091949262,-1.38211075548827,22.2171124835975));
#57275=CARTESIAN_POINT('Ctrl Pts',(29.7125665428598,-1.47927872450056,22.2355952603595));
#57276=CARTESIAN_POINT('Ctrl Pts',(29.8560312883098,-1.50000000000001,22.2430733021292));
#57277=CARTESIAN_POINT('Ctrl Pts',(30.0000000000002,-1.50000000000001,22.25));
#57278=CARTESIAN_POINT('Ctrl Pts',(30.,-1.50000000000001,22.3125));
#57279=CARTESIAN_POINT('Ctrl Pts',(29.9110895843884,-1.50000000000001,22.3082222956344));
#57280=CARTESIAN_POINT('Ctrl Pts',(29.8221645100457,-1.49209634975764,22.3037243401601));
#57281=CARTESIAN_POINT('Ctrl Pts',(29.5376207680931,-1.44087704391974,22.288611464497));
#57282=CARTESIAN_POINT('Ctrl Pts',(29.3500356587678,-1.36654835932947,22.2775215860335));
#57283=CARTESIAN_POINT('Ctrl Pts',(29.0213968226607,-1.15294073825471,22.2557763976293));
#57284=CARTESIAN_POINT('Ctrl Pts',(28.8818555948118,-1.01818896609304,22.2453196123919));
#57285=CARTESIAN_POINT('Ctrl Pts',(28.6586442869874,-0.699623440719697,
22.2257313109655));
#57286=CARTESIAN_POINT('Ctrl Pts',(28.5785399664869,-0.517856468116547,
22.2162698037842));
#57287=CARTESIAN_POINT('Ctrl Pts',(28.4929509348882,-0.133169441708886,
22.1948983023171));
#57288=CARTESIAN_POINT('Ctrl Pts',(28.4885197532221,0.0660037349236151,
22.1838331258375));
#57289=CARTESIAN_POINT('Ctrl Pts',(28.555761801385,0.44759093437612,22.1626338369791));
#57290=CARTESIAN_POINT('Ctrl Pts',(28.6240637192867,0.626835313372202,22.1529543398));
#57291=CARTESIAN_POINT('Ctrl Pts',(28.8284985352011,0.957663958533704,22.1339287805455));
#57292=CARTESIAN_POINT('Ctrl Pts',(28.9656007252824,1.10432288929781,22.1232585891618));
#57293=CARTESIAN_POINT('Ctrl Pts',(29.2858531479679,1.33342212875051,22.1014865695287));
#57294=CARTESIAN_POINT('Ctrl Pts',(29.4650586076933,1.41487321083335,22.0906020127698));
#57295=CARTESIAN_POINT('Ctrl Pts',(29.8404420905807,1.50363480947233,22.0700757665663));
#57296=CARTESIAN_POINT('Ctrl Pts',(30.0326825220108,1.51172235919918,22.0612531825154));
#57297=CARTESIAN_POINT('Ctrl Pts',(30.4195266402016,1.45401546056375,22.0410381667945));
#57298=CARTESIAN_POINT('Ctrl Pts',(30.6097995465824,1.38502427774371,22.029967235573));
#57299=CARTESIAN_POINT('Ctrl Pts',(30.9454244752463,1.18038733089544,22.0081351140291));
#57300=CARTESIAN_POINT('Ctrl Pts',(31.0891246269642,1.04926948856203,21.997579174969));
#57301=CARTESIAN_POINT('Ctrl Pts',(31.3204408508467,0.737906981306312,21.9778010094235));
#57302=CARTESIAN_POINT('Ctrl Pts',(31.4051230902783,0.560097094369773,21.9686165052427));
#57303=CARTESIAN_POINT('Ctrl Pts',(31.5023434434385,0.179258057369552,21.9474587809649));
#57304=CARTESIAN_POINT('Ctrl Pts',(31.5128623034415,-0.0203042234475934,
21.9363719875862));
#57305=CARTESIAN_POINT('Ctrl Pts',(31.4568810475112,-0.404757677376984,
21.9150134623679));
#57306=CARTESIAN_POINT('Ctrl Pts',(31.3937249627295,-0.586348141727015,
21.9049348418193));
#57307=CARTESIAN_POINT('Ctrl Pts',(31.1987850558466,-0.923274808506461,
21.8861967170992));
#57308=CARTESIAN_POINT('Ctrl Pts',(31.0660220732146,-1.07382111006007,21.8756273134093));
#57309=CARTESIAN_POINT('Ctrl Pts',(30.7521571303647,-1.31243843036869,21.8538982204082));
#57310=CARTESIAN_POINT('Ctrl Pts',(30.5748417786265,-1.39921326582906,21.8429567194739));
#57311=CARTESIAN_POINT('Ctrl Pts',(30.2597272838717,-1.48309858829145,21.8254656184301));
#57312=CARTESIAN_POINT('Ctrl Pts',(30.1300238421579,-1.50000000000003,21.8187557750226));
#57313=CARTESIAN_POINT('Ctrl Pts',(29.9999999999998,-1.50000000000001,21.8125));
#57314=CARTESIAN_POINT('Origin',(30.,-1.32966554433622E-14,16.));
#57315=CARTESIAN_POINT('',(30.,-1.50000000000001,21.25));
#57316=CARTESIAN_POINT('',(29.9999999999999,-1.50000000000001,21.3125));
#57317=CARTESIAN_POINT('',(30.,-1.50000000000001,16.));
#57318=CARTESIAN_POINT('Ctrl Pts',(30.,-1.50000000000001,21.25));
#57319=CARTESIAN_POINT('Ctrl Pts',(30.1075848726609,-1.50000000000001,21.2551761795993));
#57320=CARTESIAN_POINT('Ctrl Pts',(30.2150815962025,-1.48842822791985,21.2606695562356));
#57321=CARTESIAN_POINT('Ctrl Pts',(30.5108359622909,-1.42370950162225,21.2766967872056));
#57322=CARTESIAN_POINT('Ctrl Pts',(30.6910987866292,-1.34546461195666,21.2875431555427));
#57323=CARTESIAN_POINT('Ctrl Pts',(31.0150386063333,-1.12214805976604,21.3093319549459));
#57324=CARTESIAN_POINT('Ctrl Pts',(31.1546840327806,-0.977879417444189,
21.3200581109451));
#57325=CARTESIAN_POINT('Ctrl Pts',(31.3647735631693,-0.650743634461253,
21.3392531532717));
#57326=CARTESIAN_POINT('Ctrl Pts',(31.4361426481554,-0.472861434650035,
21.3487299202974));
#57327=CARTESIAN_POINT('Ctrl Pts',(31.5100129878737,-0.0930141634261118,
21.3698325464765));
#57328=CARTESIAN_POINT('Ctrl Pts',(31.5091680819865,0.105843895299734,21.3808802164057));
#57329=CARTESIAN_POINT('Ctrl Pts',(31.4305088048906,0.492738271362424,21.4023743484091));
#57330=CARTESIAN_POINT('Ctrl Pts',(31.3531309016418,0.676876453829759,21.4120329161916));
#57331=CARTESIAN_POINT('Ctrl Pts',(31.1347020158755,0.999644296815675,21.4315078542742));
#57332=CARTESIAN_POINT('Ctrl Pts',(30.9976338252526,1.13646112591015,21.4419030181452));
#57333=CARTESIAN_POINT('Ctrl Pts',(30.6731866853066,1.35520814296552,21.4635892944733));
#57334=CARTESIAN_POINT('Ctrl Pts',(30.4872391020676,1.43261266999426,21.474685827494));
#57335=CARTESIAN_POINT('Ctrl Pts',(30.1032980730075,1.50870030742653,21.4952717443516));
#57336=CARTESIAN_POINT('Ctrl Pts',(29.9096173130592,1.50952898426713,21.5040838450456));
#57337=CARTESIAN_POINT('Ctrl Pts',(29.5302606487566,1.43771855687004,21.5243303851611));
#57338=CARTESIAN_POINT('Ctrl Pts',(29.3483375586665,1.36492268311026,21.5351052715185));
#57339=CARTESIAN_POINT('Ctrl Pts',(29.0184009025148,1.15151905747937,21.5569072347786));
#57340=CARTESIAN_POINT('Ctrl Pts',(28.8745521744234,1.01139585435745,21.5677204711336));
#57341=CARTESIAN_POINT('Ctrl Pts',(28.6549505368779,0.690580628714703,21.5871975938919));
#57342=CARTESIAN_POINT('Ctrl Pts',(28.5784089748082,0.514933598952509,21.596392577836));
#57343=CARTESIAN_POINT('Ctrl Pts',(28.4935139297613,0.138064010695691,21.6173297771836));
#57344=CARTESIAN_POINT('Ctrl Pts',(28.4883967455728,-0.0601274794615553,
21.6283404155257));
#57345=CARTESIAN_POINT('Ctrl Pts',(28.5553929405263,-0.450590041266374,
21.6500327800704));
#57346=CARTESIAN_POINT('Ctrl Pts',(28.6281760530356,-0.63873783180513,21.6600741404618));
#57347=CARTESIAN_POINT('Ctrl Pts',(28.8386308155265,-0.968434016466414,
21.6793578772949));
#57348=CARTESIAN_POINT('Ctrl Pts',(28.9715505605447,-1.10856330761102,21.6896454618184));
#57349=CARTESIAN_POINT('Ctrl Pts',(29.2889068065357,-1.33562316156644,21.7112214894881));
#57350=CARTESIAN_POINT('Ctrl Pts',(29.4720453487169,-1.41803231498314,21.7223218898575));
#57351=CARTESIAN_POINT('Ctrl Pts',(29.7757758521236,-1.48742065117207,21.7388625842992));
#57352=CARTESIAN_POINT('Ctrl Pts',(29.8878284604463,-1.50000000000001,21.7446031442869));
#57353=CARTESIAN_POINT('Ctrl Pts',(30.,-1.50000000000001,21.75));
#57354=CARTESIAN_POINT('Ctrl Pts',(29.9999999999998,-1.50000000000001,21.8125));
#57355=CARTESIAN_POINT('Ctrl Pts',(29.9405204451645,-1.50000000000001,21.8096382885837));
#57356=CARTESIAN_POINT('Ctrl Pts',(29.8809833669271,-1.49646250510709,21.8066755458243));
#57357=CARTESIAN_POINT('Ctrl Pts',(29.6241950912386,-1.46572084178495,21.7934668790576));
#57358=CARTESIAN_POINT('Ctrl Pts',(29.4333772164259,-1.40302797833686,21.782544681346));
#57359=CARTESIAN_POINT('Ctrl Pts',(29.0921865820648,-1.20964665656295,21.760757435914));
#57360=CARTESIAN_POINT('Ctrl Pts',(28.9439925649252,-1.08269733302756,21.7501010778418));
#57361=CARTESIAN_POINT('Ctrl Pts',(28.7038088414644,-0.77933430694382,21.7301184823344));
#57362=CARTESIAN_POINT('Ctrl Pts',(28.6141674942217,-0.605760578772268,
21.7211533654873));
#57363=CARTESIAN_POINT('Ctrl Pts',(28.5043846389733,-0.22927416638246,21.7002374536878));
#57364=CARTESIAN_POINT('Ctrl Pts',(28.4872031236976,-0.0294943674923172,
21.6891385759717));
#57365=CARTESIAN_POINT('Ctrl Pts',(28.5307959749546,0.357711165892058,21.6676271574504));
#57366=CARTESIAN_POINT('Ctrl Pts',(28.588271358922,0.541814389624386,21.6573992005764));
#57367=CARTESIAN_POINT('Ctrl Pts',(28.7738533380075,0.887068805374046,21.6382183997014));
#57368=CARTESIAN_POINT('Ctrl Pts',(28.903512180976,1.043112470525,21.6279461150529));
#57369=CARTESIAN_POINT('Ctrl Pts',(29.2128905056455,1.29185751769652,21.6061515588234));
#57370=CARTESIAN_POINT('Ctrl Pts',(29.3882998946744,1.38356922217579,21.5951646233122));
#57371=CARTESIAN_POINT('Ctrl Pts',(29.7586487303438,1.49259838475184,21.5743176187989));
#57372=CARTESIAN_POINT('Ctrl Pts',(29.9494126813103,1.51113463524617,21.5652431789286));
#57373=CARTESIAN_POINT('Ctrl Pts',(30.3366113826679,1.4752126287187,21.5456162392091));
#57374=CARTESIAN_POINT('Ctrl Pts',(30.5290112502297,1.41763409463152,21.5347599925404));
#57375=CARTESIAN_POINT('Ctrl Pts',(30.8756573292315,1.23320190987312,21.512958859045));
#57376=CARTESIAN_POINT('Ctrl Pts',(31.0275193143428,1.10985575574539,21.5022261138206));
#57377=CARTESIAN_POINT('Ctrl Pts',(31.2750461098143,0.813213213668382,21.4820769047076));
#57378=CARTESIAN_POINT('Ctrl Pts',(31.3687657636095,0.643070885011216,21.4732261602783));
#57379=CARTESIAN_POINT('Ctrl Pts',(31.4888227697242,0.270291882918073,21.4525162157176));
#57380=CARTESIAN_POINT('Ctrl Pts',(31.5115128952941,0.0704953149593227,
21.4414164063865));
#57381=CARTESIAN_POINT('Ctrl Pts',(31.4782054807328,-0.318770290439176,
21.4197905394199));
#57382=CARTESIAN_POINT('Ctrl Pts',(31.4254475382382,-0.504803416717179,
21.4094553657378));
#57383=CARTESIAN_POINT('Ctrl Pts',(31.2494901966584,-0.853416070021567,
21.3900879961098));
#57384=CARTESIAN_POINT('Ctrl Pts',(31.1254658116588,-1.01138492328729,21.3802216401301));
#57385=CARTESIAN_POINT('Ctrl Pts',(30.8246930412984,-1.26828298434064,21.3586146462176));
#57386=CARTESIAN_POINT('Ctrl Pts',(30.6515224369356,-1.36534975789868,21.347586672365));
#57387=CARTESIAN_POINT('Ctrl Pts',(30.3143398429227,-1.47517879246933,21.3283131607309));
#57388=CARTESIAN_POINT('Ctrl Pts',(30.1575657374829,-1.50000000000003,21.3200808850792));
#57389=CARTESIAN_POINT('Ctrl Pts',(29.9999999999998,-1.50000000000001,21.3125));
#57390=CARTESIAN_POINT('Origin',(30.,-1.32966554433622E-14,16.));
#57391=CARTESIAN_POINT('',(29.9999999999999,-1.50000000000001,20.75));
#57392=CARTESIAN_POINT('',(30.0000000238974,-1.50000000000001,20.8125000022995));
#57393=CARTESIAN_POINT('',(30.,-1.50000000000001,16.));
#57394=CARTESIAN_POINT('Ctrl Pts',(29.9999999999998,-1.50000000000001,20.75));
#57395=CARTESIAN_POINT('Ctrl Pts',(30.1355873378723,-1.50000000000003,20.7565234488349));
#57396=CARTESIAN_POINT('Ctrl Pts',(30.2707763371628,-1.48162130053548,20.7635382520255));
#57397=CARTESIAN_POINT('Ctrl Pts',(30.5905052894202,-1.39270558594719,20.7813910993741));
#57398=CARTESIAN_POINT('Ctrl Pts',(30.767029784006,-1.30383501600373,20.7923527650226));
#57399=CARTESIAN_POINT('Ctrl Pts',(31.0784013127494,-1.06141205266722,20.8140676058879));
#57400=CARTESIAN_POINT('Ctrl Pts',(31.2094059572181,-0.909300433903993,
20.8244833092276));
#57401=CARTESIAN_POINT('Ctrl Pts',(31.4005633760122,-0.569930140644686,
20.8433372144086));
#57402=CARTESIAN_POINT('Ctrl Pts',(31.4616108021312,-0.387386085525011,
20.8534785508042));
#57403=CARTESIAN_POINT('Ctrl Pts',(31.5130288281118,-0.00193915990322278,
20.8748922688942));
#57404=CARTESIAN_POINT('Ctrl Pts',(31.5000564049022,0.197728440072968,20.8859849133374));
#57405=CARTESIAN_POINT('Ctrl Pts',(31.3981909189968,0.576981524645895,20.907054529147));
#57406=CARTESIAN_POINT('Ctrl Pts',(31.3116775745975,0.753220156722293,20.9161479987326));
#57407=CARTESIAN_POINT('Ctrl Pts',(31.0770964939546,1.06165196611475,20.9360018364982));
#57408=CARTESIAN_POINT('Ctrl Pts',(30.9317342971964,1.19125838532521,20.946595756762));
#57409=CARTESIAN_POINT('Ctrl Pts',(30.5933406580028,1.39218994814601,20.9684581606193));
#57410=CARTESIAN_POINT('Ctrl Pts',(30.4020178812766,1.458987498605,20.9795186695191));
#57411=CARTESIAN_POINT('Ctrl Pts',(30.0144815741343,1.51197726610397,20.999635956776));
#57412=CARTESIAN_POINT('Ctrl Pts',(29.8225847199203,1.50160380579917,21.0084913464817));
#57413=CARTESIAN_POINT('Ctrl Pts',(29.4482673839794,1.40844186112423,21.0290885295006));
#57414=CARTESIAN_POINT('Ctrl Pts',(29.2698358143887,1.32475295725216,21.0399980141694));
#57415=CARTESIAN_POINT('Ctrl Pts',(28.9522277915389,1.09163995424434,21.0617542984881));
#57416=CARTESIAN_POINT('Ctrl Pts',(28.8169317835683,0.943334467611102,21.0723833275575));
#57417=CARTESIAN_POINT('Ctrl Pts',(28.6164713965323,0.609937924996611,21.0912889974983));
#57418=CARTESIAN_POINT('Ctrl Pts',(28.5503235834348,0.429720618453307,21.1011266323083));
#57419=CARTESIAN_POINT('Ctrl Pts',(28.4877747716401,0.0469249157698905,
21.1223930602351));
#57420=CARTESIAN_POINT('Ctrl Pts',(28.4947443957624,-0.152432728065059,
21.1334684848926));
#57421=CARTESIAN_POINT('Ctrl Pts',(28.585202717896,-0.535530466260377,21.1547516925701));
#57422=CARTESIAN_POINT('Ctrl Pts',(28.6672227696192,-0.715637129073743,
21.1640888680802));
#57423=CARTESIAN_POINT('Ctrl Pts',(28.8938150388557,-1.03121039122832,21.1837567176656));
#57424=CARTESIAN_POINT('Ctrl Pts',(29.0350964807726,-1.16446677665445,21.1942556904709));
#57425=CARTESIAN_POINT('Ctrl Pts',(29.3666683501557,-1.37437197910307,21.2160391495426));
#57426=CARTESIAN_POINT('Ctrl Pts',(29.5553884234738,-1.44649304249621,21.2271223111757));
#57427=CARTESIAN_POINT('Ctrl Pts',(29.8346137979128,-1.49316573714005,21.2418530120072));
#57428=CARTESIAN_POINT('Ctrl Pts',(29.917323692752,-1.50000000000001,21.2460222343129));
#57429=CARTESIAN_POINT('Ctrl Pts',(30.,-1.50000000000001,21.25));
#57430=CARTESIAN_POINT('Ctrl Pts',(29.9999999999998,-1.50000000000001,21.3125));
#57431=CARTESIAN_POINT('Ctrl Pts',(29.9681380540405,-1.50000000000001,21.3109670414103));
#57432=CARTESIAN_POINT('Ctrl Pts',(29.9362464291016,-1.4989848402199,21.3094044560071));
#57433=CARTESIAN_POINT('Ctrl Pts',(29.7059061051266,-1.48427038685078,21.2979134671869));
#57434=CARTESIAN_POINT('Ctrl Pts',(29.5119585810338,-1.43225099507769,21.2871371794785));
#57435=CARTESIAN_POINT('Ctrl Pts',(29.1596955105172,-1.25764065487782,21.2653386273684));
#57436=CARTESIAN_POINT('Ctrl Pts',(29.0039750821709,-1.13829559847059,21.2545313843106));
#57437=CARTESIAN_POINT('Ctrl Pts',(28.7485987477413,-0.848934521932683,
21.2342067770101));
#57438=CARTESIAN_POINT('Ctrl Pts',(28.6505388148689,-0.682384621723858,
21.2254102567623));
#57439=CARTESIAN_POINT('Ctrl Pts',(28.5196273945211,-0.313661198442873,
21.2049256221356));
#57440=CARTESIAN_POINT('Ctrl Pts',(28.4910680085409,-0.114008266472331,
21.1938337925817));
#57441=CARTESIAN_POINT('Ctrl Pts',(28.5133617159534,0.277152561451723,21.1721026354748));
#57442=CARTESIAN_POINT('Ctrl Pts',(28.5610406223868,0.465104578293146,21.1616608567614));
#57443=CARTESIAN_POINT('Ctrl Pts',(28.7268127368948,0.817191792877632,21.1421004559512));
#57444=CARTESIAN_POINT('Ctrl Pts',(28.8450160186508,0.977157792197407,21.1325925873729));
#57445=CARTESIAN_POINT('Ctrl Pts',(29.1366994431696,1.24242044599111,21.1111905550177));
#57446=CARTESIAN_POINT('Ctrl Pts',(29.3073536529405,1.34504122266248,21.1001293733922));
#57447=CARTESIAN_POINT('Ctrl Pts',(29.6718885684984,1.47596994041667,21.0789537702634));
#57448=CARTESIAN_POINT('Ctrl Pts',(29.8613546451375,1.5056180641301,21.0693266350828));
#57449=CARTESIAN_POINT('Ctrl Pts',(30.2499905035945,1.49232790599687,21.0502592125655));
#57450=CARTESIAN_POINT('Ctrl Pts',(30.4453612619354,1.44608660162569,21.0395749518952));
#57451=CARTESIAN_POINT('Ctrl Pts',(30.8031247707546,1.28178759217525,21.017798185678));
#57452=CARTESIAN_POINT('Ctrl Pts',(30.9627170127615,1.16669332668992,21.0069227374242));
#57453=CARTESIAN_POINT('Ctrl Pts',(31.2261252563514,0.884888124749317,20.9864215801195));
#57454=CARTESIAN_POINT('Ctrl Pts',(31.3286136134484,0.721936793997485,20.9776075996665));
#57455=CARTESIAN_POINT('Ctrl Pts',(31.4704956794702,0.357450862099888,20.9573583812278));
#57456=CARTESIAN_POINT('Ctrl Pts',(31.5050292215643,0.158114714869949,20.9462841508261));
#57457=CARTESIAN_POINT('Ctrl Pts',(31.4940038450927,-0.234658795010768,
20.9244634002772));
#57458=CARTESIAN_POINT('Ctrl Pts',(31.4515503117875,-0.4244189406881,20.9139211699618));
#57459=CARTESIAN_POINT('Ctrl Pts',(31.2960889353342,-0.779942120592769,
20.8941698821893));
#57460=CARTESIAN_POINT('Ctrl Pts',(31.1836334516182,-0.941901166431575,
20.8849503363697));
#57461=CARTESIAN_POINT('Ctrl Pts',(30.9011214218994,-1.21536636315781,20.8637617145378));
#57462=CARTESIAN_POINT('Ctrl Pts',(30.7331593249481,-1.323483412269,20.8526773830162));
#57463=CARTESIAN_POINT('Ctrl Pts',(30.374104697925,-1.46471715060753,20.8314791998208));
#57464=CARTESIAN_POINT('Ctrl Pts',(30.1878361111775,-1.49999999700053,20.821537269196));
#57465=CARTESIAN_POINT('Ctrl Pts',(30.0000000239529,-1.50000000000001,20.8125000011524));
#57466=CARTESIAN_POINT('Origin',(30.,-1.32966554433622E-14,16.));
#57467=CARTESIAN_POINT('',(29.9999999999999,-1.50000000000001,20.25));
#57468=CARTESIAN_POINT('',(30.0000000000001,-1.50000000000001,20.3125));
#57469=CARTESIAN_POINT('',(30.,-1.50000000000001,16.));
#57470=CARTESIAN_POINT('Ctrl Pts',(29.9999999999999,-1.50000000000001,20.25));
#57471=CARTESIAN_POINT('Ctrl Pts',(30.1641246040904,-1.50000000000003,20.257896448696));
#57472=CARTESIAN_POINT('Ctrl Pts',(30.3273129308388,-1.47306839847894,20.2664959507697));
#57473=CARTESIAN_POINT('Ctrl Pts',(30.6694540696788,-1.35668483193177,20.2861901008358));
#57474=CARTESIAN_POINT('Ctrl Pts',(30.8415535621189,-1.25719932144175,20.2972337279289));
#57475=CARTESIAN_POINT('Ctrl Pts',(31.1383891848058,-0.996648092240175,
20.3187527726287));
#57476=CARTESIAN_POINT('Ctrl Pts',(31.2598762410215,-0.837810488997904,
20.3284549728335));
#57477=CARTESIAN_POINT('Ctrl Pts',(31.4314249865634,-0.487683998530185,
20.3479064445261));
#57478=CARTESIAN_POINT('Ctrl Pts',(31.4819950779928,-0.300804420279551,
20.3582886433178));
#57479=CARTESIAN_POINT('Ctrl Pts',(31.5105507066295,0.0893179172321859,
20.3799621065129));
#57480=CARTESIAN_POINT('Ctrl Pts',(31.4853246402279,0.289072829407564,20.3910596016338));
#57481=CARTESIAN_POINT('Ctrl Pts',(31.3605672791737,0.660112394093701,20.411672910783));
#57482=CARTESIAN_POINT('Ctrl Pts',(31.2649722312571,0.828695575895264,20.4204916500332));
#57483=CARTESIAN_POINT('Ctrl Pts',(31.0140581775355,1.12220790918685,20.4407168784407));
#57484=CARTESIAN_POINT('Ctrl Pts',(30.8605226301063,1.24384616367647,20.4514827013131));
#57485=CARTESIAN_POINT('Ctrl Pts',(30.5114243415045,1.42407146100134,20.4732849588136));
#57486=CARTESIAN_POINT('Ctrl Pts',(30.3183380047095,1.47926213924964,20.4841079039198));
#57487=CARTESIAN_POINT('Ctrl Pts',(29.9307960888716,1.51038882263748,20.5036181531332));
#57488=CARTESIAN_POINT('Ctrl Pts',(29.7403288665302,1.48951380456358,20.5127847164407));
#57489=CARTESIAN_POINT('Ctrl Pts',(29.3711639835748,1.37589985350485,20.5337021132381));
#57490=CARTESIAN_POINT('Ctrl Pts',(29.1966946677341,1.28188655628153,20.5447077525887));
#57491=CARTESIAN_POINT('Ctrl Pts',(28.8909965958092,1.02962579258236,20.5664229013678));
#57492=CARTESIAN_POINT('Ctrl Pts',(28.7637626025144,0.872753791453066,20.5765136782526));
#57493=CARTESIAN_POINT('Ctrl Pts',(28.582295287402,0.526054660802727,20.5957747410665));
#57494=CARTESIAN_POINT('Ctrl Pts',(28.5268265400693,0.341112810094873,20.6060492883281));
#57495=CARTESIAN_POINT('Ctrl Pts',(28.4876154625531,-0.0470049788678421,
20.6276113877149));
#57496=CARTESIAN_POINT('Ctrl Pts',(28.5071470207889,-0.246809925970759,
20.6387116625539));
#57497=CARTESIAN_POINT('Ctrl Pts',(28.6213243381125,-0.621726643029005,
20.6595403690571));
#57498=CARTESIAN_POINT('Ctrl Pts',(28.7127069454602,-0.793828860292424,
20.6684492190444));
#57499=CARTESIAN_POINT('Ctrl Pts',(28.9560213000323,-1.09433750409046,20.6885031487146));
#57500=CARTESIAN_POINT('Ctrl Pts',(29.1057854975977,-1.21976733917156,20.6991928441151));
#57501=CARTESIAN_POINT('Ctrl Pts',(29.4493247586543,-1.40936219023255,20.7209879081598));
#57502=CARTESIAN_POINT('Ctrl Pts',(29.6408325610402,-1.46988527163767,20.7318830283038));
#57503=CARTESIAN_POINT('Ctrl Pts',(29.8922912775479,-1.4971028845898,20.7447373862468));
#57504=CARTESIAN_POINT('Ctrl Pts',(29.9461731363168,-1.50000000000001,20.7474102538136));
#57505=CARTESIAN_POINT('Ctrl Pts',(29.9999999999998,-1.50000000000001,20.75));
#57506=CARTESIAN_POINT('Ctrl Pts',(30.0000000239529,-1.50000000000001,20.8125000011524));
#57507=CARTESIAN_POINT('Ctrl Pts',(29.9974904007656,-1.50000000004009,20.8123792568517));
#57508=CARTESIAN_POINT('Ctrl Pts',(29.994980514477,-1.49999370187214,20.8122583249421));
#57509=CARTESIAN_POINT('Ctrl Pts',(29.7936662704942,-1.49898314378545,20.8025445178046));
#57510=CARTESIAN_POINT('Ctrl Pts',(29.5970666373285,-1.45847246315053,20.7919603168594));
#57511=CARTESIAN_POINT('Ctrl Pts',(29.2341811004286,-1.30450218441903,20.7702240261379));
#57512=CARTESIAN_POINT('Ctrl Pts',(29.0708854167951,-1.19371554978206,20.7592900523783));
#57513=CARTESIAN_POINT('Ctrl Pts',(28.7996246113049,-0.919409908918738,
20.738619409654));
#57514=CARTESIAN_POINT('Ctrl Pts',(28.6928036628702,-0.759898893507146,
20.7297166051949));
#57515=CARTESIAN_POINT('Ctrl Pts',(28.540323338491,-0.399638425423168,20.7097021347457));
#57516=CARTESIAN_POINT('Ctrl Pts',(28.4999872115666,-0.200774562873281,
20.6986541423819));
#57517=CARTESIAN_POINT('Ctrl Pts',(28.5000123038317,0.193260173251348,20.6767633237083));
#57518=CARTESIAN_POINT('Ctrl Pts',(28.5373370740434,0.384636586987589,20.6661313007229));
#57519=CARTESIAN_POINT('Ctrl Pts',(28.6828216865171,0.743407395273799,20.6461995891515));
#57520=CARTESIAN_POINT('Ctrl Pts',(28.7898502936129,0.90727948583588,20.637187813622));
#57521=CARTESIAN_POINT('Ctrl Pts',(29.0635269308615,1.18843769395866,20.6162105900475));
#57522=CARTESIAN_POINT('Ctrl Pts',(29.228755223573,1.30174519776628,20.6051136094466));
#57523=CARTESIAN_POINT('Ctrl Pts',(29.5868470804747,1.45456710532649,20.5836398539607));
#57524=CARTESIAN_POINT('Ctrl Pts',(29.7752048690842,1.49530975495507,20.5734457453635));
#57525=CARTESIAN_POINT('Ctrl Pts',(30.1648759814307,1.50410182396658,20.5544534610902));
#57526=CARTESIAN_POINT('Ctrl Pts',(30.3625681263815,1.46904639647318,20.544196110566));
#57527=CARTESIAN_POINT('Ctrl Pts',(30.7301648562918,1.32486538129436,20.5225050764527));
#57528=CARTESIAN_POINT('Ctrl Pts',(30.8968384149473,1.21823387618242,20.5115240048699));
#57529=CARTESIAN_POINT('Ctrl Pts',(31.1754315899033,0.951036194862134,20.4906980266758));
#57530=CARTESIAN_POINT('Ctrl Pts',(31.2863099173977,0.794671992670377,20.4816484440372));
#57531=CARTESIAN_POINT('Ctrl Pts',(31.4475104523221,0.440765387920731,20.4619869659956));
#57532=CARTESIAN_POINT('Ctrl Pts',(31.4931266838049,0.245180433281527,20.4511211351823));
#57533=CARTESIAN_POINT('Ctrl Pts',(31.505277935416,-0.147222207316758,20.4293209884824));
#57534=CARTESIAN_POINT('Ctrl Pts',(31.4737006088925,-0.340229130529765,
20.4185983816372));
#57535=CARTESIAN_POINT('Ctrl Pts',(31.339252899941,-0.702504700740186,20.39847196107));
#57536=CARTESIAN_POINT('Ctrl Pts',(31.2380795698328,-0.868488363198902,
20.3896091209879));
#57537=CARTESIAN_POINT('Ctrl Pts',(30.9741217873874,-1.15788922779948,20.3688705333532));
#57538=CARTESIAN_POINT('Ctrl Pts',(30.8120536546578,-1.27678494801521,20.3577703677868));
#57539=CARTESIAN_POINT('Ctrl Pts',(30.4578087067642,-1.44121172280179,20.3361593393739));
#57540=CARTESIAN_POINT('Ctrl Pts',(30.2702179556352,-1.48784534045563,20.3258384968839));
#57541=CARTESIAN_POINT('Ctrl Pts',(30.052598998323,-1.49930896382792,20.3150498659359));
#57542=CARTESIAN_POINT('Ctrl Pts',(30.0262877690999,-1.50000000000001,20.3137647708805));
#57543=CARTESIAN_POINT('Ctrl Pts',(30.0000000000001,-1.50000000000001,20.3125));
#57544=CARTESIAN_POINT('Origin',(30.,-1.32966554433622E-14,16.));
#57545=CARTESIAN_POINT('',(29.9999999508795,-1.50000000000001,19.7499999952734));
#57546=CARTESIAN_POINT('',(30.0000000000001,-1.50000000000001,19.8125));
#57547=CARTESIAN_POINT('',(30.,-1.50000000000001,16.));
#57548=CARTESIAN_POINT('Ctrl Pts',(29.9999999507652,-1.50000000000001,19.7499999976312));
#57549=CARTESIAN_POINT('Ctrl Pts',(30.0036354883629,-1.50000000011934,19.7501749125187));
#57550=CARTESIAN_POINT('Ctrl Pts',(30.007271600744,-1.4999867831078,19.7503502221899));
#57551=CARTESIAN_POINT('Ctrl Pts',(30.201622915749,-1.49857339489822,19.7597402149765));
#57552=CARTESIAN_POINT('Ctrl Pts',(30.3903004853368,-1.46082693625102,19.769866481516));
#57553=CARTESIAN_POINT('Ctrl Pts',(30.7502056783764,-1.31393443624912,19.7912627754119));
#57554=CARTESIAN_POINT('Ctrl Pts',(30.9169691324023,-1.2034971179945,19.8023538891195));
#57555=CARTESIAN_POINT('Ctrl Pts',(31.1955532827852,-0.926587489668503,
19.8234492094243));
#57556=CARTESIAN_POINT('Ctrl Pts',(31.305583357368,-0.763777918932018,19.8325678933928));
#57557=CARTESIAN_POINT('Ctrl Pts',(31.4566154175894,-0.406803589900389,
19.8523998005612));
#57558=CARTESIAN_POINT('Ctrl Pts',(31.4968003232487,-0.216309448389897,
19.8629828084229));
#57559=CARTESIAN_POINT('Ctrl Pts',(31.5029527191874,0.177060648076386,19.884836702671));
#57560=CARTESIAN_POINT('Ctrl Pts',(31.4658451495388,0.376207311237188,19.8959004061799));
#57561=CARTESIAN_POINT('Ctrl Pts',(31.3192558360179,0.738832237635632,19.9160462354243));
#57562=CARTESIAN_POINT('Ctrl Pts',(31.2148503942445,0.900251242918639,19.9248907954582));
#57563=CARTESIAN_POINT('Ctrl Pts',(30.9479657510409,1.17875033469753,19.9454673747239));
#57564=CARTESIAN_POINT('Ctrl Pts',(30.7867234803792,1.29195591113542,19.9563697464337));
#57565=CARTESIAN_POINT('Ctrl Pts',(30.4266603329508,1.45171184585212,19.9781309575447));
#57566=CARTESIAN_POINT('Ctrl Pts',(30.2307253625385,1.49542562590392,19.9887721548721));
#57567=CARTESIAN_POINT('Ctrl Pts',(29.8418323593176,1.50370934578551,20.0077128815434));
#57568=CARTESIAN_POINT('Ctrl Pts',(29.6526184508184,1.47157346290215,20.0175030286082));
#57569=CARTESIAN_POINT('Ctrl Pts',(29.2894512067405,1.33570909972092,20.038749930874));
#57570=CARTESIAN_POINT('Ctrl Pts',(29.1199599079427,1.2306626568369,20.0498225415362));
#57571=CARTESIAN_POINT('Ctrl Pts',(28.8323016398048,0.961771765690436,20.0711316978356));
#57572=CARTESIAN_POINT('Ctrl Pts',(28.7166359490173,0.80092922531751,20.0805039319268));
#57573=CARTESIAN_POINT('Ctrl Pts',(28.5553841103709,0.447325657819572,20.1001485745656));
#57574=CARTESIAN_POINT('Ctrl Pts',(28.5099861175222,0.258564005548656,20.1106353330251));
#57575=CARTESIAN_POINT('Ctrl Pts',(28.4926188058233,-0.133342134639988,
20.1324078963689));
#57576=CARTESIAN_POINT('Ctrl Pts',(28.5237938243712,-0.332877530953282,
20.1434931961641));
#57577=CARTESIAN_POINT('Ctrl Pts',(28.6595170927538,-0.699759711689848,
20.1638755395383));
#57578=CARTESIAN_POINT('Ctrl Pts',(28.759513047986,-0.864726488741114,20.1726705572702));
#57579=CARTESIAN_POINT('Ctrl Pts',(29.0184002150316,-1.15079879551533,20.1930727248681));
#57580=CARTESIAN_POINT('Ctrl Pts',(29.1758229214277,-1.26830528519454,20.2039107975187));
#57581=CARTESIAN_POINT('Ctrl Pts',(29.5305217931358,-1.4384406773805,20.2257022380569));
#57582=CARTESIAN_POINT('Ctrl Pts',(29.7251117157194,-1.4879453135066,20.2364395788536));
#57583=CARTESIAN_POINT('Ctrl Pts',(29.9491466954872,-1.49935402178859,20.2475353754067));
#57584=CARTESIAN_POINT('Ctrl Pts',(29.9745837219083,-1.50000000000001,20.2487771587502));
#57585=CARTESIAN_POINT('Ctrl Pts',(29.9999999999999,-1.50000000000001,20.25));
#57586=CARTESIAN_POINT('Ctrl Pts',(30.0000000000001,-1.50000000000001,20.3125));
#57587=CARTESIAN_POINT('Ctrl Pts',(29.8275998140085,-1.50000000000001,20.3042053921841));
#57588=CARTESIAN_POINT('Ctrl Pts',(29.6562870357889,-1.47028352574469,20.2951376446808));
#57589=CARTESIAN_POINT('Ctrl Pts',(29.3085931862514,-1.34558031058123,20.2749452383464));
#57590=CARTESIAN_POINT('Ctrl Pts',(29.1384186293223,-1.24350663328035,20.2639223312337));
#57591=CARTESIAN_POINT('Ctrl Pts',(28.8520258822514,-0.983987574399218,
20.242934391019));
#57592=CARTESIAN_POINT('Ctrl Pts',(28.7368098691781,-0.830906588856551,
20.2336614771587));
#57593=CARTESIAN_POINT('Ctrl Pts',(28.5656483010559,-0.481857271883387,
20.214269848438));
#57594=CARTESIAN_POINT('Ctrl Pts',(28.5144799811963,-0.287679235979695,
20.2034821797766));
#57595=CARTESIAN_POINT('Ctrl Pts',(28.4911007681834,0.104720249591022,20.181682208356));
#57596=CARTESIAN_POINT('Ctrl Pts',(28.5173310962609,0.299077411990059,20.1708845882228));
#57597=CARTESIAN_POINT('Ctrl Pts',(28.6416246239434,0.664496311411631,20.1505835382549));
#57598=CARTESIAN_POINT('Ctrl Pts',(28.7375408574377,0.832427515421977,20.1417837739438));
#57599=CARTESIAN_POINT('Ctrl Pts',(28.9926175512114,1.12917452204563,20.1212684183864));
#57600=CARTESIAN_POINT('Ctrl Pts',(29.1516633795811,1.2530630770023,20.1101749736523));
#57601=CARTESIAN_POINT('Ctrl Pts',(29.5021040725661,1.42792836972927,20.0884570187074));
#57602=CARTESIAN_POINT('Ctrl Pts',(29.6888418601191,1.47989191267207,20.0780291609664));
#57603=CARTESIAN_POINT('Ctrl Pts',(30.0769287467939,1.5109546306831,20.0584944686474));
#57604=CARTESIAN_POINT('Ctrl Pts',(30.2747213678695,1.48776626200004,20.0489426359701));
#57605=CARTESIAN_POINT('Ctrl Pts',(30.6499367323256,1.36617967610523,20.027512673167));
#57606=CARTESIAN_POINT('Ctrl Pts',(30.8236685705517,1.26902858360925,20.0164553547449));
#57607=CARTESIAN_POINT('Ctrl Pts',(31.1182297704941,1.01768973269335,19.9953016376572));
#57608=CARTESIAN_POINT('Ctrl Pts',(31.2380227260335,0.867983838688731,19.9857213243715));
#57609=CARTESIAN_POINT('Ctrl Pts',(31.4194655172301,0.52407745893419,19.9666154143852));
#57610=CARTESIAN_POINT('Ctrl Pts',(31.4763477416476,0.331530482038543,19.9559183601132));
#57611=CARTESIAN_POINT('Ctrl Pts',(31.5113890098208,-0.0605236259430762,
19.9341375763365));
#57612=CARTESIAN_POINT('Ctrl Pts',(31.4907606610887,-0.256127601642152,
19.9232706887976));
#57613=CARTESIAN_POINT('Ctrl Pts',(31.3770092904839,-0.62473058770716,19.9027927451274));
#57614=CARTESIAN_POINT('Ctrl Pts',(31.2864311739689,-0.794691675228615,
19.8939853466257));
#57615=CARTESIAN_POINT('Ctrl Pts',(31.0405043429371,-1.09883901947073,19.8737046491109));
#57616=CARTESIAN_POINT('Ctrl Pts',(30.8847013390568,-1.22775605549742,19.8626275448131));
#57617=CARTESIAN_POINT('Ctrl Pts',(30.5384592288504,-1.41320441242881,19.8408176202706));
#57618=CARTESIAN_POINT('Ctrl Pts',(30.3527481344157,-1.47060245170435,19.8302882010938));
#57619=CARTESIAN_POINT('Ctrl Pts',(30.1075898199807,-1.49710947656403,19.8177567099449));
#57620=CARTESIAN_POINT('Ctrl Pts',(30.0537655536404,-1.50000000000001,19.8150867964056));
#57621=CARTESIAN_POINT('Ctrl Pts',(30.0000000000003,-1.50000000000001,19.8125));
#57622=CARTESIAN_POINT('Origin',(30.,-1.32966554433622E-14,16.));
#57623=CARTESIAN_POINT('',(30.0000000000001,-1.50000000000001,19.25));
#57624=CARTESIAN_POINT('',(30.,-1.50000000000001,19.3125));
#57625=CARTESIAN_POINT('',(30.,-1.50000000000001,16.));
#57626=CARTESIAN_POINT('Ctrl Pts',(30.0000000000001,-1.50000000000001,19.25));
#57627=CARTESIAN_POINT('Ctrl Pts',(30.0322695745912,-1.50000000000001,19.2515525706314));
#57628=CARTESIAN_POINT('Ctrl Pts',(30.0645714825038,-1.49895869986435,19.2531356219044));
#57629=CARTESIAN_POINT('Ctrl Pts',(30.2882590679586,-1.48448482383795,19.2642998479893));
#57630=CARTESIAN_POINT('Ctrl Pts',(30.4754930135539,-1.43550485550641,19.2746687000727));
#57631=CARTESIAN_POINT('Ctrl Pts',(30.8281012978914,-1.26647563555772,19.2963288301724));
#57632=CARTESIAN_POINT('Ctrl Pts',(30.9888581275123,-1.14537453755813,19.3074271661326));
#57633=CARTESIAN_POINT('Ctrl Pts',(31.2489169787693,-0.852727854965852,
19.328068327964));
#57634=CARTESIAN_POINT('Ctrl Pts',(31.3477723438117,-0.685891580063111,
19.3368949122188));
#57635=CARTESIAN_POINT('Ctrl Pts',(31.4777710225729,-0.322229436301838,
19.35709836465));
#57636=CARTESIAN_POINT('Ctrl Pts',(31.5070120496637,-0.128613045958812,
19.3678548307802));
#57637=CARTESIAN_POINT('Ctrl Pts',(31.4899431617665,0.263827999699887,19.3896571110945));
#57638=CARTESIAN_POINT('Ctrl Pts',(31.4418890858574,0.458816520684437,19.4004898067048));
#57639=CARTESIAN_POINT('Ctrl Pts',(31.2763170645903,0.810606892156535,19.420033716231));
#57640=CARTESIAN_POINT('Ctrl Pts',(31.1635461572557,0.965528328551652,19.4291724240899));
#57641=CARTESIAN_POINT('Ctrl Pts',(30.8815440072885,1.22938524433353,19.4500696176279));
#57642=CARTESIAN_POINT('Ctrl Pts',(30.713328176096,1.33404197013925,19.4610700368521));
#57643=CARTESIAN_POINT('Ctrl Pts',(30.3423586225268,1.47407873960012,19.4828082280827));
#57644=CARTESIAN_POINT('Ctrl Pts',(30.1427440803289,1.50655371354715,19.4929501746347));
#57645=CARTESIAN_POINT('Ctrl Pts',(29.7515262729803,1.4915957790601,19.5121881483469));
#57646=CARTESIAN_POINT('Ctrl Pts',(29.563545020268,1.44778515274356,19.522449362427));
#57647=CARTESIAN_POINT('Ctrl Pts',(29.2074099124303,1.28891068317319,19.5439971005021));
#57648=CARTESIAN_POINT('Ctrl Pts',(29.0438038910602,1.17268375630169,19.5550971246218));
#57649=CARTESIAN_POINT('Ctrl Pts',(28.7751767012687,0.88721540741588,19.5759511326745));
#57650=CARTESIAN_POINT('Ctrl Pts',(28.6712044325382,0.722248138115754,19.5848751034381));
#57651=CARTESIAN_POINT('Ctrl Pts',(28.5314450700553,0.361647735614998,19.6049084591326));
#57652=CARTESIAN_POINT('Ctrl Pts',(28.4970926988021,0.169404578017586,19.6155886345547));
#57653=CARTESIAN_POINT('Ctrl Pts',(28.5033789257342,-0.222871075081128,
19.6373817263935));
#57654=CARTESIAN_POINT('Ctrl Pts',(28.5460751647458,-0.419126971559099,
19.6482848317533));
#57655=CARTESIAN_POINT('Ctrl Pts',(28.7020419000445,-0.77553505760853,19.6680852809783));
#57656=CARTESIAN_POINT('Ctrl Pts',(28.8106757232385,-0.933630997355151,
19.6770461367592));
#57657=CARTESIAN_POINT('Ctrl Pts',(29.0852161697017,-1.20477024704427,19.697786615973));
#57658=CARTESIAN_POINT('Ctrl Pts',(29.2500326897204,-1.31371406923191,19.7087425717726));
#57659=CARTESIAN_POINT('Ctrl Pts',(29.611734771314,-1.46197087611401,19.7302632159228));
#57660=CARTESIAN_POINT('Ctrl Pts',(29.8049901134984,-1.49999999359916,19.7406175822833));
#57661=CARTESIAN_POINT('Ctrl Pts',(29.9999999507652,-1.50000000000001,19.7499999976312));
#57662=CARTESIAN_POINT('Ctrl Pts',(30.0000000000003,-1.50000000000001,19.8125));
#57663=CARTESIAN_POINT('Ctrl Pts',(29.8589500630315,-1.50000000000001,19.8057137317435));
#57664=CARTESIAN_POINT('Ctrl Pts',(29.7183576297039,-1.48011045726929,19.7983969878431));
#57665=CARTESIAN_POINT('Ctrl Pts',(29.392433533781,-1.38562863633522,19.7800914624408));
#57666=CARTESIAN_POINT('Ctrl Pts',(29.2152602016442,-1.29355450601908,19.7690095917929));
#57667=CARTESIAN_POINT('Ctrl Pts',(28.9125224323809,-1.05055621120639,19.7476941614444));
#57668=CARTESIAN_POINT('Ctrl Pts',(28.7881027470448,-0.904173072558181,
19.7377318373643));
#57669=CARTESIAN_POINT('Ctrl Pts',(28.5965141205021,-0.565467385757126,
19.7189148547643));
#57670=CARTESIAN_POINT('Ctrl Pts',(28.5340212729776,-0.374707579896709,
19.708317087772));
#57671=CARTESIAN_POINT('Ctrl Pts',(28.4874198303467,0.0166598622973653,
19.6865744520946));
#57672=CARTESIAN_POINT('Ctrl Pts',(28.5024461232084,0.213342923270549,19.6756476153738));
#57673=CARTESIAN_POINT('Ctrl Pts',(28.605730933148,0.585021358101511,19.6549988134388));
#57674=CARTESIAN_POINT('Ctrl Pts',(28.6911262279336,0.757019946925095,19.6461115535275));
#57675=CARTESIAN_POINT('Ctrl Pts',(28.9280450078188,1.06829223859541,19.6260663408692));
#57676=CARTESIAN_POINT('Ctrl Pts',(29.0805347242822,1.20204064727676,19.6150144423906));
#57677=CARTESIAN_POINT('Ctrl Pts',(29.4223784266326,1.3977266885599,19.5931317562239));
#57678=CARTESIAN_POINT('Ctrl Pts',(29.6069366918152,1.46041214264913,19.5825109299366));
#57679=CARTESIAN_POINT('Ctrl Pts',(29.9906687655378,1.51247863508202,19.562602320475));
#57680=CARTESIAN_POINT('Ctrl Pts',(30.1862339040192,1.50100007477566,19.55356759697));
#57681=CARTESIAN_POINT('Ctrl Pts',(30.5662821795392,1.40308967236277,19.5325627823883));
#57682=CARTESIAN_POINT('Ctrl Pts',(30.7466285872712,1.31600734425417,19.5214669082421));
#57683=CARTESIAN_POINT('Ctrl Pts',(31.0570470506688,1.08124306107491,19.5000106628701));
#57684=CARTESIAN_POINT('Ctrl Pts',(31.185947420448,0.938076365153711,19.4898320882731));
#57685=CARTESIAN_POINT('Ctrl Pts',(31.387173884418,0.604359282145194,19.4708806565388));
#57686=CARTESIAN_POINT('Ctrl Pts',(31.4549913450499,0.415392173173207,19.460577342954));
#57687=CARTESIAN_POINT('Ctrl Pts',(31.5125364736871,0.0248207245632997,
19.4388789291423));
#57688=CARTESIAN_POINT('Ctrl Pts',(31.5028468405333,-0.172737498474235,
19.4279034723069));
#57689=CARTESIAN_POINT('Ctrl Pts',(31.4094808313587,-0.547250043493136,
19.4070972198059));
#57690=CARTESIAN_POINT('Ctrl Pts',(31.3288984144444,-0.721204660777261,
19.3980698586427));
#57691=CARTESIAN_POINT('Ctrl Pts',(31.1018991125715,-1.03700530321776,19.3783761095713));
#57692=CARTESIAN_POINT('Ctrl Pts',(30.9548507096631,-1.17379817492847,19.3675014379958));
#57693=CARTESIAN_POINT('Ctrl Pts',(30.6204358823266,-1.37933694163779,19.3457024869274));
#57694=CARTESIAN_POINT('Ctrl Pts',(30.4373267027344,-1.44785012953098,19.3349894983086));
#57695=CARTESIAN_POINT('Ctrl Pts',(30.1646733538461,-1.49322482781476,19.3206110496582));
#57696=CARTESIAN_POINT('Ctrl Pts',(30.0823180279059,-1.50000000000001,19.3164605279642));
#57697=CARTESIAN_POINT('Ctrl Pts',(30.,-1.50000000000001,19.3125));
#57698=CARTESIAN_POINT('Origin',(30.,-1.32966554433622E-14,16.));
#57699=CARTESIAN_POINT('',(30.0000000000001,-1.50000000000001,18.75));
#57700=CARTESIAN_POINT('',(30.,-1.50000000000001,18.8125));
#57701=CARTESIAN_POINT('',(30.,-1.50000000000001,16.));
#57702=CARTESIAN_POINT('Ctrl Pts',(30.0000000000002,-1.50000000000001,18.75));
#57703=CARTESIAN_POINT('Ctrl Pts',(30.0598815861698,-1.50000000000001,18.7528810541579));
#57704=CARTESIAN_POINT('Ctrl Pts',(30.1198247627216,-1.4964145214846,18.7558646682098));
#57705=CARTESIAN_POINT('Ctrl Pts',(30.3709807388755,-1.46613984657296,18.7687893789386));
#57706=CARTESIAN_POINT('Ctrl Pts',(30.5561899070999,-1.40635296128044,18.7793610060131));
#57707=CARTESIAN_POINT('Ctrl Pts',(30.9004833554958,-1.21627199481911,18.8012058591186));
#57708=CARTESIAN_POINT('Ctrl Pts',(31.054808880873,-1.08516465668695,18.8122727199239));
#57709=CARTESIAN_POINT('Ctrl Pts',(31.2966795386424,-0.777790002612556,
18.832447912207));
#57710=CARTESIAN_POINT('Ctrl Pts',(31.3849156897549,-0.606916752329299,
18.8412824026485));
#57711=CARTESIAN_POINT('Ctrl Pts',(31.4939654845851,-0.236921615045211,
18.8618376880532));
#57712=CARTESIAN_POINT('Ctrl Pts',(31.5120817444602,-0.0408132290769898,
18.8727325983848));
#57713=CARTESIAN_POINT('Ctrl Pts',(31.4718441015158,0.350974679810523,18.8944985933229));
#57714=CARTESIAN_POINT('Ctrl Pts',(31.4124332725198,0.54273929222595,18.9051521829016));
#57715=CARTESIAN_POINT('Ctrl Pts',(31.2264254338517,0.884320880490274,18.9241289378051));
#57716=CARTESIAN_POINT('Ctrl Pts',(31.1045648671413,1.03253115218655,18.9338713522791));
#57717=CARTESIAN_POINT('Ctrl Pts',(30.8063387149155,1.2801510812434,18.9550980960807));
#57718=CARTESIAN_POINT('Ctrl Pts',(30.6310491381331,1.37504484021148,18.9661676575249));
#57719=CARTESIAN_POINT('Ctrl Pts',(30.2546711108962,1.4912245976519,18.9875033692879));
#57720=CARTESIAN_POINT('Ctrl Pts',(30.05740041095,1.51172051693628,18.9969127515258));
#57721=CARTESIAN_POINT('Ctrl Pts',(29.6702738320324,1.47589654334487,19.0165334981157));
#57722=CARTESIAN_POINT('Ctrl Pts',(29.4839742576828,1.42150925053353,19.0270075986994));
#57723=CARTESIAN_POINT('Ctrl Pts',(29.1353660189379,1.24191643228194,19.048768709802));
#57724=CARTESIAN_POINT('Ctrl Pts',(28.9777462443354,1.1157773991078,19.059856056776));
#57725=CARTESIAN_POINT('Ctrl Pts',(28.7267374929236,0.815719209989595,19.0802676706567));
#57726=CARTESIAN_POINT('Ctrl Pts',(28.6332044534767,0.64688991790973,19.0890616712273));
#57727=CARTESIAN_POINT('Ctrl Pts',(28.5135873974093,0.280047942578678,19.109441780968));
#57728=CARTESIAN_POINT('Ctrl Pts',(28.4898364137009,0.0851180238092936,
19.1202712208996));
#57729=CARTESIAN_POINT('Ctrl Pts',(28.5183897482981,-0.307171243363851,
19.1420650690759));
#57730=CARTESIAN_POINT('Ctrl Pts',(28.5720998196786,-0.500646940480604,
19.1528137189157));
#57731=CARTESIAN_POINT('Ctrl Pts',(28.747829861517,-0.847427013151625,19.1720792785085));
#57732=CARTESIAN_POINT('Ctrl Pts',(28.8650664758991,-0.999006868470888,
19.1814790094866));
#57733=CARTESIAN_POINT('Ctrl Pts',(29.1550741400796,-1.25492382568339,19.2025408141021));
#57734=CARTESIAN_POINT('Ctrl Pts',(29.3268372187205,-1.35483766663846,19.2135801535473));
#57735=CARTESIAN_POINT('Ctrl Pts',(29.6699517271029,-1.47262040644266,19.2333600008011));
#57736=CARTESIAN_POINT('Ctrl Pts',(29.8345144389513,-1.50000000000001,19.2420380722318));
#57737=CARTESIAN_POINT('Ctrl Pts',(30.0000000000001,-1.50000000000001,19.25));
#57738=CARTESIAN_POINT('Ctrl Pts',(30.,-1.50000000000001,19.3125));
#57739=CARTESIAN_POINT('Ctrl Pts',(29.8904115959066,-1.50000000000001,19.3072274254497));
#57740=CARTESIAN_POINT('Ctrl Pts',(29.7809217474217,-1.48799325955223,19.3016260720903));
#57741=CARTESIAN_POINT('Ctrl Pts',(29.479267613868,-1.42071467340943,19.2852438812078));
#57742=CARTESIAN_POINT('Ctrl Pts',(29.2956191224553,-1.33919024824593,19.2741435216794));
#57743=CARTESIAN_POINT('Ctrl Pts',(28.9769843310201,-1.11359538988626,19.2525466742853));
#57744=CARTESIAN_POINT('Ctrl Pts',(28.8433197059369,-0.97404728751911,19.2422393958357));
#57745=CARTESIAN_POINT('Ctrl Pts',(28.6314369352188,-0.64558462894177,19.2229212185382));
#57746=CARTESIAN_POINT('Ctrl Pts',(28.5578261508896,-0.458159789494097,
19.2129533216385));
#57747=CARTESIAN_POINT('Ctrl Pts',(28.4887314396478,-0.0683254796838233,
19.1912958599824));
#57748=CARTESIAN_POINT('Ctrl Pts',(28.4927829468086,0.129998312926432,19.180277871504));
#57749=CARTESIAN_POINT('Ctrl Pts',(28.5757061903925,0.507408017565263,19.1593106656908));
#57750=CARTESIAN_POINT('Ctrl Pts',(28.6513157241137,0.683452060166118,19.1500704896955));
#57751=CARTESIAN_POINT('Ctrl Pts',(28.8692063981292,1.00541452618758,19.1306438179201));
#57752=CARTESIAN_POINT('Ctrl Pts',(29.0123062748592,1.14629480240063,19.119845580885));
#57753=CARTESIAN_POINT('Ctrl Pts',(29.3411837772215,1.36149831072911,19.0980445794436));
#57754=CARTESIAN_POINT('Ctrl Pts',(29.5228193452006,1.43527924918368,19.0872561635921));
#57755=CARTESIAN_POINT('Ctrl Pts',(29.9017346505858,1.50901487689319,19.0669773805809));
#57756=CARTESIAN_POINT('Ctrl Pts',(30.095243866884,1.50920856983617,19.0581733709244));
#57757=CARTESIAN_POINT('Ctrl Pts',(30.4795337547919,1.43522535350299,19.0376291257293));
#57758=CARTESIAN_POINT('Ctrl Pts',(30.6659951148259,1.35877256279477,19.0265343107311));
#57759=CARTESIAN_POINT('Ctrl Pts',(30.9917525251624,1.14161337833726,19.0048291004505));
#57760=CARTESIAN_POINT('Ctrl Pts',(31.12959203788,1.00543319777699,18.9944145110095));
#57761=CARTESIAN_POINT('Ctrl Pts',(31.3495099297643,0.683969951441068,18.9749041718824));
#57762=CARTESIAN_POINT('Ctrl Pts',(31.4277388995994,0.500572833869038,18.9653096018815));
#57763=CARTESIAN_POINT('Ctrl Pts',(31.5085610210805,0.114360476914036,18.9438533598284));
#57764=CARTESIAN_POINT('Ctrl Pts',(31.510521839189,-0.0846024989690804,
18.9327998611683));
#57765=CARTESIAN_POINT('Ctrl Pts',(31.4387139095947,-0.464995267712227,
18.9116669295714));
#57766=CARTESIAN_POINT('Ctrl Pts',(31.3683024334794,-0.643299822803022,
18.9021297086694));
#57767=CARTESIAN_POINT('Ctrl Pts',(31.1599775839064,-0.97159308723095,18.8829874173259));
#57768=CARTESIAN_POINT('Ctrl Pts',(31.021122395481,-1.11661364586043,18.8722783951071));
#57769=CARTESIAN_POINT('Ctrl Pts',(30.6983237124874,-1.34174379218127,18.8504941210548));
#57770=CARTESIAN_POINT('Ctrl Pts',(30.5183853004494,-1.42099198981035,18.8396354913461));
#57771=CARTESIAN_POINT('Ctrl Pts',(30.220307982392,-1.48785706899676,18.8234368763837));
#57772=CARTESIAN_POINT('Ctrl Pts',(30.1102084329115,-1.50000000000001,18.8178024057007));
#57773=CARTESIAN_POINT('Ctrl Pts',(30.,-1.50000000000001,18.8125));
#57774=CARTESIAN_POINT('Origin',(30.,-1.32966554433622E-14,16.));
#57775=CARTESIAN_POINT('',(30.,-1.50000000000001,18.25));
#57776=CARTESIAN_POINT('',(29.9999999999999,-1.50000000000001,18.3125));
#57777=CARTESIAN_POINT('',(30.,-1.50000000000001,16.));
#57778=CARTESIAN_POINT('Ctrl Pts',(30.,-1.50000000000001,18.25));
#57779=CARTESIAN_POINT('Ctrl Pts',(30.0882156275205,-1.50000000000001,18.254244276358));
#57780=CARTESIAN_POINT('Ctrl Pts',(30.1764501130872,-1.49221937550789,18.2587055884823));
#57781=CARTESIAN_POINT('Ctrl Pts',(30.4546079281867,-1.44254775409159,18.2734682298626));
#57782=CARTESIAN_POINT('Ctrl Pts',(30.6370980720641,-1.37175281599007,18.2842148170619));
#57783=CARTESIAN_POINT('Ctrl Pts',(30.9691525442989,-1.16201577961996,18.3060168240942));
#57784=CARTESIAN_POINT('Ctrl Pts',(31.1145075241426,-1.02344071977941,18.3168595260404));
#57785=CARTESIAN_POINT('Ctrl Pts',(31.3375735551139,-0.704962761586156,
18.3364384054093));
#57786=CARTESIAN_POINT('Ctrl Pts',(31.4160050795816,-0.530113102524481,
18.345549272082));
#57787=CARTESIAN_POINT('Ctrl Pts',(31.5048780292219,-0.154342998497877,
18.3664253889724));
#57788=CARTESIAN_POINT('Ctrl Pts',(31.5121437205665,0.0435642244476196,
18.3774202346916));
#57789=CARTESIAN_POINT('Ctrl Pts',(31.4493976248982,0.435280459623824,18.3991822477569));
#57790=CARTESIAN_POINT('Ctrl Pts',(31.3782925123276,0.624894161678516,18.4093783750732));
#57791=CARTESIAN_POINT('Ctrl Pts',(31.1707210215853,0.957071364942045,18.428592307613));
#57792=CARTESIAN_POINT('Ctrl Pts',(31.0393074800838,1.09835818528463,18.4388395784748));
#57793=CARTESIAN_POINT('Ctrl Pts',(30.7245434883219,1.32834442072559,18.4603721746294));
#57794=CARTESIAN_POINT('Ctrl Pts',(30.5424433469957,1.41252449906513,18.4714718072734));
#57795=CARTESIAN_POINT('Ctrl Pts',(30.1611576166725,1.50380428740964,18.492351975203));
#57796=CARTESIAN_POINT('Ctrl Pts',(29.9661847612145,1.51203572283979,18.5012926108002));
#57797=CARTESIAN_POINT('Ctrl Pts',(29.583743920727,1.45401144673963,18.5213045897645));
#57798=CARTESIAN_POINT('Ctrl Pts',(29.3999206687447,1.38827539073469,18.5319747916547));
#57799=CARTESIAN_POINT('Ctrl Pts',(29.0627111089636,1.18787072518152,18.5537655904295));
#57800=CARTESIAN_POINT('Ctrl Pts',(28.9136362676481,1.05327089433686,18.5646768412665));
#57801=CARTESIAN_POINT('Ctrl Pts',(28.6818733006966,0.740747545450625,18.5845087463487));
#57802=CARTESIAN_POINT('Ctrl Pts',(28.5986773683508,0.567862991064222,18.593452056052));
#57803=CARTESIAN_POINT('Ctrl Pts',(28.4999017481138,0.194886335563048,18.6141729813576));
#57804=CARTESIAN_POINT('Ctrl Pts',(28.4872987443723,-0.0022124298529334,
18.6251229127696));
#57805=CARTESIAN_POINT('Ctrl Pts',(28.538885584329,-0.393300822235859,18.6468500456797));
#57806=CARTESIAN_POINT('Ctrl Pts',(28.6038229043615,-0.583241208522858,
18.6573608761808));
#57807=CARTESIAN_POINT('Ctrl Pts',(28.7997809979745,-0.919686600601166,
18.6761346196911));
#57808=CARTESIAN_POINT('Ctrl Pts',(28.9262538190534,-1.06460970419426,18.6862451878989));
#57809=CARTESIAN_POINT('Ctrl Pts',(29.2324514589516,-1.30386842227857,18.7076232042196));
#57810=CARTESIAN_POINT('Ctrl Pts',(29.4110795308611,-1.39369344460164,18.7187125908454));
#57811=CARTESIAN_POINT('Ctrl Pts',(29.7319270119205,-1.48199126728517,18.7366020897721));
#57812=CARTESIAN_POINT('Ctrl Pts',(29.8657845574029,-1.50000000000001,18.7435425565073));
#57813=CARTESIAN_POINT('Ctrl Pts',(30.0000000000002,-1.50000000000001,18.75));
#57814=CARTESIAN_POINT('Ctrl Pts',(30.,-1.50000000000001,18.8125));
#57815=CARTESIAN_POINT('Ctrl Pts',(29.9200694828282,-1.50000000000001,18.8086543411995));
#57816=CARTESIAN_POINT('Ctrl Pts',(29.8400989517173,-1.4936120985387,18.8046293155201));
#57817=CARTESIAN_POINT('Ctrl Pts',(29.5632380932733,-1.44889785862683,18.7900667790378));
#57818=CARTESIAN_POINT('Ctrl Pts',(29.3740258977232,-1.377754564609,18.7789871004233));
#57819=CARTESIAN_POINT('Ctrl Pts',(29.041174726881,-1.16949277461302,18.7571877412774));
#57820=CARTESIAN_POINT('Ctrl Pts',(28.8991316339595,-1.03690216726548,18.7466706173565));
#57821=CARTESIAN_POINT('Ctrl Pts',(28.6710550609186,-0.722648191218263,
18.7269680010074));
#57822=CARTESIAN_POINT('Ctrl Pts',(28.5881967902834,-0.543266122771758,
18.717681451265));
#57823=CARTESIAN_POINT('Ctrl Pts',(28.4956085723343,-0.160873384602161,
18.6964374102556));
#57824=CARTESIAN_POINT('Ctrl Pts',(28.4875239735192,0.0385552236194734,
18.6853580431322));
#57825=CARTESIAN_POINT('Ctrl Pts',(28.5480104653806,0.421875716785893,18.6640624601785));
#57826=CARTESIAN_POINT('Ctrl Pts',(28.6132160700899,0.602522755625134,18.6541515963916));
#57827=CARTESIAN_POINT('Ctrl Pts',(28.8119377533085,0.937035677616922,18.635298569339));
#57828=CARTESIAN_POINT('Ctrl Pts',(28.9464389491764,1.08605274148643,18.6246880146503));
#57829=CARTESIAN_POINT('Ctrl Pts',(29.2628767471001,1.32090830831045,18.6029396282541));
#57830=CARTESIAN_POINT('Ctrl Pts',(29.4409618987283,1.40557199772365,18.5920197332512));
#57831=CARTESIAN_POINT('Ctrl Pts',(29.814809484317,1.50065373381321,18.5713918235674));
#57832=CARTESIAN_POINT('Ctrl Pts',(30.0065604479866,1.51202122412194,18.5625182831912));
#57833=CARTESIAN_POINT('Ctrl Pts',(30.3943911928229,1.4610824148403,18.5424438008558));
#57834=CARTESIAN_POINT('Ctrl Pts',(30.58616263238,1.39524271133166,18.5313883125152));
#57835=CARTESIAN_POINT('Ctrl Pts',(30.9257469654151,1.19593240245758,18.5095136562056));
#57836=CARTESIAN_POINT('Ctrl Pts',(31.0718264769195,1.06698913560375,18.4989036450188));
#57837=CARTESIAN_POINT('Ctrl Pts',(31.3078217753803,0.759832047419874,18.4790171745892));
#57838=CARTESIAN_POINT('Ctrl Pts',(31.3951262846915,0.584269865007977,18.4699594369449));
#57839=CARTESIAN_POINT('Ctrl Pts',(31.4989966927882,0.205709858638526,18.4489283254799));
#57840=CARTESIAN_POINT('Ctrl Pts',(31.5130318328004,0.00600577899638372,
18.4378336543887));
#57841=CARTESIAN_POINT('Ctrl Pts',(31.4635867359632,-0.379900299649008,
18.4163944277973));
#57842=CARTESIAN_POINT('Ctrl Pts',(31.4034385131977,-0.562844950250642,
18.4062308360972));
#57843=CARTESIAN_POINT('Ctrl Pts',(31.213924427377,-0.903263174389702,18.387318712534));
#57844=CARTESIAN_POINT('Ctrl Pts',(31.0836707542498,-1.05603307941032,18.3769705479341));
#57845=CARTESIAN_POINT('Ctrl Pts',(30.7734274797909,-1.30006438227702,18.3552653141303));
#57846=CARTESIAN_POINT('Ctrl Pts',(30.5972523067208,-1.389838711312,18.3442953508018));
#57847=CARTESIAN_POINT('Ctrl Pts',(30.27555179434,-1.4809632576453,18.3262862902852));
#57848=CARTESIAN_POINT('Ctrl Pts',(30.1379932399681,-1.50000000000003,18.3191392028535));
#57849=CARTESIAN_POINT('Ctrl Pts',(29.9999999999998,-1.50000000000001,18.3125));
#57850=CARTESIAN_POINT('Origin',(30.,-1.32966554433622E-14,16.));
#57851=CARTESIAN_POINT('',(30.,-1.50000000000001,17.75));
#57852=CARTESIAN_POINT('',(30.,-1.50000000000001,17.8125));
#57853=CARTESIAN_POINT('',(30.,-1.50000000000001,16.));
#57854=CARTESIAN_POINT('Ctrl Pts',(30.,-1.50000000000001,17.75));
#57855=CARTESIAN_POINT('Ctrl Pts',(30.1165214576707,-1.50000000000002,17.755606141246));
#57856=CARTESIAN_POINT('Ctrl Pts',(30.2328774102524,-1.48642630258387,17.7615813667753));
#57857=CARTESIAN_POINT('Ctrl Pts',(30.5364815251301,-1.41429282343802,17.778192234317));
#57858=CARTESIAN_POINT('Ctrl Pts',(30.7156172892318,-1.33263663661631,17.7890791351975));
#57859=CARTESIAN_POINT('Ctrl Pts',(31.0356297737271,-1.1031687507031,17.8108498509785));
#57860=CARTESIAN_POINT('Ctrl Pts',(31.1725674881258,-0.956358157459637,
17.8215163418689));
#57861=CARTESIAN_POINT('Ctrl Pts',(31.376639002963,-0.625293846242278,17.8405309680715));
#57862=CARTESIAN_POINT('Ctrl Pts',(31.4447439774106,-0.445961069817197,
17.8502243850103));
#57863=CARTESIAN_POINT('Ctrl Pts',(31.5115582160321,-0.0642628969545898,
17.8714298390582));
#57864=CARTESIAN_POINT('Ctrl Pts',(31.5068955968845,0.134928419608339,17.8824960233117));
#57865=CARTESIAN_POINT('Ctrl Pts',(31.4208614242251,0.519471460613856,17.9038595255897));
#57866=CARTESIAN_POINT('Ctrl Pts',(31.3405819882652,0.701086441059189,17.9133091757132));
#57867=CARTESIAN_POINT('Ctrl Pts',(31.1170623100669,1.01937978501502,17.9329047530211));
#57868=CARTESIAN_POINT('Ctrl Pts',(30.9773620677606,1.15399638378434,17.9433654340287));
#57869=CARTESIAN_POINT('Ctrl Pts',(30.6484546459992,1.36726868066811,17.9651142302054));
#57870=CARTESIAN_POINT('Ctrl Pts',(30.4607652253454,1.44139714446346,17.9762035656613));
#57871=CARTESIAN_POINT('Ctrl Pts',(30.0756449322311,1.51026934438856,17.9966457910675));
#57872=CARTESIAN_POINT('Ctrl Pts',(29.8825476840369,1.50759466650969,18.005439964228));
#57873=CARTESIAN_POINT('Ctrl Pts',(29.5047175214704,1.42916638864856,18.025796889674));
#57874=CARTESIAN_POINT('Ctrl Pts',(29.323805468645,1.35298625851431,18.0366171395998));
#57875=CARTESIAN_POINT('Ctrl Pts',(28.9975535579724,1.13341344377778,18.0584131868245));
#57876=CARTESIAN_POINT('Ctrl Pts',(28.8562978602342,0.990703384015885,18.0691735230773));
#57877=CARTESIAN_POINT('Ctrl Pts',(28.6425900107442,0.665955504210131,18.088476321219));
#57878=CARTESIAN_POINT('Ctrl Pts',(28.5692557712623,0.488931672930093,18.0978371292817));
#57879=CARTESIAN_POINT('Ctrl Pts',(28.4911736103312,0.110209786397706,18.118877234089));
#57880=CARTESIAN_POINT('Ctrl Pts',(28.4897399259643,-0.0884146511275797,
18.1299119250627));
#57881=CARTESIAN_POINT('Ctrl Pts',(28.563963673652,-0.476687925939349,18.1514826625522));
#57882=CARTESIAN_POINT('Ctrl Pts',(28.6395954743022,-0.662348456736596,
18.1612794083161));
#57883=CARTESIAN_POINT('Ctrl Pts',(28.8549808751967,-0.987772207975308,
18.1806816918938));
#57884=CARTESIAN_POINT('Ctrl Pts',(28.9904690556508,-1.12587258901724,18.1910364917109));
#57885=CARTESIAN_POINT('Ctrl Pts',(29.3122241078786,-1.34783032180127,18.2126824314563));
#57886=CARTESIAN_POINT('Ctrl Pts',(29.4971108100191,-1.42716337813628,18.2237814930698));
#57887=CARTESIAN_POINT('Ctrl Pts',(29.7935943795659,-1.48934588454492,18.2397733573052));
#57888=CARTESIAN_POINT('Ctrl Pts',(29.8967698772032,-1.50000000000001,18.2450333384012));
#57889=CARTESIAN_POINT('Ctrl Pts',(30.,-1.50000000000001,18.25));
#57890=CARTESIAN_POINT('Ctrl Pts',(29.9999999999998,-1.50000000000001,18.3125));
#57891=CARTESIAN_POINT('Ctrl Pts',(29.9486057940186,-1.50000000000001,18.3100272951118));
#57892=CARTESIAN_POINT('Ctrl Pts',(29.8971583803719,-1.4973588143077,18.3074786639994));
#57893=CARTESIAN_POINT('Ctrl Pts',(29.6480074739756,-1.47161947014145,18.294776403644));
#57894=CARTESIAN_POINT('Ctrl Pts',(29.4562105276991,-1.41203266981329,18.2838933798658));
#57895=CARTESIAN_POINT('Ctrl Pts',(29.1116733937691,-1.22407639141983,18.2620958215476));
#57896=CARTESIAN_POINT('Ctrl Pts',(28.9612380534891,-1.09930641465076,18.2513921651757));
#57897=CARTESIAN_POINT('Ctrl Pts',(28.7165798694464,-0.800027931931824,
18.231307751621));
#57898=CARTESIAN_POINT('Ctrl Pts',(28.6244510402799,-0.628553460673264,
18.2224196367041));
#57899=CARTESIAN_POINT('Ctrl Pts',(28.5083938755392,-0.254315567480426,
18.2016286426378));
#57900=CARTESIAN_POINT('Ctrl Pts',(28.4878541874048,-0.054508044740069,
18.1905282247078));
#57901=CARTESIAN_POINT('Ctrl Pts',(28.5251827599344,0.333985841156563,18.1689452310469));
#57902=CARTESIAN_POINT('Ctrl Pts',(28.5797880070138,0.519280463308488,18.1586510853718));
#57903=CARTESIAN_POINT('Ctrl Pts',(28.7594942565881,0.866593796413574,18.1393559001993));
#57904=CARTESIAN_POINT('Ctrl Pts',(28.8856977548396,1.02381782162173,18.1293391744996));
#57905=CARTESIAN_POINT('Ctrl Pts',(29.1898211855382,1.2775694571787,18.1076583725746));
#57906=CARTESIAN_POINT('Ctrl Pts',(29.3638803222543,1.37256230066096,18.096645258358));
#57907=CARTESIAN_POINT('Ctrl Pts',(29.732534735318,1.48813273455022,18.0756980748094));
#57908=CARTESIAN_POINT('Ctrl Pts',(29.9228794435952,1.51000349618475,18.066488339394));
#57909=CARTESIAN_POINT('Ctrl Pts',(30.3105607244676,1.48091384388274,18.0470279691741));
#57910=CARTESIAN_POINT('Ctrl Pts',(30.5039294602603,1.4267400893485,18.0362196850207));
#57911=CARTESIAN_POINT('Ctrl Pts',(30.8540539626656,1.24831186951753,18.0144179726049));
#57912=CARTESIAN_POINT('Ctrl Pts',(31.0082947964679,1.12740587313612,18.0036385571291));
#57913=CARTESIAN_POINT('Ctrl Pts',(31.2606439376435,0.835225571389926,17.9833812839205));
#57914=CARTESIAN_POINT('Ctrl Pts',(31.3570327509323,0.667298431844612,17.9745721351024));
#57915=CARTESIAN_POINT('Ctrl Pts',(31.4837741625619,0.297001147228916,17.9540000637349));
#57916=CARTESIAN_POINT('Ctrl Pts',(31.5100733842477,0.0972732161684081,
17.9429040675649));
#57917=CARTESIAN_POINT('Ctrl Pts',(31.4835317838137,-0.293194316444828,
17.9212114268642));
#57918=CARTESIAN_POINT('Ctrl Pts',(31.4338905957024,-0.480424140062753,
17.9108097699965));
#57919=CARTESIAN_POINT('Ctrl Pts',(31.2642037542022,-0.83118542637216,17.8913230318682));
#57920=CARTESIAN_POINT('Ctrl Pts',(31.14378015867,-0.99038786521744,17.8816860411746));
#57921=CARTESIAN_POINT('Ctrl Pts',(30.8486060826855,-1.25246692848107,17.8602044978428));
#57922=CARTESIAN_POINT('Ctrl Pts',(30.6769673305094,-1.35296725332812,17.8491548488382));
#57923=CARTESIAN_POINT('Ctrl Pts',(30.3327732686651,-1.47215364288648,17.8292840712733));
#57924=CARTESIAN_POINT('Ctrl Pts',(30.1668871533766,-1.50000000000002,17.8205293619105));
#57925=CARTESIAN_POINT('Ctrl Pts',(29.9999999999999,-1.50000000000001,17.8125));
#57926=CARTESIAN_POINT('Origin',(30.,-1.32966554433622E-14,16.));
#57927=CARTESIAN_POINT('',(29.9999999999999,-1.50000000000001,17.25));
#57928=CARTESIAN_POINT('',(30.,-1.50000000000001,17.3125));
#57929=CARTESIAN_POINT('',(30.,-1.50000000000001,16.));
#57930=CARTESIAN_POINT('Ctrl Pts',(29.9999999999998,-1.50000000000001,17.25));
#57931=CARTESIAN_POINT('Ctrl Pts',(30.1437406795734,-1.50000000000003,17.2569157266704));
#57932=CARTESIAN_POINT('Ctrl Pts',(30.2869532673798,-1.47934432155244,17.2643798143597));
#57933=CARTESIAN_POINT('Ctrl Pts',(30.6133040117111,-1.38286217393555,17.2827614315232));
#57934=CARTESIAN_POINT('Ctrl Pts',(30.7886268831202,-1.29093521604786,17.2937501837148));
#57935=CARTESIAN_POINT('Ctrl Pts',(31.0976621700988,-1.04186059007729,17.3155373905022));
#57936=CARTESIAN_POINT('Ctrl Pts',(31.2270940102629,-0.885739363684009,
17.3257922575731));
#57937=CARTESIAN_POINT('Ctrl Pts',(31.4122925189225,-0.540349731904653,
17.3449805704497));
#57938=CARTESIAN_POINT('Ctrl Pts',(31.4695815451721,-0.356167506723217,
17.3552129162933));
#57939=CARTESIAN_POINT('Ctrl Pts',(31.5127670349393,0.0311250181831806,
17.376729167677));
#57940=CARTESIAN_POINT('Ctrl Pts',(31.4953668358477,0.230908289106308,17.3878282382838));
#57941=CARTESIAN_POINT('Ctrl Pts',(31.3851742993692,0.607249385403804,17.408736076967));
#57942=CARTESIAN_POINT('Ctrl Pts',(31.2953707932844,0.78068569360338,17.4176954906944));
#57943=CARTESIAN_POINT('Ctrl Pts',(31.054895847731,1.08378386704463,17.4376847406135));
#57944=CARTESIAN_POINT('Ctrl Pts',(30.9065553840191,1.21059289157644,17.4483442474051));
#57945=CARTESIAN_POINT('Ctrl Pts',(30.5651448786952,1.40362381134034,17.4701323379946));
#57946=CARTESIAN_POINT('Ctrl Pts',(30.3742618691092,1.46611551598061,17.4810520817598));
#57947=CARTESIAN_POINT('Ctrl Pts',(29.9878426931301,1.51196372025337,17.5009172442622));
#57948=CARTESIAN_POINT('Ctrl Pts',(29.7964276873605,1.49824842026232,17.5098430324513));
#57949=CARTESIAN_POINT('Ctrl Pts',(29.423704438961,1.39861791618851,17.5305432021031));
#57950=CARTESIAN_POINT('Ctrl Pts',(29.2464613140656,1.31164870813791,17.5414866272603));
#57951=CARTESIAN_POINT('Ctrl Pts',(28.9327465597656,1.07261781027188,17.5632199825769));
#57952=CARTESIAN_POINT('Ctrl Pts',(28.8001758891987,0.921899105215767,17.5737833830436));
#57953=CARTESIAN_POINT('Ctrl Pts',(28.6055876448106,0.584753731199478,17.5925136816001));
#57954=CARTESIAN_POINT('Ctrl Pts',(28.5426610065469,0.403064732761888,17.6026075148466));
#57955=CARTESIAN_POINT('Ctrl Pts',(28.487113056257,0.0186136653436067,17.623965907481));
#57956=CARTESIAN_POINT('Ctrl Pts',(28.4978576022209,-0.180959534499292,
17.6350533074722));
#57957=CARTESIAN_POINT('Ctrl Pts',(28.5955062015491,-0.561653522812593,
17.6562029734896));
#57958=CARTESIAN_POINT('Ctrl Pts',(28.6803571582567,-0.739318323214391,
17.6653786075964));
#57959=CARTESIAN_POINT('Ctrl Pts',(28.9119736981394,-1.05041195534416,17.6851637533487));
#57960=CARTESIAN_POINT('Ctrl Pts',(29.0558270731865,-1.1813919096406,17.6957232341464));
#57961=CARTESIAN_POINT('Ctrl Pts',(29.3917078154049,-1.38569020760041,17.7175582566121));
#57962=CARTESIAN_POINT('Ctrl Pts',(29.5820781032457,-1.45448064464283,17.7286282968298));
#57963=CARTESIAN_POINT('Ctrl Pts',(29.8532284268276,-1.49461899708891,17.7427889770903));
#57964=CARTESIAN_POINT('Ctrl Pts',(29.9266397495672,-1.50000000000001,17.7464704533054));
#57965=CARTESIAN_POINT('Ctrl Pts',(30.,-1.50000000000001,17.75));
#57966=CARTESIAN_POINT('Ctrl Pts',(29.9999999999999,-1.50000000000001,17.8125));
#57967=CARTESIAN_POINT('Ctrl Pts',(29.9772840745252,-1.50000000000001,17.811407079526));
#57968=CARTESIAN_POINT('Ctrl Pts',(29.9545509622526,-1.49948399224778,17.8102989986031));
#57969=CARTESIAN_POINT('Ctrl Pts',(29.7331702393738,-1.48941079200354,17.7993680024896));
#57970=CARTESIAN_POINT('Ctrl Pts',(29.5383211874472,-1.44096198242896,17.7886475228419));
#57971=CARTESIAN_POINT('Ctrl Pts',(29.1826189299973,-1.27271128807371,17.7668601596023));
#57972=CARTESIAN_POINT('Ctrl Pts',(29.0244894301944,-1.15598200374574,17.7560096703756));
#57973=CARTESIAN_POINT('Ctrl Pts',(28.764135320164,-0.871290254073719,17.7355752732588));
#57974=CARTESIAN_POINT('Ctrl Pts',(28.6633306533142,-0.706980266162622,
17.7267766814534));
#57975=CARTESIAN_POINT('Ctrl Pts',(28.5256044330412,-0.340872542641299,
17.70643736348));
#57976=CARTESIAN_POINT('Ctrl Pts',(28.4933384090279,-0.141395913779689,
17.6953553285433));
#57977=CARTESIAN_POINT('Ctrl Pts',(28.5086475773052,0.250803035896437,17.6735664980057));
#57978=CARTESIAN_POINT('Ctrl Pts',(28.5530910089168,0.439894111123241,17.6630614382709));
#57979=CARTESIAN_POINT('Ctrl Pts',(28.7124602775381,0.794124581104987,17.6433819677164));
#57980=CARTESIAN_POINT('Ctrl Pts',(28.8270773285161,0.955330804312479,17.6340619682235));
#57981=CARTESIAN_POINT('Ctrl Pts',(29.1130611662184,1.22571784831621,17.6127918131944));
#57982=CARTESIAN_POINT('Ctrl Pts',(29.2820600929988,1.33176716482588,17.6017150341911));
#57983=CARTESIAN_POINT('Ctrl Pts',(29.6446531268203,1.46968030941703,17.5804388480344));
#57984=CARTESIAN_POINT('Ctrl Pts',(29.8337664889299,1.50284763615596,17.5705770145346));
#57985=CARTESIAN_POINT('Ctrl Pts',(30.2227595353817,1.49663210693258,17.5516889242716));
#57986=CARTESIAN_POINT('Ctrl Pts',(30.4189176611452,1.45396403183943,17.5410660377374));
#57987=CARTESIAN_POINT('Ctrl Pts',(30.7799134803451,1.29609345193241,17.5193123244018));
#57988=CARTESIAN_POINT('Ctrl Pts',(30.9418307309724,1.18367445855365,17.5083993272327));
#57989=CARTESIAN_POINT('Ctrl Pts',(31.2101475557693,0.906543829758461,17.4877918549585));
#57990=CARTESIAN_POINT('Ctrl Pts',(31.3153431699375,0.745751786456619,17.478930654803));
#57991=CARTESIAN_POINT('Ctrl Pts',(31.463864637894,0.383898047749162,17.4588276693193));
#57992=CARTESIAN_POINT('Ctrl Pts',(31.5020303054666,0.184838532612863,17.4477688073673));
#57993=CARTESIAN_POINT('Ctrl Pts',(31.4978841524782,-0.208759642694536,
17.4259022420724));
#57994=CARTESIAN_POINT('Ctrl Pts',(31.4586348080642,-0.399547636290809,
17.4153029090948));
#57995=CARTESIAN_POINT('Ctrl Pts',(31.3094217036004,-0.757113584921528,
17.3954381341709));
#57996=CARTESIAN_POINT('Ctrl Pts',(31.200380183046,-0.920271802442848,17.3863568795276));
#57997=CARTESIAN_POINT('Ctrl Pts',(30.923406682912,-1.19858244148629,17.3653001347046));
#57998=CARTESIAN_POINT('Ctrl Pts',(30.7571425046312,-1.30996529750999,17.3542067774745));
#57999=CARTESIAN_POINT('Ctrl Pts',(30.3978227489156,-1.45880886920802,17.3327844540089));
#58000=CARTESIAN_POINT('Ctrl Pts',(30.2092450764931,-1.49754020852369,17.3226356359777));
#58001=CARTESIAN_POINT('Ctrl Pts',(30.0122952852091,-1.49996221637769,17.3130926067305));
#58002=CARTESIAN_POINT('Ctrl Pts',(30.0061468402235,-1.50000000000001,17.3127957399881));
#58003=CARTESIAN_POINT('Ctrl Pts',(30.,-1.50000000000001,17.3125));
#58004=CARTESIAN_POINT('Origin',(30.,-1.32966554433622E-14,16.));
#58005=CARTESIAN_POINT('',(30.,-1.50000000000001,16.75));
#58006=CARTESIAN_POINT('',(30.0000000000001,-1.50000000000001,16.8125));
#58007=CARTESIAN_POINT('',(30.,-1.50000000000001,16.));
#58008=CARTESIAN_POINT('Ctrl Pts',(30.,-1.50000000000001,16.75));
#58009=CARTESIAN_POINT('Ctrl Pts',(30.1733135774153,-1.50000000000002,16.7583385533812));
#58010=CARTESIAN_POINT('Ctrl Pts',(30.3454665850143,-1.46996630625128,16.767455538092));
#58011=CARTESIAN_POINT('Ctrl Pts',(30.6943533649566,-1.34416445320596,16.7877358570363));
#58012=CARTESIAN_POINT('Ctrl Pts',(30.8648984846931,-1.24131259552183,16.7987982089822));
#58013=CARTESIAN_POINT('Ctrl Pts',(31.1561999433551,-0.975703692756434,
16.8201914820235));
#58014=CARTESIAN_POINT('Ctrl Pts',(31.2741613882488,-0.815654351280513,
16.8296858693734));
#58015=CARTESIAN_POINT('Ctrl Pts',(31.4395048489934,-0.463422668720622,
16.8492542961822));
#58016=CARTESIAN_POINT('Ctrl Pts',(31.4869681438372,-0.275392752547583,
16.8597004026363));
#58017=CARTESIAN_POINT('Ctrl Pts',(31.5087956503657,0.115841301406496,16.881435627856));
#58018=CARTESIAN_POINT('Ctrl Pts',(31.4799884843839,0.315484512989904,16.8925269173884));
#58019=CARTESIAN_POINT('Ctrl Pts',(31.3486206066034,0.684034451059388,16.9130019139478));
#58020=CARTESIAN_POINT('Ctrl Pts',(31.2503774147184,0.850433854559545,16.9217976845453));
#58021=CARTESIAN_POINT('Ctrl Pts',(30.994668844219,1.13948462780369,16.9421296570253));
#58022=CARTESIAN_POINT('Ctrl Pts',(30.8387866934565,1.25865700214481,16.9529398842324));
#58023=CARTESIAN_POINT('Ctrl Pts',(30.4862910667067,1.43284604521895,16.9747379225116));
#58024=CARTESIAN_POINT('Ctrl Pts',(30.2922814189341,1.48462820882751,16.9855106094757));
#58025=CARTESIAN_POINT('Ctrl Pts',(29.904287970164,1.50893843055208,17.0048532369201));
#58026=CARTESIAN_POINT('Ctrl Pts',(29.714222422622,1.48472560659638,17.014173768808));
#58027=CARTESIAN_POINT('Ctrl Pts',(29.3467837907597,1.36454370703768,17.0351905543248));
#58028=CARTESIAN_POINT('Ctrl Pts',(29.1737126610206,1.26724866527873,17.0462200829857));
#58029=CARTESIAN_POINT('Ctrl Pts',(28.8733100927186,1.01000510192613,17.0678188628294));
#58030=CARTESIAN_POINT('Ctrl Pts',(28.7495253450837,0.851954282658887,17.0776692065189));
#58031=CARTESIAN_POINT('Ctrl Pts',(28.5739823591041,0.503198698880474,17.0970445167289));
#58032=CARTESIAN_POINT('Ctrl Pts',(28.5214293436323,0.317084997718663,17.1073841667934));
#58033=CARTESIAN_POINT('Ctrl Pts',(28.4885674976081,-0.0722634762162506,
17.1290146375676));
#58034=CARTESIAN_POINT('Ctrl Pts',(28.5114956545415,-0.272057456078969,
17.1401143031155));
#58035=CARTESIAN_POINT('Ctrl Pts',(28.6319945909535,-0.644674063533988,
17.1608152257519));
#58036=CARTESIAN_POINT('Ctrl Pts',(28.7258902835189,-0.814669507709904,
17.1696624095652));
#58037=CARTESIAN_POINT('Ctrl Pts',(28.9737348011573,-1.1110192567928,17.1898187719544));
#58038=CARTESIAN_POINT('Ctrl Pts',(29.1257542814876,-1.2342064357884,17.2005546786951));
#58039=CARTESIAN_POINT('Ctrl Pts',(29.4726321438156,-1.41824610841819,17.2223560607564));
#58040=CARTESIAN_POINT('Ctrl Pts',(29.6650975807577,-1.47560141498182,17.2332092613688));
#58041=CARTESIAN_POINT('Ctrl Pts',(29.9087297050291,-1.49791971441829,17.2455509701752));
#58042=CARTESIAN_POINT('Ctrl Pts',(29.9543886563371,-1.50000000000001,17.2478055232048));
#58043=CARTESIAN_POINT('Ctrl Pts',(29.9999999999998,-1.50000000000001,17.25));
#58044=CARTESIAN_POINT('Ctrl Pts',(30.,-1.50000000000001,17.3125));
#58045=CARTESIAN_POINT('Ctrl Pts',(29.8075276745562,-1.50000000000001,17.3032396709245));
#58046=CARTESIAN_POINT('Ctrl Pts',(29.6167265402445,-1.46295509134636,17.2930307218294));
#58047=CARTESIAN_POINT('Ctrl Pts',(29.2565239800332,-1.31741270776536,17.2716576240826));
#58048=CARTESIAN_POINT('Ctrl Pts',(29.0910935230227,-1.20922562866616,17.2606931508671));
#58049=CARTESIAN_POINT('Ctrl Pts',(28.8152192771185,-0.939380042859163,
17.2399244343056));
#58050=CARTESIAN_POINT('Ctrl Pts',(28.7058473428781,-0.781856067083356,
17.2309364481713));
#58051=CARTESIAN_POINT('Ctrl Pts',(28.5481536416827,-0.426269472803969,
17.211181637378));
#58052=CARTESIAN_POINT('Ctrl Pts',(28.5044938401357,-0.230229772369996,
17.2002905429095));
#58053=CARTESIAN_POINT('Ctrl Pts',(28.4962752409133,0.162097483734217,17.178494584237));
#58054=CARTESIAN_POINT('Ctrl Pts',(28.5297146688179,0.3545967167103,17.167800182405));
#58055=CARTESIAN_POINT('Ctrl Pts',(28.6677231734513,0.715751667501951,17.1477360184722));
#58056=CARTESIAN_POINT('Ctrl Pts',(28.7707689938353,0.881053857184024,17.1388343527704));
#58057=CARTESIAN_POINT('Ctrl Pts',(29.0378553430027,1.16782543883526,17.1180182775366));
#58058=CARTESIAN_POINT('Ctrl Pts',(29.2009578477084,1.28493633443696,17.1069179241867));
#58059=CARTESIAN_POINT('Ctrl Pts',(29.5564777297123,1.44564779283652,17.0853487587108));
#58060=CARTESIAN_POINT('Ctrl Pts',(29.7443345881639,1.49039149544099,17.0750676107666));
#58061=CARTESIAN_POINT('Ctrl Pts',(30.1352017346056,1.50720082969336,17.0557950804638));
#58062=CARTESIAN_POINT('Ctrl Pts',(30.3346031531762,1.47580805773789,17.0457293998907));
#58063=CARTESIAN_POINT('Ctrl Pts',(30.7060862860091,1.33790450333634,17.02402575504));
#58064=CARTESIAN_POINT('Ctrl Pts',(30.8749553104054,1.23409963004519,17.0130175716131));
#58065=CARTESIAN_POINT('Ctrl Pts',(31.1584137835032,0.971677105747927,16.9920901549037));
#58066=CARTESIAN_POINT('Ctrl Pts',(31.271994699923,0.817368296550736,16.9829093498084));
#58067=CARTESIAN_POINT('Ctrl Pts',(31.4394257557863,0.466485221859018,16.9634158456588));
#58068=CARTESIAN_POINT('Ctrl Pts',(31.488516036617,0.271760297088586,16.9525977942827));
#58069=CARTESIAN_POINT('Ctrl Pts',(31.5076810248584,-0.120678265071266,
16.9307956519405));
#58070=CARTESIAN_POINT('Ctrl Pts',(31.4794384691607,-0.314545865899112,
16.9200252296723));
#58071=CARTESIAN_POINT('Ctrl Pts',(31.3513352758344,-0.678794152386266,
16.8997892137563));
#58072=CARTESIAN_POINT('Ctrl Pts',(31.2534603041453,-0.845994238167287,
16.890973963719));
#58073=CARTESIAN_POINT('Ctrl Pts',(30.9950590391717,-1.14001068930543,16.8703745034186));
#58074=CARTESIAN_POINT('Ctrl Pts',(30.8348670617779,-1.26204295887652,16.8592774780469));
#58075=CARTESIAN_POINT('Ctrl Pts',(30.4829704713108,-1.43301939771413,16.8375974999208));
#58076=CARTESIAN_POINT('Ctrl Pts',(30.2958966065637,-1.48299380376918,16.8272087264607));
#58077=CARTESIAN_POINT('Ctrl Pts',(30.0696474084832,-1.49878860163674,16.8158845624575));
#58078=CARTESIAN_POINT('Ctrl Pts',(30.0348056486057,-1.50000000000001,16.8141745875493));
#58079=CARTESIAN_POINT('Ctrl Pts',(30.0000000000002,-1.50000000000001,16.8125));
#58080=CARTESIAN_POINT('Origin',(30.,-1.32966554433622E-14,16.));
#58081=CARTESIAN_POINT('',(30.0000000000023,1.33373412263454,16.1584936490537));
#58082=CARTESIAN_POINT('',(30.,1.1752404735808,16.));
#58083=CARTESIAN_POINT('',(30.,1.17524047358083,16.));
#58084=CARTESIAN_POINT('',(30.,-1.17524047358085,16.));
#58085=CARTESIAN_POINT('Ctrl Pts',(30.,-1.17524047358083,16.));
#58086=CARTESIAN_POINT('Ctrl Pts',(30.0938726776238,-1.17889502189498,16.0036545483141));
#58087=CARTESIAN_POINT('Ctrl Pts',(30.2222715669962,-1.17292308708929,16.0088746896198));
#58088=CARTESIAN_POINT('Ctrl Pts',(30.4821758748939,-1.10061359842964,16.0205734257761));
#58089=CARTESIAN_POINT('Ctrl Pts',(30.5904809486724,-1.05245648363552,16.0257840816621));
#58090=CARTESIAN_POINT('Ctrl Pts',(30.8133642274912,-0.91102859460423,16.0372929849601));
#58091=CARTESIAN_POINT('Ctrl Pts',(30.9213977318432,-0.810903247446717,
16.0434573291476));
#58092=CARTESIAN_POINT('Ctrl Pts',(31.1067869536601,-0.562636269482013,
16.0555173993883));
#58093=CARTESIAN_POINT('Ctrl Pts',(31.1779495349821,-0.411557996758087,
16.0617064115579));
#58094=CARTESIAN_POINT('Ctrl Pts',(31.2569648094213,-0.0966670523057213,
16.075198195417));
#58095=CARTESIAN_POINT('Ctrl Pts',(31.2657685184509,0.0650399419384585,
16.0820144838088));
#58096=CARTESIAN_POINT('Ctrl Pts',(31.2286447980599,0.334175553677255,16.0931820826379));
#58097=CARTESIAN_POINT('Ctrl Pts',(31.1927617340632,0.495209878479218,16.0995752755442));
#58098=CARTESIAN_POINT('Ctrl Pts',(31.0046982036223,0.825162649859306,16.1133508913014));
#58099=CARTESIAN_POINT('Ctrl Pts',(30.8901527526008,0.956864086379422,16.1201881413696));
#58100=CARTESIAN_POINT('Ctrl Pts',(30.6234294043457,1.16264469041258,16.1337830625282));
#58101=CARTESIAN_POINT('Ctrl Pts',(30.4758334589096,1.2374906559331,16.1404068749596));
#58102=CARTESIAN_POINT('Ctrl Pts',(30.2026344427889,1.31649705751482,16.1513204506313));
#58103=CARTESIAN_POINT('Ctrl Pts',(30.094862299376,1.33047991225226,16.1552394386714));
#58104=CARTESIAN_POINT('Ctrl Pts',(30.0000000000046,1.33373412263454,16.1584936490537));
#58105=CARTESIAN_POINT('Origin',(30.,-1.32966554433622E-14,16.));
#58106=CARTESIAN_POINT('Origin',(30.,-1.21864324187371E-14,15.78125));
#58107=CARTESIAN_POINT('',(30.0000000000002,-1.17524047358085,16.0625));
#58108=CARTESIAN_POINT('',(30.,-1.17524047358085,15.78125));
#58109=CARTESIAN_POINT('',(29.1765921258349,-0.838564036615843,16.));
#58110=CARTESIAN_POINT('Ctrl Pts',(30.0000000000004,-1.17524047358085,16.0625));
#58111=CARTESIAN_POINT('Ctrl Pts',(29.8936372832897,-1.17524047358089,16.0559685129868));
#58112=CARTESIAN_POINT('Ctrl Pts',(29.7875857388152,-1.16080842474563,16.0489444642731));
#58113=CARTESIAN_POINT('Ctrl Pts',(29.5893382840682,-1.10559796441283,16.034813132098));
#58114=CARTESIAN_POINT('Ctrl Pts',(29.4977179176601,-1.06709869274158,16.0278219954706));
#58115=CARTESIAN_POINT('Ctrl Pts',(29.3263212626278,-0.968061456605931,
16.0137856854629));
#58116=CARTESIAN_POINT('Ctrl Pts',(29.2472234502441,-0.90791877416947,16.0067961899552));
#58117=CARTESIAN_POINT('Ctrl Pts',(29.176592125834,-0.838564036614912,15.9999999999999));
#58118=CARTESIAN_POINT('Origin',(30.,-1.32966554433622E-14,16.));
#58119=CARTESIAN_POINT('Origin',(30.,-1.21864324187371E-14,15.78125));
#58120=CARTESIAN_POINT('',(30.0000000000002,-1.17524047358085,16.5625));
#58121=CARTESIAN_POINT('',(30.,-1.17524047358085,16.5));
#58122=CARTESIAN_POINT('',(30.,-1.17524047358085,15.78125));
#58123=CARTESIAN_POINT('Ctrl Pts',(30.0000000000004,-1.17524047358085,16.5625));
#58124=CARTESIAN_POINT('Ctrl Pts',(29.8712710011335,-1.17524047358089,16.5545950516279));
#58125=CARTESIAN_POINT('Ctrl Pts',(29.7432544697015,-1.15409887958747,16.5459843057103));
#58126=CARTESIAN_POINT('Ctrl Pts',(29.4749058017838,-1.06268366571272,16.5262646272929));
#58127=CARTESIAN_POINT('Ctrl Pts',(29.3400104190766,-0.984598569044377,
16.515212607152));
#58128=CARTESIAN_POINT('Ctrl Pts',(29.1121607207208,-0.784303734398693,
16.4941196868072));
#58129=CARTESIAN_POINT('Ctrl Pts',(29.0200231478196,-0.665589512335134,
16.4846952710458));
#58130=CARTESIAN_POINT('Ctrl Pts',(28.8817974975863,-0.393869611486594,
16.465428299239));
#58131=CARTESIAN_POINT('Ctrl Pts',(28.83947486215,-0.242215228858268,16.4546748700446));
#58132=CARTESIAN_POINT('Ctrl Pts',(28.8167032491755,0.0653802904577292,
16.4328640487538));
#58133=CARTESIAN_POINT('Ctrl Pts',(28.8351718353917,0.218291541824621,16.422021498172));
#58134=CARTESIAN_POINT('Ctrl Pts',(28.9287391651494,0.506051914833821,16.4016171370023));
#58135=CARTESIAN_POINT('Ctrl Pts',(29.0019741006921,0.638460005621421,16.3928173224174));
#58136=CARTESIAN_POINT('Ctrl Pts',(29.1986594960153,0.873851822283252,16.3723938102577));
#58137=CARTESIAN_POINT('Ctrl Pts',(29.3222166226463,0.972810188230982,16.3612980106481));
#58138=CARTESIAN_POINT('Ctrl Pts',(29.5955374213776,1.11370354874836,16.3395188200451));
#58139=CARTESIAN_POINT('Ctrl Pts',(29.7416409158841,1.1563714827732,16.3290342066007));
#58140=CARTESIAN_POINT('Ctrl Pts',(30.0452139523297,1.18442751027465,16.309397801581));
#58141=CARTESIAN_POINT('Ctrl Pts',(30.1998697024494,1.16832333055968,16.2999812279383));
#58142=CARTESIAN_POINT('Ctrl Pts',(30.4949641982123,1.07710916023858,16.2786262781941));
#58143=CARTESIAN_POINT('Ctrl Pts',(30.6323783558426,1.00262103976947,16.2675471121926));
#58144=CARTESIAN_POINT('Ctrl Pts',(30.8661146099677,0.80826573510396,16.246303290685));
#58145=CARTESIAN_POINT('Ctrl Pts',(30.9615634972897,0.691955855651338,16.2365648418493));
#58146=CARTESIAN_POINT('Ctrl Pts',(31.1071384709944,0.423965303495795,16.217562308738));
#58147=CARTESIAN_POINT('Ctrl Pts',(31.153539286677,0.273539680121433,16.2068960077584));
#58148=CARTESIAN_POINT('Ctrl Pts',(31.1846742020807,-0.0336925499575308,
16.1851109463897));
#58149=CARTESIAN_POINT('Ctrl Pts',(31.1702391074247,-0.187447361382806,
16.174208581095));
#58150=CARTESIAN_POINT('Ctrl Pts',(31.0842361864784,-0.477469105777865,
16.1536438717926));
#58151=CARTESIAN_POINT('Ctrl Pts',(31.0147909316618,-0.611342914691707,
16.1448082262658));
#58152=CARTESIAN_POINT('Ctrl Pts',(30.8246452237759,-0.851973319529638,
16.1246005735716));
#58153=CARTESIAN_POINT('Ctrl Pts',(30.7034471847234,-0.954486386541281,
16.1135236126058));
#58154=CARTESIAN_POINT('Ctrl Pts',(30.4332129266933,-1.10289061678379,16.0916676708875));
#58155=CARTESIAN_POINT('Ctrl Pts',(30.2878849143487,-1.14942616400118,16.0810935566577));
#58156=CARTESIAN_POINT('Ctrl Pts',(30.0919105154022,-1.17254804866719,16.0682394674743));
#58157=CARTESIAN_POINT('Ctrl Pts',(30.0459321343385,-1.17524047358084,16.0653205855228));
#58158=CARTESIAN_POINT('Ctrl Pts',(30.0000000000004,-1.17524047358085,16.0625));
#58159=CARTESIAN_POINT('Ctrl Pts',(29.9999999999986,-1.17524047358085,15.9999999999999));
#58160=CARTESIAN_POINT('Ctrl Pts',(30.1214028111116,-1.17524047358099,16.0074550642242));
#58161=CARTESIAN_POINT('Ctrl Pts',(30.2421537204218,-1.15643017464734,16.0155369920666));
#58162=CARTESIAN_POINT('Ctrl Pts',(30.4776301337898,-1.08113291233427,16.0326666201836));
#58163=CARTESIAN_POINT('Ctrl Pts',(30.5903997908,-1.02391620718435,16.0416200885134));
#58164=CARTESIAN_POINT('Ctrl Pts',(30.8179173133188,-0.858187726048923,
16.0614671043063));
#58165=CARTESIAN_POINT('Ctrl Pts',(30.9244135286053,-0.742266950950034,
16.0721166138301));
#58166=CARTESIAN_POINT('Ctrl Pts',(31.0824458543846,-0.481384401141323,
16.0910702726526));
#58167=CARTESIAN_POINT('Ctrl Pts',(31.1347636661213,-0.340257482296023,
16.1008732014181));
#58168=CARTESIAN_POINT('Ctrl Pts',(31.1847167047507,-0.0402726429290417,
16.1221443686182));
#58169=CARTESIAN_POINT('Ctrl Pts',(31.1797095913038,0.116033015525934,16.1332276080324));
#58170=CARTESIAN_POINT('Ctrl Pts',(31.1096057651028,0.416692954381308,16.1545466448319));
#58171=CARTESIAN_POINT('Ctrl Pts',(31.0456145958404,0.558153128413804,16.1639131875247));
#58172=CARTESIAN_POINT('Ctrl Pts',(30.868452148125,0.806074678480504,16.1835820667589));
#58173=CARTESIAN_POINT('Ctrl Pts',(30.7578944192075,0.910792535772415,16.1940837990854));
#58174=CARTESIAN_POINT('Ctrl Pts',(30.4982839285527,1.07586594639843,16.2158783446996));
#58175=CARTESIAN_POINT('Ctrl Pts',(30.350445183185,1.13268560339106,16.2269712473271));
#58176=CARTESIAN_POINT('Ctrl Pts',(30.0480054721768,1.18378716120051,16.2473551076386));
#58177=CARTESIAN_POINT('Ctrl Pts',(29.8968386090012,1.18026105605562,16.2561569026374));
#58178=CARTESIAN_POINT('Ctrl Pts',(29.6011798659176,1.11599305250821,16.276591159187));
#58179=CARTESIAN_POINT('Ctrl Pts',(29.4597499374869,1.05480717934155,16.2874453099545));
#58180=CARTESIAN_POINT('Ctrl Pts',(29.2055652972218,0.87997645163687,16.3092526000714));
#58181=CARTESIAN_POINT('Ctrl Pts',(29.0959568884663,0.766951615708884,16.3199905502909));
#58182=CARTESIAN_POINT('Ctrl Pts',(28.9310246543964,0.510549118020342,16.3392090818415));
#58183=CARTESIAN_POINT('Ctrl Pts',(28.8749728808886,0.371095429589151,16.348686560472));
#58184=CARTESIAN_POINT('Ctrl Pts',(28.8169184420094,0.0732292943615943,
16.3698074957134));
#58185=CARTESIAN_POINT('Ctrl Pts',(28.817543647408,-0.0827153411142831,
16.3808651359001));
#58186=CARTESIAN_POINT('Ctrl Pts',(28.8792006517981,-0.386085589929172,
16.4023763539327));
#58187=CARTESIAN_POINT('Ctrl Pts',(28.9398691853048,-0.530428612710414,
16.4120388426041));
#58188=CARTESIAN_POINT('Ctrl Pts',(29.1111806434797,-0.783487027051828,
16.4315305472161));
#58189=CARTESIAN_POINT('Ctrl Pts',(29.2187204550675,-0.890749010718532,
16.441937155047));
#58190=CARTESIAN_POINT('Ctrl Pts',(29.4732317621912,-1.06214794881238,16.4636428352494));
#58191=CARTESIAN_POINT('Ctrl Pts',(29.6190899112583,-1.1227476098516,16.4747481293347));
#58192=CARTESIAN_POINT('Ctrl Pts',(29.8476395120001,-1.16783357420714,16.490381294589));
#58193=CARTESIAN_POINT('Ctrl Pts',(29.9238084968367,-1.17524047358085,16.4953212570267));
#58194=CARTESIAN_POINT('Ctrl Pts',(30.,-1.17524047358085,16.5));
#58195=CARTESIAN_POINT('Origin',(30.,-1.21864324187371E-14,15.78125));
#58196=CARTESIAN_POINT('',(30.,-1.17524047358085,17.0625));
#58197=CARTESIAN_POINT('',(30.0000000000001,-1.17524047358085,17.));
#58198=CARTESIAN_POINT('',(30.,-1.17524047358085,15.78125));
#58199=CARTESIAN_POINT('Ctrl Pts',(30.,-1.17524047358085,17.0625));
#58200=CARTESIAN_POINT('Ctrl Pts',(29.8500434788821,-1.17524047358086,17.0532915188657));
#58201=CARTESIAN_POINT('Ctrl Pts',(29.7013448813168,-1.14654165820119,17.0431428036379));
#58202=CARTESIAN_POINT('Ctrl Pts',(29.4194581258723,-1.03331719487298,17.0218185633632));
#58203=CARTESIAN_POINT('Ctrl Pts',(29.2895397758247,-0.948696042884902,
17.0108404436342));
#58204=CARTESIAN_POINT('Ctrl Pts',(29.0728347660888,-0.737413048700427,
16.9900423213744));
#58205=CARTESIAN_POINT('Ctrl Pts',(28.9869014388118,-0.614031092098323,
16.9810393937031));
#58206=CARTESIAN_POINT('Ctrl Pts',(28.8628735458866,-0.335358890642938,
16.9612794518217));
#58207=CARTESIAN_POINT('Ctrl Pts',(28.82846267168,-0.181667965469806,16.9503816165397));
#58208=CARTESIAN_POINT('Ctrl Pts',(28.8217124648996,0.125982959524893,16.9285668665722));
#58209=CARTESIAN_POINT('Ctrl Pts',(28.8478169965895,0.276986540894418,16.9178595840512));
#58210=CARTESIAN_POINT('Ctrl Pts',(28.9558731518301,0.560261316962501,16.89777328523));
#58211=CARTESIAN_POINT('Ctrl Pts',(29.0365906245512,0.68988311408331,16.8888684608487));
#58212=CARTESIAN_POINT('Ctrl Pts',(29.2459337687842,0.914815990147539,16.868038474302));
#58213=CARTESIAN_POINT('Ctrl Pts',(29.3738173058995,1.00667300394252,16.8569287693601));
#58214=CARTESIAN_POINT('Ctrl Pts',(29.6525904034611,1.13269913332434,16.8353418646716));
#58215=CARTESIAN_POINT('Ctrl Pts',(29.7999172965718,1.16777128086699,16.825051424181));
#58216=CARTESIAN_POINT('Ctrl Pts',(30.1064062467105,1.18085135988937,16.8057669130232));
#58217=CARTESIAN_POINT('Ctrl Pts',(30.2627337376109,1.15617395633467,16.7956901530542));
#58218=CARTESIAN_POINT('Ctrl Pts',(30.5539694020395,1.04785975388265,16.7739659051239));
#58219=CARTESIAN_POINT('Ctrl Pts',(30.6863296582614,0.96635719030164,16.7629483992302));
#58220=CARTESIAN_POINT('Ctrl Pts',(30.9084297587183,0.760352988428474,16.7420061299136));
#58221=CARTESIAN_POINT('Ctrl Pts',(30.9973576321623,0.639251123876904,16.7328276824508));
#58222=CARTESIAN_POINT('Ctrl Pts',(31.1283061935881,0.363925745860841,16.7133050553655));
#58223=CARTESIAN_POINT('Ctrl Pts',(31.1665770325591,0.21117202309341,16.7024736747387));
#58224=CARTESIAN_POINT('Ctrl Pts',(31.1811107740607,-0.0965571386816749,
16.6806533771987));
#58225=CARTESIAN_POINT('Ctrl Pts',(31.1587010998539,-0.248535347285279,
16.6698769863224));
#58226=CARTESIAN_POINT('Ctrl Pts',(31.0576874952353,-0.534014859537023,
16.6496343552276));
#58227=CARTESIAN_POINT('Ctrl Pts',(30.9806443499075,-0.664990212129755,
16.6408093669374));
#58228=CARTESIAN_POINT('Ctrl Pts',(30.7774744062741,-0.895077677115282,
16.6201757128395));
#58229=CARTESIAN_POINT('Ctrl Pts',(30.6516599935628,-0.990433515302137,
16.6090690216144));
#58230=CARTESIAN_POINT('Ctrl Pts',(30.3754577665479,-1.12376244747141,16.5873810764564));
#58231=CARTESIAN_POINT('Ctrl Pts',(30.2286809422177,-1.16255586785604,16.5769924813814));
#58232=CARTESIAN_POINT('Ctrl Pts',(30.0523684587312,-1.17436628643519,16.5657468184328));
#58233=CARTESIAN_POINT('Ctrl Pts',(30.0261713894288,-1.17524047358084,16.5641071241452));
#58234=CARTESIAN_POINT('Ctrl Pts',(30.0000000000004,-1.17524047358085,16.5625));
#58235=CARTESIAN_POINT('Ctrl Pts',(30.,-1.17524047358085,16.5));
#58236=CARTESIAN_POINT('Ctrl Pts',(30.073608323754,-1.17524047358085,16.5045201159347));
#58237=CARTESIAN_POINT('Ctrl Pts',(30.1472072638744,-1.16832718018639,16.5092847577281));
#58238=CARTESIAN_POINT('Ctrl Pts',(30.369441082132,-1.12600740446215,16.5244320137475));
#58239=CARTESIAN_POINT('Ctrl Pts',(30.5120596783037,-1.06872004059094,16.5352209411127));
#58240=CARTESIAN_POINT('Ctrl Pts',(30.770540092832,-0.900978381413799,16.5570406907631));
#58241=CARTESIAN_POINT('Ctrl Pts',(30.8831588051698,-0.790914789141215,
16.5678585095693));
#58242=CARTESIAN_POINT('Ctrl Pts',(31.0548992370084,-0.539025681589464,
16.5873351001607));
#58243=CARTESIAN_POINT('Ctrl Pts',(31.1146464335618,-0.40117702528207,16.5965535505072));
#58244=CARTESIAN_POINT('Ctrl Pts',(31.1805926646682,-0.105443065986663,
16.6175232985392));
#58245=CARTESIAN_POINT('Ctrl Pts',(31.1842348048322,0.0500317177053629,
16.6285476227227));
#58246=CARTESIAN_POINT('Ctrl Pts',(31.1309192517252,0.355959076743607,16.650240158982));
#58247=CARTESIAN_POINT('Ctrl Pts',(31.0735350939833,0.503164977113694,16.6602491192277));
#58248=CARTESIAN_POINT('Ctrl Pts',(30.9079406905516,0.761174069707616,16.6795652728517));
#58249=CARTESIAN_POINT('Ctrl Pts',(30.8033709986449,0.870813111599809,16.6898737681392));
#58250=CARTESIAN_POINT('Ctrl Pts',(30.5539282192807,1.04817985026245,16.7114797826742));
#58251=CARTESIAN_POINT('Ctrl Pts',(30.4100715847777,1.1123704677318,16.7225894812308));
#58252=CARTESIAN_POINT('Ctrl Pts',(30.1103488398163,1.179778360742,16.7433846194973));
#58253=CARTESIAN_POINT('Ctrl Pts',(29.957856215253,1.1841771173115,16.7522711143702));
#58254=CARTESIAN_POINT('Ctrl Pts',(29.6587896018035,1.13483145500942,16.7723855875496));
#58255=CARTESIAN_POINT('Ctrl Pts',(29.5151366653971,1.08127741557342,16.7831056710399));
#58256=CARTESIAN_POINT('Ctrl Pts',(29.252747940286,0.920389087589127,16.80492244475));
#58257=CARTESIAN_POINT('Ctrl Pts',(29.137337166046,0.813224513877345,16.8158089365411));
#58258=CARTESIAN_POINT('Ctrl Pts',(28.9591466935998,0.565701034789473,16.8355268312788));
#58259=CARTESIAN_POINT('Ctrl Pts',(28.8958814901205,0.429333298679841,16.8445570602832));
#58260=CARTESIAN_POINT('Ctrl Pts',(28.8225467136217,0.135655218439199,16.8653810311245));
#58261=CARTESIAN_POINT('Ctrl Pts',(28.8149165149687,-0.0192736957647923,
16.8763666490815));
#58262=CARTESIAN_POINT('Ctrl Pts',(28.8600359901893,-0.325574492875678,
16.8980856648912));
#58263=CARTESIAN_POINT('Ctrl Pts',(28.9132427466147,-0.473736863683124,
16.908393840582));
#58264=CARTESIAN_POINT('Ctrl Pts',(29.0711075417097,-0.735375844223955,
16.9273640300312));
#58265=CARTESIAN_POINT('Ctrl Pts',(29.1722563389189,-0.847605887640186,
16.9375543168196));
#58266=CARTESIAN_POINT('Ctrl Pts',(29.4158032201734,-1.03154789820323,16.9590313959273));
#58267=CARTESIAN_POINT('Ctrl Pts',(29.5572939812199,-1.09972494823153,16.97013714563));
#58268=CARTESIAN_POINT('Ctrl Pts',(29.8035947514828,-1.1629117021743,16.9875021095456));
#58269=CARTESIAN_POINT('Ctrl Pts',(29.9016938547886,-1.17524047358087,16.9939632483014));
#58270=CARTESIAN_POINT('Ctrl Pts',(30.0000000000002,-1.17524047358085,17.));
#58271=CARTESIAN_POINT('Origin',(30.,-1.21864324187371E-14,15.78125));
#58272=CARTESIAN_POINT('',(30.,-1.17524047358085,17.5625));
#58273=CARTESIAN_POINT('',(30.0000000000003,-1.17524047358085,17.5));
#58274=CARTESIAN_POINT('',(30.,-1.17524047358085,15.78125));
#58275=CARTESIAN_POINT('Ctrl Pts',(29.9999999999999,-1.17524047358085,17.5625));
#58276=CARTESIAN_POINT('Ctrl Pts',(29.9853039952848,-1.17524047358085,17.5615975525362));
#58277=CARTESIAN_POINT('Ctrl Pts',(29.9705988101993,-1.17496482223763,17.560684768457));
#58278=CARTESIAN_POINT('Ctrl Pts',(29.8000675583885,-1.16856010727206,17.5499857698916));
#58279=CARTESIAN_POINT('Ctrl Pts',(29.6469974366404,-1.13175546252589,17.53928122759));
#58280=CARTESIAN_POINT('Ctrl Pts',(29.3669883306193,-1.00191414640604,17.51748315987));
#58281=CARTESIAN_POINT('Ctrl Pts',(29.2422159979844,-0.911212372037981,
17.5066054643129));
#58282=CARTESIAN_POINT('Ctrl Pts',(29.0365009193432,-0.689398438610156,
17.4861088470066));
#58283=CARTESIAN_POINT('Ctrl Pts',(28.9566358845376,-0.561238966410083,
17.477296037423));
#58284=CARTESIAN_POINT('Ctrl Pts',(28.8466374529962,-0.274946499836391,
17.4569957617908));
#58285=CARTESIAN_POINT('Ctrl Pts',(28.8202715815142,-0.118602529031394,
17.4459098057446));
#58286=CARTESIAN_POINT('Ctrl Pts',(28.8303001790337,0.189193535952347,17.4240847642671));
#58287=CARTESIAN_POINT('Ctrl Pts',(28.8642598713376,0.337792935402822,17.413547956213));
#58288=CARTESIAN_POINT('Ctrl Pts',(28.9875332190235,0.616132121834573,17.3938116275857));
#58289=CARTESIAN_POINT('Ctrl Pts',(29.0764632180064,0.742831294355827,17.3845427667776));
#58290=CARTESIAN_POINT('Ctrl Pts',(29.2992557500629,0.956131495581886,17.3632993064049));
#58291=CARTESIAN_POINT('Ctrl Pts',(29.431365525465,1.04013508414132,17.3522085112739));
#58292=CARTESIAN_POINT('Ctrl Pts',(29.7152659077079,1.14996876403328,17.3308808348058));
#58293=CARTESIAN_POINT('Ctrl Pts',(29.8634965281812,1.17678287245723,17.3209370444755));
#58294=CARTESIAN_POINT('Ctrl Pts',(30.1685869462377,1.17348866615416,17.3020853596773));
#58295=CARTESIAN_POINT('Ctrl Pts',(30.3225567032231,1.14080144678595,17.291471550985));
#58296=CARTESIAN_POINT('Ctrl Pts',(30.6062809135034,1.01837161133764,17.269708112041));
#58297=CARTESIAN_POINT('Ctrl Pts',(30.7337302229979,0.930754504232001,17.2587753925441));
#58298=CARTESIAN_POINT('Ctrl Pts',(30.9451039338725,0.714326579760782,17.2381222459404));
#58299=CARTESIAN_POINT('Ctrl Pts',(31.0280898505948,0.588650269560749,17.2292397036887));
#58300=CARTESIAN_POINT('Ctrl Pts',(31.1457356989614,0.305390771140385,17.209154488167));
#58301=CARTESIAN_POINT('Ctrl Pts',(31.1762844162632,0.149369866697047,17.1980914399405));
#58302=CARTESIAN_POINT('Ctrl Pts',(31.1741828829317,-0.159374372954329,
17.1761991657924));
#58303=CARTESIAN_POINT('Ctrl Pts',(31.1439148549186,-0.309160960295119,
17.1655781772438));
#58304=CARTESIAN_POINT('Ctrl Pts',(31.0278391895685,-0.589863984020037,
17.1456742348851));
#58305=CARTESIAN_POINT('Ctrl Pts',(30.9428415818715,-0.717947604052165,
17.1366104494432));
#58306=CARTESIAN_POINT('Ctrl Pts',(30.7264277284841,-0.936836489561928,
17.1155605491468));
#58307=CARTESIAN_POINT('Ctrl Pts',(30.5962729133073,-1.02460346942682,17.10445637729));
#58308=CARTESIAN_POINT('Ctrl Pts',(30.3147671476396,-1.1421454095557,17.0830024620243));
#58309=CARTESIAN_POINT('Ctrl Pts',(30.1669216238945,-1.17291749944691,17.0728326267459));
#58310=CARTESIAN_POINT('Ctrl Pts',(30.0114948569556,-1.17519832475422,17.06320736676));
#58311=CARTESIAN_POINT('Ctrl Pts',(30.0057465951805,-1.17524047358085,17.0628528850424));
#58312=CARTESIAN_POINT('Ctrl Pts',(30.,-1.17524047358085,17.0625));
#58313=CARTESIAN_POINT('Ctrl Pts',(30.0000000000002,-1.17524047358085,17.));
#58314=CARTESIAN_POINT('Ctrl Pts',(30.0532026451947,-1.17524047358084,17.0032670506819));
#58315=CARTESIAN_POINT('Ctrl Pts',(30.1064500803375,-1.17162840402792,17.0066649131742));
#58316=CARTESIAN_POINT('Ctrl Pts',(30.3094843531048,-1.14383638948677,17.0201181063427));
#58317=CARTESIAN_POINT('Ctrl Pts',(30.4541770343026,-1.0944632219883,17.0307538106078));
#58318=CARTESIAN_POINT('Ctrl Pts',(30.7220117324143,-0.94057404805184,17.0526568626846));
#58319=CARTESIAN_POINT('Ctrl Pts',(30.8414109395085,-0.835479490322757,
17.0637148850572));
#58320=CARTESIAN_POINT('Ctrl Pts',(31.0267110546809,-0.591037021798696,
17.0837601330781));
#58321=CARTESIAN_POINT('Ctrl Pts',(31.0933788874677,-0.456058910657645,
17.0926620146465));
#58322=CARTESIAN_POINT('Ctrl Pts',(31.1737387540124,-0.16438811954927,17.1133436536858));
#58323=CARTESIAN_POINT('Ctrl Pts',(31.1851490819135,-0.0100732318962758,
17.1242857325711));
#58324=CARTESIAN_POINT('Ctrl Pts',(31.1477867853133,0.296739304676255,17.1460410345334));
#58325=CARTESIAN_POINT('Ctrl Pts',(31.0983725298423,0.446176311422578,17.156637235205));
#58326=CARTESIAN_POINT('Ctrl Pts',(30.9473434585081,0.711342976495719,17.1754395336164));
#58327=CARTESIAN_POINT('Ctrl Pts',(30.8493881217234,0.825870653120103,17.1854545855523));
#58328=CARTESIAN_POINT('Ctrl Pts',(30.6112318646727,1.01569990967513,17.2068093638384));
#58329=CARTESIAN_POINT('Ctrl Pts',(30.4719800604887,1.0874234537732,17.2179033608764));
#58330=CARTESIAN_POINT('Ctrl Pts',(30.1755334231398,1.17210985582506,17.2391099087106));
#58331=CARTESIAN_POINT('Ctrl Pts',(30.0214941231326,1.18498177307235,17.2483347304275));
#58332=CARTESIAN_POINT('Ctrl Pts',(29.7191034448427,1.1511421779865,17.2681035786673));
#58333=CARTESIAN_POINT('Ctrl Pts',(29.5735822533488,1.10552321949792,17.2786570590835));
#58334=CARTESIAN_POINT('Ctrl Pts',(29.3025973986068,0.958895356196027,17.3004961143537));
#58335=CARTESIAN_POINT('Ctrl Pts',(29.1808306521913,0.85722095928387,17.3115782643265));
#58336=CARTESIAN_POINT('Ctrl Pts',(28.9891285746956,0.617827320312939,17.3318376420863));
#58337=CARTESIAN_POINT('Ctrl Pts',(28.918785924397,0.484304768960115,17.3406591721831));
#58338=CARTESIAN_POINT('Ctrl Pts',(28.8309775509286,0.194817478373176,17.361185984716));
#58339=CARTESIAN_POINT('Ctrl Pts',(28.8155773691905,0.0412543792472424,
17.3720747561758));
#58340=CARTESIAN_POINT('Ctrl Pts',(28.8447173912596,-0.266085346871024,
17.3938674398171));
#58341=CARTESIAN_POINT('Ctrl Pts',(28.8901486797617,-0.416814366578493,
17.4045552538642));
#58342=CARTESIAN_POINT('Ctrl Pts',(29.0339735284972,-0.685700945089528,
17.423621321941));
#58343=CARTESIAN_POINT('Ctrl Pts',(29.1286271803726,-0.802582950507819,
17.4332789203108));
#58344=CARTESIAN_POINT('Ctrl Pts',(29.3609543925255,-0.998368963070605,
17.45448693977));
#58345=CARTESIAN_POINT('Ctrl Pts',(29.4977729352126,-1.07372697749091,17.4655603714348));
#58346=CARTESIAN_POINT('Ctrl Pts',(29.7602131749374,-1.15682002764215,17.484622175217));
#58347=CARTESIAN_POINT('Ctrl Pts',(29.879837116137,-1.1752404735809,17.4926210768238));
#58348=CARTESIAN_POINT('Ctrl Pts',(30.0000000000005,-1.17524047358085,17.5));
#58349=CARTESIAN_POINT('Origin',(30.,-1.21864324187371E-14,15.78125));
#58350=CARTESIAN_POINT('',(29.9999999999998,-1.17524047358085,18.0625));
#58351=CARTESIAN_POINT('',(30.,-1.17524047358085,18.));
#58352=CARTESIAN_POINT('',(30.,-1.17524047358085,15.78125));
#58353=CARTESIAN_POINT('Ctrl Pts',(29.9999999999995,-1.17524047358085,18.0625));
#58354=CARTESIAN_POINT('Ctrl Pts',(29.9645254254169,-1.17524047358085,18.0603215888955));
#58355=CARTESIAN_POINT('Ctrl Pts',(29.929015100466,-1.17363438891304,18.0580840407407));
#58356=CARTESIAN_POINT('Ctrl Pts',(29.7382382629168,-1.15628718990462,18.0457538558988));
#58357=CARTESIAN_POINT('Ctrl Pts',(29.5872914572777,-1.11138228831714,18.0348925171245));
#58358=CARTESIAN_POINT('Ctrl Pts',(29.315235711072,-0.96715790012321,18.0130729130751));
#58359=CARTESIAN_POINT('Ctrl Pts',(29.1959940490486,-0.870565282945587,
18.0023259907432));
#58360=CARTESIAN_POINT('Ctrl Pts',(29.0016396885941,-0.638155310236294,
17.9821513395236));
#58361=CARTESIAN_POINT('Ctrl Pts',(28.9280461950896,-0.504858426874225,
17.9732982357813));
#58362=CARTESIAN_POINT('Ctrl Pts',(28.8336569152641,-0.212647772939916,
17.9525783164326));
#58363=CARTESIAN_POINT('Ctrl Pts',(28.8157570812338,-0.0559802507924535,
17.9414694181781));
#58364=CARTESIAN_POINT('Ctrl Pts',(28.841716723376,0.249283949869151,17.9198239048041));
#58365=CARTESIAN_POINT('Ctrl Pts',(28.8830393993721,0.395199804389445,17.9094773801424));
#58366=CARTESIAN_POINT('Ctrl Pts',(29.0209639808548,0.668562290928518,17.8900939367334));
#58367=CARTESIAN_POINT('Ctrl Pts',(29.1181759703235,0.792402282110926,17.8802238069267));
#58368=CARTESIAN_POINT('Ctrl Pts',(29.3540263292146,0.993822233016871,17.8585996950535));
#58369=CARTESIAN_POINT('Ctrl Pts',(29.4898462594122,1.06991069869815,17.8475616886318));
#58370=CARTESIAN_POINT('Ctrl Pts',(29.7781387158762,1.16368326761588,17.8265337315072));
#58371=CARTESIAN_POINT('Ctrl Pts',(29.9272121099849,1.18239624377936,17.817223433802));
#58372=CARTESIAN_POINT('Ctrl Pts',(30.231427568808,1.16273575019751,17.7978452321702));
#58373=CARTESIAN_POINT('Ctrl Pts',(30.3834744853667,1.1218012564522,17.7870571039388));
#58374=CARTESIAN_POINT('Ctrl Pts',(30.6595367886018,0.984593855649311,17.7652402449678));
#58375=CARTESIAN_POINT('Ctrl Pts',(30.78153371397,0.890859052478792,17.7544254485094));
#58376=CARTESIAN_POINT('Ctrl Pts',(30.9814968973686,0.663646825098318,17.7340906520159));
#58377=CARTESIAN_POINT('Ctrl Pts',(31.0581916579204,0.532910080900297,17.7252873077101));
#58378=CARTESIAN_POINT('Ctrl Pts',(31.1603311881744,0.243593094566313,17.7047725710215));
#58379=CARTESIAN_POINT('Ctrl Pts',(31.1824208985569,0.0870303935487086,
17.6936711053685));
#58380=CARTESIAN_POINT('Ctrl Pts',(31.1643265939555,-0.219589452433675,
17.6719294666093));
#58381=CARTESIAN_POINT('Ctrl Pts',(31.126629625228,-0.366880394031282,17.6614854379963));
#58382=CARTESIAN_POINT('Ctrl Pts',(30.9959732548856,-0.642739672382233,
17.6419249533869));
#58383=CARTESIAN_POINT('Ctrl Pts',(30.9029171297163,-0.76800751067264,17.6323839709445));
#58384=CARTESIAN_POINT('Ctrl Pts',(30.6735549835348,-0.97540763183831,17.6109462657373));
#58385=CARTESIAN_POINT('Ctrl Pts',(30.5395284406378,-1.05546393695081,17.5998777123224));
#58386=CARTESIAN_POINT('Ctrl Pts',(30.2672665806154,-1.15230702152505,17.5797252955804));
#58387=CARTESIAN_POINT('Ctrl Pts',(30.1340643685791,-1.17524047358085,17.5707325810151));
#58388=CARTESIAN_POINT('Ctrl Pts',(29.9999999999999,-1.17524047358085,17.5625));
#58389=CARTESIAN_POINT('Ctrl Pts',(30.0000000000005,-1.17524047358085,17.5));
#58390=CARTESIAN_POINT('Ctrl Pts',(30.033668671514,-1.17524047358084,17.5020675147979));
#58391=CARTESIAN_POINT('Ctrl Pts',(30.0673733741507,-1.17379373295066,17.504188534545));
#58392=CARTESIAN_POINT('Ctrl Pts',(30.2512194694897,-1.15793171152857,17.5160404635345));
#58393=CARTESIAN_POINT('Ctrl Pts',(30.3974945854731,-1.11619705184184,17.5265025277916));
#58394=CARTESIAN_POINT('Ctrl Pts',(30.6715286389123,-0.977122112696594,
17.5482610478741));
#58395=CARTESIAN_POINT('Ctrl Pts',(30.7956391457863,-0.8790277241657,17.559360198049));
#58396=CARTESIAN_POINT('Ctrl Pts',(30.9938921656194,-0.644908297614295,
17.579834863399));
#58397=CARTESIAN_POINT('Ctrl Pts',(31.0680432549382,-0.51284781086492,17.5886352571811));
#58398=CARTESIAN_POINT('Ctrl Pts',(31.1634155774875,-0.225635628704456,
17.6090007475224));
#58399=CARTESIAN_POINT('Ctrl Pts',(31.1828424433655,-0.0729412614644995,
17.6198279193986));
#58400=CARTESIAN_POINT('Ctrl Pts',(31.1620678214981,0.234707081573543,17.6416424862861));
#58401=CARTESIAN_POINT('Ctrl Pts',(31.120724241081,0.386638085314584,17.6524155299848));
#58402=CARTESIAN_POINT('Ctrl Pts',(30.9842587758127,0.659238100700609,17.6717449084903));
#58403=CARTESIAN_POINT('Ctrl Pts',(30.8929036275603,0.778529076192667,17.6811039637465));
#58404=CARTESIAN_POINT('Ctrl Pts',(30.6664518626416,0.98022024209091,17.7021605454119));
#58405=CARTESIAN_POINT('Ctrl Pts',(30.5321662358965,1.05914504613978,17.7132048926221));
#58406=CARTESIAN_POINT('Ctrl Pts',(30.2394356343315,1.16107865610412,17.7347947253164));
#58407=CARTESIAN_POINT('Ctrl Pts',(30.0837395746803,1.18253750639866,17.7445990404306));
#58408=CARTESIAN_POINT('Ctrl Pts',(29.7783085058998,1.16389753061854,17.7640157086725));
#58409=CARTESIAN_POINT('Ctrl Pts',(29.6313883618284,1.12601470121935,17.7743808208261));
#58410=CARTESIAN_POINT('Ctrl Pts',(29.3545393068819,0.994469365010162,17.7960452510406));
#58411=CARTESIAN_POINT('Ctrl Pts',(29.2282096618696,0.899966183720928,17.8071533516094));
#58412=CARTESIAN_POINT('Ctrl Pts',(29.0235241701317,0.671134004766118,17.8278355674102));
#58413=CARTESIAN_POINT('Ctrl Pts',(28.9455840780504,0.540492245953914,17.8366750601186));
#58414=CARTESIAN_POINT('Ctrl Pts',(28.8428376707835,0.255550540540784,17.8568795566889));
#58415=CARTESIAN_POINT('Ctrl Pts',(28.819515816648,0.103803872119581,17.8676395296357));
#58416=CARTESIAN_POINT('Ctrl Pts',(28.8321334408652,-0.203924479248023,
17.8894597697118));
#58417=CARTESIAN_POINT('Ctrl Pts',(28.8694569005926,-0.356918085677502,
17.9003081598831));
#58418=CARTESIAN_POINT('Ctrl Pts',(28.9987062002081,-0.633072693900888,
17.9198895855878));
#58419=CARTESIAN_POINT('Ctrl Pts',(29.0868937988439,-0.754733453808526,
17.9290197269592));
#58420=CARTESIAN_POINT('Ctrl Pts',(29.3076626510103,-0.962047131353844,
17.9499266732212));
#58421=CARTESIAN_POINT('Ctrl Pts',(29.439425880769,-1.04432722335896,17.9609350833968));
#58422=CARTESIAN_POINT('Ctrl Pts',(29.7165797609128,-1.14942800619046,17.981680673977));
#58423=CARTESIAN_POINT('Ctrl Pts',(29.857771536572,-1.17524047358086,17.9912660809114));
#58424=CARTESIAN_POINT('Ctrl Pts',(30.0000000000001,-1.17524047358085,18.));
#58425=CARTESIAN_POINT('Origin',(30.,-1.21864324187371E-14,15.78125));
#58426=CARTESIAN_POINT('',(29.9999999999999,-1.17524047358085,18.5625));
#58427=CARTESIAN_POINT('',(30.,-1.17524047358085,18.5));
#58428=CARTESIAN_POINT('',(30.,-1.17524047358085,15.78125));
#58429=CARTESIAN_POINT('Ctrl Pts',(29.9999999999998,-1.17524047358085,18.5625));
#58430=CARTESIAN_POINT('Ctrl Pts',(29.9448799883238,-1.17524047358085,18.5591152083026));
#58431=CARTESIAN_POINT('Ctrl Pts',(29.8897199177939,-1.17136342891428,18.5555905009623));
#58432=CARTESIAN_POINT('Ctrl Pts',(29.6792216999803,-1.14149919812993,18.5416054964814));
#58433=CARTESIAN_POINT('Ctrl Pts',(29.5295600411529,-1.08838822549331,18.5305321396985));
#58434=CARTESIAN_POINT('Ctrl Pts',(29.2651715824486,-0.929562358041593,
18.5086656889335));
#58435=CARTESIAN_POINT('Ctrl Pts',(29.1517563578462,-0.827380506823195,
18.4980783953365));
#58436=CARTESIAN_POINT('Ctrl Pts',(28.9690035888602,-0.584433789122884,
18.4782426038757));
#58437=CARTESIAN_POINT('Ctrl Pts',(28.9018681826973,-0.445680079983302,
18.4691020486872));
#58438=CARTESIAN_POINT('Ctrl Pts',(28.8237798560613,-0.147691887525462,
18.4479724586759));
#58439=CARTESIAN_POINT('Ctrl Pts',(28.8145788645707,0.00884554058040183,
18.4368727850612));
#58440=CARTESIAN_POINT('Ctrl Pts',(28.8567482751501,0.310649796974269,18.4154726075955));
#58441=CARTESIAN_POINT('Ctrl Pts',(28.9054833559201,0.453415390787842,18.4053494599629));
#58442=CARTESIAN_POINT('Ctrl Pts',(29.0569965845258,0.718468314308288,18.3865552266777));
#58443=CARTESIAN_POINT('Ctrl Pts',(29.1604683184012,0.83707730034545,18.3760428358642));
#58444=CARTESIAN_POINT('Ctrl Pts',(29.4058248734932,1.0255154952049,18.3542952223602));
#58445=CARTESIAN_POINT('Ctrl Pts',(29.544631443668,1.0942445155017,18.3433347331662));
#58446=CARTESIAN_POINT('Ctrl Pts',(29.8366929775619,1.17335763361873,18.3225950580774));
#58447=CARTESIAN_POINT('Ctrl Pts',(29.986714530993,1.18458952273488,18.3136472884771));
#58448=CARTESIAN_POINT('Ctrl Pts',(30.2898186404183,1.14957783224746,18.2937930749288));
#58449=CARTESIAN_POINT('Ctrl Pts',(30.4396462258347,1.10100720458506,18.2828705011767));
#58450=CARTESIAN_POINT('Ctrl Pts',(30.7078144176317,0.95036138884417,18.2610619591969));
#58451=CARTESIAN_POINT('Ctrl Pts',(30.8244348872713,0.851181456147988,18.250384268188));
#58452=CARTESIAN_POINT('Ctrl Pts',(31.0135314789776,0.613960284599869,18.2303619093383));
#58453=CARTESIAN_POINT('Ctrl Pts',(31.0842069749077,0.478217809229905,18.2214092168781));
#58454=CARTESIAN_POINT('Ctrl Pts',(31.1712537448649,0.183351777827692,18.2005010114207));
#58455=CARTESIAN_POINT('Ctrl Pts',(31.1852144107931,0.026684835425868,18.1893921542744));
#58456=CARTESIAN_POINT('Ctrl Pts',(31.151894218573,-0.277120859310672,18.1678500598715));
#58457=CARTESIAN_POINT('Ctrl Pts',(31.1071955868466,-0.421659698179358,
18.1576011759113));
#58458=CARTESIAN_POINT('Ctrl Pts',(30.9623980704004,-0.692609521716023,
18.1383888083414));
#58459=CARTESIAN_POINT('Ctrl Pts',(30.8611688824271,-0.815074867780112,
18.1281515944925));
#58460=CARTESIAN_POINT('Ctrl Pts',(30.6191698348665,-1.010677278137,18.1063561595037));
#58461=CARTESIAN_POINT('Ctrl Pts',(30.481744547401,-1.08294295672688,18.0953551039148));
#58462=CARTESIAN_POINT('Ctrl Pts',(30.2255864017037,-1.15894806928573,18.0769303627887));
#58463=CARTESIAN_POINT('Ctrl Pts',(30.1130100641695,-1.17524047358085,18.0694396851576));
#58464=CARTESIAN_POINT('Ctrl Pts',(29.9999999999995,-1.17524047358085,18.0625));
#58465=CARTESIAN_POINT('Ctrl Pts',(30.0000000000001,-1.17524047358085,18.));
#58466=CARTESIAN_POINT('Ctrl Pts',(30.0145244311397,-1.17524047358085,18.0008919115297));
#58467=CARTESIAN_POINT('Ctrl Pts',(30.0290585224951,-1.1749712210064,18.0017939622806));
#58468=CARTESIAN_POINT('Ctrl Pts',(30.1935181174434,-1.16886648233729,18.0121094792412));
#58469=CARTESIAN_POINT('Ctrl Pts',(30.3409577753235,-1.13464684718278,18.022376619604));
#58470=CARTESIAN_POINT('Ctrl Pts',(30.6202928748417,-1.01029888563142,18.0439385382044));
#58471=CARTESIAN_POINT('Ctrl Pts',(30.7486368752819,-0.919248747112441,
18.055047912384));
#58472=CARTESIAN_POINT('Ctrl Pts',(30.9593869332128,-0.695506306327382,
18.0759220888488));
#58473=CARTESIAN_POINT('Ctrl Pts',(31.0409497614259,-0.566191331080132,
18.084852802908));
#58474=CARTESIAN_POINT('Ctrl Pts',(31.1506054030915,-0.283424289026694,
18.1049030995926));
#58475=CARTESIAN_POINT('Ctrl Pts',(31.1775442736485,-0.132654402671248,
18.1155938113905));
#58476=CARTESIAN_POINT('Ctrl Pts',(31.1725598607287,0.174951078257229,18.1374053390341));
#58477=CARTESIAN_POINT('Ctrl Pts',(31.1390289434739,0.328840847644919,18.148317273857));
#58478=CARTESIAN_POINT('Ctrl Pts',(31.0165781905916,0.608264397522364,18.1681304919571));
#58479=CARTESIAN_POINT('Ctrl Pts',(30.9313199722933,0.732167484063905,18.1771012136858));
#58480=CARTESIAN_POINT('Ctrl Pts',(30.7158345492886,0.944633593585631,18.1978663898215));
#58481=CARTESIAN_POINT('Ctrl Pts',(30.5864762504196,1.02994768568734,18.208834685427));
#58482=CARTESIAN_POINT('Ctrl Pts',(30.3000115977578,1.14695518635867,18.2305741665317));
#58483=CARTESIAN_POINT('Ctrl Pts',(30.1454149851266,1.17656763909288,18.2410233510493));
#58484=CARTESIAN_POINT('Ctrl Pts',(29.8400425266379,1.17387642244061,18.2598709770579));
#58485=CARTESIAN_POINT('Ctrl Pts',(29.6921041520777,1.14400535739554,18.2700145693908));
#58486=CARTESIAN_POINT('Ctrl Pts',(29.4100579886469,1.02824734385133,18.2914384223622));
#58487=CARTESIAN_POINT('Ctrl Pts',(29.2794434337127,0.941343746808855,18.3025402156205));
#58488=CARTESIAN_POINT('Ctrl Pts',(29.061555804029,0.723734320476339,18.3236352554819));
#58489=CARTESIAN_POINT('Ctrl Pts',(28.9756558249342,0.595970538008072,18.3327412345668));
#58490=CARTESIAN_POINT('Ctrl Pts',(28.8579142725366,0.315809924655313,18.3526067159761));
#58491=CARTESIAN_POINT('Ctrl Pts',(28.8267878271973,0.166290213657428,18.3632087809973));
#58492=CARTESIAN_POINT('Ctrl Pts',(28.8228465258246,-0.142252171918218,
18.3850867421828));
#58493=CARTESIAN_POINT('Ctrl Pts',(28.8524261916584,-0.298357527348321,
18.3961557786154));
#58494=CARTESIAN_POINT('Ctrl Pts',(28.9683032793772,-0.582326286319503,
18.4162912860112));
#58495=CARTESIAN_POINT('Ctrl Pts',(29.0505638845767,-0.708574806470949,
18.4251522948912));
#58496=CARTESIAN_POINT('Ctrl Pts',(29.2606233813178,-0.926260402003281,
18.4457693278011));
#58497=CARTESIAN_POINT('Ctrl Pts',(29.3874559625716,-1.01460273580079,18.4566898874478));
#58498=CARTESIAN_POINT('Ctrl Pts',(29.670332667393,-1.13876808411125,18.4784628134696));
#58499=CARTESIAN_POINT('Ctrl Pts',(29.8241031351402,-1.17241612945781,18.4890984491449));
#58500=CARTESIAN_POINT('Ctrl Pts',(29.9866645216768,-1.17518374723239,18.4991790881359));
#58501=CARTESIAN_POINT('Ctrl Pts',(29.9933333092278,-1.17524047358085,18.4995906140276));
#58502=CARTESIAN_POINT('Ctrl Pts',(30.,-1.17524047358085,18.5));
#58503=CARTESIAN_POINT('Origin',(30.,-1.21864324187371E-14,15.78125));
#58504=CARTESIAN_POINT('',(30.,-1.17524047358085,19.0625));
#58505=CARTESIAN_POINT('',(29.9999999999998,-1.17524047358085,18.9999999999999));
#58506=CARTESIAN_POINT('',(30.,-1.17524047358085,15.78125));
#58507=CARTESIAN_POINT('Ctrl Pts',(30.,-1.17524047358085,19.0625));
#58508=CARTESIAN_POINT('Ctrl Pts',(29.9235115354988,-1.17524047358085,19.0578030213218));
#58509=CARTESIAN_POINT('Ctrl Pts',(29.84704716558,-1.16777574293408,19.0528428696387));
#58510=CARTESIAN_POINT('Ctrl Pts',(29.6182505756017,-1.12246086107485,19.0371864213689));
#58511=CARTESIAN_POINT('Ctrl Pts',(29.4724485773796,-1.06175746863862,19.0260808977107));
#58512=CARTESIAN_POINT('Ctrl Pts',(29.2180805672544,-0.890185564352666,
19.0043778847458));
#58513=CARTESIAN_POINT('Ctrl Pts',(29.1106251205818,-0.782854361416016,
18.9939740034863));
#58514=CARTESIAN_POINT('Ctrl Pts',(28.9394765622835,-0.529653947083613,
18.9744872677464));
#58515=CARTESIAN_POINT('Ctrl Pts',(28.8789010658566,-0.385229961133875,
18.9648156834562));
#58516=CARTESIAN_POINT('Ctrl Pts',(28.8174805423046,-0.0817855742350542,
18.9432992084794));
#58517=CARTESIAN_POINT('Ctrl Pts',(28.8169771571136,0.0741472763924911,
18.9322424039265));
#58518=CARTESIAN_POINT('Ctrl Pts',(28.8752567923883,0.371953492557534,18.9111257173945));
#58519=CARTESIAN_POINT('Ctrl Pts',(28.9314131886074,0.511361040736907,18.9016564371649));
#58520=CARTESIAN_POINT('Ctrl Pts',(29.0965385184593,0.767636822695621,18.8824305405978));
#58521=CARTESIAN_POINT('Ctrl Pts',(29.2062331582591,0.880579083863968,18.8716902227143));
#58522=CARTESIAN_POINT('Ctrl Pts',(29.4605419802015,1.05521085002794,18.8498823608196));
#58523=CARTESIAN_POINT('Ctrl Pts',(29.6020069692685,1.11628678080371,18.8390299549287));
#58524=CARTESIAN_POINT('Ctrl Pts',(29.8977163387384,1.18033932535056,18.8186002283572));
#58525=CARTESIAN_POINT('Ctrl Pts',(30.0489012110254,1.18375239923791,18.8097988699583));
#58526=CARTESIAN_POINT('Ctrl Pts',(30.351304458352,1.13241772416719,18.7894089839185));
#58527=CARTESIAN_POINT('Ctrl Pts',(30.4990888608278,1.07549105419273,18.7783156243515));
#58528=CARTESIAN_POINT('Ctrl Pts',(30.7585582244441,0.910237971254531,18.7565233749656));
#58529=CARTESIAN_POINT('Ctrl Pts',(30.869032001546,0.80544751578808,18.7460242240482));
#58530=CARTESIAN_POINT('Ctrl Pts',(31.0460310070461,0.557381504027199,18.7263602597134));
#58531=CARTESIAN_POINT('Ctrl Pts',(31.1099298338315,0.41584148204013,18.7169862690792));
#58532=CARTESIAN_POINT('Ctrl Pts',(31.1797989523814,0.115104609901925,18.6956617771348));
#58533=CARTESIAN_POINT('Ctrl Pts',(31.1846835245906,-0.0411926090939851,
18.6845791361414));
#58534=CARTESIAN_POINT('Ctrl Pts',(31.134503841219,-0.341119161052378,18.6633121019541));
#58535=CARTESIAN_POINT('Ctrl Pts',(31.082082323541,-0.482198917475646,18.6535190714213));
#58536=CARTESIAN_POINT('Ctrl Pts',(30.9238582069445,-0.74295817680152,18.6345580062792));
#58537=CARTESIAN_POINT('Ctrl Pts',(30.8172746962663,-0.85879990158245,18.6239059387776));
#58538=CARTESIAN_POINT('Ctrl Pts',(30.5674863902569,-1.04046451233651,18.6021263306283));
#58539=CARTESIAN_POINT('Ctrl Pts',(30.4273223446806,-1.10544579712631,18.5912153532567));
#58540=CARTESIAN_POINT('Ctrl Pts',(30.1872213612661,-1.164041447155,18.5743938756203));
#58541=CARTESIAN_POINT('Ctrl Pts',(30.0936931422672,-1.17524047358085,18.5682534779185));
#58542=CARTESIAN_POINT('Ctrl Pts',(29.9999999999998,-1.17524047358085,18.5625));
#58543=CARTESIAN_POINT('Ctrl Pts',(30.,-1.17524047358085,18.5));
#58544=CARTESIAN_POINT('Ctrl Pts',(30.1423690472132,-1.17524047358085,18.5087425520117));
#58545=CARTESIAN_POINT('Ctrl Pts',(30.2836710124158,-1.14937338085773,18.5183366621019));
#58546=CARTESIAN_POINT('Ctrl Pts',(30.561858730089,-1.04379601878612,18.5391626347549));
#58547=CARTESIAN_POINT('Ctrl Pts',(30.6944274791866,-0.96071277520592,18.550248984724));
#58548=CARTESIAN_POINT('Ctrl Pts',(30.9187624839086,-0.748784365111015,
18.5715385296331));
#58549=CARTESIAN_POINT('Ctrl Pts',(31.0086541273172,-0.622420436396325,
18.5808657390843));
#58550=CARTESIAN_POINT('Ctrl Pts',(31.1336634286392,-0.344659292163419,
18.6005610801994));
#58551=CARTESIAN_POINT('Ctrl Pts',(31.1685065373813,-0.196359387070609,
18.6110766518651));
#58552=CARTESIAN_POINT('Ctrl Pts',(31.1804379609257,0.111178530247992,18.6328833887437));
#58553=CARTESIAN_POINT('Ctrl Pts',(31.1550790566304,0.267584160665563,18.6439737169172));
#58554=CARTESIAN_POINT('Ctrl Pts',(31.0469271232095,0.554595748580105,18.6643249836272));
#58555=CARTESIAN_POINT('Ctrl Pts',(30.9678100781097,0.68335841703765,18.6731299773448));
#58556=CARTESIAN_POINT('Ctrl Pts',(30.763452167876,0.90645295543942,18.6935886563282));
#58557=CARTESIAN_POINT('Ctrl Pts',(30.6393299618342,0.997879761179756,18.7044521341951));
#58558=CARTESIAN_POINT('Ctrl Pts',(30.3602369836734,1.12947461105548,18.7262561139589));
#58559=CARTESIAN_POINT('Ctrl Pts',(30.207398548302,1.16725893034935,18.7369811620628));
#58560=CARTESIAN_POINT('Ctrl Pts',(29.9028111520737,1.18064726329168,18.7561598319717));
#58561=CARTESIAN_POINT('Ctrl Pts',(29.7540809815473,1.15884794274813,18.7656824913455));
#58562=CARTESIAN_POINT('Ctrl Pts',(29.4674235177593,1.05897426017317,18.7868263546523));
#58563=CARTESIAN_POINT('Ctrl Pts',(29.332959967187,0.979858413005439,18.7978884009434));
#58564=CARTESIAN_POINT('Ctrl Pts',(29.1020498086111,0.773870883761844,18.8193710843283));
#58565=CARTESIAN_POINT('Ctrl Pts',(29.0080096312967,0.648942084974305,18.8289851559772));
#58566=CARTESIAN_POINT('Ctrl Pts',(28.8756172989166,0.373674108747255,18.8485037128466));
#58567=CARTESIAN_POINT('Ctrl Pts',(28.8370493704244,0.226703861544607,18.85892500183));
#58568=CARTESIAN_POINT('Ctrl Pts',(28.8170693542027,-0.0796098764074361,
18.8806449352421));
#58569=CARTESIAN_POINT('Ctrl Pts',(28.838156352639,-0.236207536581086,18.8917488797605));
#58570=CARTESIAN_POINT('Ctrl Pts',(28.9384458248014,-0.526222673597261,
18.9123131205504));
#58571=CARTESIAN_POINT('Ctrl Pts',(29.0143989785152,-0.657569956199922,
18.921123179589));
#58572=CARTESIAN_POINT('Ctrl Pts',(29.2130173163762,-0.886033452067211,
18.9414197543903));
#58573=CARTESIAN_POINT('Ctrl Pts',(29.3343580168877,-0.980462303689547,
18.9522188602181));
#58574=CARTESIAN_POINT('Ctrl Pts',(29.609473809437,-1.11936682716347,18.9740377655105));
#58575=CARTESIAN_POINT('Ctrl Pts',(29.7612660994758,-1.16125829944545,18.9848441861849));
#58576=CARTESIAN_POINT('Ctrl Pts',(29.9445511530895,-1.1742603871282,18.9965602675684));
#58577=CARTESIAN_POINT('Ctrl Pts',(29.9722886221142,-1.17524047358085,18.998298308746));
#58578=CARTESIAN_POINT('Ctrl Pts',(29.9999999999996,-1.17524047358085,18.9999999999999));
#58579=CARTESIAN_POINT('Origin',(30.,-1.21864324187371E-14,15.78125));
#58580=CARTESIAN_POINT('',(30.0000000000001,-1.17524047358085,19.5625));
#58581=CARTESIAN_POINT('',(29.9999999999998,-1.17524047358085,19.4999999999999));
#58582=CARTESIAN_POINT('',(30.,-1.17524047358085,15.78125));
#58583=CARTESIAN_POINT('Ctrl Pts',(30.0000000000003,-1.17524047358085,19.5625));
#58584=CARTESIAN_POINT('Ctrl Pts',(29.9013941092948,-1.17524047358088,19.5564448416279));
#58585=CARTESIAN_POINT('Ctrl Pts',(29.8029987638489,-1.16283641906691,19.549962842264));
#58586=CARTESIAN_POINT('Ctrl Pts',(29.5564668004839,-1.09938994466242,19.5325744732568));
#58587=CARTESIAN_POINT('Ctrl Pts',(29.415037771559,-1.03111229808663,19.5214689478566));
#58588=CARTESIAN_POINT('Ctrl Pts',(29.1716434679328,-0.847005065425004,
19.4999953804452));
#58589=CARTESIAN_POINT('Ctrl Pts',(29.0705827398005,-0.734710314058229,
19.4898082076353));
#58590=CARTESIAN_POINT('Ctrl Pts',(28.9129094963582,-0.472970867922037,
19.4708462190468));
#58591=CARTESIAN_POINT('Ctrl Pts',(28.8598073237114,-0.32477237703938,19.4605287888834));
#58592=CARTESIAN_POINT('Ctrl Pts',(28.8149047814539,-0.0184511328725056,
19.4388083232246));
#58593=CARTESIAN_POINT('Ctrl Pts',(28.8226412643137,0.136461808695805,19.4278238378469));
#58594=CARTESIAN_POINT('Ctrl Pts',(28.8961732267534,0.430084241574931,19.4070038128194));
#58595=CARTESIAN_POINT('Ctrl Pts',(28.9595331463533,0.5664127336681,19.3979778677293));
#58596=CARTESIAN_POINT('Ctrl Pts',(29.137896746023,0.813817787616469,19.3782535402653));
#58597=CARTESIAN_POINT('Ctrl Pts',(29.2533816215898,0.92090330809607,19.3673653008166));
#58598=CARTESIAN_POINT('Ctrl Pts',(29.5158730245192,1.08160589182486,19.3455488072285));
#58599=CARTESIAN_POINT('Ctrl Pts',(29.6595524720356,1.13505921849913,19.3348306663965));
#58600=CARTESIAN_POINT('Ctrl Pts',(29.9586626554596,1.18420822106571,19.3147204900089));
#58601=CARTESIAN_POINT('Ctrl Pts',(30.1111738123977,1.17970362181747,19.305831310076));
#58602=CARTESIAN_POINT('Ctrl Pts',(30.4108580361143,1.11207867833533,19.2850308420592));
#58603=CARTESIAN_POINT('Ctrl Pts',(30.5546592354692,1.0477915906526,19.2739211274165));
#58604=CARTESIAN_POINT('Ctrl Pts',(30.8039627363725,0.870265103601911,19.2523180019705));
#58605=CARTESIAN_POINT('Ctrl Pts',(30.9084512058835,0.760562755820576,19.242012249931));
#58606=CARTESIAN_POINT('Ctrl Pts',(31.0738897348627,0.502419631313023,19.2227009162624));
#58607=CARTESIAN_POINT('Ctrl Pts',(31.1311837638208,0.355135076925594,19.2126817312365));
#58608=CARTESIAN_POINT('Ctrl Pts',(31.1842706831827,0.04913932312708,19.1909843452775));
#58609=CARTESIAN_POINT('Ctrl Pts',(31.1805124566442,-0.106321035688241,
19.1799610439256));
#58610=CARTESIAN_POINT('Ctrl Pts',(31.1143513914742,-0.401996025434437,
19.1589954772754));
#58611=CARTESIAN_POINT('Ctrl Pts',(31.0545027280943,-0.539801328735837,
19.1497832518808));
#58612=CARTESIAN_POINT('Ctrl Pts',(30.8825757787308,-0.791565442014421,
19.1302996391962));
#58613=CARTESIAN_POINT('Ctrl Pts',(30.7698754890686,-0.90154647307845,19.1194797380197));
#58614=CARTESIAN_POINT('Ctrl Pts',(30.5112798180774,-1.06909180183037,19.0976598713853));
#58615=CARTESIAN_POINT('Ctrl Pts',(30.3686300461772,-1.12627173763864,19.0868728383175));
#58616=CARTESIAN_POINT('Ctrl Pts',(30.146651557919,-1.16837939048486,19.071748782068));
#58617=CARTESIAN_POINT('Ctrl Pts',(30.0733297917687,-1.17524047358085,19.0670030119334));
#58618=CARTESIAN_POINT('Ctrl Pts',(30.,-1.17524047358085,19.0625));
#58619=CARTESIAN_POINT('Ctrl Pts',(29.9999999999996,-1.17524047358085,18.9999999999999));
#58620=CARTESIAN_POINT('Ctrl Pts',(30.1208018343283,-1.17524047358085,19.0074181596379));
#58621=CARTESIAN_POINT('Ctrl Pts',(30.2410273417982,-1.15662316578329,19.0154609815185));
#58622=CARTESIAN_POINT('Ctrl Pts',(30.5033214237856,-1.07312795539109,19.0345280681775));
#58623=CARTESIAN_POINT('Ctrl Pts',(30.6395388198866,-0.997960158889978,
19.0455578408927));
#58624=CARTESIAN_POINT('Ctrl Pts',(30.876878941369,-0.797935916319293,19.067223952545));
#58625=CARTESIAN_POINT('Ctrl Pts',(30.9750570407496,-0.674426741281125,
19.0771781033725));
#58626=CARTESIAN_POINT('Ctrl Pts',(31.1146479426385,-0.401644540658674,
19.0965204001729));
#58627=CARTESIAN_POINT('Ctrl Pts',(31.1567939343853,-0.256055794064216,
19.1068437304378));
#58628=CARTESIAN_POINT('Ctrl Pts',(31.1845453028865,0.0488704061743495,
19.1284652770555));
#58629=CARTESIAN_POINT('Ctrl Pts',(31.1676027188842,0.205546638234067,19.1395747929079));
#58630=CARTESIAN_POINT('Ctrl Pts',(31.0749923240704,0.498408501569657,19.1603408878703));
#58631=CARTESIAN_POINT('Ctrl Pts',(31.0021074917097,0.632295920687204,19.1692134966416));
#58632=CARTESIAN_POINT('Ctrl Pts',(30.8090318381138,0.865881565613648,19.1893513074212));
#58633=CARTESIAN_POINT('Ctrl Pts',(30.6904244547157,0.963111668252584,19.2000818814201));
#58634=CARTESIAN_POINT('Ctrl Pts',(30.419302827982,1.10891198567697,19.2218999959461));
#58635=CARTESIAN_POINT('Ctrl Pts',(30.2686205389783,1.15471361101177,19.232776883577));
#58636=CARTESIAN_POINT('Ctrl Pts',(29.9650775926592,1.18413115670169,19.2524597117397));
#58637=CARTESIAN_POINT('Ctrl Pts',(29.8154193388389,1.17018311968912,19.2615139711268));
#58638=CARTESIAN_POINT('Ctrl Pts',(29.5246945745281,1.08577187830739,19.2823593965739));
#58639=CARTESIAN_POINT('Ctrl Pts',(29.3869225275025,1.01437069769904,19.2933510961767));
#58640=CARTESIAN_POINT('Ctrl Pts',(29.1449076103833,0.821179121928182,19.3150620325829));
#58641=CARTESIAN_POINT('Ctrl Pts',(29.0436548787038,0.700625409307818,19.3253204220004));
#58642=CARTESIAN_POINT('Ctrl Pts',(28.8969987915807,0.43246305184088,19.3443351373923));
#58643=CARTESIAN_POINT('Ctrl Pts',(28.8509250755758,0.288512534702925,19.3545423049446));
#58644=CARTESIAN_POINT('Ctrl Pts',(28.8145962917767,-0.0146433580687103,
19.3760383235316));
#58645=CARTESIAN_POINT('Ctrl Pts',(28.8269416915671,-0.171282191603316,
19.3871451875491));
#58646=CARTESIAN_POINT('Ctrl Pts',(28.9109596159865,-0.467218400914038,
19.4081292766188));
#58647=CARTESIAN_POINT('Ctrl Pts',(28.9804361831083,-0.603975745967944,
19.4171374882925));
#58648=CARTESIAN_POINT('Ctrl Pts',(29.167379298401,-0.843150163563664,19.4370968570367));
#58649=CARTESIAN_POINT('Ctrl Pts',(29.2829166096857,-0.943363871775425,
19.447744685016));
#58650=CARTESIAN_POINT('Ctrl Pts',(29.5508199561077,-1.09737775425148,19.4696563740096));
#58651=CARTESIAN_POINT('Ctrl Pts',(29.7018004358378,-1.14764798506443,19.4807100016028));
#58652=CARTESIAN_POINT('Ctrl Pts',(29.9053565213586,-1.17238533019257,19.4940869386326));
#58653=CARTESIAN_POINT('Ctrl Pts',(29.9526999581129,-1.17524047358085,19.4970954144566));
#58654=CARTESIAN_POINT('Ctrl Pts',(29.9999999999997,-1.17524047358085,19.4999999999999));
#58655=CARTESIAN_POINT('Origin',(30.,-1.21864324187371E-14,15.78125));
#58656=CARTESIAN_POINT('',(30.0000000000003,-1.17524047358085,20.0625));
#58657=CARTESIAN_POINT('',(30.,-1.17524047358085,20.));
#58658=CARTESIAN_POINT('',(30.,-1.17524047358085,15.78125));
#58659=CARTESIAN_POINT('Ctrl Pts',(30.0000000000005,-1.17524047358085,20.0625));
#58660=CARTESIAN_POINT('Ctrl Pts',(29.8795085612599,-1.17524047358091,20.0551009010331));
#58661=CARTESIAN_POINT('Ctrl Pts',(29.7595622632698,-1.15671912815303,20.0470786269818));
#58662=CARTESIAN_POINT('Ctrl Pts',(29.4968909328774,-1.07331217196907,20.0279915033172));
#58663=CARTESIAN_POINT('Ctrl Pts',(29.3601452160293,-0.997848639613717,
20.0169188027128));
#58664=CARTESIAN_POINT('Ctrl Pts',(29.1279895360134,-0.801888849412877,
19.9957151555763));
#58665=CARTESIAN_POINT('Ctrl Pts',(29.0334325756294,-0.684937055319331,
19.9860671564471));
#58666=CARTESIAN_POINT('Ctrl Pts',(28.8898211655935,-0.415941538872162,
19.9669933638564));
#58667=CARTESIAN_POINT('Ctrl Pts',(28.8445081931777,-0.265175978908636,
19.956302958832));
#58668=CARTESIAN_POINT('Ctrl Pts',(28.8156113317766,0.0421759568632406,
19.934509409435));
#58669=CARTESIAN_POINT('Ctrl Pts',(28.8311290214712,0.195715280521655,19.9236223238335));
#58670=CARTESIAN_POINT('Ctrl Pts',(28.9191574051752,0.485137216573778,19.9031001454256));
#58671=CARTESIAN_POINT('Ctrl Pts',(28.9896097101006,0.618617028321211,19.8942800985803));
#58672=CARTESIAN_POINT('Ctrl Pts',(29.1815016413357,0.8578593810217,19.8740144260076));
#58673=CARTESIAN_POINT('Ctrl Pts',(29.3033374545183,0.95943115864218,19.8629316730427));
#58674=CARTESIAN_POINT('Ctrl Pts',(29.5744131919249,1.10584185120943,19.8410947363937));
#58675=CARTESIAN_POINT('Ctrl Pts',(29.7199575824398,1.1513488317962,19.8305438014147));
#58676=CARTESIAN_POINT('Ctrl Pts',(30.0223936436952,1.18496921575338,19.8107799381662));
#58677=CARTESIAN_POINT('Ctrl Pts',(30.17645595477,1.17197553997772,19.8015484961906));
#58678=CARTESIAN_POINT('Ctrl Pts',(30.4728526803367,1.08704252391974,19.7803362699347));
#58679=CARTESIAN_POINT('Ctrl Pts',(30.6120360120599,1.01521369720442,19.7692427449689));
#58680=CARTESIAN_POINT('Ctrl Pts',(30.8500255075595,0.825212607475584,19.7478921149936));
#58681=CARTESIAN_POINT('Ctrl Pts',(30.9478859340228,0.710618012755788,19.7378881282691));
#58682=CARTESIAN_POINT('Ctrl Pts',(31.0987101974267,0.445344450081356,19.7190782500187));
#58683=CARTESIAN_POINT('Ctrl Pts',(31.148011535677,0.295869142851177,19.7084793335565));
#58684=CARTESIAN_POINT('Ctrl Pts',(31.1851397417262,-0.0109614779842622,
19.6867227492848));
#58685=CARTESIAN_POINT('Ctrl Pts',(31.1736153786499,-0.165256365490512,
19.6757820885594));
#58686=CARTESIAN_POINT('Ctrl Pts',(31.093043155488,-0.456865689692268,19.6551048079831));
#58687=CARTESIAN_POINT('Ctrl Pts',(31.0262715370984,-0.591802059151614,
19.6462060198927));
#58688=CARTESIAN_POINT('Ctrl Pts',(30.8407896047275,-0.836102523209368,
19.6261546414896));
#58689=CARTESIAN_POINT('Ctrl Pts',(30.7213221432726,-0.941101033293042,
19.6150958330235));
#58690=CARTESIAN_POINT('Ctrl Pts',(30.4533957183897,-1.09478566221008,19.5931944001043));
#58691=CARTESIAN_POINT('Ctrl Pts',(30.3086782810935,-1.14405280540599,19.5825609345826));
#58692=CARTESIAN_POINT('Ctrl Pts',(30.1059062370161,-1.17166523878134,19.5691302110914));
#58693=CARTESIAN_POINT('Ctrl Pts',(30.0529306288365,-1.17524047358084,19.5657503467901));
#58694=CARTESIAN_POINT('Ctrl Pts',(30.0000000000003,-1.17524047358085,19.5625));
#58695=CARTESIAN_POINT('Ctrl Pts',(29.9999999999997,-1.17524047358085,19.4999999999999));
#58696=CARTESIAN_POINT('Ctrl Pts',(30.1013134091967,-1.17524047358085,19.5062214207844));
#58697=CARTESIAN_POINT('Ctrl Pts',(30.2023703512557,-1.16214610944681,19.5128913366607));
#58698=CARTESIAN_POINT('Ctrl Pts',(30.4489451189351,-1.0968832859302,19.530346730545));
#58699=CARTESIAN_POINT('Ctrl Pts',(30.5880725807912,-1.02901377075515,19.5412964522821));
#58700=CARTESIAN_POINT('Ctrl Pts',(30.8343712795547,-0.842194481571482,
19.5630445243813));
#58701=CARTESIAN_POINT('Ctrl Pts',(30.9385897374703,-0.724253666071193,
19.5736257801046));
#58702=CARTESIAN_POINT('Ctrl Pts',(31.0916505061583,-0.460199205120922,
19.5923866032744));
#58703=CARTESIAN_POINT('Ctrl Pts',(31.1412805360793,-0.317836464065441,
19.6024630191855));
#58704=CARTESIAN_POINT('Ctrl Pts',(31.1853286010408,-0.0163533735884271,
19.6238404235873));
#58705=CARTESIAN_POINT('Ctrl Pts',(31.1771308821554,0.140138676220234,19.6349368795415));
#58706=CARTESIAN_POINT('Ctrl Pts',(31.1009443941398,0.438772825443172,19.6561122727154));
#58707=CARTESIAN_POINT('Ctrl Pts',(31.0345585763112,0.578169376036336,19.6653017627446));
#58708=CARTESIAN_POINT('Ctrl Pts',(30.8531427469532,0.82231181712456,19.6850978487155));
#58709=CARTESIAN_POINT('Ctrl Pts',(30.7404083067898,0.925109501957493,19.6956651705268));
#58710=CARTESIAN_POINT('Ctrl Pts',(30.4771535858122,1.08544747135218,19.7175156107599));
#58711=CARTESIAN_POINT('Ctrl Pts',(30.3279214291812,1.13945389596675,19.7285943399309));
#58712=CARTESIAN_POINT('Ctrl Pts',(30.0245530133835,1.1844610145353,19.7488191591971));
#58713=CARTESIAN_POINT('Ctrl Pts',(29.8738446796079,1.17798106878653,19.7576497404222));
#58714=CARTESIAN_POINT('Ctrl Pts',(29.5795308296296,1.10805786067705,19.7782019083499));
#58715=CARTESIAN_POINT('Ctrl Pts',(29.4390520876789,1.04399036655414,19.7890998131999));
#58716=CARTESIAN_POINT('Ctrl Pts',(29.1881857877585,0.86396490371117,19.8108875045287));
#58717=CARTESIAN_POINT('Ctrl Pts',(29.0808654270878,0.748795351686304,19.8215609892382));
#58718=CARTESIAN_POINT('Ctrl Pts',(28.9210185508111,0.489082061917269,19.8405846207479));
#58719=CARTESIAN_POINT('Ctrl Pts',(28.8677194354805,0.348399842158546,19.8502958472478));
#58720=CARTESIAN_POINT('Ctrl Pts',(28.8156254684423,0.0489678765559477,
19.8715278115659));
#58721=CARTESIAN_POINT('Ctrl Pts',(28.8194748723048,-0.107254256712007,
19.88260512842));
#58722=CARTESIAN_POINT('Ctrl Pts',(28.8873579337553,-0.408638429267571,
19.9039755188019));
#58723=CARTESIAN_POINT('Ctrl Pts',(28.9504754704978,-0.550854728104584,
19.9134143320288));
#58724=CARTESIAN_POINT('Ctrl Pts',(29.1260934520651,-0.800139160205639,
19.9330366884507));
#58725=CARTESIAN_POINT('Ctrl Pts',(29.2358570179041,-0.905539531949709,
19.9435138507578));
#58726=CARTESIAN_POINT('Ctrl Pts',(29.4941308064619,-1.07230397107708,19.9652862658853));
#58727=CARTESIAN_POINT('Ctrl Pts',(29.6414537313008,-1.13013161490591,19.9763832300743));
#58728=CARTESIAN_POINT('Ctrl Pts',(29.8633704190017,-1.16928660340085,19.9913988083098));
#58729=CARTESIAN_POINT('Ctrl Pts',(29.9316910379181,-1.17524047358085,19.9958053055382));
#58730=CARTESIAN_POINT('Ctrl Pts',(30.,-1.17524047358085,20.));
#58731=CARTESIAN_POINT('Origin',(30.,-1.21864324187371E-14,15.78125));
#58732=CARTESIAN_POINT('',(30.,-1.17524047358085,20.5625));
#58733=CARTESIAN_POINT('',(30.,-1.17524047358085,20.5));
#58734=CARTESIAN_POINT('',(30.,-1.17524047358085,15.78125));
#58735=CARTESIAN_POINT('Ctrl Pts',(30.0000000000001,-1.17524047358085,20.5625));
#58736=CARTESIAN_POINT('Ctrl Pts',(29.857466677664,-1.17524047358086,20.5537473602351));
#58737=CARTESIAN_POINT('Ctrl Pts',(29.7159780885029,-1.14931710991913,20.5441397949867));
#58738=CARTESIAN_POINT('Ctrl Pts',(29.4386327044728,-1.04389937724848,20.5233712075421));
#58739=CARTESIAN_POINT('Ctrl Pts',(29.3069416102485,-0.961526015490682,
20.5123639202805));
#58740=CARTESIAN_POINT('Ctrl Pts',(29.086333053172,-0.75405497378,20.4914612382194));
#58741=CARTESIAN_POINT('Ctrl Pts',(28.998234525789,-0.632326756560098,20.4823366930552));
#58742=CARTESIAN_POINT('Ctrl Pts',(28.8691902031313,-0.356072447869899,
20.4627481978422));
#58743=CARTESIAN_POINT('Ctrl Pts',(28.8319810448841,-0.203050335093991,
20.4518977863579));
#58744=CARTESIAN_POINT('Ctrl Pts',(28.8195943462911,0.104677105391675,20.4300776108702));
#58745=CARTESIAN_POINT('Ctrl Pts',(28.8430260194231,0.256395499280261,20.419319642799));
#58746=CARTESIAN_POINT('Ctrl Pts',(28.9459812899286,0.541272174450661,20.399119757359));
#58747=CARTESIAN_POINT('Ctrl Pts',(29.0240298052411,0.671873753047622,20.3902782906932));
#58748=CARTESIAN_POINT('Ctrl Pts',(29.2288981247322,0.900554058537053,20.3695902323474));
#58749=CARTESIAN_POINT('Ctrl Pts',(29.3552896087803,0.99495410007641,20.3584819910769));
#58750=CARTESIAN_POINT('Ctrl Pts',(29.6322160097862,1.12628386030684,20.3368204541948));
#58751=CARTESIAN_POINT('Ctrl Pts',(29.7791530812878,1.16405670631925,20.3264582018892));
#58752=CARTESIAN_POINT('Ctrl Pts',(30.0846260087116,1.18247957174534,20.3070466605788));
#58753=CARTESIAN_POINT('Ctrl Pts',(30.2403465146444,1.16089584876694,20.297232309072));
#58754=CARTESIAN_POINT('Ctrl Pts',(30.5330201521523,1.05871377596515,20.2756371654718));
#58755=CARTESIAN_POINT('Ctrl Pts',(30.6672316693715,0.979687699230499,20.2645937786601));
#58756=CARTESIAN_POINT('Ctrl Pts',(30.8935142020877,0.777827856358351,20.2435416089216));
#58757=CARTESIAN_POINT('Ctrl Pts',(30.9847747247484,0.658466900361099,20.2341902246224));
#58758=CARTESIAN_POINT('Ctrl Pts',(31.1210267097183,0.385760488516485,20.2148533018128));
#58759=CARTESIAN_POINT('Ctrl Pts',(31.1622514979646,0.233796400148884,20.2040779121667));
#58760=CARTESIAN_POINT('Ctrl Pts',(31.1827840987885,-0.0738574566284658,
20.1822629543138));
#58761=CARTESIAN_POINT('Ctrl Pts',(31.1632412224874,-0.226525134572718,
20.1714376749082));
#58762=CARTESIAN_POINT('Ctrl Pts',(31.0676501608268,-0.513670659031922,
20.1510769110961));
#58763=CARTESIAN_POINT('Ctrl Pts',(30.9933877261944,-0.645689071009633,
20.1422762056128));
#58764=CARTESIAN_POINT('Ctrl Pts',(30.7949445520148,-0.879653706050947,
20.1217953512642));
#58765=CARTESIAN_POINT('Ctrl Pts',(30.670767244765,-0.977642983856647,20.1106958256016));
#58766=CARTESIAN_POINT('Ctrl Pts',(30.3966473841018,-1.11649688166864,20.0889398730384));
#58767=CARTESIAN_POINT('Ctrl Pts',(30.2503518300705,-1.15811817698529,20.0784805729189));
#58768=CARTESIAN_POINT('Ctrl Pts',(30.0667947188483,-1.17381847353791,20.0666521235228));
#58769=CARTESIAN_POINT('Ctrl Pts',(30.0333795266192,-1.17524047358084,20.0645497590825));
#58770=CARTESIAN_POINT('Ctrl Pts',(30.0000000000005,-1.17524047358085,20.0625));
#58771=CARTESIAN_POINT('Ctrl Pts',(30.,-1.17524047358085,20.));
#58772=CARTESIAN_POINT('Ctrl Pts',(30.0810461612404,-1.17524047358085,20.0049768562329));
#58773=CARTESIAN_POINT('Ctrl Pts',(30.1620390634994,-1.16685998246121,20.0102475616837));
#58774=CARTESIAN_POINT('Ctrl Pts',(30.3910188268312,-1.11873616439623,20.0260148454886));
#58775=CARTESIAN_POINT('Ctrl Pts',(30.5327757448135,-1.05858684074315,20.0368523263699));
#58776=CARTESIAN_POINT('Ctrl Pts',(30.7881241531233,-0.885634167315425,
20.0586644967329));
#58777=CARTESIAN_POINT('Ctrl Pts',(30.8985424642913,-0.773390023616368,
20.0694245027186));
#58778=CARTESIAN_POINT('Ctrl Pts',(31.0652926267422,-0.518183463935382,
20.0887122685505));
#58779=CARTESIAN_POINT('Ctrl Pts',(31.1223297618129,-0.379162720763723,
20.0981145292327));
#58780=CARTESIAN_POINT('Ctrl Pts',(31.182501138976,-0.0818619977066759,
20.1191953725253));
#58781=CARTESIAN_POINT('Ctrl Pts',(31.1830210318339,0.0739680814447177,
20.1302448898124));
#58782=CARTESIAN_POINT('Ctrl Pts',(31.1235906320717,0.378032609170699,20.1518053374088));
#58783=CARTESIAN_POINT('Ctrl Pts',(31.0637982215859,0.523138441463073,20.1615551718639));
#58784=CARTESIAN_POINT('Ctrl Pts',(30.8940186419568,0.777530022608243,20.1810000731231));
#58785=CARTESIAN_POINT('Ctrl Pts',(30.7872728375238,0.885439479392022,20.1913808781633));
#58786=CARTESIAN_POINT('Ctrl Pts',(30.5341117586616,1.05845819784869,20.2130610712561));
#58787=CARTESIAN_POINT('Ctrl Pts',(30.3887837233288,1.12003007025227,20.2241682808161));
#58788=CARTESIAN_POINT('Ctrl Pts',(30.0880464072922,1.18158358213937,20.2448181618436));
#58789=CARTESIAN_POINT('Ctrl Pts',(29.9360438868879,1.18313176496437,20.2536476203627));
#58790=CARTESIAN_POINT('Ctrl Pts',(29.6381705506099,1.1284628410545,20.2738775466838));
#58791=CARTESIAN_POINT('Ctrl Pts',(29.4952627894061,1.07218329111658,20.2846485002308));
#58792=CARTESIAN_POINT('Ctrl Pts',(29.2357076507194,0.906285518142771,20.3064688735353));
#58793=CARTESIAN_POINT('Ctrl Pts',(29.1223265216238,0.796998466553187,20.3173059793119));
#58794=CARTESIAN_POINT('Ctrl Pts',(28.94883850375,0.546283376626024,20.3368482617845));
#58795=CARTESIAN_POINT('Ctrl Pts',(28.8881400415123,0.408839661433748,20.3460102123335));
#58796=CARTESIAN_POINT('Ctrl Pts',(28.8201837019616,0.113659356458156,20.3669407021362));
#58797=CARTESIAN_POINT('Ctrl Pts',(28.8154556440784,-0.0416770716817043,
20.377955215877));
#58798=CARTESIAN_POINT('Ctrl Pts',(28.8666287496698,-0.348241759389233,
20.3996929435023));
#58799=CARTESIAN_POINT('Ctrl Pts',(28.923168044506,-0.496185032937023,20.4097992015263));
#58800=CARTESIAN_POINT('Ctrl Pts',(29.0873034963183,-0.755446668555585,
20.4290701716561));
#58801=CARTESIAN_POINT('Ctrl Pts',(29.1911125253156,-0.865675121623956,
20.4393528532326));
#58802=CARTESIAN_POINT('Ctrl Pts',(29.4392495659902,-1.04453090441881,20.4609314775711));
#58803=CARTESIAN_POINT('Ctrl Pts',(29.5825856119781,-1.10962145963742,20.4720411141544));
#58804=CARTESIAN_POINT('Ctrl Pts',(29.8217321396476,-1.16509155071327,20.4886931681386));
#58805=CARTESIAN_POINT('Ctrl Pts',(29.9108091908387,-1.17524047358086,20.4945229998842));
#58806=CARTESIAN_POINT('Ctrl Pts',(30.0000000000001,-1.17524047358085,20.5));
#58807=CARTESIAN_POINT('Origin',(30.,-1.21864324187371E-14,15.78125));
#58808=CARTESIAN_POINT('',(30.,-1.17524047358085,21.0625));
#58809=CARTESIAN_POINT('',(30.0000000000003,-1.17524047358085,21.));
#58810=CARTESIAN_POINT('',(30.,-1.17524047358085,15.78125));
#58811=CARTESIAN_POINT('Ctrl Pts',(30.,-1.17524047358085,21.0625));
#58812=CARTESIAN_POINT('Ctrl Pts',(29.9930425354756,-1.17524047358085,21.062072758288));
#58813=CARTESIAN_POINT('Ctrl Pts',(29.9860827950433,-1.17517869098314,21.0616431863938));
#58814=CARTESIAN_POINT('Ctrl Pts',(29.8232316065342,-1.17228514735699,21.0515402867957));
#58815=CARTESIAN_POINT('Ctrl Pts',(29.6694853244495,-1.13852257202281,21.0409020757897));
#58816=CARTESIAN_POINT('Ctrl Pts',(29.3867104280309,-1.01415059452875,21.0191280758083));
#58817=CARTESIAN_POINT('Ctrl Pts',(29.2599516823908,-0.925722033008617,
21.0082089931399));
#58818=CARTESIAN_POINT('Ctrl Pts',(29.0500490851207,-0.707886564567504,
20.9875962815068));
#58819=CARTESIAN_POINT('Ctrl Pts',(28.9678750474644,-0.58156955059427,20.9787376277926));
#58820=CARTESIAN_POINT('Ctrl Pts',(28.852209421352,-0.297516308143681,20.9585961298867));
#58821=CARTESIAN_POINT('Ctrl Pts',(28.8227455494544,-0.141401249035421,
20.9475264053908));
#58822=CARTESIAN_POINT('Ctrl Pts',(28.8269065561122,0.16711629798966,20.9256502054441));
#58823=CARTESIAN_POINT('Ctrl Pts',(28.8581354481118,0.316603790040456,20.915050424987));
#58824=CARTESIAN_POINT('Ctrl Pts',(28.9760761175465,0.596699382404322,20.8951895540518));
#58825=CARTESIAN_POINT('Ctrl Pts',(29.0620842641545,0.724424918144287,20.8860783197069));
#58826=CARTESIAN_POINT('Ctrl Pts',(29.2801481558297,0.941880855388224,20.8649778977684));
#58827=CARTESIAN_POINT('Ctrl Pts',(29.4108173740059,1.02868094436595,20.8538764175153));
#58828=CARTESIAN_POINT('Ctrl Pts',(29.6929274853784,1.14422525088517,20.8324562143623));
#58829=CARTESIAN_POINT('Ctrl Pts',(29.8408766090356,1.17398844910975,20.8223157862342));
#58830=CARTESIAN_POINT('Ctrl Pts',(30.146238089068,1.17646530253954,20.8034764343644));
#58831=CARTESIAN_POINT('Ctrl Pts',(30.3008127704194,1.14674523024735,20.7930175246536));
#58832=CARTESIAN_POINT('Ctrl Pts',(30.5871854304481,1.02954198948055,20.7712767528846));
#58833=CARTESIAN_POINT('Ctrl Pts',(30.7164764357369,0.944145175747713,20.7603096568304));
#58834=CARTESIAN_POINT('Ctrl Pts',(30.9318157386174,0.731537563311469,20.7395484367846));
#58835=CARTESIAN_POINT('Ctrl Pts',(31.0169931096024,0.607571893797524,20.7305813882675));
#58836=CARTESIAN_POINT('Ctrl Pts',(31.1392545858023,0.328058458126713,20.7107617965928));
#58837=CARTESIAN_POINT('Ctrl Pts',(31.1726798971535,0.174145191638854,20.6998481956499));
#58838=CARTESIAN_POINT('Ctrl Pts',(31.177452605602,-0.133454152417299,20.6780371031564));
#58839=CARTESIAN_POINT('Ctrl Pts',(31.1504138008343,-0.284195707834949,
20.6673484002337));
#58840=CARTESIAN_POINT('Ctrl Pts',(31.0405663350578,-0.566901684154618,
20.647302433566));
#58841=CARTESIAN_POINT('Ctrl Pts',(30.9589018497076,-0.696179869646961,
20.6383684206626));
#58842=CARTESIAN_POINT('Ctrl Pts',(30.7479829469593,-0.919779045347213,
20.6174889551129));
#58843=CARTESIAN_POINT('Ctrl Pts',(30.6195839675717,-1.0107321163549,20.6063796462101));
#58844=CARTESIAN_POINT('Ctrl Pts',(30.3401820261614,-1.13487834149049,20.5848207753144));
#58845=CARTESIAN_POINT('Ctrl Pts',(30.1927291526794,-1.16899555973842,20.5745564544744));
#58846=CARTESIAN_POINT('Ctrl Pts',(30.02853673898,-1.17498080122699,20.5642615811144));
#58847=CARTESIAN_POINT('Ctrl Pts',(30.0142636931895,-1.17524047358085,20.5633759002187));
#58848=CARTESIAN_POINT('Ctrl Pts',(30.0000000000001,-1.17524047358085,20.5625));
#58849=CARTESIAN_POINT('Ctrl Pts',(30.0000000000001,-1.17524047358085,20.5));
#58850=CARTESIAN_POINT('Ctrl Pts',(30.0615320920417,-1.17524047358085,20.5037785426368));
#58851=CARTESIAN_POINT('Ctrl Pts',(30.1230970944725,-1.17040913175211,20.5077303953467));
#58852=CARTESIAN_POINT('Ctrl Pts',(30.3340845761439,-1.13693724894346,20.5218733491291));
#58853=CARTESIAN_POINT('Ctrl Pts',(30.4779822284686,-1.08432359797014,20.5325751197693));
#58854=CARTESIAN_POINT('Ctrl Pts',(30.7413240882277,-0.925171378815601,
20.5543888717152));
#58855=CARTESIAN_POINT('Ctrl Pts',(30.8574242886598,-0.818746672756081,
20.5652914684918));
#58856=CARTESIAN_POINT('Ctrl Pts',(31.0372296037246,-0.572330389441825,
20.5850692727305));
#58857=CARTESIAN_POINT('Ctrl Pts',(31.1013789298939,-0.436327710632643,
20.5940611041994));
#58858=CARTESIAN_POINT('Ctrl Pts',(31.1765507195451,-0.143169609179877,
20.6148482046583));
#58859=CARTESIAN_POINT('Ctrl Pts',(31.1851707108535,0.0116076749541518,
20.6258230709101));
#58860=CARTESIAN_POINT('Ctrl Pts',(31.1420730921553,0.318093458162843,20.6475552036167));
#58861=CARTESIAN_POINT('Ctrl Pts',(31.0898417933348,0.466589648702242,20.6579510306787));
#58862=CARTESIAN_POINT('Ctrl Pts',(30.9337645237733,0.729159361106415,20.6768444502657));
#58863=CARTESIAN_POINT('Ctrl Pts',(30.8334379992983,0.84198975683026,20.6870055279311));
#58864=CARTESIAN_POINT('Ctrl Pts',(30.591317195237,1.02746666327729,20.7084494527507));
#58865=CARTESIAN_POINT('Ctrl Pts',(30.4504043784541,1.09657907803444,20.7195528744157));
#58866=CARTESIAN_POINT('Ctrl Pts',(30.1527579068286,1.17519666342875,20.7406179390521));
#58867=CARTESIAN_POINT('Ctrl Pts',(29.9992772327099,1.18508027808452,20.7496955256169));
#58868=CARTESIAN_POINT('Ctrl Pts',(29.6980213394833,1.14582802600215,20.7695865882633));
#58869=CARTESIAN_POINT('Ctrl Pts',(29.5531012936116,1.09744171629364,20.7802012666676));
#58870=CARTESIAN_POINT('Ctrl Pts',(29.2844190436536,0.945457598499347,20.8020888235724));
#58871=CARTESIAN_POINT('Ctrl Pts',(29.1643876737344,0.84125826030012,20.8131539267157));
#58872=CARTESIAN_POINT('Ctrl Pts',(28.9773975743441,0.59813879267389,20.8332560474103));
#58873=CARTESIAN_POINT('Ctrl Pts',(28.9097638018428,0.463547729800393,20.8421310013978));
#58874=CARTESIAN_POINT('Ctrl Pts',(28.8274319674294,0.172449502758382,20.8627720413655));
#58875=CARTESIAN_POINT('Ctrl Pts',(28.8149632933605,0.0183235810432114,
20.8737007211534));
#58876=CARTESIAN_POINT('Ctrl Pts',(28.850150967155,-0.288650006351519,20.8954674428227));
#58877=CARTESIAN_POINT('Ctrl Pts',(28.898515176706,-0.438439388541448,20.906088629547));
#58878=CARTESIAN_POINT('Ctrl Pts',(29.047641063206,-0.704596833168998,20.9249611816339));
#58879=CARTESIAN_POINT('Ctrl Pts',(29.1447168471359,-0.819746341645053,
20.9348754556746));
#58880=CARTESIAN_POINT('Ctrl Pts',(29.381325819526,-1.01116668011756,20.9561916286088));
#58881=CARTESIAN_POINT('Ctrl Pts',(29.5199396968772,-1.08386414625954,20.96728098122));
#58882=CARTESIAN_POINT('Ctrl Pts',(29.7764916553148,-1.15925176815251,20.9857080131187));
#58883=CARTESIAN_POINT('Ctrl Pts',(29.8880479255875,-1.1752404735809,20.9931252835322));
#58884=CARTESIAN_POINT('Ctrl Pts',(30.0000000000005,-1.17524047358085,21.));
#58885=CARTESIAN_POINT('Origin',(30.,-1.21864324187371E-14,15.78125));
#58886=CARTESIAN_POINT('',(29.9999999999998,-1.17524047358085,21.5625));
#58887=CARTESIAN_POINT('',(30.0000000000001,-1.17524047358085,21.5));
#58888=CARTESIAN_POINT('',(30.,-1.17524047358085,15.78125));
#58889=CARTESIAN_POINT('Ctrl Pts',(29.9999999999996,-1.17524047358085,21.5625));
#58890=CARTESIAN_POINT('Ctrl Pts',(29.9719988088573,-1.17524047358085,21.5607805119881));
#58891=CARTESIAN_POINT('Ctrl Pts',(29.9439711363572,-1.17423978092491,21.5590239195234));
#58892=CARTESIAN_POINT('Ctrl Pts',(29.7604047377572,-1.16108096387714,21.547285004757));
#58893=CARTESIAN_POINT('Ctrl Pts',(29.6086428973266,-1.11907669828182,21.5364764549777));
#58894=CARTESIAN_POINT('Ctrl Pts',(29.3336394628651,-0.979972388454951,
21.5146573661612));
#58895=CARTESIAN_POINT('Ctrl Pts',(29.2123764352237,-0.885461951955829,
21.503860137555));
#58896=CARTESIAN_POINT('Ctrl Pts',(29.0139169118187,-0.656850944948416,
21.4835680853588));
#58897=CARTESIAN_POINT('Ctrl Pts',(28.9380513713638,-0.525431379870783,
21.4747570119112));
#58898=CARTESIAN_POINT('Ctrl Pts',(28.8379806985326,-0.235334014126339,
21.4541869404899));
#58899=CARTESIAN_POINT('Ctrl Pts',(28.81701218115,-0.0787326333033737,21.4430827321496));
#58900=CARTESIAN_POINT('Ctrl Pts',(28.8372148732154,0.227544173701852,21.4213654174177));
#58901=CARTESIAN_POINT('Ctrl Pts',(28.8758855793473,0.374476178993786,21.4109468400715));
#58902=CARTESIAN_POINT('Ctrl Pts',(29.008483168462,0.64967403277934,21.3914332554072));
#58903=CARTESIAN_POINT('Ctrl Pts',(29.1026400510551,0.774562668949264,21.3818103125428));
#58904=CARTESIAN_POINT('Ctrl Pts',(29.3337333173752,0.980382528955385,21.3603223294383));
#58905=CARTESIAN_POINT('Ctrl Pts',(29.4682481852686,1.05938687455618,21.3492610850172));
#58906=CARTESIAN_POINT('Ctrl Pts',(29.7549668128984,1.15903498567807,21.3281214631321));
#58907=CARTESIAN_POINT('Ctrl Pts',(29.9037091563498,1.1807204220266,21.3186072813687));
#58908=CARTESIAN_POINT('Ctrl Pts',(30.2082836909242,1.16710140483065,21.2994212226452));
#58909=CARTESIAN_POINT('Ctrl Pts',(30.3610942123922,1.12920096767185,21.2886937718569));
#58910=CARTESIAN_POINT('Ctrl Pts',(30.6400777787282,0.99739853025376,21.2668891510646));
#58911=CARTESIAN_POINT('Ctrl Pts',(30.7641225887122,0.905886016702667,21.2560273872475));
#58912=CARTESIAN_POINT('Ctrl Pts',(30.9683193471767,0.682639701404097,21.2355732231612));
#58913=CARTESIAN_POINT('Ctrl Pts',(31.0473475790777,0.553805208866279,21.2267689284532));
#58914=CARTESIAN_POINT('Ctrl Pts',(31.1552799375254,0.266708452111841,21.2064116226359));
#58915=CARTESIAN_POINT('Ctrl Pts',(31.1805191858716,0.110295910456217,21.195320804404));
#58916=CARTESIAN_POINT('Ctrl Pts',(31.1683617956532,-0.197210560675315,
21.173516297295));
#58917=CARTESIAN_POINT('Ctrl Pts',(31.1334138492448,-0.345474524238407,
21.1630032741523));
#58918=CARTESIAN_POINT('Ctrl Pts',(31.0081981695942,-0.623166742222595,
21.1433128204234));
#58919=CARTESIAN_POINT('Ctrl Pts',(30.9181918552343,-0.749490769431124,
21.1339784439808));
#58920=CARTESIAN_POINT('Ctrl Pts',(30.6936733778382,-0.961255467276285,
21.1126834366527));
#58921=CARTESIAN_POINT('Ctrl Pts',(30.5610503971428,-1.04422897430134,21.1015976470182));
#58922=CARTESIAN_POINT('Ctrl Pts',(30.283074075588,-1.14948332004627,21.080796107845));
#58923=CARTESIAN_POINT('Ctrl Pts',(30.1420666819575,-1.17524047358085,21.0712239844648));
#58924=CARTESIAN_POINT('Ctrl Pts',(30.,-1.17524047358085,21.0625));
#58925=CARTESIAN_POINT('Ctrl Pts',(30.0000000000005,-1.17524047358085,21.));
#58926=CARTESIAN_POINT('Ctrl Pts',(30.0409368563611,-1.17524047358083,21.0025138371222));
#58927=CARTESIAN_POINT('Ctrl Pts',(30.0819173014533,-1.17310176285816,21.0051061762144));
#58928=CARTESIAN_POINT('Ctrl Pts',(30.2729829235624,-1.15303120950392,21.0175506477331));
#58929=CARTESIAN_POINT('Ctrl Pts',(30.4187156327833,-1.10844931428969,21.0280803491923));
#58930=CARTESIAN_POINT('Ctrl Pts',(30.6905353954506,-0.963834030798816,
21.0498993207407));
#58931=CARTESIAN_POINT('Ctrl Pts',(30.8129383742835,-0.863111359129209,
21.0609867980498));
#58932=CARTESIAN_POINT('Ctrl Pts',(31.0063964161767,-0.625120486728277,
21.0813042721815));
#58933=CARTESIAN_POINT('Ctrl Pts',(31.0777548462909,-0.49199236060375,21.0901140644785));
#58934=CARTESIAN_POINT('Ctrl Pts',(31.1675962416571,-0.203110857145286,
21.1105979221763));
#58935=CARTESIAN_POINT('Ctrl Pts',(31.1840814343856,-0.0497708726068158,
21.1214708731443));
#58936=CARTESIAN_POINT('Ctrl Pts',(31.1571888276141,0.257674311285982,21.14327103453));
#58937=CARTESIAN_POINT('Ctrl Pts',(31.1128522255693,0.408737402730974,21.1539825367601));
#58938=CARTESIAN_POINT('Ctrl Pts',(30.9710010878299,0.678628541040232,21.1731198356347));
#58939=CARTESIAN_POINT('Ctrl Pts',(30.8772391714915,0.796156039182743,21.1826908232652));
#58940=CARTESIAN_POINT('Ctrl Pts',(30.6464955823919,0.993543206250726,21.2038583630273));
#58941=CARTESIAN_POINT('Ctrl Pts',(30.5103519798164,1.06987223749504,21.214924774365));
#58942=CARTESIAN_POINT('Ctrl Pts',(30.2162079552513,1.16549604568273,21.2363776960251));
#58943=CARTESIAN_POINT('Ctrl Pts',(30.061127965963,1.18379547472913,21.2459429670447));
#58944=CARTESIAN_POINT('Ctrl Pts',(29.7567781749822,1.15962478754955,21.2654893209196));
#58945=CARTESIAN_POINT('Ctrl Pts',(29.6103180879013,1.11893466526318,21.2759257110673));
#58946=CARTESIAN_POINT('Ctrl Pts',(29.3355002124366,0.981897695520532,21.2976601102058));
#58947=CARTESIAN_POINT('Ctrl Pts',(29.2107776319456,0.884773136393355,21.3087624623211));
#58948=CARTESIAN_POINT('Ctrl Pts',(29.0107746609087,0.652081932742376,21.3292939522647));
#58949=CARTESIAN_POINT('Ctrl Pts',(28.9355970901093,0.52040794626517,21.3380991870768));
#58950=CARTESIAN_POINT('Ctrl Pts',(28.8382134265824,0.233810524699486,21.3584210862971));
#58951=CARTESIAN_POINT('Ctrl Pts',(28.8177208295725,0.0813648692728661,
21.3692306226469));
#58952=CARTESIAN_POINT('Ctrl Pts',(28.8362699803681,-0.22632694032349,21.3910482716382));
#58953=CARTESIAN_POINT('Ctrl Pts',(28.8765201026755,-0.378558584509325,
21.4018426329915));
#58954=CARTESIAN_POINT('Ctrl Pts',(29.0110211856253,-0.652134791815677,
21.4212412308003));
#58955=CARTESIAN_POINT('Ctrl Pts',(29.1015077791443,-0.772069972681635,
21.4305317818752));
#58956=CARTESIAN_POINT('Ctrl Pts',(29.3264048767426,-0.975307798634206,
21.4515477299157));
#58957=CARTESIAN_POINT('Ctrl Pts',(29.4600073333855,-1.05515984377402,21.4625829994009));
#58958=CARTESIAN_POINT('Ctrl Pts',(29.7321091399909,-1.15220558787994,21.4827327726726));
#58959=CARTESIAN_POINT('Ctrl Pts',(29.8656344449969,-1.17524047358088,21.4917489238272));
#58960=CARTESIAN_POINT('Ctrl Pts',(30.0000000000003,-1.17524047358085,21.5));
#58961=CARTESIAN_POINT('Origin',(30.,-1.21864324187371E-14,15.78125));
#58962=CARTESIAN_POINT('',(29.9999999999998,-1.17524047358085,22.0625));
#58963=CARTESIAN_POINT('',(30.000000003784,-1.17524047358085,22.0000000004647));
#58964=CARTESIAN_POINT('',(30.,-1.17524047358085,15.78125));
#58965=CARTESIAN_POINT('Ctrl Pts',(29.9999999999997,-1.17524047358085,22.0625));
#58966=CARTESIAN_POINT('Ctrl Pts',(29.9524010211782,-1.17524047358085,22.0595770574349));
#58967=CARTESIAN_POINT('Ctrl Pts',(29.9047586284152,-1.17234913259513,22.0565489400777));
#58968=CARTESIAN_POINT('Ctrl Pts',(29.7009349924679,-1.1474210952591,22.0431488126472));
#58969=CARTESIAN_POINT('Ctrl Pts',(29.5500039838267,-1.09704169086814,22.0320943523472));
#58970=CARTESIAN_POINT('Ctrl Pts',(29.2822334508411,-0.942842462410207,
22.01018424791));
#58971=CARTESIAN_POINT('Ctrl Pts',(29.1667766500969,-0.842552714869588,
21.9995386680174));
#58972=CARTESIAN_POINT('Ctrl Pts',(28.9799931885339,-0.603233884932394,
21.9795839832802));
#58973=CARTESIAN_POINT('Ctrl Pts',(28.910605612196,-0.466400997640195,21.9705713166174));
#58974=CARTESIAN_POINT('Ctrl Pts',(28.8268127379948,-0.170385863417145,
21.9495816311816));
#58975=CARTESIAN_POINT('Ctrl Pts',(28.8145871174915,-0.0137497615287427,
21.9384749608582));
#58976=CARTESIAN_POINT('Ctrl Pts',(28.85113877829,0.289356743861303,21.9169824442057));
#58977=CARTESIAN_POINT('Ctrl Pts',(28.8973142483913,0.433263084581444,21.9067784090915));
#58978=CARTESIAN_POINT('Ctrl Pts',(29.0441562961032,0.701308793511537,21.8877719649526));
#58979=CARTESIAN_POINT('Ctrl Pts',(29.145494108998,0.821789237943167,21.8775043861745));
#58980=CARTESIAN_POINT('Ctrl Pts',(29.3876377187977,1.01480099788269,21.8557919221934));
#58981=CARTESIAN_POINT('Ctrl Pts',(29.5254500415353,1.08610079854932,21.8448013436507));
#58982=CARTESIAN_POINT('Ctrl Pts',(29.8162261597603,1.17031056565349,21.8239599076952));
#58983=CARTESIAN_POINT('Ctrl Pts',(29.965897796871,1.18415559330363,21.814910211276));
#58984=CARTESIAN_POINT('Ctrl Pts',(30.2694248477664,1.15452627142302,21.7952208509568));
#58985=CARTESIAN_POINT('Ctrl Pts',(30.4200757340443,1.10861951539323,21.7843421644183));
#58986=CARTESIAN_POINT('Ctrl Pts',(30.6910871340011,0.962634653497324,21.762524275871));
#58987=CARTESIAN_POINT('Ctrl Pts',(30.8096198631452,0.865330005993902,21.7517956433222));
#58988=CARTESIAN_POINT('Ctrl Pts',(31.0025452942337,0.631606479581076,21.7316621689435));
#58989=CARTESIAN_POINT('Ctrl Pts',(31.075346835895,0.497649504779323,21.7227870693252));
#58990=CARTESIAN_POINT('Ctrl Pts',(31.1677479593254,0.204711362167963,21.7020155655921));
#58991=CARTESIAN_POINT('Ctrl Pts',(31.1845780485819,0.0480344792828584,
21.6909060035913));
#58992=CARTESIAN_POINT('Ctrl Pts',(31.1566162472742,-0.256851307753155,
21.6692873225717));
#58993=CARTESIAN_POINT('Ctrl Pts',(31.1143736239456,-0.402401296420415,
21.6589667405334));
#58994=CARTESIAN_POINT('Ctrl Pts',(30.9745867433069,-0.675115053903835,
21.6396292968631));
#58995=CARTESIAN_POINT('Ctrl Pts',(30.8762946890393,-0.798585224220405,
21.6296650545771));
#58996=CARTESIAN_POINT('Ctrl Pts',(30.6387793080734,-0.998444700485959,
21.6079940222289));
#58997=CARTESIAN_POINT('Ctrl Pts',(30.5025155082578,-1.07350395293815,21.5969652482617));
#58998=CARTESIAN_POINT('Ctrl Pts',(30.2404480736925,-1.15671325182863,21.5779222161248));
#58999=CARTESIAN_POINT('Ctrl Pts',(30.1205093503255,-1.17524047358085,21.5699001988757));
#59000=CARTESIAN_POINT('Ctrl Pts',(29.9999999999996,-1.17524047358085,21.5625));
#59001=CARTESIAN_POINT('Ctrl Pts',(30.0000000000003,-1.17524047358085,21.5));
#59002=CARTESIAN_POINT('Ctrl Pts',(30.0212839202784,-1.17524047358085,21.5013069960338));
#59003=CARTESIAN_POINT('Ctrl Pts',(30.0425864419315,-1.17466229796956,21.5026356328208));
#59004=CARTESIAN_POINT('Ctrl Pts',(30.2139454930837,-1.16533366693515,21.5134891283695));
#59005=CARTESIAN_POINT('Ctrl Pts',(30.3610177391346,-1.12845915530085,21.523827832119));
#59006=CARTESIAN_POINT('Ctrl Pts',(30.6385696146112,-0.998891400827412,
21.5454653082446));
#59007=CARTESIAN_POINT('Ctrl Pts',(30.7654630357173,-0.905335035089088,
21.5565744608423));
#59008=CARTESIAN_POINT('Ctrl Pts',(30.9718229035628,-0.677897335355307,
21.5773100566854));
#59009=CARTESIAN_POINT('Ctrl Pts',(31.0507577571561,-0.547623084998762,
21.5861694304673));
#59010=CARTESIAN_POINT('Ctrl Pts',(31.1570604439752,-0.258809326298121,
21.6066484845527));
#59011=CARTESIAN_POINT('Ctrl Pts',(31.1812214838473,-0.102338491331391,
21.6177434360859));
#59012=CARTESIAN_POINT('Ctrl Pts',(31.1670292938221,0.204877234262332,21.6395273271632));
#59013=CARTESIAN_POINT('Ctrl Pts',(31.1311379778152,0.352813947812694,21.6500171458341));
#59014=CARTESIAN_POINT('Ctrl Pts',(31.0040616369159,0.629882761963365,21.6696633955718));
#59015=CARTESIAN_POINT('Ctrl Pts',(30.9130181373807,0.755846555951633,21.6790645983814));
#59016=CARTESIAN_POINT('Ctrl Pts',(30.6868446220844,0.966129203413541,21.7004086935125));
#59017=CARTESIAN_POINT('Ctrl Pts',(30.553735937256,1.0481102897547,21.711489124086));
#59018=CARTESIAN_POINT('Ctrl Pts',(30.2686762405413,1.15380487275931,21.7327412449065));
#59019=CARTESIAN_POINT('Ctrl Pts',(30.1202468756007,1.17853792824007,21.7424990119962));
#59020=CARTESIAN_POINT('Ctrl Pts',(29.8153503696085,1.17107054155024,21.7614867439455));
#59021=CARTESIAN_POINT('Ctrl Pts',(29.661826921183,1.13627251461424,21.7721479818837));
#59022=CARTESIAN_POINT('Ctrl Pts',(29.3799800833098,1.01003478165367,21.7939311399523));
#59023=CARTESIAN_POINT('Ctrl Pts',(29.253891997555,0.920828765085568,21.8048366026441));
#59024=CARTESIAN_POINT('Ctrl Pts',(29.0454103417907,0.701638656512355,21.8254100846196));
#59025=CARTESIAN_POINT('Ctrl Pts',(28.9640200854668,0.5746995746724,21.8342495048467));
#59026=CARTESIAN_POINT('Ctrl Pts',(28.8502724171258,0.289883112959693,21.8544451207025));
#59027=CARTESIAN_POINT('Ctrl Pts',(28.8218581810328,0.133683866085342,21.8655208147403));
#59028=CARTESIAN_POINT('Ctrl Pts',(28.8280094580603,-0.174601530686287,
21.8873805534988));
#59029=CARTESIAN_POINT('Ctrl Pts',(28.8601657562679,-0.323793761637004,
21.8979593977371));
#59030=CARTESIAN_POINT('Ctrl Pts',(28.9799119697649,-0.603297917389521,
21.9177783313962));
#59031=CARTESIAN_POINT('Ctrl Pts',(29.0669039974813,-0.730676428244075,
21.9269392883002));
#59032=CARTESIAN_POINT('Ctrl Pts',(29.2865672059309,-0.946735069741176,
21.9480883812055));
#59033=CARTESIAN_POINT('Ctrl Pts',(29.4177292577255,-1.03259356038437,21.9591867420451));
#59034=CARTESIAN_POINT('Ctrl Pts',(29.7004129009365,-1.14619538664958,21.98057329627));
#59035=CARTESIAN_POINT('Ctrl Pts',(29.8484560704769,-1.17497884076058,21.9906847639469));
#59036=CARTESIAN_POINT('Ctrl Pts',(29.9986381885534,-1.17523988185415,21.9999163533479));
#59037=CARTESIAN_POINT('Ctrl Pts',(29.9993191103818,-1.17524047358524,21.9999581881525));
#59038=CARTESIAN_POINT('Ctrl Pts',(30.0000000075681,-1.17524047358085,22.0000000004647));
#59039=CARTESIAN_POINT('Origin',(30.,-1.21864324187371E-14,15.78125));
#59040=CARTESIAN_POINT('',(30.,-1.17524047358085,22.5625));
#59041=CARTESIAN_POINT('',(29.9999999999999,-1.17524047358085,22.4999999999999));
#59042=CARTESIAN_POINT('',(30.,-1.17524047358085,15.78125));
#59043=CARTESIAN_POINT('Ctrl Pts',(30.,-1.17524047358085,22.5625));
#59044=CARTESIAN_POINT('Ctrl Pts',(29.9313687068489,-1.17524047358085,22.5582855119371));
#59045=CARTESIAN_POINT('Ctrl Pts',(29.8627268799626,-1.16923029327301,22.55385729367));
#59046=CARTESIAN_POINT('Ctrl Pts',(29.6405360439417,-1.12983827415446,22.5388164770024));
#59047=CARTESIAN_POINT('Ctrl Pts',(29.4932720438495,-1.07189657475161,22.5277190875488));
#59048=CARTESIAN_POINT('Ctrl Pts',(29.2351505504649,-0.904940984815958,
22.505949247503));
#59049=CARTESIAN_POINT('Ctrl Pts',(29.125477326134,-0.799463570556349,22.4954749014128));
#59050=CARTESIAN_POINT('Ctrl Pts',(28.9500348086396,-0.550024618450246,
22.4758578415198));
#59051=CARTESIAN_POINT('Ctrl Pts',(28.8870166724079,-0.407722193677489,
22.4664105508506));
#59052=CARTESIAN_POINT('Ctrl Pts',(28.8193863135494,-0.106256134735224,
22.4450343541119));
#59053=CARTESIAN_POINT('Ctrl Pts',(28.8156683957017,0.0499559751614321,
22.4339577479897));
#59054=CARTESIAN_POINT('Ctrl Pts',(28.8680054797788,0.349324836623415,22.4127302582268));
#59055=CARTESIAN_POINT('Ctrl Pts',(28.9214162690158,0.489956671932254,22.4030291896045));
#59056=CARTESIAN_POINT('Ctrl Pts',(29.0814696037689,0.749536525817022,22.3839976107609));
#59057=CARTESIAN_POINT('Ctrl Pts',(29.1888834831425,0.864620134172483,22.3733214303097));
#59058=CARTESIAN_POINT('Ctrl Pts',(29.4398862783311,1.04443640573476,22.3515327737366));
#59059=CARTESIAN_POINT('Ctrl Pts',(29.5804046735503,1.10838743829029,22.3406365628695));
#59060=CARTESIAN_POINT('Ctrl Pts',(29.874773559948,1.17808176091705,22.320089130129));
#59061=CARTESIAN_POINT('Ctrl Pts',(30.0254999210416,1.18444262102585,22.3112603596819));
#59062=CARTESIAN_POINT('Ctrl Pts',(30.3288317944626,1.13918974891494,22.2910290715165));
#59063=CARTESIAN_POINT('Ctrl Pts',(30.4780087858284,1.08506931516396,22.2799496878662));
#59064=CARTESIAN_POINT('Ctrl Pts',(30.7411182596149,0.924538989516088,22.2581013471772));
#59065=CARTESIAN_POINT('Ctrl Pts',(30.8537656083098,0.82166305580017,22.2475365992352));
#59066=CARTESIAN_POINT('Ctrl Pts',(31.0350106463268,0.577368135111118,22.2277455951917));
#59067=CARTESIAN_POINT('Ctrl Pts',(31.1013006049905,0.437889260334813,22.2185496213456));
#59068=CARTESIAN_POINT('Ctrl Pts',(31.1772437890897,0.139172903087767,22.1973683990083));
#59069=CARTESIAN_POINT('Ctrl Pts',(31.185313349087,-0.0173128950364053,
22.1862723863453));
#59070=CARTESIAN_POINT('Ctrl Pts',(31.1410279217834,-0.318736522964712,
22.1648991982826));
#59071=CARTESIAN_POINT('Ctrl Pts',(31.0912903592309,-0.461049327500964,
22.1548343474741));
#59072=CARTESIAN_POINT('Ctrl Pts',(30.9380306919572,-0.724977765907907,
22.136065778375));
#59073=CARTESIAN_POINT('Ctrl Pts',(30.8337205687989,-0.842838844072579,
22.1254817206889));
#59074=CARTESIAN_POINT('Ctrl Pts',(30.5872857957992,-1.02946130111843,22.1037322710222));
#59075=CARTESIAN_POINT('Ctrl Pts',(30.4481174203718,-1.09722011431045,22.0927839616769));
#59076=CARTESIAN_POINT('Ctrl Pts',(30.2017882631029,-1.16222172164091,22.0753529112466));
#59077=CARTESIAN_POINT('Ctrl Pts',(30.1010204315162,-1.17524047358085,22.0687034297066));
#59078=CARTESIAN_POINT('Ctrl Pts',(29.9999999999997,-1.17524047358085,22.0625));
#59079=CARTESIAN_POINT('Ctrl Pts',(30.0000000075681,-1.17524047358085,22.0000000004647));
#59080=CARTESIAN_POINT('Ctrl Pts',(30.1550617076756,-1.17524047258231,22.0095219788006));
#59081=CARTESIAN_POINT('Ctrl Pts',(30.3087125624576,-1.14455036320512,22.020045399438));
#59082=CARTESIAN_POINT('Ctrl Pts',(30.5936146237504,-1.02583437646268,22.0417494976575));
#59083=CARTESIAN_POINT('Ctrl Pts',(30.7222919834293,-0.9396884903777,22.0527054685765));
#59084=CARTESIAN_POINT('Ctrl Pts',(30.9363028934711,-0.725796874489648,
22.0734306378289));
#59085=CARTESIAN_POINT('Ctrl Pts',(31.0207456221836,-0.60126080890756,22.0823661148205));
#59086=CARTESIAN_POINT('Ctrl Pts',(31.1412832329984,-0.320931550152795,
22.1022435544492));
#59087=CARTESIAN_POINT('Ctrl Pts',(31.1737467539974,-0.166807893544759,
22.1131720736242));
#59088=CARTESIAN_POINT('Ctrl Pts',(31.1765934878998,0.140728845238564,22.1349787269359));
#59089=CARTESIAN_POINT('Ctrl Pts',(31.148646481366,0.291209583454888,22.1456489359696));
#59090=CARTESIAN_POINT('Ctrl Pts',(31.0370532707971,0.573358102978206,22.165655374784));
#59091=CARTESIAN_POINT('Ctrl Pts',(30.9544609034821,0.702301510156061,22.1746213225474));
#59092=CARTESIAN_POINT('Ctrl Pts',(30.7420042686145,0.924591934894812,22.1955488165371));
#59093=CARTESIAN_POINT('Ctrl Pts',(30.6131073712558,1.01465868002552,22.2066572778597));
#59094=CARTESIAN_POINT('Ctrl Pts',(30.3331026676289,1.1369643062698,22.228187906872));
#59095=CARTESIAN_POINT('Ctrl Pts',(30.1855325771707,1.17014774287538,22.2384263196851));
#59096=CARTESIAN_POINT('Ctrl Pts',(29.8783465649041,1.17947691083341,22.2576206519922));
#59097=CARTESIAN_POINT('Ctrl Pts',(29.7215875906434,1.15260328305267,22.2678992314176));
#59098=CARTESIAN_POINT('Ctrl Pts',(29.4314038660401,1.03996407151785,22.2897122199048));
#59099=CARTESIAN_POINT('Ctrl Pts',(29.3003745517226,0.9567417174806,22.3007089687507));
#59100=CARTESIAN_POINT('Ctrl Pts',(29.0812311411824,0.747835374300097,22.3215725663721));
#59101=CARTESIAN_POINT('Ctrl Pts',(28.9939461402353,0.625488946274541,22.3306481587999));
#59102=CARTESIAN_POINT('Ctrl Pts',(28.866779072646,0.34832483100282,22.3503011660994));
#59103=CARTESIAN_POINT('Ctrl Pts',(28.8306169080572,0.195045951299282,22.3611697842779));
#59104=CARTESIAN_POINT('Ctrl Pts',(28.8203429359976,-0.112665031360941,
22.3829887927828));
#59105=CARTESIAN_POINT('Ctrl Pts',(28.844778193878,-0.264121048518041,22.3937281563827));
#59106=CARTESIAN_POINT('Ctrl Pts',(28.9496447173484,-0.548400594969454,
22.4138857009336));
#59107=CARTESIAN_POINT('Ctrl Pts',(29.0286885091485,-0.678634752036216,
22.4227474921567));
#59108=CARTESIAN_POINT('Ctrl Pts',(29.2352313232766,-0.905919594975383,
22.4434889029608));
#59109=CARTESIAN_POINT('Ctrl Pts',(29.3621859947411,-0.999372204838993,
22.454598138267));
#59110=CARTESIAN_POINT('Ctrl Pts',(29.6398139077013,-1.12872343697434,22.4762326071516));
#59111=CARTESIAN_POINT('Ctrl Pts',(29.7869023742936,-1.1654876328242,22.4865683958599));
#59112=CARTESIAN_POINT('Ctrl Pts',(29.9579757834663,-1.17467745886044,22.4973994296432));
#59113=CARTESIAN_POINT('Ctrl Pts',(29.9789969929607,-1.17524047358085,22.4987102541947));
#59114=CARTESIAN_POINT('Ctrl Pts',(29.9999999999997,-1.17524047358085,22.4999999999999));
#59115=CARTESIAN_POINT('Origin',(30.,-1.21864324187371E-14,15.78125));
#59116=CARTESIAN_POINT('',(30.,-1.17524047358085,23.0625));
#59117=CARTESIAN_POINT('',(29.9999999999997,-1.17524047358085,22.9999999999999));
#59118=CARTESIAN_POINT('',(30.,-1.17524047358085,15.78125));
#59119=CARTESIAN_POINT('Ctrl Pts',(30.0000000000001,-1.17524047358085,23.0625));
#59120=CARTESIAN_POINT('Ctrl Pts',(29.9105144759955,-1.17524047358086,23.0570049021313));
#59121=CARTESIAN_POINT('Ctrl Pts',(29.8211453329131,-1.16502438899623,23.0511547525684));
#59122=CARTESIAN_POINT('Ctrl Pts',(29.5817638222111,-1.10931034878277,23.0344796199141));
#59123=CARTESIAN_POINT('Ctrl Pts',(29.4384864599594,-1.04411918186912,23.0233700199021));
#59124=CARTESIAN_POINT('Ctrl Pts',(29.1904963016638,-0.865097093142698,
23.001794519102));
#59125=CARTESIAN_POINT('Ctrl Pts',(29.0867727283959,-0.754802905276228,
22.9915147546188));
#59126=CARTESIAN_POINT('Ctrl Pts',(28.9228010666229,-0.495400927229172,
22.9722488667908));
#59127=CARTESIAN_POINT('Ctrl Pts',(28.8663568012591,-0.347374707529959,
22.9621314630453));
#59128=CARTESIAN_POINT('Ctrl Pts',(28.8154245654916,-0.0407388679671123,
22.9403886902216));
#59129=CARTESIAN_POINT('Ctrl Pts',(28.820274444704,0.114581560721945,22.9293753109615));
#59130=CARTESIAN_POINT('Ctrl Pts',(28.8884563534747,0.409699470717337,22.9084492454292));
#59131=CARTESIAN_POINT('Ctrl Pts',(28.9492618301764,0.547097841052301,22.8992933904858));
#59132=CARTESIAN_POINT('Ctrl Pts',(29.1229462954904,0.797680554149997,22.8797437378863));
#59133=CARTESIAN_POINT('Ctrl Pts',(29.2364128570735,0.906879897838648,22.8689044954722));
#59134=CARTESIAN_POINT('Ctrl Pts',(29.4960880788397,1.07256979024568,22.8470841182882));
#59135=CARTESIAN_POINT('Ctrl Pts',(29.6390279331417,1.12873587584898,22.8363152167134));
#59136=CARTESIAN_POINT('Ctrl Pts',(29.9369514995214,1.18318311725145,22.8160900653519));
#59137=CARTESIAN_POINT('Ctrl Pts',(30.0889739777062,1.18151676550276,22.8072588330028));
#59138=CARTESIAN_POINT('Ctrl Pts',(30.3896701123462,1.11972025811827,22.7866028657307));
#59139=CARTESIAN_POINT('Ctrl Pts',(30.5349379950004,1.05803905954289,22.7754954739854));
#59140=CARTESIAN_POINT('Ctrl Pts',(30.7879462278465,0.88483838172195,22.7538182156715));
#59141=CARTESIAN_POINT('Ctrl Pts',(30.894602280459,0.776856295524231,22.7434403470977));
#59142=CARTESIAN_POINT('Ctrl Pts',(31.0642088755634,0.522314474535101,22.7240007418519));
#59143=CARTESIAN_POINT('Ctrl Pts',(31.1239021773863,0.377122301428262,22.7142407897863));
#59144=CARTESIAN_POINT('Ctrl Pts',(31.1830807507881,0.07297978420699,22.6926748121518));
#59145=CARTESIAN_POINT('Ctrl Pts',(31.1824316194307,-0.0828368341019099,
22.681626249339));
#59146=CARTESIAN_POINT('Ctrl Pts',(31.1220212984731,-0.380073436416841,
22.6605499526862));
#59147=CARTESIAN_POINT('Ctrl Pts',(31.0648726782981,-0.5190454232441,22.6511559208149));
#59148=CARTESIAN_POINT('Ctrl Pts',(30.897916936256,-0.774116322820778,22.6318603404761));
#59149=CARTESIAN_POINT('Ctrl Pts',(30.7874073117601,-0.886271721025917,
22.6210978735108));
#59150=CARTESIAN_POINT('Ctrl Pts',(30.5319280571356,-1.05901132752472,22.5992852221989));
#59151=CARTESIAN_POINT('Ctrl Pts',(30.390134598554,-1.11904322637321,22.5884496605924));
#59152=CARTESIAN_POINT('Ctrl Pts',(30.1614293865023,-1.16692310230727,22.5727078850032));
#59153=CARTESIAN_POINT('Ctrl Pts',(30.0807402688424,-1.17524047358085,22.5674580720923));
#59154=CARTESIAN_POINT('Ctrl Pts',(30.,-1.17524047358085,22.5625));
#59155=CARTESIAN_POINT('Ctrl Pts',(29.9999999999997,-1.17524047358085,22.4999999999999));
#59156=CARTESIAN_POINT('Ctrl Pts',(30.1346907701741,-1.17524047358085,22.5082710468799));
#59157=CARTESIAN_POINT('Ctrl Pts',(30.2685335864829,-1.15209385827977,22.5173106568969));
#59158=CARTESIAN_POINT('Ctrl Pts',(30.5408486178537,-1.05471955701661,22.5374851723845));
#59159=CARTESIAN_POINT('Ctrl Pts',(30.6743758210798,-0.974766233245233,
22.5485194114384));
#59160=CARTESIAN_POINT('Ctrl Pts',(30.8991023951896,-0.771359157149707,
22.5695308885782));
#59161=CARTESIAN_POINT('Ctrl Pts',(30.9894938192057,-0.651353133995038,
22.5788141945814));
#59162=CARTESIAN_POINT('Ctrl Pts',(31.1237789969096,-0.377670022359416,
22.598220372706));
#59163=CARTESIAN_POINT('Ctrl Pts',(31.1639088895479,-0.225405854113982,
22.6090170402582));
#59164=CARTESIAN_POINT('Ctrl Pts',(31.1822136536976,0.0822897394418652,
22.6308349575606));
#59165=CARTESIAN_POINT('Ctrl Pts',(31.1616041653703,0.234707632570292,22.6416425253559));
#59166=CARTESIAN_POINT('Ctrl Pts',(31.0639996311159,0.521237294982461,22.6619596199458));
#59167=CARTESIAN_POINT('Ctrl Pts',(30.9887089758802,0.652868889710107,22.6707656569643));
#59168=CARTESIAN_POINT('Ctrl Pts',(30.7885136410845,0.885402585167096,22.6913033752648));
#59169=CARTESIAN_POINT('Ctrl Pts',(30.6637241461389,0.982420191755087,22.7024060445739));
#59170=CARTESIAN_POINT('Ctrl Pts',(30.38882091141,1.11923262290395,22.724137724694));
#59171=CARTESIAN_POINT('Ctrl Pts',(30.2423409189137,1.15980775171446,22.7345712602384));
#59172=CARTESIAN_POINT('Ctrl Pts',(29.9379463484727,1.1837522744206,22.75411234554));
#59173=CARTESIAN_POINT('Ctrl Pts',(29.7828414350779,1.1653244529442,22.7636867623073));
#59174=CARTESIAN_POINT('Ctrl Pts',(29.4887538037787,1.06944336967731,22.7851453423512));
#59175=CARTESIAN_POINT('Ctrl Pts',(29.3526850446683,0.993007607592932,22.7962109417328));
#59176=CARTESIAN_POINT('Ctrl Pts',(29.1221162292212,0.795444169323972,22.8173739985243));
#59177=CARTESIAN_POINT('Ctrl Pts',(29.0284526004007,0.677845266859518,22.8269357043589));
#59178=CARTESIAN_POINT('Ctrl Pts',(28.8868197290406,0.407843425299078,22.8460808529214));
#59179=CARTESIAN_POINT('Ctrl Pts',(28.8426042638403,0.256743916657897,22.8567949374029));
#59180=CARTESIAN_POINT('Ctrl Pts',(28.8159600292804,-0.0507119050410385,
22.8785958530886));
#59181=CARTESIAN_POINT('Ctrl Pts',(28.8325649861531,-0.204026768591548,
22.8894670227908));
#59182=CARTESIAN_POINT('Ctrl Pts',(28.9226310063267,-0.492841082076786,
22.9099461162173));
#59183=CARTESIAN_POINT('Ctrl Pts',(28.994102015515,-0.625925698199416,22.918754883105));
#59184=CARTESIAN_POINT('Ctrl Pts',(29.1877542901984,-0.863760919482141,
22.9390787662067));
#59185=CARTESIAN_POINT('Ctrl Pts',(29.3102272892874,-0.964377961033194,
22.9501667983144));
#59186=CARTESIAN_POINT('Ctrl Pts',(29.5821386201159,-1.10877008329771,22.9719834809511));
#59187=CARTESIAN_POINT('Ctrl Pts',(29.7278943046296,-1.1532370774207,22.9825105195965));
#59188=CARTESIAN_POINT('Ctrl Pts',(29.9186700556686,-1.17313232338821,22.9949309755051));
#59189=CARTESIAN_POINT('Ctrl Pts',(29.9593567068785,-1.17524047358085,22.9975041899134));
#59190=CARTESIAN_POINT('Ctrl Pts',(29.9999999999995,-1.17524047358085,22.9999999999999));
#59191=CARTESIAN_POINT('Origin',(30.,-1.21864324187371E-14,15.78125));
#59192=CARTESIAN_POINT('',(30.0000000000003,-1.17524047358085,23.5625));
#59193=CARTESIAN_POINT('',(30.,-1.17524047358085,23.5));
#59194=CARTESIAN_POINT('',(30.,-1.17524047358085,15.78125));
#59195=CARTESIAN_POINT('Ctrl Pts',(30.0000000000005,-1.17524047358085,23.5625));
#59196=CARTESIAN_POINT('Ctrl Pts',(29.8877180837681,-1.1752404735809,23.5556050287134));
#59197=CARTESIAN_POINT('Ctrl Pts',(29.7758372881673,-1.15915740880452,23.548164484563));
#59198=CARTESIAN_POINT('Ctrl Pts',(29.5190446425994,-1.08346545175016,23.5297118828087));
#59199=CARTESIAN_POINT('Ctrl Pts',(29.3805019669677,-1.01066023747548,23.5186230824555));
#59200=CARTESIAN_POINT('Ctrl Pts',(29.1440648218203,-0.81906365611398,23.4973112125635));
#59201=CARTESIAN_POINT('Ctrl Pts',(29.0470865676084,-0.703844960553528,
23.4874078682461));
#59202=CARTESIAN_POINT('Ctrl Pts',(28.8981724330839,-0.43757763652763,23.4685275248886));
#59203=CARTESIAN_POINT('Ctrl Pts',(28.8499251562346,-0.287749538271772,
23.4579035929059));
#59204=CARTESIAN_POINT('Ctrl Pts',(28.8149793372208,0.0192409990811535,
23.4361356693579));
#59205=CARTESIAN_POINT('Ctrl Pts',(28.8275655785823,0.173345465604893,23.4252085109033));
#59206=CARTESIAN_POINT('Ctrl Pts',(28.9101166290744,0.46437979734691,23.4045720015899));
#59207=CARTESIAN_POINT('Ctrl Pts',(28.9778580847147,0.598927911512345,23.3956997913279));
#59208=CARTESIAN_POINT('Ctrl Pts',(29.1650362747697,0.841899704480849,23.3755913560416));
#59209=CARTESIAN_POINT('Ctrl Pts',(29.2851376881026,0.945999066866448,23.3645254962114));
#59210=CARTESIAN_POINT('Ctrl Pts',(29.5539135664443,1.09777062977422,23.3426397256705));
#59211=CARTESIAN_POINT('Ctrl Pts',(29.6988585362439,1.14604691671332,23.3320274174642));
#59212=CARTESIAN_POINT('Ctrl Pts',(30.0001600354305,1.18508412542801,23.3121411783529));
#59213=CARTESIAN_POINT('Ctrl Pts',(30.1536625413848,1.17508243739145,23.3030583378086));
#59214=CARTESIAN_POINT('Ctrl Pts',(30.4512625228178,1.09622449574564,23.2819876064994));
#59215=CARTESIAN_POINT('Ctrl Pts',(30.592110439614,1.02700793469459,23.2708844778163));
#59216=CARTESIAN_POINT('Ctrl Pts',(30.8340714315268,0.841360319080231,23.2494443144111));
#59217=CARTESIAN_POINT('Ctrl Pts',(30.9343059293982,0.728463261371192,23.2392865244689));
#59218=CARTESIAN_POINT('Ctrl Pts',(31.0901832738534,0.465790392750319,23.2204017245443));
#59219=CARTESIAN_POINT('Ctrl Pts',(31.1423055420081,0.317257314781848,23.2099959148018));
#59220=CARTESIAN_POINT('Ctrl Pts',(31.1851773743111,0.010751647338072,23.1882623721543));
#59221=CARTESIAN_POINT('Ctrl Pts',(31.1764469607209,-0.144008319910697,
23.1772887337992));
#59222=CARTESIAN_POINT('Ctrl Pts',(31.1010701340243,-0.437108167734962,
23.1565057639579));
#59223=CARTESIAN_POINT('Ctrl Pts',(31.0368218842674,-0.573070176242618,
23.1475180074206));
#59224=CARTESIAN_POINT('Ctrl Pts',(30.8568360573785,-0.819362332337596,
23.1277335191445));
#59225=CARTESIAN_POINT('Ctrl Pts',(30.7406590361852,-0.925703986430565,
23.1168291494862));
#59226=CARTESIAN_POINT('Ctrl Pts',(30.477211273408,-1.08466164141258,23.0950157923094));
#59227=CARTESIAN_POINT('Ctrl Pts',(30.3332866239118,-1.13717003604433,23.0843160955662));
#59228=CARTESIAN_POINT('Ctrl Pts',(30.1225555529996,-1.17045159552602,23.0701956350453));
#59229=CARTESIAN_POINT('Ctrl Pts',(30.0612610274847,-1.17524047358085,23.066261897193));
#59230=CARTESIAN_POINT('Ctrl Pts',(30.0000000000001,-1.17524047358085,23.0625));
#59231=CARTESIAN_POINT('Ctrl Pts',(29.9999999999995,-1.17524047358085,22.9999999999999));
#59232=CARTESIAN_POINT('Ctrl Pts',(30.1122819160637,-1.17524047358085,23.0068949712763));
#59233=CARTESIAN_POINT('Ctrl Pts',(30.2241627114991,-1.15915740885253,23.0143355154149));
#59234=CARTESIAN_POINT('Ctrl Pts',(30.4809553569443,-1.08346545195345,23.0327881171562));
#59235=CARTESIAN_POINT('Ctrl Pts',(30.6194980326123,-1.01066023773368,23.0438769175097));
#59236=CARTESIAN_POINT('Ctrl Pts',(30.8559351778473,-0.819063656461988,
23.0651887874038));
#59237=CARTESIAN_POINT('Ctrl Pts',(30.952913432109,-0.703844960936813,23.0750921317269));
#59238=CARTESIAN_POINT('Ctrl Pts',(31.1018275667414,-0.437577636966923,
23.0939724750804));
#59239=CARTESIAN_POINT('Ctrl Pts',(31.1500748436503,-0.287749538730812,
23.1045964070617));
#59240=CARTESIAN_POINT('Ctrl Pts',(31.1850206627874,0.0192409986134863,
23.126364330609));
#59241=CARTESIAN_POINT('Ctrl Pts',(31.1724344214858,0.173345465148191,23.1372914890643));
#59242=CARTESIAN_POINT('Ctrl Pts',(31.0898833711054,0.464379796922714,23.15792799838));
#59243=CARTESIAN_POINT('Ctrl Pts',(31.0221419155201,0.598927911110121,23.1668002086434));
#59244=CARTESIAN_POINT('Ctrl Pts',(30.8349637255609,0.841899704153978,23.1869086439265));
#59245=CARTESIAN_POINT('Ctrl Pts',(30.7148623122637,0.945999066590532,23.1979745037564));
#59246=CARTESIAN_POINT('Ctrl Pts',(30.4460864339697,1.09777062960664,23.2198602742982));
#59247=CARTESIAN_POINT('Ctrl Pts',(30.3011414641827,1.1460469166018,23.2304725825058));
#59248=CARTESIAN_POINT('Ctrl Pts',(29.9998399650194,1.18508412542607,23.2503588216195));
#59249=CARTESIAN_POINT('Ctrl Pts',(29.8463374590763,1.17508243744973,23.2594416621611));
#59250=CARTESIAN_POINT('Ctrl Pts',(29.5487374776195,1.09622449592641,23.2805123934674));
#59251=CARTESIAN_POINT('Ctrl Pts',(29.4078895607902,1.02700793492841,23.2916155221506));
#59252=CARTESIAN_POINT('Ctrl Pts',(29.1659285687959,0.841360319401014,23.3130556855578));
#59253=CARTESIAN_POINT('Ctrl Pts',(29.0656940708777,0.72846326172594,23.3232134755017));
#59254=CARTESIAN_POINT('Ctrl Pts',(28.9098167263205,0.465790393157422,23.3420982754308));
#59255=CARTESIAN_POINT('Ctrl Pts',(28.8576944581104,0.317257315207477,23.3525040851682));
#59256=CARTESIAN_POINT('Ctrl Pts',(28.8148226256923,0.0107516477743395,
23.3742376278149));
#59257=CARTESIAN_POINT('Ctrl Pts',(28.8235530392262,-0.144008319483296,
23.3852112661707));
#59258=CARTESIAN_POINT('Ctrl Pts',(28.8989298658185,-0.437108167337535,
23.4059942360141));
#59259=CARTESIAN_POINT('Ctrl Pts',(28.9631781155251,-0.573070175865714,
23.4149819925535));
#59260=CARTESIAN_POINT('Ctrl Pts',(29.1431639423218,-0.819362332023802,
23.4347664808262));
#59261=CARTESIAN_POINT('Ctrl Pts',(29.2593409634759,-0.925703986159073,
23.4456708504836));
#59262=CARTESIAN_POINT('Ctrl Pts',(29.5227887261992,-1.08466164124026,23.4674842076606));
#59263=CARTESIAN_POINT('Ctrl Pts',(29.6667133756817,-1.13717003592563,23.4781839044047));
#59264=CARTESIAN_POINT('Ctrl Pts',(29.8774444467245,-1.17045159550418,23.4923043649371));
#59265=CARTESIAN_POINT('Ctrl Pts',(29.9387389723772,-1.17524047358085,23.4962381027985));
#59266=CARTESIAN_POINT('Ctrl Pts',(29.9999999999999,-1.17524047358085,23.5));
#59267=CARTESIAN_POINT('Origin',(30.,-1.21864324187371E-14,15.78125));
#59268=CARTESIAN_POINT('',(30.0000000000001,-1.17524047358085,24.0625));
#59269=CARTESIAN_POINT('',(30.,-1.17524047358085,24.));
#59270=CARTESIAN_POINT('',(30.,-1.17524047358085,15.78125));
#59271=CARTESIAN_POINT('Ctrl Pts',(30.0000000000002,-1.17524047358085,24.0625));
#59272=CARTESIAN_POINT('Ctrl Pts',(29.8653092296601,-1.17524047358088,24.0542289531099));
#59273=CARTESIAN_POINT('Ctrl Pts',(29.7314664131893,-1.15209385822287,24.045189343081));
#59274=CARTESIAN_POINT('Ctrl Pts',(29.4591513817099,-1.05471955679206,24.0250148275808));
#59275=CARTESIAN_POINT('Ctrl Pts',(29.3256241785221,-0.974766232969058,
24.0139805885274));
#59276=CARTESIAN_POINT('Ctrl Pts',(29.1008976044993,-0.771359156787199,
23.99296911139));
#59277=CARTESIAN_POINT('Ctrl Pts',(29.0105061805318,-0.651353133596405,
23.9836858053905));
#59278=CARTESIAN_POINT('Ctrl Pts',(28.876221002938,-0.377670021906335,23.9642796272619));
#59279=CARTESIAN_POINT('Ctrl Pts',(28.8360911103609,-0.225405853644338,
23.9534829597086));
#59280=CARTESIAN_POINT('Ctrl Pts',(28.8177863463358,0.0822897399134218,
23.931665042406));
#59281=CARTESIAN_POINT('Ctrl Pts',(28.8383958347227,0.234707633027682,23.9208574746117));
#59282=CARTESIAN_POINT('Ctrl Pts',(28.9360003690899,0.521237295405437,23.9005403800242));
#59283=CARTESIAN_POINT('Ctrl Pts',(29.0112910243832,0.652868890111379,23.8917343430053));
#59284=CARTESIAN_POINT('Ctrl Pts',(29.211486359277,0.885402585487968,23.8711966247017));
#59285=CARTESIAN_POINT('Ctrl Pts',(29.3362758542566,0.98242019202142,23.8600939553924));
#59286=CARTESIAN_POINT('Ctrl Pts',(29.611179089029,1.11923262305578,23.8383622752737));
#59287=CARTESIAN_POINT('Ctrl Pts',(29.7576590815354,1.15980775180767,23.8279287397307));
#59288=CARTESIAN_POINT('Ctrl Pts',(30.0620536519992,1.1837522743985,23.8083876544318));
#59289=CARTESIAN_POINT('Ctrl Pts',(30.2171585654068,1.16532445285658,23.7988132376599));
#59290=CARTESIAN_POINT('Ctrl Pts',(30.5112461966771,1.06944336945855,23.7773546576131));
#59291=CARTESIAN_POINT('Ctrl Pts',(30.6473149557494,0.993007607319778,23.7662890582319));
#59292=CARTESIAN_POINT('Ctrl Pts',(30.8778837711073,0.795444168961031,23.7451260014428));
#59293=CARTESIAN_POINT('Ctrl Pts',(30.9715473998777,0.67784526646015,23.735564295613));
#59294=CARTESIAN_POINT('Ctrl Pts',(31.1131802711266,0.407843424843195,23.7164191470464));
#59295=CARTESIAN_POINT('Ctrl Pts',(31.1573957362652,0.25674391618342,23.7057050625635));
#59296=CARTESIAN_POINT('Ctrl Pts',(31.1840399706984,-0.0507119055208601,
23.6839041468775));
#59297=CARTESIAN_POINT('Ctrl Pts',(31.1674350137646,-0.204026769058537,
23.6730329771762));
#59298=CARTESIAN_POINT('Ctrl Pts',(31.0773689934766,-0.492841082509219,
23.6525538837521));
#59299=CARTESIAN_POINT('Ctrl Pts',(31.0058979842309,-0.625925698609867,
23.643745116865));
#59300=CARTESIAN_POINT('Ctrl Pts',(30.8122457094484,-0.863760919813326,
23.62342123376));
#59301=CARTESIAN_POINT('Ctrl Pts',(30.6897727103237,-0.964377961310509,
23.612333201652));
#59302=CARTESIAN_POINT('Ctrl Pts',(30.4178613794486,-1.10877008346121,23.5905165190165));
#59303=CARTESIAN_POINT('Ctrl Pts',(30.2721056949232,-1.15323707752562,23.5799894803724));
#59304=CARTESIAN_POINT('Ctrl Pts',(30.081329944032,-1.17313232340388,23.5675690244761));
#59305=CARTESIAN_POINT('Ctrl Pts',(30.0406432929718,-1.17524047358083,23.5649958100773));
#59306=CARTESIAN_POINT('Ctrl Pts',(30.0000000000005,-1.17524047358085,23.5625));
#59307=CARTESIAN_POINT('Ctrl Pts',(29.9999999999999,-1.17524047358085,23.5));
#59308=CARTESIAN_POINT('Ctrl Pts',(30.0894855238544,-1.17524047358085,23.5054950978594));
#59309=CARTESIAN_POINT('Ctrl Pts',(30.178854666788,-1.16502438903023,23.5113452474122));
#59310=CARTESIAN_POINT('Ctrl Pts',(30.4182361773703,-1.10931034894115,23.5280203800546));
#59311=CARTESIAN_POINT('Ctrl Pts',(30.5615135396518,-1.04411918207875,23.5391299800668));
#59312=CARTESIAN_POINT('Ctrl Pts',(30.8095036980223,-0.865097093436967,
23.5607054808684));
#59313=CARTESIAN_POINT('Ctrl Pts',(30.9132272713337,-0.75480290560396,23.5709852453531));
#59314=CARTESIAN_POINT('Ctrl Pts',(31.0771989331901,-0.495400927628404,
23.5902511331837));
#59315=CARTESIAN_POINT('Ctrl Pts',(31.1336431986023,-0.347374707971562,
23.6003685369235));
#59316=CARTESIAN_POINT('Ctrl Pts',(31.1845754344926,-0.0407388684447008,
23.6221113097446));
#59317=CARTESIAN_POINT('Ctrl Pts',(31.1797255553422,0.114581560252514,23.6331246890053));
#59318=CARTESIAN_POINT('Ctrl Pts',(31.1115436466863,0.409699470279596,23.6540507545398));
#59319=CARTESIAN_POINT('Ctrl Pts',(31.0507381700391,0.547097840637693,23.6632066094863));
#59320=CARTESIAN_POINT('Ctrl Pts',(30.877053704825,0.797680553802843,23.6827562620821));
#59321=CARTESIAN_POINT('Ctrl Pts',(30.7635871432854,0.906879897536129,23.6935955044951));
#59322=CARTESIAN_POINT('Ctrl Pts',(30.5039119215803,1.07256979004896,23.7154158816792));
#59323=CARTESIAN_POINT('Ctrl Pts',(30.3609720672946,1.12873587571,23.726184783255));
#59324=CARTESIAN_POINT('Ctrl Pts',(30.0630485009405,1.18318311722529,23.7464099346189));
#59325=CARTESIAN_POINT('Ctrl Pts',(29.9110260227659,1.18151676553675,23.755241166967));
#59326=CARTESIAN_POINT('Ctrl Pts',(29.6103298881048,1.1197202582759,23.7758971342361));
#59327=CARTESIAN_POINT('Ctrl Pts',(29.46506200542,1.05803905975613,23.7870045259814));
#59328=CARTESIAN_POINT('Ctrl Pts',(29.2120537724961,0.884838382027716,23.8086817842968));
#59329=CARTESIAN_POINT('Ctrl Pts',(29.1053977198379,0.776856295866943,23.8190596528721));
#59330=CARTESIAN_POINT('Ctrl Pts',(28.9357911246459,0.52231447495466,23.8384992581206));
#59331=CARTESIAN_POINT('Ctrl Pts',(28.8760978227722,0.377122301892393,23.8482592101808));
#59332=CARTESIAN_POINT('Ctrl Pts',(28.816919249242,0.0729797847098555,23.8698251878126));
#59333=CARTESIAN_POINT('Ctrl Pts',(28.8175683805337,-0.0828368336059415,
23.8808737506258));
#59334=CARTESIAN_POINT('Ctrl Pts',(28.8779787013698,-0.380073435953635,
23.9019500472809));
#59335=CARTESIAN_POINT('Ctrl Pts',(28.9351273214881,-0.519045422805617,
23.9113440791565));
#59336=CARTESIAN_POINT('Ctrl Pts',(29.1020830634255,-0.774116322451291,
23.9306396594913));
#59337=CARTESIAN_POINT('Ctrl Pts',(29.212592687875,-0.88627172070161,23.9414021264554));
#59338=CARTESIAN_POINT('Ctrl Pts',(29.4680719424329,-1.05901132730886,23.963214777767));
#59339=CARTESIAN_POINT('Ctrl Pts',(29.609865400996,-1.11904322621712,23.9740503393744));
#59340=CARTESIAN_POINT('Ctrl Pts',(29.8385706131875,-1.1669231022752,23.9897921149766));
#59341=CARTESIAN_POINT('Ctrl Pts',(29.9192597310019,-1.17524047358085,23.9950419278981));
#59342=CARTESIAN_POINT('Ctrl Pts',(30.,-1.17524047358085,24.));
#59343=CARTESIAN_POINT('Origin',(30.,-1.21864324187371E-14,15.78125));
#59344=CARTESIAN_POINT('',(29.9999999962159,-1.17524047358085,24.5624999995353));
#59345=CARTESIAN_POINT('',(30.0000000000002,-1.17524047358085,24.5));
#59346=CARTESIAN_POINT('',(30.,-1.17524047358085,15.78125));
#59347=CARTESIAN_POINT('Ctrl Pts',(29.9999999924319,-1.17524047358085,24.5624999995353));
#59348=CARTESIAN_POINT('Ctrl Pts',(29.8449382921852,-1.17524047258231,24.5529780211908));
#59349=CARTESIAN_POINT('Ctrl Pts',(29.6912874372683,-1.14455036315003,24.5424546005433));
#59350=CARTESIAN_POINT('Ctrl Pts',(29.4063853758944,-1.0258343762565,24.5207505023134));
#59351=CARTESIAN_POINT('Ctrl Pts',(29.2777080162496,-0.939688490130196,
24.5097945313951));
#59352=CARTESIAN_POINT('Ctrl Pts',(29.0636971062813,-0.72579687417109,24.4890693621447));
#59353=CARTESIAN_POINT('Ctrl Pts',(28.9792543776096,-0.601260808557374,
24.4801338851547));
#59354=CARTESIAN_POINT('Ctrl Pts',(28.8587167668904,-0.3209315497576,24.4602564455228));
#59355=CARTESIAN_POINT('Ctrl Pts',(28.8262532459446,-0.166807893138082,
24.449327926347));
#59356=CARTESIAN_POINT('Ctrl Pts',(28.823406512149,0.140728845641508,24.4275212730356));
#59357=CARTESIAN_POINT('Ctrl Pts',(28.851353518733,0.291209583843224,24.4168510640028));
#59358=CARTESIAN_POINT('Ctrl Pts',(28.9629467293987,0.573358103335639,24.3968446251906));
#59359=CARTESIAN_POINT('Ctrl Pts',(29.0455390967654,0.702301510494977,24.3878786774254));
#59360=CARTESIAN_POINT('Ctrl Pts',(29.2579957317181,0.924591935160839,24.3669511834331));
#59361=CARTESIAN_POINT('Ctrl Pts',(29.3868926291043,1.01465868024229,24.3558427221105));
#59362=CARTESIAN_POINT('Ctrl Pts',(29.6668973327643,1.13696430638437,24.3343120930999));
#59363=CARTESIAN_POINT('Ctrl Pts',(29.8144674232288,1.17014774293813,24.3240736802882));
#59364=CARTESIAN_POINT('Ctrl Pts',(30.1216534355145,1.17947691079308,24.3048793479835));
#59365=CARTESIAN_POINT('Ctrl Pts',(30.2784124097871,1.15260328295164,24.2946007685524));
#59366=CARTESIAN_POINT('Ctrl Pts',(30.5685961343608,1.03996407129779,24.2727877800628));
#59367=CARTESIAN_POINT('Ctrl Pts',(30.6996254486415,0.956741717213513,24.2617910312175));
#59368=CARTESIAN_POINT('Ctrl Pts',(30.9187688591,0.747835373953449,24.2409274335984));
#59369=CARTESIAN_POINT('Ctrl Pts',(31.006053860002,0.625488945893405,24.2318518411732));
#59370=CARTESIAN_POINT('Ctrl Pts',(31.1332209274868,0.348324830571042,24.2121988338701));
#59371=CARTESIAN_POINT('Ctrl Pts',(31.1693830920172,0.195045950853365,24.2013302156905));
#59372=CARTESIAN_POINT('Ctrl Pts',(31.1796570639592,-0.112665031805443,
24.1795112071857));
#59373=CARTESIAN_POINT('Ctrl Pts',(31.1552218060231,-0.264121048947789,
24.1687718435869));
#59374=CARTESIAN_POINT('Ctrl Pts',(31.0503552824464,-0.548400595365726,
24.1486142990383));
#59375=CARTESIAN_POINT('Ctrl Pts',(30.9713114905908,-0.678634752411996,
24.1397525078141));
#59376=CARTESIAN_POINT('Ctrl Pts',(30.7647686763693,-0.905919595273436,
24.119011097007));
#59377=CARTESIAN_POINT('Ctrl Pts',(30.6378140048735,-0.999372205084128,
24.1079018617007));
#59378=CARTESIAN_POINT('Ctrl Pts',(30.3601860918747,-1.12872343710904,24.0862673928177));
#59379=CARTESIAN_POINT('Ctrl Pts',(30.2130976252741,-1.16548763290266,24.0759316041108));
#59380=CARTESIAN_POINT('Ctrl Pts',(30.042024216247,-1.17467745886824,24.065100570339));
#59381=CARTESIAN_POINT('Ctrl Pts',(30.021003006896,-1.17524047358085,24.0637897457965));
#59382=CARTESIAN_POINT('Ctrl Pts',(30.0000000000002,-1.17524047358085,24.0625));
#59383=CARTESIAN_POINT('Ctrl Pts',(30.,-1.17524047358085,24.));
#59384=CARTESIAN_POINT('Ctrl Pts',(30.068631292987,-1.17524047358085,24.0042144880528));
#59385=CARTESIAN_POINT('Ctrl Pts',(30.1372731197099,-1.16923029330172,24.0086427063088));
#59386=CARTESIAN_POINT('Ctrl Pts',(30.3594639555913,-1.12983827430394,24.0236835229636));
#59387=CARTESIAN_POINT('Ctrl Pts',(30.5067279557135,-1.07189657495913,24.034780912417));
#59388=CARTESIAN_POINT('Ctrl Pts',(30.7648494491756,-0.904940985120749,
24.0565507524641));
#59389=CARTESIAN_POINT('Ctrl Pts',(30.8745226735525,-0.799463570900332,
24.0670250985558));
#59390=CARTESIAN_POINT('Ctrl Pts',(31.0499651911362,-0.550024618872908,
24.0866421584515));
#59391=CARTESIAN_POINT('Ctrl Pts',(31.1129833274185,-0.407722194144101,
24.0960894491163));
#59392=CARTESIAN_POINT('Ctrl Pts',(31.1806136864057,-0.106256135243321,
24.117465645852));
#59393=CARTESIAN_POINT('Ctrl Pts',(31.1843316043204,0.0499559746584703,
24.1285422519746));
#59394=CARTESIAN_POINT('Ctrl Pts',(31.131994520367,0.349324836152535,24.1497697417397));
#59395=CARTESIAN_POINT('Ctrl Pts',(31.0785837311869,0.489956671487056,24.1594708103671));
#59396=CARTESIAN_POINT('Ctrl Pts',(30.9185303965388,0.749536525439823,24.1785023892068));
#59397=CARTESIAN_POINT('Ctrl Pts',(30.8111165172128,0.864620133839068,24.1891785696567));
#59398=CARTESIAN_POINT('Ctrl Pts',(30.5601137220937,1.04443640550787,24.2109672262292));
#59399=CARTESIAN_POINT('Ctrl Pts',(30.4195953268947,1.10838743812269,24.2218634370972));
#59400=CARTESIAN_POINT('Ctrl Pts',(30.125226440525,1.17808176086598,24.2424108698401));
#59401=CARTESIAN_POINT('Ctrl Pts',(29.9745000794406,1.18444262103543,24.2512396402881));
#59402=CARTESIAN_POINT('Ctrl Pts',(29.671168206001,1.13918974904968,24.2714709284502));
#59403=CARTESIAN_POINT('Ctrl Pts',(29.5219912146071,1.08506931535676,24.2825503121002));
#59404=CARTESIAN_POINT('Ctrl Pts',(29.2588817407465,0.924538989806815,24.3043986527903));
#59405=CARTESIAN_POINT('Ctrl Pts',(29.1462343920073,0.821663056130735,24.3149634007337));
#59406=CARTESIAN_POINT('Ctrl Pts',(28.9649893539032,0.577368135519195,24.3347544047798));
#59407=CARTESIAN_POINT('Ctrl Pts',(28.8986993951907,0.437889260784583,24.3439503786226));
#59408=CARTESIAN_POINT('Ctrl Pts',(28.8227562109677,0.139172903579825,24.3651316009568));
#59409=CARTESIAN_POINT('Ctrl Pts',(28.814686650905,-0.0173128945475468,
24.3762276136201));
#59410=CARTESIAN_POINT('Ctrl Pts',(28.8589720780878,-0.318736522506238,
24.3976008016849));
#59411=CARTESIAN_POINT('Ctrl Pts',(28.9087096405855,-0.46104932706788,24.4076656524993));
#59412=CARTESIAN_POINT('Ctrl Pts',(29.0619693077579,-0.724977765539007,
24.4264342215945));
#59413=CARTESIAN_POINT('Ctrl Pts',(29.1662794308695,-0.84283884374432,24.4370182792792));
#59414=CARTESIAN_POINT('Ctrl Pts',(29.4127142037999,-1.0294613008905,24.4587677289451));
#59415=CARTESIAN_POINT('Ctrl Pts',(29.5518825792064,-1.09722011413893,24.4697160382912));
#59416=CARTESIAN_POINT('Ctrl Pts',(29.7982117366005,-1.1622217216024,24.4871470887339));
#59417=CARTESIAN_POINT('Ctrl Pts',(29.8989795683345,-1.17524047358088,24.4937965702842));
#59418=CARTESIAN_POINT('Ctrl Pts',(30.0000000000003,-1.17524047358085,24.5));
#59419=CARTESIAN_POINT('Origin',(30.,-1.21864324187371E-14,15.78125));
#59420=CARTESIAN_POINT('',(29.9999999999999,-1.17524047358085,25.0625));
#59421=CARTESIAN_POINT('',(30.0000000000002,-1.17524047358085,25.));
#59422=CARTESIAN_POINT('',(30.,-1.17524047358085,15.78125));
#59423=CARTESIAN_POINT('Ctrl Pts',(29.9999999999998,-1.17524047358085,25.0625));
#59424=CARTESIAN_POINT('Ctrl Pts',(29.9787160795735,-1.17524047358085,25.0611930039571));
#59425=CARTESIAN_POINT('Ctrl Pts',(29.9574135577721,-1.17466229796152,25.0598643671606));
#59426=CARTESIAN_POINT('Ctrl Pts',(29.7860545064693,-1.16533366685381,25.0490108716001));
#59427=CARTESIAN_POINT('Ctrl Pts',(29.638982260427,-1.12845915516134,25.0386721678491));
#59428=CARTESIAN_POINT('Ctrl Pts',(29.3614303849904,-0.998891400573746,
25.0170346917219));
#59429=CARTESIAN_POINT('Ctrl Pts',(29.2345369639167,-0.905335034780717,
25.0059255391243));
#59430=CARTESIAN_POINT('Ctrl Pts',(29.0281770961676,-0.677897334966365,
24.9851899432843));
#59431=CARTESIAN_POINT('Ctrl Pts',(28.9492422426318,-0.547623084588669,
24.9763305695037));
#59432=CARTESIAN_POINT('Ctrl Pts',(28.8429395559285,-0.25880932586385,24.9558515154165));
#59433=CARTESIAN_POINT('Ctrl Pts',(28.8187785161156,-0.102338490894112,
24.9447565638831));
#59434=CARTESIAN_POINT('Ctrl Pts',(28.8329707062525,0.20487723468326,24.9229726728069));
#59435=CARTESIAN_POINT('Ctrl Pts',(28.8688620223111,0.352813948215486,24.9124828541373));
#59436=CARTESIAN_POINT('Ctrl Pts',(28.9959383633127,0.629882762331914,24.8928366044019));
#59437=CARTESIAN_POINT('Ctrl Pts',(29.0869818629053,0.755846556300386,24.8834354015886));
#59438=CARTESIAN_POINT('Ctrl Pts',(29.3131553782924,0.966129203680405,24.8620913064548));
#59439=CARTESIAN_POINT('Ctrl Pts',(29.4462640631474,1.04811028996687,24.8510108758816));
#59440=CARTESIAN_POINT('Ctrl Pts',(29.731323759893,1.1538048728599,24.8297587550632));
#59441=CARTESIAN_POINT('Ctrl Pts',(29.8797531248391,1.17853792828451,24.8200009879783));
#59442=CARTESIAN_POINT('Ctrl Pts',(30.1846496308258,1.17107054148177,24.8010132560253));
#59443=CARTESIAN_POINT('Ctrl Pts',(30.3381730792388,1.13627251448872,24.7903520180859));
#59444=CARTESIAN_POINT('Ctrl Pts',(30.6200199170605,1.01003478142549,24.7685688600169));
#59445=CARTESIAN_POINT('Ctrl Pts',(30.7461080027782,0.920828764814659,24.7576633973259));
#59446=CARTESIAN_POINT('Ctrl Pts',(30.954589658464,0.701638656166971,24.7370899153526));
#59447=CARTESIAN_POINT('Ctrl Pts',(31.0359799147447,0.574699574292555,24.7282504951265));
#59448=CARTESIAN_POINT('Ctrl Pts',(31.1497275829798,0.289883112537678,24.7080548792676));
#59449=CARTESIAN_POINT('Ctrl Pts',(31.1781418190148,0.133683865658838,24.6969791852295));
#59450=CARTESIAN_POINT('Ctrl Pts',(31.1719905418774,-0.174601531099527,
24.6751194464719));
#59451=CARTESIAN_POINT('Ctrl Pts',(31.1398342436188,-0.323793762033814,
24.6645406022347));
#59452=CARTESIAN_POINT('Ctrl Pts',(31.020088030022,-0.603297917753395,24.644721668578));
#59453=CARTESIAN_POINT('Ctrl Pts',(30.9330960022514,-0.730676428588708,
24.6355607116713));
#59454=CARTESIAN_POINT('Ctrl Pts',(30.7134327937131,-0.946735070008641,
24.6144116187632));
#59455=CARTESIAN_POINT('Ctrl Pts',(30.5822707418913,-1.03259356059966,24.6033132579239));
#59456=CARTESIAN_POINT('Ctrl Pts',(30.299587098649,-1.14619538675731,24.5819267037008));
#59457=CARTESIAN_POINT('Ctrl Pts',(30.1515439291036,-1.17497884081411,24.5718152360255));
#59458=CARTESIAN_POINT('Ctrl Pts',(30.0013618111703,-1.17523988185447,24.5625836466351));
#59459=CARTESIAN_POINT('Ctrl Pts',(30.0006808894801,-1.17524047358524,24.5625418118389));
#59460=CARTESIAN_POINT('Ctrl Pts',(29.9999999924319,-1.17524047358085,24.5624999995353));
#59461=CARTESIAN_POINT('Ctrl Pts',(30.0000000000003,-1.17524047358085,24.5));
#59462=CARTESIAN_POINT('Ctrl Pts',(30.0475989786694,-1.17524047358084,24.5029229425557));
#59463=CARTESIAN_POINT('Ctrl Pts',(30.0952413712801,-1.17234913261358,24.5059510599029));
#59464=CARTESIAN_POINT('Ctrl Pts',(30.2990650070911,-1.14742109537484,24.5193511873216));
#59465=CARTESIAN_POINT('Ctrl Pts',(30.4499960157575,-1.0970416910395,24.5304056476212));
#59466=CARTESIAN_POINT('Ctrl Pts',(30.7177665488108,-0.942842462676014,
24.5523157520592));
#59467=CARTESIAN_POINT('Ctrl Pts',(30.833223349596,-0.842552715174129,24.5629613319529));
#59468=CARTESIAN_POINT('Ctrl Pts',(31.0200068112404,-0.603233885310555,
24.5829160166926));
#59469=CARTESIAN_POINT('Ctrl Pts',(31.0893943876237,-0.466400998056969,
24.591928683353));
#59470=CARTESIAN_POINT('Ctrl Pts',(31.1731872619397,-0.170385863873932,
24.612918368786));
#59471=CARTESIAN_POINT('Ctrl Pts',(31.185412882504,-0.0137497619841131,
24.6240250391094));
#59472=CARTESIAN_POINT('Ctrl Pts',(31.1488612218191,0.289356743431089,24.6455175557638));
#59473=CARTESIAN_POINT('Ctrl Pts',(31.1026857517696,0.433263084173784,24.6557215908795));
#59474=CARTESIAN_POINT('Ctrl Pts',(30.9558437041525,0.701308793163264,24.6747280350226));
#59475=CARTESIAN_POINT('Ctrl Pts',(30.8545058913013,0.821789237632239,24.6849956137961));
#59476=CARTESIAN_POINT('Ctrl Pts',(30.6123622815668,1.01480099766359,24.7067080777764));
#59477=CARTESIAN_POINT('Ctrl Pts',(30.4745499588497,1.08610079838188,24.7176986563197));
#59478=CARTESIAN_POINT('Ctrl Pts',(30.1837738406509,1.17031056558872,24.7385400922772));
#59479=CARTESIAN_POINT('Ctrl Pts',(30.0341022035471,1.18415559329136,24.7475897886987));
#59480=CARTESIAN_POINT('Ctrl Pts',(29.7305751526436,1.15452627151871,24.7672791490145));
#59481=CARTESIAN_POINT('Ctrl Pts',(29.5799242663497,1.10861951554252,24.7781578355522));
#59482=CARTESIAN_POINT('Ctrl Pts',(29.3089128663366,0.962634653740643,24.7999757240996));
#59483=CARTESIAN_POINT('Ctrl Pts',(29.1903801371545,0.865330006275208,24.8107043566494));
#59484=CARTESIAN_POINT('Ctrl Pts',(28.9974547059893,0.631606479932577,24.8308378310304));
#59485=CARTESIAN_POINT('Ctrl Pts',(28.9246531642855,0.497649505166107,24.8397129306474));
#59486=CARTESIAN_POINT('Ctrl Pts',(28.8322520407485,0.204711362593916,24.8604844343777));
#59487=CARTESIAN_POINT('Ctrl Pts',(28.8154219514347,0.0480344797090969,
24.8715939963785));
#59488=CARTESIAN_POINT('Ctrl Pts',(28.8433837526351,-0.256851307347509,
24.8932126773996));
#59489=CARTESIAN_POINT('Ctrl Pts',(28.8856263759144,-0.402401296034548,
24.9035332594392));
#59490=CARTESIAN_POINT('Ctrl Pts',(29.0254132564532,-0.675115053553108,
24.9228707031121));
#59491=CARTESIAN_POINT('Ctrl Pts',(29.1237053106631,-0.798585223889617,
24.932834945393));
#59492=CARTESIAN_POINT('Ctrl Pts',(29.3612206915393,-0.998444700238917,
24.9545059777387));
#59493=CARTESIAN_POINT('Ctrl Pts',(29.4974844913312,-1.07350395274647,24.9655347517064));
#59494=CARTESIAN_POINT('Ctrl Pts',(29.7595519260122,-1.15671325178265,24.9845777838555));
#59495=CARTESIAN_POINT('Ctrl Pts',(29.8794906495254,-1.17524047358089,24.9925998011151));
#59496=CARTESIAN_POINT('Ctrl Pts',(30.0000000000004,-1.17524047358085,25.));
#59497=CARTESIAN_POINT('Origin',(30.,-1.21864324187371E-14,15.78125));
#59498=CARTESIAN_POINT('',(29.9999999999997,-1.17524047358085,25.5625));
#59499=CARTESIAN_POINT('',(30.,-1.17524047358085,25.5));
#59500=CARTESIAN_POINT('',(30.,-1.17524047358085,15.78125));
#59501=CARTESIAN_POINT('Ctrl Pts',(29.9999999999995,-1.17524047358085,25.5625));
#59502=CARTESIAN_POINT('Ctrl Pts',(29.9590631434842,-1.17524047358085,25.5599861628683));
#59503=CARTESIAN_POINT('Ctrl Pts',(29.9180826982373,-1.17310176284205,25.557393823766));
#59504=CARTESIAN_POINT('Ctrl Pts',(29.7270170759755,-1.15303120939534,25.5449493522346));
#59505=CARTESIAN_POINT('Ctrl Pts',(29.5812843667667,-1.10844931412058,25.534419650774));
#59506=CARTESIAN_POINT('Ctrl Pts',(29.3094646041477,-0.963834030512161,
25.5126006792245));
#59507=CARTESIAN_POINT('Ctrl Pts',(29.1870616253517,-0.863111358786919,
25.5015132019157));
#59508=CARTESIAN_POINT('Ctrl Pts',(28.9936035835609,-0.625120486304078,
25.4811957277874));
#59509=CARTESIAN_POINT('Ctrl Pts',(28.922245153506,-0.491992360156719,25.4723859354899));
#59510=CARTESIAN_POINT('Ctrl Pts',(28.8324037582581,-0.203110856662721,
25.4519020777895));
#59511=CARTESIAN_POINT('Ctrl Pts',(28.8159185655927,-0.0497708721110285,
25.4410291268206));
#59512=CARTESIAN_POINT('Ctrl Pts',(28.8428111724951,0.257674311776114,25.4192289654353));
#59513=CARTESIAN_POINT('Ctrl Pts',(28.8871477746036,0.408737403201897,25.4085174632064));
#59514=CARTESIAN_POINT('Ctrl Pts',(29.028998912458,0.678628541452795,25.389380164336));
#59515=CARTESIAN_POINT('Ctrl Pts',(29.1227608288482,0.796156039557689,25.3798091767006));
#59516=CARTESIAN_POINT('Ctrl Pts',(29.3535044180399,0.99354320653279,25.3586416369362));
#59517=CARTESIAN_POINT('Ctrl Pts',(29.4896480206548,1.06987223772086,25.3475752255981));
#59518=CARTESIAN_POINT('Ctrl Pts',(29.7837920452496,1.16549604577304,25.326122303941));
#59519=CARTESIAN_POINT('Ctrl Pts',(29.9388720345248,1.18379547475176,25.3165570329261));
#59520=CARTESIAN_POINT('Ctrl Pts',(30.243221825482,1.15962478745302,25.2970106790485));
#59521=CARTESIAN_POINT('Ctrl Pts',(30.3896819125524,1.11893466510606,25.2865742888993));
#59522=CARTESIAN_POINT('Ctrl Pts',(30.664499787972,0.981897695245122,25.2648398897594));
#59523=CARTESIAN_POINT('Ctrl Pts',(30.7892223684277,0.884773136061606,25.2537375376443));
#59524=CARTESIAN_POINT('Ctrl Pts',(30.9892253393634,0.652081932327525,25.233206047704));
#59525=CARTESIAN_POINT('Ctrl Pts',(31.0644029101032,0.520407945827758,25.2244008128923));
#59526=CARTESIAN_POINT('Ctrl Pts',(31.1617865735135,0.233810524226684,25.2040789136694));
#59527=CARTESIAN_POINT('Ctrl Pts',(31.1822791704619,0.0813648687854731,
25.1932693773186));
#59528=CARTESIAN_POINT('Ctrl Pts',(31.1637300195375,-0.226326940808914,
25.1714517283273));
#59529=CARTESIAN_POINT('Ctrl Pts',(31.1234798971667,-0.378558584977568,
25.1606573669753));
#59530=CARTESIAN_POINT('Ctrl Pts',(30.9889788141031,-0.652134792227603,
25.1412587691706));
#59531=CARTESIAN_POINT('Ctrl Pts',(30.8984922205339,-0.772069973056249,
25.1319682180917));
#59532=CARTESIAN_POINT('Ctrl Pts',(30.6735951228457,-0.975307798919531,
25.1109522700489));
#59533=CARTESIAN_POINT('Ctrl Pts',(30.5399926661631,-1.05515984400593,25.0999170005632));
#59534=CARTESIAN_POINT('Ctrl Pts',(30.2678908596704,-1.15220558793873,25.0797672273045));
#59535=CARTESIAN_POINT('Ctrl Pts',(30.1343655548317,-1.17524047358085,25.0707510761622));
#59536=CARTESIAN_POINT('Ctrl Pts',(29.9999999999998,-1.17524047358085,25.0625));
#59537=CARTESIAN_POINT('Ctrl Pts',(30.0000000000004,-1.17524047358085,25.));
#59538=CARTESIAN_POINT('Ctrl Pts',(30.0280011909949,-1.17524047358084,25.0017194880028));
#59539=CARTESIAN_POINT('Ctrl Pts',(30.056028863347,-1.17423978093536,25.0034760804581));
#59540=CARTESIAN_POINT('Ctrl Pts',(30.2395952618035,-1.16108096396762,25.0152149952129));
#59541=CARTESIAN_POINT('Ctrl Pts',(30.3913571022497,-1.11907669842983,25.0260235449911));
#59542=CARTESIAN_POINT('Ctrl Pts',(30.6663605367685,-0.979972388704826,
25.0478426338075));
#59543=CARTESIAN_POINT('Ctrl Pts',(30.7876235644496,-0.885461952247295,
25.0586398624147));
#59544=CARTESIAN_POINT('Ctrl Pts',(30.9860830879355,-0.656850945315206,
25.0789319146131));
#59545=CARTESIAN_POINT('Ctrl Pts',(31.0619486284351,-0.525431380274417,
25.0877429880603));
#59546=CARTESIAN_POINT('Ctrl Pts',(31.162019301378,-0.235334014571736,25.1083130594786));
#59547=CARTESIAN_POINT('Ctrl Pts',(31.182987818821,-0.0787326337506094,
25.1194172678187));
#59548=CARTESIAN_POINT('Ctrl Pts',(31.162785126869,0.227544173273347,25.1411345825519));
#59549=CARTESIAN_POINT('Ctrl Pts',(31.1241144207896,0.374476178584838,25.1515531598995));
#59550=CARTESIAN_POINT('Ctrl Pts',(30.9915168317796,0.649674032406111,25.1710667445663));
#59551=CARTESIAN_POINT('Ctrl Pts',(30.8973599492461,0.774562668596496,25.1806896874262));
#59552=CARTESIAN_POINT('Ctrl Pts',(30.6662666830193,0.980382528688255,25.202177670528));
#59553=CARTESIAN_POINT('Ctrl Pts',(30.531751815152,1.05938687434591,25.2132389149495));
#59554=CARTESIAN_POINT('Ctrl Pts',(30.2450331875533,1.15903498558282,25.2343785368368));
#59555=CARTESIAN_POINT('Ctrl Pts',(30.0962908441082,1.18072042198942,25.2438927186044));
#59556=CARTESIAN_POINT('Ctrl Pts',(29.7917163095273,1.16710140491111,25.2630787773242));
#59557=CARTESIAN_POINT('Ctrl Pts',(29.638905788045,1.12920096781154,25.2738062281113));
#59558=CARTESIAN_POINT('Ctrl Pts',(29.3599222216531,0.997398530499289,25.2956108489033));
#59559=CARTESIAN_POINT('Ctrl Pts',(29.2358774116296,0.905886016991888,25.3064726127214));
#59560=CARTESIAN_POINT('Ctrl Pts',(29.0316806530828,0.682639701770527,25.32692677681));
#59561=CARTESIAN_POINT('Ctrl Pts',(28.9526524211366,0.553805209269406,25.3357310715183));
#59562=CARTESIAN_POINT('Ctrl Pts',(28.844720062577,0.266708452558536,25.3560883773325));
#59563=CARTESIAN_POINT('Ctrl Pts',(28.8194808141697,0.110295910906438,25.3671791955642));
#59564=CARTESIAN_POINT('Ctrl Pts',(28.8316382042729,-0.197210560241239,
25.3889837026743));
#59565=CARTESIAN_POINT('Ctrl Pts',(28.8665861506279,-0.345474523822663,
25.3994967258182));
#59566=CARTESIAN_POINT('Ctrl Pts',(28.9918018301732,-0.623166741842213,
25.4191871795497));
#59567=CARTESIAN_POINT('Ctrl Pts',(29.081808144475,-0.749490769071139,25.4285215559887));
#59568=CARTESIAN_POINT('Ctrl Pts',(29.3063266217772,-0.961255466999539,
25.449816563314));
#59569=CARTESIAN_POINT('Ctrl Pts',(29.438949602445,-1.04422897408056,25.4609023529488));
#59570=CARTESIAN_POINT('Ctrl Pts',(29.7169259241077,-1.14948331999011,25.4817038921344));
#59571=CARTESIAN_POINT('Ctrl Pts',(29.8579333178884,-1.17524047358086,25.4912760155257));
#59572=CARTESIAN_POINT('Ctrl Pts',(30.,-1.17524047358085,25.5));
#59573=CARTESIAN_POINT('Origin',(30.,-1.21864324187371E-14,15.78125));
#59574=CARTESIAN_POINT('',(30.,-1.17524047358085,26.0625));
#59575=CARTESIAN_POINT('',(30.,-1.17524047358085,26.));
#59576=CARTESIAN_POINT('',(30.,-1.17524047358085,15.78125));
#59577=CARTESIAN_POINT('Ctrl Pts',(29.9999999999999,-1.17524047358085,26.0625));
#59578=CARTESIAN_POINT('Ctrl Pts',(29.9384679078155,-1.17524047358085,26.0587214573544));
#59579=CARTESIAN_POINT('Ctrl Pts',(29.8769029052424,-1.17040913172972,26.054769604635));
#59580=CARTESIAN_POINT('Ctrl Pts',(29.6659154234359,-1.13693724882076,26.0406266508408));
#59581=CARTESIAN_POINT('Ctrl Pts',(29.5220177711255,-1.084323597792,26.0299248801994));
#59582=CARTESIAN_POINT('Ctrl Pts',(29.2586759114222,-0.925171378535031,
26.0081111282534));
#59583=CARTESIAN_POINT('Ctrl Pts',(29.1425757110306,-0.818746672431791,
25.9972085314777));
#59584=CARTESIAN_POINT('Ctrl Pts',(28.9627703960609,-0.572330389052239,
25.9774307272425));
#59585=CARTESIAN_POINT('Ctrl Pts',(28.8986210699436,-0.436327710221708,
25.9684388957715));
#59586=CARTESIAN_POINT('Ctrl Pts',(28.8234492804003,-0.143169608738148,
25.9476517953103));
#59587=CARTESIAN_POINT('Ctrl Pts',(28.8148292891501,0.0116076754049962,
25.936676929058));
#59588=CARTESIAN_POINT('Ctrl Pts',(28.8579269079672,0.318093458602922,25.9149447963521));
#59589=CARTESIAN_POINT('Ctrl Pts',(28.910158206845,0.466589649123026,25.9045489692953));
#59590=CARTESIAN_POINT('Ctrl Pts',(29.0662354765119,0.729159361472922,25.8856555497038));
#59591=CARTESIAN_POINT('Ctrl Pts',(29.1665620010353,0.841989757161643,25.8754944720367));
#59592=CARTESIAN_POINT('Ctrl Pts',(29.4086828051808,1.02746666351878,25.8540505472151));
#59593=CARTESIAN_POINT('Ctrl Pts',(29.5495956219979,1.09657907822105,25.84294712555));
#59594=CARTESIAN_POINT('Ctrl Pts',(29.8472420936479,1.17519666348882,25.8218820609165));
#59595=CARTESIAN_POINT('Ctrl Pts',(30.000722767755,1.18508027808238,25.8128044743545));
#59596=CARTESIAN_POINT('Ctrl Pts',(30.3019786609575,1.14582802588677,25.7929134117055));
#59597=CARTESIAN_POINT('Ctrl Pts',(30.4468987068161,1.09744171612032,25.7822987333));
#59598=CARTESIAN_POINT('Ctrl Pts',(30.7155809567247,0.94545759821414,25.7604111763944));
#59599=CARTESIAN_POINT('Ctrl Pts',(30.835612326607,0.841258259962285,25.7493460732515));
#59600=CARTESIAN_POINT('Ctrl Pts',(31.0226024258984,0.598138792258194,25.7292439525602));
#59601=CARTESIAN_POINT('Ctrl Pts',(31.0902361983429,0.463547729361891,25.7203689985712));
#59602=CARTESIAN_POINT('Ctrl Pts',(31.1725680326408,0.172449502286477,25.6997279586011));
#59603=CARTESIAN_POINT('Ctrl Pts',(31.1850367066478,0.0183235805600113,
25.6887992788123));
#59604=CARTESIAN_POINT('Ctrl Pts',(31.149849032726,-0.288650006825612,25.6670325571437));
#59605=CARTESIAN_POINT('Ctrl Pts',(31.1014848231134,-0.438439388995189,
25.6564113704209));
#59606=CARTESIAN_POINT('Ctrl Pts',(30.9523589365019,-0.704596833564904,
25.637538818338));
#59607=CARTESIAN_POINT('Ctrl Pts',(30.8552831525205,-0.819746342004528,
25.6276245442916));
#59608=CARTESIAN_POINT('Ctrl Pts',(30.6186741800399,-1.01116668038418,25.6063083713552));
#59609=CARTESIAN_POINT('Ctrl Pts',(30.4800603026513,-1.08386414646939,25.5952190187437));
#59610=CARTESIAN_POINT('Ctrl Pts',(30.2235083443405,-1.15925176820215,25.5767919868584));
#59611=CARTESIAN_POINT('Ctrl Pts',(30.1119520742388,-1.17524047358085,25.5693747164571));
#59612=CARTESIAN_POINT('Ctrl Pts',(29.9999999999995,-1.17524047358085,25.5625));
#59613=CARTESIAN_POINT('Ctrl Pts',(30.,-1.17524047358085,25.5));
#59614=CARTESIAN_POINT('Ctrl Pts',(30.0069574643761,-1.17524047358085,25.5004272417029));
#59615=CARTESIAN_POINT('Ctrl Pts',(30.01391720466,-1.17517869098561,25.5008568135879));
#59616=CARTESIAN_POINT('Ctrl Pts',(30.1767683930213,-1.17228514742378,25.5109597131747));
#59617=CARTESIAN_POINT('Ctrl Pts',(30.3305146751184,-1.13852257214804,25.5215979241794));
#59618=CARTESIAN_POINT('Ctrl Pts',(30.613289571589,-1.01415059475931,25.5433719241602));
#59619=CARTESIAN_POINT('Ctrl Pts',(30.7400483172667,-0.925722033283128,
25.5542910068295));
#59620=CARTESIAN_POINT('Ctrl Pts',(30.9499509146168,-0.707886564918499,
25.5749037184647));
#59621=CARTESIAN_POINT('Ctrl Pts',(31.0321249523172,-0.581569550980178,
25.5837623721801));
#59622=CARTESIAN_POINT('Ctrl Pts',(31.1477905785375,-0.297516308572578,
25.6039038700829));
#59623=CARTESIAN_POINT('Ctrl Pts',(31.1772544504942,-0.141401249469257,
25.6149735945785));
#59624=CARTESIAN_POINT('Ctrl Pts',(31.1730934439483,0.167116297568546,25.636849794526));
#59625=CARTESIAN_POINT('Ctrl Pts',(31.1418645520009,0.316603789635784,25.6474495749843));
#59626=CARTESIAN_POINT('Ctrl Pts',(31.0239238826678,0.596699382032703,25.6673104459219));
#59627=CARTESIAN_POINT('Ctrl Pts',(30.9379157361151,0.724424917792123,25.6764216802641));
#59628=CARTESIAN_POINT('Ctrl Pts',(30.7198518445296,0.941880855114492,25.6975221021999));
#59629=CARTESIAN_POINT('Ctrl Pts',(30.5891826263813,1.02868094414498,25.7086235824532));
#59630=CARTESIAN_POINT('Ctrl Pts',(30.3070725150413,1.14422525077315,25.730043785608));
#59631=CARTESIAN_POINT('Ctrl Pts',(30.1591233913896,1.1739884490527,25.7401842137377));
#59632=CARTESIAN_POINT('Ctrl Pts',(29.8537619113516,1.17646530259176,25.7590235656117));
#59633=CARTESIAN_POINT('Ctrl Pts',(29.6991872299891,1.1467452303545,25.7694824753175));
#59634=CARTESIAN_POINT('Ctrl Pts',(29.4128145699134,1.02954198968741,25.7912232470859));
#59635=CARTESIAN_POINT('Ctrl Pts',(29.2835235645903,0.944145175996724,25.8021903431407));
#59636=CARTESIAN_POINT('Ctrl Pts',(29.0681842616351,0.731537563632497,25.8229515631887));
#59637=CARTESIAN_POINT('Ctrl Pts',(28.9830068906091,0.607571894150497,25.8319186117076));
#59638=CARTESIAN_POINT('Ctrl Pts',(28.8607454143127,0.328058458525624,25.851738203379));
#59639=CARTESIAN_POINT('Ctrl Pts',(28.8273201029076,0.174145192049772,25.8626518043211));
#59640=CARTESIAN_POINT('Ctrl Pts',(28.8225473943512,-0.133454152009573,
25.8844628968148));
#59641=CARTESIAN_POINT('Ctrl Pts',(28.849586199068,-0.284195707441678,25.8951515997385));
#59642=CARTESIAN_POINT('Ctrl Pts',(28.9594336647467,-0.566901683792667,
25.9151975664084));
#59643=CARTESIAN_POINT('Ctrl Pts',(29.0410981500453,-0.696179869303813,
25.9241315793102));
#59644=CARTESIAN_POINT('Ctrl Pts',(29.2520170527073,-0.919779045076863,
25.9450110448572));
#59645=CARTESIAN_POINT('Ctrl Pts',(29.3804160320669,-1.01073211613404,25.95612035376));
#59646=CARTESIAN_POINT('Ctrl Pts',(29.6598179734432,-1.13487834137248,25.9776792246572));
#59647=CARTESIAN_POINT('Ctrl Pts',(29.8072708469184,-1.1689955596726,25.9879435454987));
#59648=CARTESIAN_POINT('Ctrl Pts',(29.9714632607541,-1.17498080122199,25.9982384188692));
#59649=CARTESIAN_POINT('Ctrl Pts',(29.9857363066776,-1.17524047358085,25.9991240997731));
#59650=CARTESIAN_POINT('Ctrl Pts',(29.9999999999999,-1.17524047358085,26.));
#59651=CARTESIAN_POINT('Origin',(30.,-1.21864324187371E-14,15.78125));
#59652=CARTESIAN_POINT('',(30.,-1.17524047358085,26.5625));
#59653=CARTESIAN_POINT('',(29.9999999999997,-1.17524047358085,26.4999999999999));
#59654=CARTESIAN_POINT('',(30.,-1.17524047358085,15.78125));
#59655=CARTESIAN_POINT('Ctrl Pts',(30.,-1.17524047358085,26.5625));
#59656=CARTESIAN_POINT('Ctrl Pts',(29.9189538385986,-1.17524047358085,26.5575231437572));
#59657=CARTESIAN_POINT('Ctrl Pts',(29.8379609361797,-1.16685998242801,26.5522524382954));
#59658=CARTESIAN_POINT('Ctrl Pts',(29.6089811727034,-1.1187361642345,26.5364851544771));
#59659=CARTESIAN_POINT('Ctrl Pts',(29.4672242547403,-1.05858684051961,26.5256476735947));
#59660=CARTESIAN_POINT('Ctrl Pts',(29.2118758464994,-0.885634166979752,
26.5038355032321));
#59661=CARTESIAN_POINT('Ctrl Pts',(29.1014575353795,-0.773390023233997,
26.4930754972477));
#59662=CARTESIAN_POINT('Ctrl Pts',(28.9347073730369,-0.518183463481665,
26.4737877314199));
#59663=CARTESIAN_POINT('Ctrl Pts',(28.8776702380248,-0.379162720284378,
26.4643854707334));
#59664=CARTESIAN_POINT('Ctrl Pts',(28.8174988609875,-0.0818619971934983,
26.4433046274383));
#59665=CARTESIAN_POINT('Ctrl Pts',(28.8169789681977,0.0739680819649894,
26.4322551101507));
#59666=CARTESIAN_POINT('Ctrl Pts',(28.8764093680924,0.378032609649621,26.4106946625572));
#59667=CARTESIAN_POINT('Ctrl Pts',(28.9362017786302,0.523138441896699,26.4009448281074));
#59668=CARTESIAN_POINT('Ctrl Pts',(29.1059813583505,0.777530022962841,26.3814999268455));
#59669=CARTESIAN_POINT('Ctrl Pts',(29.2127271628307,0.885439479708375,26.3711191218038));
#59670=CARTESIAN_POINT('Ctrl Pts',(29.4658882417733,1.05845819806925,26.3494389287095));
#59671=CARTESIAN_POINT('Ctrl Pts',(29.6112162771377,1.12003007041528,26.3383317191495));
#59672=CARTESIAN_POINT('Ctrl Pts',(29.9119535931961,1.18158358217449,26.3176818381253));
#59673=CARTESIAN_POINT('Ctrl Pts',(30.0639561135899,1.18313176493728,26.308852379607));
#59674=CARTESIAN_POINT('Ctrl Pts',(30.3618294498414,1.12846284091072,26.2886224532834));
#59675=CARTESIAN_POINT('Ctrl Pts',(30.5047372110283,1.07218329091309,26.2778514997354));
#59676=CARTESIAN_POINT('Ctrl Pts',(30.7642923496518,0.906285517829887,26.2560311264309));
#59677=CARTESIAN_POINT('Ctrl Pts',(30.8776734787023,0.796998466194141,26.2451940206555));
#59678=CARTESIAN_POINT('Ctrl Pts',(31.0511614964728,0.546283376197254,26.2256517381869));
#59679=CARTESIAN_POINT('Ctrl Pts',(31.1118599586541,0.408839660981002,26.2164897876345));
#59680=CARTESIAN_POINT('Ctrl Pts',(31.179816298086,0.113659355972694,26.1955592978295));
#59681=CARTESIAN_POINT('Ctrl Pts',(31.1845443559052,-0.0416770721755796,
26.1845447840881));
#59682=CARTESIAN_POINT('Ctrl Pts',(31.1333712501869,-0.348241759846019,
26.1628070564654));
#59683=CARTESIAN_POINT('Ctrl Pts',(31.0768319553006,-0.496185033349922,
26.1527007984472));
#59684=CARTESIAN_POINT('Ctrl Pts',(30.9126965034022,-0.755446668894444,
26.1334298283147));
#59685=CARTESIAN_POINT('Ctrl Pts',(30.8088874743598,-0.865675121928193,
26.1231471467367));
#59686=CARTESIAN_POINT('Ctrl Pts',(30.5607504336079,-1.04453090463544,26.1015685223966));
#59687=CARTESIAN_POINT('Ctrl Pts',(30.4174143875892,-1.10962145980108,26.0904588858133));
#59688=CARTESIAN_POINT('Ctrl Pts',(30.1782678600435,-1.16509155074858,26.0738068318412));
#59689=CARTESIAN_POINT('Ctrl Pts',(30.0891908090061,-1.17524047358085,26.0679770001062));
#59690=CARTESIAN_POINT('Ctrl Pts',(29.9999999999999,-1.17524047358085,26.0625));
#59691=CARTESIAN_POINT('Ctrl Pts',(29.9999999999999,-1.17524047358085,26.));
#59692=CARTESIAN_POINT('Ctrl Pts',(30.1425333221801,-1.17524047358085,26.0087526397553));
#59693=CARTESIAN_POINT('Ctrl Pts',(30.2840219111895,-1.14931710997616,26.0183602049923));
#59694=CARTESIAN_POINT('Ctrl Pts',(30.561367295123,-1.04389937746679,26.0391287924253));
#59695=CARTESIAN_POINT('Ctrl Pts',(30.6930583893841,-0.961526015756511,
26.0501360796874));
#59696=CARTESIAN_POINT('Ctrl Pts',(30.9136669465422,-0.754054974126117,
26.0710387617507));
#59697=CARTESIAN_POINT('Ctrl Pts',(31.0017654739708,-0.632326756940585,
26.0801633069178));
#59698=CARTESIAN_POINT('Ctrl Pts',(31.130809796733,-0.356072448301099,26.0997518021271));
#59699=CARTESIAN_POINT('Ctrl Pts',(31.1680189550385,-0.20305033553964,26.1106022136104));
#59700=CARTESIAN_POINT('Ctrl Pts',(31.1804056537492,0.10467710494643,26.1324223890981));
#59701=CARTESIAN_POINT('Ctrl Pts',(31.1569739806732,0.256395498849484,26.1431803571703));
#59702=CARTESIAN_POINT('Ctrl Pts',(31.0540187102742,0.541272174052999,26.1633802426127));
#59703=CARTESIAN_POINT('Ctrl Pts',(30.9759701950171,0.671873752670431,26.1722217092774));
#59704=CARTESIAN_POINT('Ctrl Pts',(30.7711018756191,0.900554058237447,26.1929097676203));
#59705=CARTESIAN_POINT('Ctrl Pts',(30.6447103916025,0.994954099829424,26.2040180088908));
#59706=CARTESIAN_POINT('Ctrl Pts',(30.3677839906361,1.12628386016982,26.2256795457743));
#59707=CARTESIAN_POINT('Ctrl Pts',(30.2208469191431,1.16405670623833,26.2360417980814));
#59708=CARTESIAN_POINT('Ctrl Pts',(29.9153739917407,1.18247957177519,26.2554533393943));
#59709=CARTESIAN_POINT('Ctrl Pts',(29.7596534858204,1.16089584886057,26.265267690896));
#59710=CARTESIAN_POINT('Ctrl Pts',(29.4669798482834,1.05871377618554,26.2868628344935));
#59711=CARTESIAN_POINT('Ctrl Pts',(29.3327683310263,0.97968769950255,26.2979062213058));
#59712=CARTESIAN_POINT('Ctrl Pts',(29.1064857982236,0.777827856716442,26.3189583910466));
#59713=CARTESIAN_POINT('Ctrl Pts',(29.0152252755147,0.658466900754918,26.3283097753497));
#59714=CARTESIAN_POINT('Ctrl Pts',(28.8789732904358,0.385760488964649,26.3476466981555));
#59715=CARTESIAN_POINT('Ctrl Pts',(28.8377485021289,0.233796400613908,26.3584220878003));
#59716=CARTESIAN_POINT('Ctrl Pts',(28.8172159011814,-0.0738574561607104,
26.3802370456529));
#59717=CARTESIAN_POINT('Ctrl Pts',(28.8367587774233,-0.226525134118623,
26.3910623250595));
#59718=CARTESIAN_POINT('Ctrl Pts',(28.9323498389723,-0.513670658612161,
26.411423088874));
#59719=CARTESIAN_POINT('Ctrl Pts',(29.0066122735479,-0.645689070611162,
26.4202237943573));
#59720=CARTESIAN_POINT('Ctrl Pts',(29.2050554476303,-0.879653705731429,
26.4407046487027));
#59721=CARTESIAN_POINT('Ctrl Pts',(29.329232754846,-0.977642983590833,26.4518041743651));
#59722=CARTESIAN_POINT('Ctrl Pts',(29.6033526154654,-1.11649688151574,26.4735601269295));
#59723=CARTESIAN_POINT('Ctrl Pts',(29.7496481694863,-1.15811817689029,26.4840194270505));
#59724=CARTESIAN_POINT('Ctrl Pts',(29.9332052808561,-1.1738184735254,26.4958478764586));
#59725=CARTESIAN_POINT('Ctrl Pts',(29.9666204732331,-1.17524047358085,26.4979502409084));
#59726=CARTESIAN_POINT('Ctrl Pts',(29.9999999999995,-1.17524047358085,26.4999999999999));
#59727=CARTESIAN_POINT('Origin',(30.,-1.21864324187371E-14,15.78125));
#59728=CARTESIAN_POINT('',(30.0000000000002,-1.17524047358085,27.0625));
#59729=CARTESIAN_POINT('',(29.9999999999999,-1.17524047358085,26.9999999999999));
#59730=CARTESIAN_POINT('',(30.,-1.17524047358085,15.78125));
#59731=CARTESIAN_POINT('Ctrl Pts',(30.0000000000003,-1.17524047358085,27.0625));
#59732=CARTESIAN_POINT('Ctrl Pts',(29.898686590649,-1.17524047358088,27.0562785792061));
#59733=CARTESIAN_POINT('Ctrl Pts',(29.7976296484377,-1.16214610940709,27.0496086633191));
#59734=CARTESIAN_POINT('Ctrl Pts',(29.5510548806291,-1.0968832857528,27.032153269422));
#59735=CARTESIAN_POINT('Ctrl Pts',(29.4119274187945,-1.02901377051944,27.0212035476842));
#59736=CARTESIAN_POINT('Ctrl Pts',(29.1656287201027,-0.842194481232163,
26.9994554755857));
#59737=CARTESIAN_POINT('Ctrl Pts',(29.0614102622354,-0.72425366568988,26.9888742198639));
#59738=CARTESIAN_POINT('Ctrl Pts',(28.9083494936521,-0.460199204673261,
26.9701133966982));
#59739=CARTESIAN_POINT('Ctrl Pts',(28.8587194637877,-0.317836463591476,
26.960036980781));
#59740=CARTESIAN_POINT('Ctrl Pts',(28.8146713989512,-0.0163533730831442,
26.9386595763769));
#59741=CARTESIAN_POINT('Ctrl Pts',(28.8228691179041,0.140138676728786,26.9275631204225));
#59742=CARTESIAN_POINT('Ctrl Pts',(28.8990556060477,0.438772825908234,26.9063877272517));
#59743=CARTESIAN_POINT('Ctrl Pts',(28.9654414239268,0.578169376458166,26.8971982372258));
#59744=CARTESIAN_POINT('Ctrl Pts',(29.1468572533747,0.822311817466142,26.8774021512523));
#59745=CARTESIAN_POINT('Ctrl Pts',(29.259591693584,0.925109502257862,26.8668348294397));
#59746=CARTESIAN_POINT('Ctrl Pts',(29.522846414638,1.08544747155122,26.8449843892055));
#59747=CARTESIAN_POINT('Ctrl Pts',(29.672078571298,1.13945389610578,26.8339056600349));
#59748=CARTESIAN_POINT('Ctrl Pts',(29.9754469871149,1.18446101454497,26.813680840772));
#59749=CARTESIAN_POINT('Ctrl Pts',(30.1261553208811,1.17798106873351,26.804850259546));
#59750=CARTESIAN_POINT('Ctrl Pts',(30.4204691708303,1.10805786050355,26.7842980916158));
#59751=CARTESIAN_POINT('Ctrl Pts',(30.5609479127602,1.04399036631935,26.7734001867649));
#59752=CARTESIAN_POINT('Ctrl Pts',(30.8118142126087,0.8639649033663,26.7516124954367));
#59753=CARTESIAN_POINT('Ctrl Pts',(30.9191345732301,0.748795351296203,26.7409390107287));
#59754=CARTESIAN_POINT('Ctrl Pts',(31.0789814493982,0.489082061456906,26.7219153792232));
#59755=CARTESIAN_POINT('Ctrl Pts',(31.13228056467,0.348399841671576,26.7122041527178));
#59756=CARTESIAN_POINT('Ctrl Pts',(31.1843745315803,0.0489678760358684,
26.6909721883974));
#59757=CARTESIAN_POINT('Ctrl Pts',(31.1805251276485,-0.10725425723734,26.6798948715428));
#59758=CARTESIAN_POINT('Ctrl Pts',(31.112642066065,-0.408638429750164,26.658524481164));
#59759=CARTESIAN_POINT('Ctrl Pts',(31.04952452927,-0.550854728541633,26.6490856679416));
#59760=CARTESIAN_POINT('Ctrl Pts',(30.8739065476105,-0.80013916056119,26.6294633115169));
#59761=CARTESIAN_POINT('Ctrl Pts',(30.7641429817239,-0.90553953226469,26.6189861492083));
#59762=CARTESIAN_POINT('Ctrl Pts',(30.5058691930861,-1.0723039712914,26.5972137340794));
#59763=CARTESIAN_POINT('Ctrl Pts',(30.3585462682162,-1.13013161506019,26.5861167698907));
#59764=CARTESIAN_POINT('Ctrl Pts',(30.1366295806596,-1.1692866034305,26.5711011916684));
#59765=CARTESIAN_POINT('Ctrl Pts',(30.0683089619122,-1.17524047358085,26.5666946944513));
#59766=CARTESIAN_POINT('Ctrl Pts',(30.,-1.17524047358085,26.5625));
#59767=CARTESIAN_POINT('Ctrl Pts',(29.9999999999995,-1.17524047358085,26.4999999999999));
#59768=CARTESIAN_POINT('Ctrl Pts',(30.1204914385722,-1.17524047358085,26.5073990989566));
#59769=CARTESIAN_POINT('Ctrl Pts',(30.2404377363977,-1.1567191282047,26.5154213729959));
#59770=CARTESIAN_POINT('Ctrl Pts',(30.503109066672,-1.07331217218126,26.5345084966475));
#59771=CARTESIAN_POINT('Ctrl Pts',(30.6398547835573,-0.997848639879795,
26.5455811972524));
#59772=CARTESIAN_POINT('Ctrl Pts',(30.8720104636609,-0.801888849767787,
26.566784844391));
#59773=CARTESIAN_POINT('Ctrl Pts',(30.9665674240944,-0.684937055709897,
26.5764328435252));
#59774=CARTESIAN_POINT('Ctrl Pts',(31.1101788342394,-0.415941539318355,
26.595506636112));
#59775=CARTESIAN_POINT('Ctrl Pts',(31.1554918067157,-0.265175979373474,
26.606197041135));
#59776=CARTESIAN_POINT('Ctrl Pts',(31.184388668241,0.0421759563922281,26.6279905905315));
#59777=CARTESIAN_POINT('Ctrl Pts',(31.1688709786064,0.195715280062819,26.6388776761339));
#59778=CARTESIAN_POINT('Ctrl Pts',(31.080842595015,0.4851372161482,26.6593998545441));
#59779=CARTESIAN_POINT('Ctrl Pts',(31.0103902901456,0.618617027917578,26.6682199013902));
#59780=CARTESIAN_POINT('Ctrl Pts',(30.8184983590075,0.857859380695496,26.6884855739597));
#59781=CARTESIAN_POINT('Ctrl Pts',(30.6966625458602,0.959431158368461,26.6995683269243));
#59782=CARTESIAN_POINT('Ctrl Pts',(30.4255868085001,1.10584185104675,26.7214052635744));
#59783=CARTESIAN_POINT('Ctrl Pts',(30.280042417997,1.15134883169079,26.7319561985547));
#59784=CARTESIAN_POINT('Ctrl Pts',(29.9776063567648,1.18496921576007,26.7517200618056));
#59785=CARTESIAN_POINT('Ctrl Pts',(29.8235440457018,1.17197554004672,26.7609515037779));
#59786=CARTESIAN_POINT('Ctrl Pts',(29.5271473201095,1.08704252411486,26.7821637300309));
#59787=CARTESIAN_POINT('Ctrl Pts',(29.3879639883513,1.01521369745337,26.7932572549969));
#59788=CARTESIAN_POINT('Ctrl Pts',(29.1499744927664,0.825212607812385,26.8146078849744));
#59789=CARTESIAN_POINT('Ctrl Pts',(29.0521140662545,0.710618013126823,26.8246118717047));
#59790=CARTESIAN_POINT('Ctrl Pts',(28.9012898027458,0.445344450507133,26.8434217499511));
#59791=CARTESIAN_POINT('Ctrl Pts',(28.8519884644377,0.295869143296566,26.8540206664119));
#59792=CARTESIAN_POINT('Ctrl Pts',(28.8148602582687,-0.0109614775297701,
26.8757772506829));
#59793=CARTESIAN_POINT('Ctrl Pts',(28.8263846212866,-0.165256365046284,
26.886717911409));
#59794=CARTESIAN_POINT('Ctrl Pts',(28.90695684434,-0.456865689279699,26.9073951919876));
#59795=CARTESIAN_POINT('Ctrl Pts',(28.9737284626765,-0.591802058760263,
26.9162939800796));
#59796=CARTESIAN_POINT('Ctrl Pts',(29.1592103949543,-0.836102522890621,
26.9363453584795));
#59797=CARTESIAN_POINT('Ctrl Pts',(29.2786778563743,-0.94110103302348,26.9474041669452));
#59798=CARTESIAN_POINT('Ctrl Pts',(29.5466042812102,-1.09478566204523,26.9693055998652));
#59799=CARTESIAN_POINT('Ctrl Pts',(29.6913217184938,-1.14405280529544,26.9799390653881));
#59800=CARTESIAN_POINT('Ctrl Pts',(29.8940937627055,-1.17166523876262,26.9933697888908));
#59801=CARTESIAN_POINT('Ctrl Pts',(29.9470693710243,-1.17524047358085,26.9967496532013));
#59802=CARTESIAN_POINT('Ctrl Pts',(29.9999999999997,-1.17524047358085,26.9999999999999));
#59803=CARTESIAN_POINT('Origin',(30.,-1.21864324187371E-14,15.78125));
#59804=CARTESIAN_POINT('',(30.0000000000002,-1.17524047358085,27.5625));
#59805=CARTESIAN_POINT('',(30.,-1.17524047358085,27.5));
#59806=CARTESIAN_POINT('',(30.,-1.17524047358085,15.78125));
#59807=CARTESIAN_POINT('Ctrl Pts',(30.0000000000004,-1.17524047358085,27.5625));
#59808=CARTESIAN_POINT('Ctrl Pts',(29.8791981655177,-1.17524047358089,27.5550818403526));
#59809=CARTESIAN_POINT('Ctrl Pts',(29.7589726578968,-1.15662316573575,27.547039018461));
#59810=CARTESIAN_POINT('Ctrl Pts',(29.4966785757901,-1.0731279551929,27.5279719317893));
#59811=CARTESIAN_POINT('Ctrl Pts',(29.3604611797136,-0.99796015863462,27.5169421590736));
#59812=CARTESIAN_POINT('Ctrl Pts',(29.1231210583237,-0.797935915977368,
27.495276047424));
#59813=CARTESIAN_POINT('Ctrl Pts',(29.0249429590029,-0.674426740918645,
27.4853218966019));
#59814=CARTESIAN_POINT('Ctrl Pts',(28.8853520572172,-0.401644540260052,
27.4659795997989));
#59815=CARTESIAN_POINT('Ctrl Pts',(28.8432060655213,-0.256055793645229,
27.4556562695324));
#59816=CARTESIAN_POINT('Ctrl Pts',(28.8154546971309,0.0488704066146756,
27.4340347229132));
#59817=CARTESIAN_POINT('Ctrl Pts',(28.8323972811925,0.205546638674019,27.4229252070608));
#59818=CARTESIAN_POINT('Ctrl Pts',(28.9250076761164,0.498408501969224,27.4021591121013));
#59819=CARTESIAN_POINT('Ctrl Pts',(28.997892508521,0.632295921050251,27.3932865033313));
#59820=CARTESIAN_POINT('Ctrl Pts',(29.1909681621961,0.865881565904131,27.3731486925495));
#59821=CARTESIAN_POINT('Ctrl Pts',(29.3095755456334,0.963111668503783,27.3624181185496));
#59822=CARTESIAN_POINT('Ctrl Pts',(29.5806971724252,1.10891198583092,27.3406000040234));
#59823=CARTESIAN_POINT('Ctrl Pts',(29.7313794614454,1.15471361111034,27.3297231163935));
#59824=CARTESIAN_POINT('Ctrl Pts',(30.0349224077729,1.1841311566887,27.3100402882342));
#59825=CARTESIAN_POINT('Ctrl Pts',(30.1845806615862,1.17018311962186,27.3009860288447));
#59826=CARTESIAN_POINT('Ctrl Pts',(30.4753054258698,1.08577187813399,27.2801406033955));
#59827=CARTESIAN_POINT('Ctrl Pts',(30.6130774728742,1.01437069747224,27.2691489037921));
#59828=CARTESIAN_POINT('Ctrl Pts',(30.8550923899249,0.82117912160722,27.2474379673869));
#59829=CARTESIAN_POINT('Ctrl Pts',(30.9563451215602,0.700625408948211,27.2371795779744));
#59830=CARTESIAN_POINT('Ctrl Pts',(31.1030012085855,0.43246305141941,27.218164862578));
#59831=CARTESIAN_POINT('Ctrl Pts',(31.1490749245368,0.288512534258167,27.207957695024));
#59832=CARTESIAN_POINT('Ctrl Pts',(31.1854037082186,-0.0146433585393976,
27.1864616764351));
#59833=CARTESIAN_POINT('Ctrl Pts',(31.173058308365,-0.171282192075426,27.1753548124176));
#59834=CARTESIAN_POINT('Ctrl Pts',(31.089040383827,-0.467218401344852,27.1543707233508));
#59835=CARTESIAN_POINT('Ctrl Pts',(31.0195638166583,-0.603975746358807,
27.1453625116794));
#59836=CARTESIAN_POINT('Ctrl Pts',(30.8326207012815,-0.843150163878356,
27.1254031429327));
#59837=CARTESIAN_POINT('Ctrl Pts',(30.7170833899544,-0.943363872050058,
27.1147553149523));
#59838=CARTESIAN_POINT('Ctrl Pts',(30.4491800434626,-1.09737775442843,27.0928436259578));
#59839=CARTESIAN_POINT('Ctrl Pts',(30.2981995637065,-1.14764798518389,27.0817899983651));
#59840=CARTESIAN_POINT('Ctrl Pts',(30.0946434783266,-1.17238533021172,27.0684130613475));
#59841=CARTESIAN_POINT('Ctrl Pts',(30.0473000417297,-1.17524047358084,27.0654045855337));
#59842=CARTESIAN_POINT('Ctrl Pts',(30.0000000000003,-1.17524047358085,27.0625));
#59843=CARTESIAN_POINT('Ctrl Pts',(29.9999999999997,-1.17524047358085,26.9999999999999));
#59844=CARTESIAN_POINT('Ctrl Pts',(30.0986058905517,-1.17524047358085,27.0060551583626));
#59845=CARTESIAN_POINT('Ctrl Pts',(30.197001235846,-1.16283641910558,27.0125371577158));
#59846=CARTESIAN_POINT('Ctrl Pts',(30.4435331990926,-1.0993899448342,27.029925526711));
#59847=CARTESIAN_POINT('Ctrl Pts',(30.5849622280491,-1.0311122983099,27.0410310521114));
#59848=CARTESIAN_POINT('Ctrl Pts',(30.8283565317534,-0.84700506573289,27.0625046195245));
#59849=CARTESIAN_POINT('Ctrl Pts',(30.9294172599309,-0.734710314399227,
27.0726917923361));
#59850=CARTESIAN_POINT('Ctrl Pts',(31.0870905034712,-0.472970868314495,
27.0916537809288));
#59851=CARTESIAN_POINT('Ctrl Pts',(31.1401926761717,-0.324772377450416,
27.1019712110874));
#59852=CARTESIAN_POINT('Ctrl Pts',(31.1850952185403,-0.0184511332937437,
27.1236916767454));
#59853=CARTESIAN_POINT('Ctrl Pts',(31.1773587357349,0.136461808282747,27.1346761621237));
#59854=CARTESIAN_POINT('Ctrl Pts',(31.1038267733963,0.430084241190232,27.1554961871532));
#59855=CARTESIAN_POINT('Ctrl Pts',(31.0404668538449,0.566412733303589,27.1645221322455));
#59856=CARTESIAN_POINT('Ctrl Pts',(30.8621032542639,0.813817787312719,27.1842464597062));
#59857=CARTESIAN_POINT('Ctrl Pts',(30.746618378735,0.920903307832853,27.195134699154));
#59858=CARTESIAN_POINT('Ctrl Pts',(30.4841269758582,1.08160589165682,27.2169511927423));
#59859=CARTESIAN_POINT('Ctrl Pts',(30.3404475283553,1.13505921838268,27.2276693335753));
#59860=CARTESIAN_POINT('Ctrl Pts',(30.0413373449537,1.18420822105003,27.2477795099651));
#59861=CARTESIAN_POINT('Ctrl Pts',(29.8888261880251,1.17970362185606,27.2566686898965));
#59862=CARTESIAN_POINT('Ctrl Pts',(29.5891419642887,1.11207867848515,27.2774691579106));
#59863=CARTESIAN_POINT('Ctrl Pts',(29.4453407649054,1.04779159085184,27.2885788725534));
#59864=CARTESIAN_POINT('Ctrl Pts',(29.1960372639306,0.870265103883027,27.3101819980009));
#59865=CARTESIAN_POINT('Ctrl Pts',(29.091548794378,0.760562756134129,27.3204877500418));
#59866=CARTESIAN_POINT('Ctrl Pts',(28.9261102653187,0.502419631695097,27.3397990837129));
#59867=CARTESIAN_POINT('Ctrl Pts',(28.8688162363146,0.355135077347701,27.3498182687336));
#59868=CARTESIAN_POINT('Ctrl Pts',(28.8157293168355,0.0491393235848099,
27.3715156546901));
#59869=CARTESIAN_POINT('Ctrl Pts',(28.8194875433144,-0.106321035237959,
27.3825389560425));
#59870=CARTESIAN_POINT('Ctrl Pts',(28.8856486083743,-0.401996025014571,
27.4035045226948));
#59871=CARTESIAN_POINT('Ctrl Pts',(28.9454972717022,-0.539801328338099,
27.4127167480926));
#59872=CARTESIAN_POINT('Ctrl Pts',(29.11742422097,-0.791565441680741,27.4322003607736));
#59873=CARTESIAN_POINT('Ctrl Pts',(29.2301245105903,-0.901546472787143,
27.4430202619491));
#59874=CARTESIAN_POINT('Ctrl Pts',(29.4887201815225,-1.06909180163981,27.4648401285834));
#59875=CARTESIAN_POINT('Ctrl Pts',(29.6313699534066,-1.1262717375032,27.4756271616522));
#59876=CARTESIAN_POINT('Ctrl Pts',(29.853348441796,-1.16837939045814,27.4907512179135));
#59877=CARTESIAN_POINT('Ctrl Pts',(29.9266702080884,-1.17524047358085,27.4954969880578));
#59878=CARTESIAN_POINT('Ctrl Pts',(30.,-1.17524047358085,27.5));
#59879=CARTESIAN_POINT('Origin',(30.,-1.21864324187371E-14,15.78125));
#59880=CARTESIAN_POINT('',(30.,-1.17524047358085,28.0625));
#59881=CARTESIAN_POINT('',(30.0000000000001,-1.17524047358085,28.));
#59882=CARTESIAN_POINT('',(30.,-1.17524047358085,15.78125));
#59883=CARTESIAN_POINT('Ctrl Pts',(30.,-1.17524047358085,28.0625));
#59884=CARTESIAN_POINT('Ctrl Pts',(29.8576309526277,-1.17524047358085,28.0537574479785));
#59885=CARTESIAN_POINT('Ctrl Pts',(29.7163289872701,-1.14937338079985,28.0441633378768));
#59886=CARTESIAN_POINT('Ctrl Pts',(29.4381412694858,-1.0437960185582,28.0233373652109));
#59887=CARTESIAN_POINT('Ctrl Pts',(29.3055725204167,-0.960712774920266,
28.0122510152415));
#59888=CARTESIAN_POINT('Ctrl Pts',(29.0812375157914,-0.748784364739409,
27.9909614703353));
#59889=CARTESIAN_POINT('Ctrl Pts',(28.991345872443,-0.622420436003701,27.9816342608879));
#59890=CARTESIAN_POINT('Ctrl Pts',(28.8663365712296,-0.344659291734443,
27.9619389197703));
#59891=CARTESIAN_POINT('Ctrl Pts',(28.8314934625426,-0.196359386622749,
27.9514233481032));
#59892=CARTESIAN_POINT('Ctrl Pts',(28.8195620391171,0.111178530712451,27.9296166112233));
#59893=CARTESIAN_POINT('Ctrl Pts',(28.8449209434754,0.267584161126331,27.9185262830501));
#59894=CARTESIAN_POINT('Ctrl Pts',(28.9530728770119,0.554595748995939,27.8981750163432));
#59895=CARTESIAN_POINT('Ctrl Pts',(29.0321899221582,0.683358417415679,27.8893700226253));
#59896=CARTESIAN_POINT('Ctrl Pts',(29.2365478324768,0.90645295573766,27.8689113436395));
#59897=CARTESIAN_POINT('Ctrl Pts',(29.3606700385593,0.997879761432882,27.8580478657718));
#59898=CARTESIAN_POINT('Ctrl Pts',(29.6397630167776,1.12947461119937,27.8362438860083));
#59899=CARTESIAN_POINT('Ctrl Pts',(29.7926014521638,1.16725893043214,27.8255188379057));
#59900=CARTESIAN_POINT('Ctrl Pts',(30.0971888483988,1.18064726325309,27.8063401680006));
#59901=CARTESIAN_POINT('Ctrl Pts',(30.2459190189188,1.15884794264961,27.7968175086224));
#59902=CARTESIAN_POINT('Ctrl Pts',(30.5325764826745,1.05897425995597,27.7756736453134));
#59903=CARTESIAN_POINT('Ctrl Pts',(30.6670400332198,0.979858412729581,27.7646115990219));
#59904=CARTESIAN_POINT('Ctrl Pts',(30.8979501916997,0.773870883397489,27.7431289156398));
#59905=CARTESIAN_POINT('Ctrl Pts',(30.9919903689524,0.648942084588862,27.7335148439956));
#59906=CARTESIAN_POINT('Ctrl Pts',(31.1243827012244,0.373674108325156,27.7139962871235));
#59907=CARTESIAN_POINT('Ctrl Pts',(31.1629506296625,0.226703861102418,27.7035749981386));
#59908=CARTESIAN_POINT('Ctrl Pts',(31.182930645767,-0.0796098768690557,
27.6818550647252));
#59909=CARTESIAN_POINT('Ctrl Pts',(31.1618436472684,-0.236207537040712,
27.6707511202069));
#59910=CARTESIAN_POINT('Ctrl Pts',(31.0615541749908,-0.526222674013738,
27.6501868794201));
#59911=CARTESIAN_POINT('Ctrl Pts',(30.9856010212307,-0.657569956578418,
27.641376820382));
#59912=CARTESIAN_POINT('Ctrl Pts',(30.7869826832863,-0.886033452367878,
27.6210802455783));
#59913=CARTESIAN_POINT('Ctrl Pts',(30.6656419827339,-0.980462303947253,
27.6102811397496));
#59914=CARTESIAN_POINT('Ctrl Pts',(30.3905261901255,-1.11936682731598,27.5884622344572));
#59915=CARTESIAN_POINT('Ctrl Pts',(30.2387339000707,-1.16125829953858,27.5776558137839));
#59916=CARTESIAN_POINT('Ctrl Pts',(30.0554488466051,-1.17426038713893,27.5659397324124));
#59917=CARTESIAN_POINT('Ctrl Pts',(30.0277113777332,-1.17524047358084,27.5642016912446));
#59918=CARTESIAN_POINT('Ctrl Pts',(30.0000000000004,-1.17524047358085,27.5625));
#59919=CARTESIAN_POINT('Ctrl Pts',(30.,-1.17524047358085,27.5));
#59920=CARTESIAN_POINT('Ctrl Pts',(30.0764884643488,-1.17524047358085,27.5046969786688));
#59921=CARTESIAN_POINT('Ctrl Pts',(30.1529528341161,-1.16777574296381,27.5096571303415));
#59922=CARTESIAN_POINT('Ctrl Pts',(30.3817494239676,-1.12246086122216,27.5253135785994));
#59923=CARTESIAN_POINT('Ctrl Pts',(30.5275514222186,-1.06175746883915,27.5364191022575));
#59924=CARTESIAN_POINT('Ctrl Pts',(30.7819194324173,-0.890185564641921,
27.5581221152238));
#59925=CARTESIAN_POINT('Ctrl Pts',(30.8893748791333,-0.782854361740771,
27.5685259964847));
#59926=CARTESIAN_POINT('Ctrl Pts',(31.0605234375151,-0.529653947481304,
27.5880127322271));
#59927=CARTESIAN_POINT('Ctrl Pts',(31.1210989339899,-0.385229961573254,
27.5976843165126));
#59928=CARTESIAN_POINT('Ctrl Pts',(31.1825194576632,-0.0817855747122669,
27.6192007914867));
#59929=CARTESIAN_POINT('Ctrl Pts',(31.1830228429167,0.0741472759213479,
27.63025759604));
#59930=CARTESIAN_POINT('Ctrl Pts',(31.1247432077576,0.371953492117145,27.6513742825742));
#59931=CARTESIAN_POINT('Ctrl Pts',(31.0685868115923,0.511361040320207,27.6608435628079));
#59932=CARTESIAN_POINT('Ctrl Pts',(30.9034614818395,0.767636822344003,27.6800694593713));
#59933=CARTESIAN_POINT('Ctrl Pts',(30.7937668420839,0.880579083554765,27.6908097772536));
#59934=CARTESIAN_POINT('Ctrl Pts',(30.5394580202052,1.05521084982092,27.712617639148));
#59935=CARTESIAN_POINT('Ctrl Pts',(30.3979930311562,1.11628678065312,27.7234700450399));
#59936=CARTESIAN_POINT('Ctrl Pts',(30.102283661711,1.18033932531086,27.7438997716137));
#59937=CARTESIAN_POINT('Ctrl Pts',(29.9510987894339,1.18375239925559,27.752701130013));
#59938=CARTESIAN_POINT('Ctrl Pts',(29.6486955420892,1.13241772430468,27.7730910160496));
#59939=CARTESIAN_POINT('Ctrl Pts',(29.5009111395855,1.07549105438516,27.7841843756164));
#59940=CARTESIAN_POINT('Ctrl Pts',(29.2414417758967,0.910237971539166,27.8059766250036));
#59941=CARTESIAN_POINT('Ctrl Pts',(29.1309679987517,0.805447516109976,27.8164757759223));
#59942=CARTESIAN_POINT('Ctrl Pts',(28.9539689931679,0.557381504423619,27.8361397402596));
#59943=CARTESIAN_POINT('Ctrl Pts',(28.8900701663349,0.415841482478183,27.8455137308899));
#59944=CARTESIAN_POINT('Ctrl Pts',(28.8202010476643,0.115104610378523,27.8668382228314));
#59945=CARTESIAN_POINT('Ctrl Pts',(28.8153164753922,-0.0411926086217122,
27.8779208638252));
#59946=CARTESIAN_POINT('Ctrl Pts',(28.8654961586475,-0.341119160610214,
27.8991878980145));
#59947=CARTESIAN_POINT('Ctrl Pts',(28.9179176762722,-0.482198917057609,
27.9089809285524));
#59948=CARTESIAN_POINT('Ctrl Pts',(29.0761417927703,-0.742958176446737,
27.9279419936907));
#59949=CARTESIAN_POINT('Ctrl Pts',(29.1827253034037,-0.858799901268264,
27.938594061191));
#59950=CARTESIAN_POINT('Ctrl Pts',(29.4325136093474,-1.04046451212148,27.9603736693398));
#59951=CARTESIAN_POINT('Ctrl Pts',(29.5726776549044,-1.10544579696665,27.9712846467122));
#59952=CARTESIAN_POINT('Ctrl Pts',(29.8127786384444,-1.16404144712018,27.9881061243607));
#59953=CARTESIAN_POINT('Ctrl Pts',(29.9063068575872,-1.17524047358087,27.9942465220726));
#59954=CARTESIAN_POINT('Ctrl Pts',(30.0000000000002,-1.17524047358085,28.));
#59955=CARTESIAN_POINT('Origin',(30.,-1.21864324187371E-14,15.78125));
#59956=CARTESIAN_POINT('',(30.,-1.17524047358085,28.5625));
#59957=CARTESIAN_POINT('',(30.0000000000002,-1.17524047358085,28.5));
#59958=CARTESIAN_POINT('',(30.,-1.17524047358085,15.78125));
#59959=CARTESIAN_POINT('Ctrl Pts',(29.9999999999999,-1.17524047358085,28.5625));
#59960=CARTESIAN_POINT('Ctrl Pts',(29.9854755687231,-1.17524047358085,28.5616080884619));
#59961=CARTESIAN_POINT('Ctrl Pts',(29.9709414772303,-1.17497122100143,28.5607060377023));
#59962=CARTESIAN_POINT('Ctrl Pts',(29.8064818821414,-1.16886648226933,28.5503905207309));
#59963=CARTESIAN_POINT('Ctrl Pts',(29.6590422242683,-1.13464684706092,28.5401233803667));
#59964=CARTESIAN_POINT('Ctrl Pts',(29.3797071247853,-1.01029888540339,28.5185614617647));
#59965=CARTESIAN_POINT('Ctrl Pts',(29.251363124374,-0.919248746833339,28.507452087585));
#59966=CARTESIAN_POINT('Ctrl Pts',(29.0406130665321,-0.695506305973089,
28.486577911123));
#59967=CARTESIAN_POINT('Ctrl Pts',(28.9590502383724,-0.56619133070644,28.4776471970656));
#59968=CARTESIAN_POINT('Ctrl Pts',(28.8493945968077,-0.283424288620792,
28.4575969003786));
#59969=CARTESIAN_POINT('Ctrl Pts',(28.8224557263032,-0.132654402250458,
28.4469061885797));
#59970=CARTESIAN_POINT('Ctrl Pts',(28.8274401393345,0.174951078681269,28.4250946609358));
#59971=CARTESIAN_POINT('Ctrl Pts',(28.8609710566448,0.328840848056597,28.4141827261138));
#59972=CARTESIAN_POINT('Ctrl Pts',(28.9834218096268,0.608264397886715,28.394369508017));
#59973=CARTESIAN_POINT('Ctrl Pts',(29.0686800279675,0.732167484395331,28.3853987862865));
#59974=CARTESIAN_POINT('Ctrl Pts',(29.2841654510491,0.944633593842617,28.3646336101487));
#59975=CARTESIAN_POINT('Ctrl Pts',(29.4135237499535,1.0299476859008,28.3536653145426));
#59976=CARTESIAN_POINT('Ctrl Pts',(29.6999884026637,1.14695518646917,28.3319258334386));
#59977=CARTESIAN_POINT('Ctrl Pts',(29.8545850153065,1.1765676391467,28.321476648926));
#59978=CARTESIAN_POINT('Ctrl Pts',(30.1599574738008,1.17387642238167,28.3026290229131));
#59979=CARTESIAN_POINT('Ctrl Pts',(30.3078958483554,1.14400535727984,28.2924854305785));
#59980=CARTESIAN_POINT('Ctrl Pts',(30.5899420117525,1.02824734362325,28.2710615776053));
#59981=CARTESIAN_POINT('Ctrl Pts',(30.7205565666579,0.941343746526345,28.2599597843468));
#59982=CARTESIAN_POINT('Ctrl Pts',(30.9384441962492,0.723734320112842,28.2388647444883));
#59983=CARTESIAN_POINT('Ctrl Pts',(31.0243441752868,0.5959705376245,28.2297587654061));
#59984=CARTESIAN_POINT('Ctrl Pts',(31.1420857275796,0.315809924237744,28.2098932839944));
#59985=CARTESIAN_POINT('Ctrl Pts',(31.1732121728651,0.166290213222924,28.1992912189719));
#59986=CARTESIAN_POINT('Ctrl Pts',(31.1771534741222,-0.14225217236566,28.1774132577855));
#59987=CARTESIAN_POINT('Ctrl Pts',(31.1475738082276,-0.298357527790664,
28.1663442213532));
#59988=CARTESIAN_POINT('Ctrl Pts',(31.0316967203975,-0.582326286717529,
28.1462087139606));
#59989=CARTESIAN_POINT('Ctrl Pts',(30.9494361151523,-0.708574806833004,
28.1373477050794));
#59990=CARTESIAN_POINT('Ctrl Pts',(30.7393766183288,-0.926260402286338,
28.1167306721673));
#59991=CARTESIAN_POINT('Ctrl Pts',(30.6125440370362,-1.01460273603848,28.1058101125197));
#59992=CARTESIAN_POINT('Ctrl Pts',(30.3296673321613,-1.13876808424026,28.0840371864985));
#59993=CARTESIAN_POINT('Ctrl Pts',(30.1758968644013,-1.17241612952657,28.0734015508245));
#59994=CARTESIAN_POINT('Ctrl Pts',(30.0133354780172,-1.17518374723503,28.0633209118452));
#59995=CARTESIAN_POINT('Ctrl Pts',(30.0066666906193,-1.17524047358085,28.0629093859629));
#59996=CARTESIAN_POINT('Ctrl Pts',(30.,-1.17524047358085,28.0625));
#59997=CARTESIAN_POINT('Ctrl Pts',(30.0000000000002,-1.17524047358085,28.));
#59998=CARTESIAN_POINT('Ctrl Pts',(30.055120011526,-1.17524047358084,28.0033847916881));
#59999=CARTESIAN_POINT('Ctrl Pts',(30.1102800819057,-1.17136342893539,28.0069094990185));
#60000=CARTESIAN_POINT('Ctrl Pts',(30.320778299587,-1.14149919825233,28.0208945034877));
#60001=CARTESIAN_POINT('Ctrl Pts',(30.4704399584402,-1.08838822567003,28.0319678602702));
#60002=CARTESIAN_POINT('Ctrl Pts',(30.7348284172129,-0.929562358310031,
28.0538343110362));
#60003=CARTESIAN_POINT('Ctrl Pts',(30.8482436418564,-0.827380507129033,
28.0644216046344));
#60004=CARTESIAN_POINT('Ctrl Pts',(31.0309964109232,-0.58443378950115,28.0842573960977));
#60005=CARTESIAN_POINT('Ctrl Pts',(31.0981318171314,-0.445680080400429,
28.0933979512832));
#60006=CARTESIAN_POINT('Ctrl Pts',(31.1762201438822,-0.147691887981632,
28.1145275412917));
#60007=CARTESIAN_POINT('Ctrl Pts',(31.1854211354334,0.00884554012676132,
28.1256272149066));
#60008=CARTESIAN_POINT('Ctrl Pts',(31.1432517249665,0.310649796547867,28.1470273923742));
#60009=CARTESIAN_POINT('Ctrl Pts',(31.0945166442476,0.453415390384783,28.1571505400084));
#60010=CARTESIAN_POINT('Ctrl Pts',(30.9430034157352,0.718468313966014,28.1759447732979));
#60011=CARTESIAN_POINT('Ctrl Pts',(30.8395316819024,0.837077300041102,28.1864571641064));
#60012=CARTESIAN_POINT('Ctrl Pts',(30.594175126874,1.02551549499305,28.2082047776097));
#60013=CARTESIAN_POINT('Ctrl Pts',(30.4553685567187,1.0942445153416,28.2191652668043));
#60014=CARTESIAN_POINT('Ctrl Pts',(30.1633070228503,1.17335763356101,28.2399049418951));
#60015=CARTESIAN_POINT('Ctrl Pts',(30.0132854694265,1.18458952272981,28.2488527114972));
#60016=CARTESIAN_POINT('Ctrl Pts',(29.7101813599922,1.14957783235101,28.2687069250423));
#60017=CARTESIAN_POINT('Ctrl Pts',(29.5603537745588,1.10100720474222,28.2796294987935));
#60018=CARTESIAN_POINT('Ctrl Pts',(29.2921855827035,0.950361389094781,28.3014380407736));
#60019=CARTESIAN_POINT('Ctrl Pts',(29.1755651130251,0.851181456436058,28.3121157317836));
#60020=CARTESIAN_POINT('Ctrl Pts',(28.9864685212412,0.613960284958293,28.3321380906356));
#60021=CARTESIAN_POINT('Ctrl Pts',(28.9157930252681,0.478217809624506,28.341090783094));
#60022=CARTESIAN_POINT('Ctrl Pts',(28.8287462552022,0.18335177826131,28.3619989885486));
#60023=CARTESIAN_POINT('Ctrl Pts',(28.8147855892159,0.0266848358587583,
28.3731078456949));
#60024=CARTESIAN_POINT('Ctrl Pts',(28.8481057813277,-0.277120858900621,
28.3946499400995));
#60025=CARTESIAN_POINT('Ctrl Pts',(28.8928044130046,-0.421659697790202,
28.4048988240612));
#60026=CARTESIAN_POINT('Ctrl Pts',(29.0376019293491,-0.692609521363159,
28.4241111916336));
#60027=CARTESIAN_POINT('Ctrl Pts',(29.1388311172626,-0.815074867447836,
28.4343484054768));
#60028=CARTESIAN_POINT('Ctrl Pts',(29.3808301647318,-1.01067727789171,28.456143840463));
#60029=CARTESIAN_POINT('Ctrl Pts',(29.5182554521743,-1.08294295653866,28.4671448960526));
#60030=CARTESIAN_POINT('Ctrl Pts',(29.7744135979937,-1.15894806924162,28.4855696371912));
#60031=CARTESIAN_POINT('Ctrl Pts',(29.8869899356779,-1.1752404735809,28.493060314833));
#60032=CARTESIAN_POINT('Ctrl Pts',(30.0000000000005,-1.17524047358085,28.5));
#60033=CARTESIAN_POINT('Origin',(30.,-1.21864324187371E-14,15.78125));
#60034=CARTESIAN_POINT('',(29.9999999999997,-1.17524047358085,29.0625));
#60035=CARTESIAN_POINT('',(30.,-1.17524047358085,29.));
#60036=CARTESIAN_POINT('',(30.,-1.17524047358085,15.78125));
#60037=CARTESIAN_POINT('Ctrl Pts',(29.9999999999995,-1.17524047358085,29.0625));
#60038=CARTESIAN_POINT('Ctrl Pts',(29.9663313283337,-1.17524047358085,29.0604324851927));
#60039=CARTESIAN_POINT('Ctrl Pts',(29.9326266255446,-1.17379373293774,29.0583114654359));
#60040=CARTESIAN_POINT('Ctrl Pts',(29.7487805300534,-1.15793171143038,29.046459536434));
#60041=CARTESIAN_POINT('Ctrl Pts',(29.6025054140808,-1.11619705168394,29.0359974721754));
#60042=CARTESIAN_POINT('Ctrl Pts',(29.3284713606868,-0.977122112422326,
29.0142389520917));
#60043=CARTESIAN_POINT('Ctrl Pts',(29.204360853848,-0.879027723836093,29.003139801917));
#60044=CARTESIAN_POINT('Ctrl Pts',(29.0061078341151,-0.644908297203287,
28.9826651365702));
#60045=CARTESIAN_POINT('Ctrl Pts',(28.9319567448549,-0.512847810431858,
28.9738647427883));
#60046=CARTESIAN_POINT('Ctrl Pts',(28.8365844224207,-0.225635628236165,
28.9534992524445));
#60047=CARTESIAN_POINT('Ctrl Pts',(28.8171575566038,-0.0729412609821712,
28.9426720805673));
#60048=CARTESIAN_POINT('Ctrl Pts',(28.8379321785986,0.234707082052963,28.92085751368));
#60049=CARTESIAN_POINT('Ctrl Pts',(28.8792757590782,0.386638085776581,28.9100844699825));
#60050=CARTESIAN_POINT('Ctrl Pts',(29.0157412244589,0.659238101106546,28.8907550914809));
#60051=CARTESIAN_POINT('Ctrl Pts',(29.107096372761,0.778529076561771,28.8813960362208));
#60052=CARTESIAN_POINT('Ctrl Pts',(29.3335481377689,0.980220242371224,28.8603394545531));
#60053=CARTESIAN_POINT('Ctrl Pts',(29.4678337645529,1.05914504636678,28.8492951073424));
#60054=CARTESIAN_POINT('Ctrl Pts',(29.760564366148,1.1610786562004,28.8277052746509));
#60055=CARTESIAN_POINT('Ctrl Pts',(29.9162604257863,1.18253750642917,28.8179009595418));
#60056=CARTESIAN_POINT('Ctrl Pts',(30.2216914945448,1.16389753053477,28.7984842912973));
#60057=CARTESIAN_POINT('Ctrl Pts',(30.3686116386073,1.12601470107769,28.7881191791422));
#60058=CARTESIAN_POINT('Ctrl Pts',(30.645460693513,0.994469364755083,28.7664547489262));
#60059=CARTESIAN_POINT('Ctrl Pts',(30.7717903384927,0.899966183411579,28.7553466483575));
#60060=CARTESIAN_POINT('Ctrl Pts',(30.9764758301347,0.671134004376585,28.7346644325598));
#60061=CARTESIAN_POINT('Ctrl Pts',(31.0544159221586,0.540492245543279,28.7258249398524));
#60062=CARTESIAN_POINT('Ctrl Pts',(31.1571623293156,0.255550540096121,28.7056204432797));
#60063=CARTESIAN_POINT('Ctrl Pts',(31.1804841833933,0.103803871660056,28.6948604703318));
#60064=CARTESIAN_POINT('Ctrl Pts',(31.1678665590545,-0.203924479708025,
28.6730402302557));
#60065=CARTESIAN_POINT('Ctrl Pts',(31.130543099267,-0.356918086122505,28.6621918400855));
#60066=CARTESIAN_POINT('Ctrl Pts',(31.0012937995436,-0.633072694293491,
28.6426104143845));
#60067=CARTESIAN_POINT('Ctrl Pts',(30.9131062008608,-0.754733454165662,
28.6334802730101));
#60068=CARTESIAN_POINT('Ctrl Pts',(30.6923373486102,-0.962047131628042,
28.6125733267459));
#60069=CARTESIAN_POINT('Ctrl Pts',(30.5605741188135,-1.04432722358406,28.6015649165697));
#60070=CARTESIAN_POINT('Ctrl Pts',(30.2834202387706,-1.14942800624881,28.5808193260016));
#60071=CARTESIAN_POINT('Ctrl Pts',(30.1422284632676,-1.17524047358085,28.5712339190787));
#60072=CARTESIAN_POINT('Ctrl Pts',(29.9999999999999,-1.17524047358085,28.5625));
#60073=CARTESIAN_POINT('Ctrl Pts',(30.0000000000005,-1.17524047358085,28.5));
#60074=CARTESIAN_POINT('Ctrl Pts',(30.0354745744302,-1.17524047358084,28.5021784110951));
#60075=CARTESIAN_POINT('Ctrl Pts',(30.070984899228,-1.17363438892678,28.50441595924));
#60076=CARTESIAN_POINT('Ctrl Pts',(30.2617617366305,-1.15628719000694,28.5167461440698));
#60077=CARTESIAN_POINT('Ctrl Pts',(30.4127085422869,-1.11138228847866,28.527607482843));
#60078=CARTESIAN_POINT('Ctrl Pts',(30.6847642885538,-0.967157900388871,
28.5494270868925));
#60079=CARTESIAN_POINT('Ctrl Pts',(30.804005950619,-0.870565283253422,28.5601740092255));
#60080=CARTESIAN_POINT('Ctrl Pts',(30.9983603111577,-0.638155310621775,
28.5803486604476));
#60081=CARTESIAN_POINT('Ctrl Pts',(31.0719538047089,-0.504858427298666,
28.5892017641887));
#60082=CARTESIAN_POINT('Ctrl Pts',(31.1663430846515,-0.212647773407092,
28.6099216835343));
#60083=CARTESIAN_POINT('Ctrl Pts',(31.1842429187448,-0.0559802512603478,
28.6210305817888));
#60084=CARTESIAN_POINT('Ctrl Pts',(31.1582832767207,0.249283949423046,28.6426760951642));
#60085=CARTESIAN_POINT('Ctrl Pts',(31.1169606007789,0.395199803964739,28.6530226198275));
#60086=CARTESIAN_POINT('Ctrl Pts',(30.9790360194058,0.668562290541804,28.6724060632391));
#60087=CARTESIAN_POINT('Ctrl Pts',(30.8818240300007,0.792402281745908,28.6822761930404));
#60088=CARTESIAN_POINT('Ctrl Pts',(30.6459736712074,0.993822232743541,28.7039003049109));
#60089=CARTESIAN_POINT('Ctrl Pts',(30.5101537410361,1.06991069848525,28.7149383113331));
#60090=CARTESIAN_POINT('Ctrl Pts',(30.2218612846042,1.16368326752433,28.7359662684601));
#60091=CARTESIAN_POINT('Ctrl Pts',(30.0727878905027,1.18239624374933,28.7452765661691));
#60092=CARTESIAN_POINT('Ctrl Pts',(29.7685724316717,1.16273575029291,28.764654767797));
#60093=CARTESIAN_POINT('Ctrl Pts',(29.6165255150965,1.12180125661046,28.7754428960271));
#60094=CARTESIAN_POINT('Ctrl Pts',(29.3404632117996,0.984593855919108,28.797259754998));
#60095=CARTESIAN_POINT('Ctrl Pts',(29.2184662863885,0.890859052794272,28.8080745514575));
#60096=CARTESIAN_POINT('Ctrl Pts',(29.0185031029016,0.663646825495766,28.8284093479536));
#60097=CARTESIAN_POINT('Ctrl Pts',(28.9418083423014,0.532910081337728,28.8372126922591));
#60098=CARTESIAN_POINT('Ctrl Pts',(28.8396688119263,0.243593095049782,28.8577274289443));
#60099=CARTESIAN_POINT('Ctrl Pts',(28.8175791014781,0.0870303940346913,
28.8688288945971));
#60100=CARTESIAN_POINT('Ctrl Pts',(28.8356734059559,-0.219589451967425,
28.8905705333577));
#60101=CARTESIAN_POINT('Ctrl Pts',(28.8733703746263,-0.366880393585839,
28.9010145619721));
#60102=CARTESIAN_POINT('Ctrl Pts',(29.0040267448551,-0.642739671975603,
28.9205750465844));
#60103=CARTESIAN_POINT('Ctrl Pts',(29.0970828699605,-0.768007510288218,
28.9301160290222));
#60104=CARTESIAN_POINT('Ctrl Pts',(29.3264450160403,-0.975407631545752,
28.9515537342264));
#60105=CARTESIAN_POINT('Ctrl Pts',(29.4604715589085,-1.05546393671967,28.9626222876417));
#60106=CARTESIAN_POINT('Ctrl Pts',(29.7327334190531,-1.15230702146743,28.9827747043974));
#60107=CARTESIAN_POINT('Ctrl Pts',(29.8659356312532,-1.17524047358086,28.9917674189746));
#60108=CARTESIAN_POINT('Ctrl Pts',(30.0000000000001,-1.17524047358085,29.));
#60109=CARTESIAN_POINT('Origin',(30.,-1.21864324187371E-14,15.78125));
#60110=CARTESIAN_POINT('',(29.9999999999999,-1.17524047358085,29.5625));
#60111=CARTESIAN_POINT('',(30.,-1.17524047358085,29.5));
#60112=CARTESIAN_POINT('',(30.,-1.17524047358085,15.78125));
#60113=CARTESIAN_POINT('Ctrl Pts',(29.9999999999998,-1.17524047358085,29.5625));
#60114=CARTESIAN_POINT('Ctrl Pts',(29.9467973546619,-1.17524047358085,29.5592329493093));
#60115=CARTESIAN_POINT('Ctrl Pts',(29.8935499193759,-1.17162840400865,29.5558350868076));
#60116=CARTESIAN_POINT('Ctrl Pts',(29.6905156464705,-1.14383638937277,29.5423818936273));
#60117=CARTESIAN_POINT('Ctrl Pts',(29.5458229652857,-1.09446322181842,29.531746189361));
#60118=CARTESIAN_POINT('Ctrl Pts',(29.2779882672223,-0.940574047774209,
29.5098431372833));
#60119=CARTESIAN_POINT('Ctrl Pts',(29.1585890601641,-0.835479489994527,
29.4987851149112));
#60120=CARTESIAN_POINT('Ctrl Pts',(28.9732889450876,-0.591037021395749,
29.4787398668936));
#60121=CARTESIAN_POINT('Ctrl Pts',(28.9066211123554,-0.456058910232785,
29.4698379853235));
#60122=CARTESIAN_POINT('Ctrl Pts',(28.8262612459225,-0.164388119091858,
29.4491563462818));
#60123=CARTESIAN_POINT('Ctrl Pts',(28.8148509180816,-0.0100732314283097,
29.4382142673958));
#60124=CARTESIAN_POINT('Ctrl Pts',(28.852213214805,0.296739305134607,29.4164589654342));
#60125=CARTESIAN_POINT('Ctrl Pts',(28.9016274703356,0.446176311860775,29.405862764764));
#60126=CARTESIAN_POINT('Ctrl Pts',(29.0526565417776,0.711342976877612,29.3870604663565));
#60127=CARTESIAN_POINT('Ctrl Pts',(29.1506118786123,0.825870653466757,29.3770454144149));
#60128=CARTESIAN_POINT('Ctrl Pts',(29.3887681357508,1.01569990993121,29.3556906361267));
#60129=CARTESIAN_POINT('Ctrl Pts',(29.5280199399709,1.08742345397384,29.3445966390884));
#60130=CARTESIAN_POINT('Ctrl Pts',(29.8244665773462,1.17210985589585,29.3233900912571));
#60131=CARTESIAN_POINT('Ctrl Pts',(29.9785058773413,1.18498177307898,29.3141652695437));
#60132=CARTESIAN_POINT('Ctrl Pts',(30.2808965556073,1.15114217787766,29.2943964213012));
#60133=CARTESIAN_POINT('Ctrl Pts',(30.4264177470889,1.1055232193301,29.2838429408837));
#60134=CARTESIAN_POINT('Ctrl Pts',(30.697402601783,0.95889535591386,29.2620038856125));
#60135=CARTESIAN_POINT('Ctrl Pts',(30.819169348162,0.85722095894767,29.2509217356401));
#60136=CARTESIAN_POINT('Ctrl Pts',(31.0108714255578,0.617827319896978,29.2306623578836));
#60137=CARTESIAN_POINT('Ctrl Pts',(31.0812140757987,0.48430476852144,29.221840827786));
#60138=CARTESIAN_POINT('Ctrl Pts',(31.1690224491511,0.194817477900372,29.2013140152506));
#60139=CARTESIAN_POINT('Ctrl Pts',(31.1844226308274,0.0412543787619307,
29.1904252437899));
#60140=CARTESIAN_POINT('Ctrl Pts',(31.1552826086302,-0.266085347349785,
29.1686325601491));
#60141=CARTESIAN_POINT('Ctrl Pts',(31.1098513200658,-0.416814367038074,
29.1579447461033));
#60142=CARTESIAN_POINT('Ctrl Pts',(30.9660264712179,-0.685700945491834,
29.1388786780306));
#60143=CARTESIAN_POINT('Ctrl Pts',(30.8713728192914,-0.802582950873403,
29.1292210796557));
#60144=CARTESIAN_POINT('Ctrl Pts',(30.6390456070483,-0.99836896334456,29.1080130601942));
#60145=CARTESIAN_POINT('Ctrl Pts',(30.5022270643229,-1.07372697770931,29.0969396285291));
#60146=CARTESIAN_POINT('Ctrl Pts',(30.2397868247199,-1.15682002769535,29.0778778247601));
#60147=CARTESIAN_POINT('Ctrl Pts',(30.1201628836901,-1.17524047358085,29.0698789231656));
#60148=CARTESIAN_POINT('Ctrl Pts',(29.9999999999995,-1.17524047358085,29.0625));
#60149=CARTESIAN_POINT('Ctrl Pts',(30.0000000000001,-1.17524047358085,29.));
#60150=CARTESIAN_POINT('Ctrl Pts',(30.0146960045521,-1.17524047358085,29.0009024474538));
#60151=CARTESIAN_POINT('Ctrl Pts',(30.0294011894743,-1.17496482224357,29.0018152315228));
#60152=CARTESIAN_POINT('Ctrl Pts',(30.199932441124,-1.16856010735523,29.0125142300756));
#60153=CARTESIAN_POINT('Ctrl Pts',(30.353002562887,-1.13175546267305,29.0232187723758));
#60154=CARTESIAN_POINT('Ctrl Pts',(30.6330116689674,-1.00191414666784,29.0450168400954));
#60155=CARTESIAN_POINT('Ctrl Pts',(30.7577840016447,-0.911212372347243,
29.0558945356534));
#60156=CARTESIAN_POINT('Ctrl Pts',(30.9634990803743,-0.689398439003151,
29.0763911529622));
#60157=CARTESIAN_POINT('Ctrl Pts',(31.0433641152287,-0.561238966842274,
29.0852039625465));
#60158=CARTESIAN_POINT('Ctrl Pts',(31.1533625468904,-0.274946500315461,
29.1055042381753));
#60159=CARTESIAN_POINT('Ctrl Pts',(31.1797284184379,-0.118602529514694,
29.1165901942211));
#60160=CARTESIAN_POINT('Ctrl Pts',(31.1696998210424,0.189193535485508,29.1384152356998));
#60161=CARTESIAN_POINT('Ctrl Pts',(31.1357401287962,0.337792934955289,29.1489520437553));
#60162=CARTESIAN_POINT('Ctrl Pts',(31.0124667812232,0.616132121424454,29.1686883723852));
#60163=CARTESIAN_POINT('Ctrl Pts',(30.9235367823029,0.742831293967475,29.1779572331897));
#60164=CARTESIAN_POINT('Ctrl Pts',(30.7007442503466,0.956131495282673,29.1992006935594));
#60165=CARTESIAN_POINT('Ctrl Pts',(30.5686344749746,1.04013508390185,29.2102914886907));
#60166=CARTESIAN_POINT('Ctrl Pts',(30.2847340927663,1.14996876391647,29.231619165161));
#60167=CARTESIAN_POINT('Ctrl Pts',(30.1365034722987,1.17678287240203,29.241562955497));
#60168=CARTESIAN_POINT('Ctrl Pts',(29.8314130542368,1.17348866622216,29.2604146402912));
#60169=CARTESIAN_POINT('Ctrl Pts',(29.6774432972388,1.14080144691636,29.271028448982));
#60170=CARTESIAN_POINT('Ctrl Pts',(29.3937190869037,1.01837161158084,29.2927918879254));
#60171=CARTESIAN_POINT('Ctrl Pts',(29.2662697773694,0.930754504522398,29.3037246074232));
#60172=CARTESIAN_POINT('Ctrl Pts',(29.0548960664095,0.714326580132712,29.3243777540292));
#60173=CARTESIAN_POINT('Ctrl Pts',(28.9719101496403,0.588650269969742,29.3332602962825));
#60174=CARTESIAN_POINT('Ctrl Pts',(28.8542643011592,0.305390771595589,29.3533455118009));
#60175=CARTESIAN_POINT('Ctrl Pts',(28.8237155837947,0.14936986715794,29.3644085600269));
#60176=CARTESIAN_POINT('Ctrl Pts',(28.8258171170069,-0.159374372506235,
29.386300834176));
#60177=CARTESIAN_POINT('Ctrl Pts',(28.8560851449643,-0.309160959864127,
29.3969218227258));
#60178=CARTESIAN_POINT('Ctrl Pts',(28.9721608102066,-0.589863983624277,
29.416825765087));
#60179=CARTESIAN_POINT('Ctrl Pts',(29.0571584178456,-0.717947603677171,
29.4258895505263));
#60180=CARTESIAN_POINT('Ctrl Pts',(29.2735722711375,-0.936836489269234,
29.4469394508198));
#60181=CARTESIAN_POINT('Ctrl Pts',(29.4037270862843,-1.02460346918986,29.4580436226767));
#60182=CARTESIAN_POINT('Ctrl Pts',(29.6852328519168,-1.14214540943397,29.4794975379443));
#60183=CARTESIAN_POINT('Ctrl Pts',(29.8330783756557,-1.1729174993834,29.4896673732243));
#60184=CARTESIAN_POINT('Ctrl Pts',(29.9885051427478,-1.17519832475183,29.4992926332218));
#60185=CARTESIAN_POINT('Ctrl Pts',(29.9942534046712,-1.17524047358085,29.4996471149485));
#60186=CARTESIAN_POINT('Ctrl Pts',(30.,-1.17524047358085,29.5));
#60187=CARTESIAN_POINT('Origin',(30.,-1.21864324187371E-14,15.78125));
#60188=CARTESIAN_POINT('',(30.,-1.17524047358085,30.0625));
#60189=CARTESIAN_POINT('',(29.9999999999998,-1.17524047358085,29.9999999999999));
#60190=CARTESIAN_POINT('',(30.,-1.17524047358085,15.78125));
#60191=CARTESIAN_POINT('Ctrl Pts',(30.,-1.17524047358085,30.0625));
#60192=CARTESIAN_POINT('Ctrl Pts',(29.9263916760993,-1.17524047358085,30.0579798840563));
#60193=CARTESIAN_POINT('Ctrl Pts',(29.8527927358329,-1.1683271801588,30.0532152422529));
#60194=CARTESIAN_POINT('Ctrl Pts',(29.6305589174408,-1.12600740432272,30.0380679862212));
#60195=CARTESIAN_POINT('Ctrl Pts',(29.4879403212856,-1.06872004039491,30.0272790588551));
#60196=CARTESIAN_POINT('Ctrl Pts',(29.229459906818,-0.900978381114361,30.0054593092048));
#60197=CARTESIAN_POINT('Ctrl Pts',(29.1168411945232,-0.790914788798306,
29.9946414903997));
#60198=CARTESIAN_POINT('Ctrl Pts',(28.9451007627829,-0.539025681180781,
29.975164899812));
#60199=CARTESIAN_POINT('Ctrl Pts',(28.885353566283,-0.401177024850609,29.9659464494622));
#60200=CARTESIAN_POINT('Ctrl Pts',(28.8194073352897,-0.10544306552401,29.944976701428));
#60201=CARTESIAN_POINT('Ctrl Pts',(28.8157651951869,0.0500317181756064,
29.9339523772439));
#60202=CARTESIAN_POINT('Ctrl Pts',(28.8690807484143,0.355959077177534,29.9122598409872));
#60203=CARTESIAN_POINT('Ctrl Pts',(28.9264649062036,0.503164977506288,29.9022508807468));
#60204=CARTESIAN_POINT('Ctrl Pts',(29.0920593097175,0.761174070029624,29.8829347271204));
#60205=CARTESIAN_POINT('Ctrl Pts',(29.1966290016669,0.870813111888444,29.8726262318314));
#60206=CARTESIAN_POINT('Ctrl Pts',(29.4460717811045,1.04817985046692,29.851020217295));
#60207=CARTESIAN_POINT('Ctrl Pts',(29.5899284156368,1.11237046788542,29.8399105187383));
#60208=CARTESIAN_POINT('Ctrl Pts',(29.8896511606184,1.17977836078127,29.8191153804746));
#60209=CARTESIAN_POINT('Ctrl Pts',(30.042143785172,1.18417711729498,29.810228885603));
#60210=CARTESIAN_POINT('Ctrl Pts',(30.3412103985985,1.13483145488925,29.7901144124214));
#60211=CARTESIAN_POINT('Ctrl Pts',(30.484863334991,1.08127741540018,29.7793943289302));
#60212=CARTESIAN_POINT('Ctrl Pts',(30.7472520600478,0.920389087318013,29.7575775552199));
#60213=CARTESIAN_POINT('Ctrl Pts',(30.8626628342488,0.813224513564577,29.7466910634298));
#60214=CARTESIAN_POINT('Ctrl Pts',(31.0408533066038,0.565701034414209,29.7269731686955));
#60215=CARTESIAN_POINT('Ctrl Pts',(31.1041185100332,0.42933329828376,29.7179429396888));
#60216=CARTESIAN_POINT('Ctrl Pts',(31.1774532864279,0.13565521801398,29.6971189688454));
#60217=CARTESIAN_POINT('Ctrl Pts',(31.185083485025,-0.0192736961984122,
29.6861333508878));
#60218=CARTESIAN_POINT('Ctrl Pts',(31.1399640096901,-0.325574493297471,
29.6644143350789));
#60219=CARTESIAN_POINT('Ctrl Pts',(31.0867572532099,-0.473736864086508,
29.654106159393));
#60220=CARTESIAN_POINT('Ctrl Pts',(30.9288924580137,-0.735375844574816,
29.6351359699395));
#60221=CARTESIAN_POINT('Ctrl Pts',(30.827743660758,-0.847605887956935,29.6249456831495));
#60222=CARTESIAN_POINT('Ctrl Pts',(30.5841967794232,-1.03154789843284,29.6034686040399));
#60223=CARTESIAN_POINT('Ctrl Pts',(30.4427060183441,-1.0997249484081,29.5923628543371));
#60224=CARTESIAN_POINT('Ctrl Pts',(30.1964052482032,-1.16291170221409,29.5749978904338));
#60225=CARTESIAN_POINT('Ctrl Pts',(30.0983061450535,-1.17524047358085,29.5685367516888));
#60226=CARTESIAN_POINT('Ctrl Pts',(29.9999999999998,-1.17524047358085,29.5625));
#60227=CARTESIAN_POINT('Ctrl Pts',(30.,-1.17524047358085,29.5));
#60228=CARTESIAN_POINT('Ctrl Pts',(30.1499565209686,-1.17524047358085,29.5092084811251));
#60229=CARTESIAN_POINT('Ctrl Pts',(30.2986551183888,-1.14654165825818,29.5193571963421));
#60230=CARTESIAN_POINT('Ctrl Pts',(30.5805418737435,-1.03331719508937,29.5406814366056));
#60231=CARTESIAN_POINT('Ctrl Pts',(30.7104602238272,-0.948696043146186,
29.5516595563353));
#60232=CARTESIAN_POINT('Ctrl Pts',(30.9271652336418,-0.73741304903825,29.5724576785973));
#60233=CARTESIAN_POINT('Ctrl Pts',(31.0130985609625,-0.614031092469691,
29.5814606062707));
#60234=CARTESIAN_POINT('Ctrl Pts',(31.1371264539894,-0.335358891062759,
29.6012205481486));
#60235=CARTESIAN_POINT('Ctrl Pts',(31.1715373282526,-0.181667965902616,
29.6121183834297));
#60236=CARTESIAN_POINT('Ctrl Pts',(31.1782875351469,0.125982959094587,29.6339331333974));
#60237=CARTESIAN_POINT('Ctrl Pts',(31.1521830035108,0.27698654047903,29.6446404159195));
#60238=CARTESIAN_POINT('Ctrl Pts',(31.0441268483734,0.560261316579686,29.6647267147429));
#60239=CARTESIAN_POINT('Ctrl Pts',(30.9634093757068,0.689883113720223,29.6736315391227));
#60240=CARTESIAN_POINT('Ctrl Pts',(30.7540662315648,0.914815989860588,29.6944615256665));
#60241=CARTESIAN_POINT('Ctrl Pts',(30.6261826944801,1.0066730037076,29.7055712306082));
#60242=CARTESIAN_POINT('Ctrl Pts',(30.3474095969538,1.1326991331979,29.7271581352984));
#60243=CARTESIAN_POINT('Ctrl Pts',(30.2000827038505,1.16777128079541,29.7374485757904));
#60244=CARTESIAN_POINT('Ctrl Pts',(29.8935937537322,1.18085135992657,29.7567330869508));
#60245=CARTESIAN_POINT('Ctrl Pts',(29.7372662628443,1.15617395643532,29.7668098469142));
#60246=CARTESIAN_POINT('Ctrl Pts',(29.4460305983855,1.04785975410839,29.7885340948419));
#60247=CARTESIAN_POINT('Ctrl Pts',(29.3136703421255,0.966357190577468,29.7995516007362));
#60248=CARTESIAN_POINT('Ctrl Pts',(29.091570241583,0.760352988788506,29.8204938700552));
#60249=CARTESIAN_POINT('Ctrl Pts',(29.0026423680915,0.639251124272773,29.8296723175212));
#60250=CARTESIAN_POINT('Ctrl Pts',(28.8716938065568,0.363925746310141,29.8491949446027));
#60251=CARTESIAN_POINT('Ctrl Pts',(28.8334229675251,0.211172023558316,29.8600263252283));
#60252=CARTESIAN_POINT('Ctrl Pts',(28.8188892259004,-0.0965571382164996,
29.8818466227683));
#60253=CARTESIAN_POINT('Ctrl Pts',(28.8412989000486,-0.248535346834791,
29.8926230136456));
#60254=CARTESIAN_POINT('Ctrl Pts',(28.942312504556,-0.5340148591211,29.9128656447428));
#60255=CARTESIAN_POINT('Ctrl Pts',(29.0193556498266,-0.664990211735325,
29.9216906330323));
#60256=CARTESIAN_POINT('Ctrl Pts',(29.2225255933627,-0.895077676800941,
29.9423242871271));
#60257=CARTESIAN_POINT('Ctrl Pts',(29.3483400060408,-0.990433515042349,
29.9534309783521));
#60258=CARTESIAN_POINT('Ctrl Pts',(29.6245422330139,-1.1237624473258,29.9751189235115));
#60259=CARTESIAN_POINT('Ctrl Pts',(29.7713190573348,-1.16255586776877,29.985507518588));
#60260=CARTESIAN_POINT('Ctrl Pts',(29.9476315409713,-1.1743662864253,29.9967531815485));
#60261=CARTESIAN_POINT('Ctrl Pts',(29.9738286104226,-1.17524047358085,29.9983928758457));
#60262=CARTESIAN_POINT('Ctrl Pts',(29.9999999999996,-1.17524047358085,29.9999999999999));
#60263=CARTESIAN_POINT('Origin',(30.,-1.21864324187371E-14,15.78125));
#60264=CARTESIAN_POINT('',(30.,-1.17524047358085,30.5625));
#60265=CARTESIAN_POINT('',(29.9999999999998,-1.17524047358085,30.4999999999999));
#60266=CARTESIAN_POINT('',(30.,-1.17524047358085,15.78125));
#60267=CARTESIAN_POINT('Ctrl Pts',(29.9999999999999,-1.17524047358085,30.5625));
#60268=CARTESIAN_POINT('Ctrl Pts',(29.87859718881,-1.17524047358085,30.555044935771));
#60269=CARTESIAN_POINT('Ctrl Pts',(29.7578462794256,-1.15643017462348,30.5469630079231));
#60270=CARTESIAN_POINT('Ctrl Pts',(29.5223698659242,-1.08113291221706,30.5298333797947));
#60271=CARTESIAN_POINT('Ctrl Pts',(29.4096002088597,-1.02391620699781,30.5208799114591));
#60272=CARTESIAN_POINT('Ctrl Pts',(29.1820826863431,-0.858187725726655,
30.5010328956616));
#60273=CARTESIAN_POINT('Ctrl Pts',(29.0755864711026,-0.74226695058618,30.4903833861391));
#60274=CARTESIAN_POINT('Ctrl Pts',(28.9175541454242,-0.481384400712606,
30.4714297273205));
#60275=CARTESIAN_POINT('Ctrl Pts',(28.8652363337421,-0.340257481842474,
30.4616267985498));
#60276=CARTESIAN_POINT('Ctrl Pts',(28.815283295232,-0.0402726424447981,
30.4403556313474));
#60277=CARTESIAN_POINT('Ctrl Pts',(28.8202904087434,0.116033016014593,30.4292723919329));
#60278=CARTESIAN_POINT('Ctrl Pts',(28.8903942350679,0.41669295482916,30.4079533551363));
#60279=CARTESIAN_POINT('Ctrl Pts',(28.9543854043788,0.558153128819785,30.3985868124474));
#60280=CARTESIAN_POINT('Ctrl Pts',(29.1315478521803,0.806074678810529,30.3789179332106));
#60281=CARTESIAN_POINT('Ctrl Pts',(29.2421055811419,0.910792536064214,30.3684162008828));
#60282=CARTESIAN_POINT('Ctrl Pts',(29.5017160718709,1.07586594659562,30.3466216552675));
#60283=CARTESIAN_POINT('Ctrl Pts',(29.6495548172672,1.13268560353193,30.3355287526402));
#60284=CARTESIAN_POINT('Ctrl Pts',(29.9519945282947,1.1837871612187,30.3151448923318));
#60285=CARTESIAN_POINT('Ctrl Pts',(30.1031613914609,1.18026105601431,30.3063430973327));
#60286=CARTESIAN_POINT('Ctrl Pts',(30.3988201345177,1.11599305235349,30.2859088407808));
#60287=CARTESIAN_POINT('Ctrl Pts',(30.5402500629299,1.05480717912897,30.2750546900124));
#60288=CARTESIAN_POINT('Ctrl Pts',(30.7944347031296,0.879976451319597,30.2532473998958));
#60289=CARTESIAN_POINT('Ctrl Pts',(30.9040431118398,0.766951615348157,30.2425094496776));
#60290=CARTESIAN_POINT('Ctrl Pts',(31.0689753458081,0.510549117592882,30.223290918131));
#60291=CARTESIAN_POINT('Ctrl Pts',(31.1250271192607,0.371095429137332,30.2138134394961));
#60292=CARTESIAN_POINT('Ctrl Pts',(31.1830815580213,0.0732292938782705,
30.1926925042524));
#60293=CARTESIAN_POINT('Ctrl Pts',(31.1824563525586,-0.0827153416037653,
30.1816348640652));
#60294=CARTESIAN_POINT('Ctrl Pts',(31.1207993480439,-0.386085590380016,
30.1601236460354));
#60295=CARTESIAN_POINT('Ctrl Pts',(31.0601308144882,-0.530428613118422,
30.1504611573687));
#60296=CARTESIAN_POINT('Ctrl Pts',(30.8888193562276,-0.783487027384905,
30.1309694527541));
#60297=CARTESIAN_POINT('Ctrl Pts',(30.7812795445953,-0.890749011015136,
30.1205628449218));
#60298=CARTESIAN_POINT('Ctrl Pts',(30.5267682373962,-1.06214794901788,30.0988571647179));
#60299=CARTESIAN_POINT('Ctrl Pts',(30.3809100882996,-1.12274761000244,30.0877518706328));
#60300=CARTESIAN_POINT('Ctrl Pts',(30.1523604876879,-1.16783357423751,30.0721187053907));
#60301=CARTESIAN_POINT('Ctrl Pts',(30.0761915030069,-1.17524047358085,30.0671787429637));
#60302=CARTESIAN_POINT('Ctrl Pts',(30.,-1.17524047358085,30.0625));
#60303=CARTESIAN_POINT('Ctrl Pts',(29.9999999999996,-1.17524047358085,29.9999999999999));
#60304=CARTESIAN_POINT('Ctrl Pts',(30.1287289986958,-1.17524047358085,30.0079049483617));
#60305=CARTESIAN_POINT('Ctrl Pts',(30.2567455299606,-1.1540988796436,30.0165156942669));
#60306=CARTESIAN_POINT('Ctrl Pts',(30.5250941977629,-1.06268366593765,30.0362353726713));
#60307=CARTESIAN_POINT('Ctrl Pts',(30.659989580509,-0.984598569323181,30.0472873928126));
#60308=CARTESIAN_POINT('Ctrl Pts',(30.8878392789542,-0.78430373476697,30.0683803131598));
#60309=CARTESIAN_POINT('Ctrl Pts',(30.9799768519055,-0.665589512740196,
30.0778047289255));
#60310=CARTESIAN_POINT('Ctrl Pts',(31.1182025022512,-0.393869611947964,
30.0970717007283));
#60311=CARTESIAN_POINT('Ctrl Pts',(31.16052513775,-0.242215229337512,30.1078251299214));
#60312=CARTESIAN_POINT('Ctrl Pts',(31.183296750852,0.0653802899747305,30.1296359512119));
#60313=CARTESIAN_POINT('Ctrl Pts',(31.1648281646971,0.218291541355271,30.1404785017947));
#60314=CARTESIAN_POINT('Ctrl Pts',(31.0712608350547,0.506051914399227,30.1608828629668));
#60315=CARTESIAN_POINT('Ctrl Pts',(30.9980258995704,0.638460005209143,30.1696826775517));
#60316=CARTESIAN_POINT('Ctrl Pts',(30.8013405043472,0.873851821952036,30.1901061897083));
#60317=CARTESIAN_POINT('Ctrl Pts',(30.6777833777517,0.972810187954768,30.2012019893176));
#60318=CARTESIAN_POINT('Ctrl Pts',(30.4044625790663,1.11370354858798,30.222981179922));
#60319=CARTESIAN_POINT('Ctrl Pts',(30.2583590845709,1.15637148267232,30.2334657933678));
#60320=CARTESIAN_POINT('Ctrl Pts',(29.9547860481489,1.18442751029054,30.2531021983901));
#60321=CARTESIAN_POINT('Ctrl Pts',(29.8001302980418,1.16832333064129,30.2625187720286));
#60322=CARTESIAN_POINT('Ctrl Pts',(29.5050358022508,1.07710916045235,30.2838737217699));
#60323=CARTESIAN_POINT('Ctrl Pts',(29.3676216445827,1.00262104003874,30.2949528877718));
#60324=CARTESIAN_POINT('Ctrl Pts',(29.133885390368,0.808265735464436,30.3161967092816));
#60325=CARTESIAN_POINT('Ctrl Pts',(29.0384365029953,0.691955856048158,30.3259351581227));
#60326=CARTESIAN_POINT('Ctrl Pts',(28.8928615291795,0.423965303949737,30.3449376912299));
#60327=CARTESIAN_POINT('Ctrl Pts',(28.8464607134353,0.273539680594875,30.3556039922081));
#60328=CARTESIAN_POINT('Ctrl Pts',(28.8153257979048,-0.0336925494769084,
30.3773890535762));
#60329=CARTESIAN_POINT('Ctrl Pts',(28.8297608924994,-0.187447360914171,
30.3882914188718));
#60330=CARTESIAN_POINT('Ctrl Pts',(28.915763813331,-0.477469105343294,30.4088561281766));
#60331=CARTESIAN_POINT('Ctrl Pts',(28.9852090680907,-0.611342914279369,
30.4176917737044));
#60332=CARTESIAN_POINT('Ctrl Pts',(29.1753547758778,-0.851973319195576,
30.4378994263954));
#60333=CARTESIAN_POINT('Ctrl Pts',(29.296552814894,-0.954486386260336,30.4489763873607));
#60334=CARTESIAN_POINT('Ctrl Pts',(29.5667870728762,-1.10289061661543,30.4708323290802));
#60335=CARTESIAN_POINT('Ctrl Pts',(29.7121150852083,-1.14942616389095,30.4814064433112));
#60336=CARTESIAN_POINT('Ctrl Pts',(29.9080894843003,-1.17254804864973,30.4942605325068));
#60337=CARTESIAN_POINT('Ctrl Pts',(29.9540678655128,-1.17524047358085,30.497179414468));
#60338=CARTESIAN_POINT('Ctrl Pts',(29.9999999999996,-1.17524047358085,30.4999999999999));
#60339=CARTESIAN_POINT('Origin',(30.,-1.21864324187371E-14,15.78125));
#60340=CARTESIAN_POINT('',(30.8234078741651,-0.838564036615812,30.5625));
#60341=CARTESIAN_POINT('Ctrl Pts',(29.9999999999996,-1.17524047358085,30.4999999999999));
#60342=CARTESIAN_POINT('Ctrl Pts',(30.1063627165445,-1.17524047358085,30.506531487003));
#60343=CARTESIAN_POINT('Ctrl Pts',(30.2124142608556,-1.16080842479057,30.5135555357051));
#60344=CARTESIAN_POINT('Ctrl Pts',(30.4106617155444,-1.10559796456395,30.5276868678729));
#60345=CARTESIAN_POINT('Ctrl Pts',(30.5022820820407,-1.06709869288998,30.5346780045058));
#60346=CARTESIAN_POINT('Ctrl Pts',(30.673678737238,-0.968061456707972,30.5487143145253));
#60347=CARTESIAN_POINT('Ctrl Pts',(30.7527765496958,-0.90791877422844,30.555703810039));
#60348=CARTESIAN_POINT('Ctrl Pts',(30.823407874166,-0.83856403661491,30.5625000000001));
#60349=CARTESIAN_POINT('Origin',(30.,-1.56558793706907E-14,30.5625000000001));
#60350=CARTESIAN_POINT('Origin',(30.,-1.32966554433622E-14,16.));
#60351=CARTESIAN_POINT('Origin',(30.,-1.32966554433622E-14,16.));
#60352=CARTESIAN_POINT('',(31.2041934952953,-0.894381364904537,16.3247595264192));
#60353=CARTESIAN_POINT('Ctrl Pts',(29.1765921258349,-0.838564036615844,
16.));
#60354=CARTESIAN_POINT('Ctrl Pts',(29.2487520159976,-0.936812680701164,
16.0195455809545));
#60355=CARTESIAN_POINT('Ctrl Pts',(29.3353435467743,-1.0235639347367,16.039234228078));
#60356=CARTESIAN_POINT('Ctrl Pts',(29.5376779891223,-1.17276771461038,16.0788670880384));
#60357=CARTESIAN_POINT('Ctrl Pts',(29.6536089107031,-1.23245734148137,16.0985110228563));
#60358=CARTESIAN_POINT('Ctrl Pts',(29.9561347058367,-1.33132329595442,16.1436679915754));
#60359=CARTESIAN_POINT('Ctrl Pts',(30.1342881765676,-1.34356937043143,16.1651272257976));
#60360=CARTESIAN_POINT('Ctrl Pts',(30.4639364648848,-1.31596498262617,16.2103767681647));
#60361=CARTESIAN_POINT('Ctrl Pts',(30.6256204275016,-1.27296147517128,16.233574208582));
#60362=CARTESIAN_POINT('Ctrl Pts',(30.9367837613818,-1.12785658919505,16.2803666131763));
#60363=CARTESIAN_POINT('Ctrl Pts',(31.0819753809162,-1.0232586553723,16.3034869854933));
#60364=CARTESIAN_POINT('Ctrl Pts',(31.2041934952953,-0.894381364904556,
16.3247595264192));
#60365=CARTESIAN_POINT('',(30.2433378840047,-1.48013062741372,16.3247595264192));
#60366=CARTESIAN_POINT('Origin',(30.,-1.32966554433622E-14,16.3247595264192));
#60367=CARTESIAN_POINT('Ctrl Pts',(30.0000000000046,1.33373412263454,16.1584936490537));
#60368=CARTESIAN_POINT('Ctrl Pts',(29.9229566197526,1.33637706265986,16.161136589079));
#60369=CARTESIAN_POINT('Ctrl Pts',(29.8544450638259,1.33215454753135,16.163603109717));
#60370=CARTESIAN_POINT('Ctrl Pts',(29.6282514683273,1.30599264999734,16.1719556820851));
#60371=CARTESIAN_POINT('Ctrl Pts',(29.4645017898244,1.25493599443995,16.1785525854589));
#60372=CARTESIAN_POINT('Ctrl Pts',(29.1556314965168,1.0904442613039,16.1921322573206));
#60373=CARTESIAN_POINT('Ctrl Pts',(29.0151927695643,0.975180135374777,16.1989814826418));
#60374=CARTESIAN_POINT('Ctrl Pts',(28.7777605589636,0.68493937081347,16.2122079855113));
#60375=CARTESIAN_POINT('Ctrl Pts',(28.6970848553023,0.520026749838233,16.218047438772));
#60376=CARTESIAN_POINT('Ctrl Pts',(28.5955913245901,0.191124499754384,16.2305887595464));
#60377=CARTESIAN_POINT('Ctrl Pts',(28.5759298114947,0.010043627653028,16.2373963058958));
#60378=CARTESIAN_POINT('Ctrl Pts',(28.6063542045486,-0.355647637044131,
16.2509482038391));
#60379=CARTESIAN_POINT('Ctrl Pts',(28.6584675525716,-0.536586390481523,
16.2575508938686));
#60380=CARTESIAN_POINT('Ctrl Pts',(28.804769485922,-0.819110586341092,16.2677424893791));
#60381=CARTESIAN_POINT('Ctrl Pts',(28.9031317119719,-0.969713974958467,
16.273653025791));
#60382=CARTESIAN_POINT('Ctrl Pts',(29.199410976174,-1.23941646392093,16.2879449223019));
#60383=CARTESIAN_POINT('Ctrl Pts',(29.3637987944395,-1.33889148571261,16.2948596529243));
#60384=CARTESIAN_POINT('Ctrl Pts',(29.6508112528307,-1.44362228182862,16.3055460935814));
#60385=CARTESIAN_POINT('Ctrl Pts',(29.7632922636866,-1.47020844863719,16.3094443635539));
#60386=CARTESIAN_POINT('Ctrl Pts',(29.9994132050485,-1.49732183809384,16.3170683877131));
#60387=CARTESIAN_POINT('Ctrl Pts',(30.1229027402064,-1.49587628373705,16.3207589898335));
#60388=CARTESIAN_POINT('Ctrl Pts',(30.2433378840021,-1.48013062741405,16.3247595264191));
#60389=CARTESIAN_POINT('Origin',(30.,-1.32966554433622E-14,16.));
#60390=CARTESIAN_POINT('Ctrl Pts',(30.0000000000002,-1.50000000000001,16.8125));
#60391=CARTESIAN_POINT('Ctrl Pts',(29.8374309170617,-1.50000000000001,16.8046783913503));
#60392=CARTESIAN_POINT('Ctrl Pts',(29.6757197620765,-1.47357729444258,16.7961640957352));
#60393=CARTESIAN_POINT('Ctrl Pts',(29.3345753610171,-1.35867108066285,16.7765589388149));
#60394=CARTESIAN_POINT('Ctrl Pts',(29.1621497524653,-1.25967607222118,16.7655132465099));
#60395=CARTESIAN_POINT('Ctrl Pts',(28.8706191056789,-1.00528518925076,16.7444205583108));
#60396=CARTESIAN_POINT('Ctrl Pts',(28.7525289442937,-0.85433413605806,16.7349630075588));
#60397=CARTESIAN_POINT('Ctrl Pts',(28.5748830688675,-0.508513347476126,
16.7157507415264));
#60398=CARTESIAN_POINT('Ctrl Pts',(28.5201083225798,-0.315342861227666,
16.705019047846));
#60399=CARTESIAN_POINT('Ctrl Pts',(28.4893812381258,0.0768796360488758,
16.6832289091084));
#60400=CARTESIAN_POINT('Ctrl Pts',(28.5120877046559,0.272040866827356,16.6723866185096));
#60401=CARTESIAN_POINT('Ctrl Pts',(28.6297398561329,0.63947572665909,16.6519735707412));
#60402=CARTESIAN_POINT('Ctrl Pts',(28.7222788636186,0.808683440996407,16.6431776245867));
#60403=CARTESIAN_POINT('Ctrl Pts',(28.9715826684579,1.11011928821307,16.6228097717056));
#60404=CARTESIAN_POINT('Ctrl Pts',(29.1285972489479,1.2371944826493,16.6117255376675));
#60405=CARTESIAN_POINT('Ctrl Pts',(29.4764211128784,1.41875808710319,16.5899474207545));
#60406=CARTESIAN_POINT('Ctrl Pts',(29.6625283053455,1.47415762233606,16.5794544583034));
#60407=CARTESIAN_POINT('Ctrl Pts',(30.0492497355351,1.51196727264003,16.5597980467542));
#60408=CARTESIAN_POINT('Ctrl Pts',(30.2463054645629,1.49258742024928,16.5504437178179));
#60409=CARTESIAN_POINT('Ctrl Pts',(30.6231564270347,1.37865583779414,16.529147701253));
#60410=CARTESIAN_POINT('Ctrl Pts',(30.7990856424485,1.28470816478719,16.5180736453463));
#60411=CARTESIAN_POINT('Ctrl Pts',(31.0988336211311,1.03864170876325,16.4968168346638));
#60412=CARTESIAN_POINT('Ctrl Pts',(31.2215556301223,0.891049402060874,16.4870027445589));
#60413=CARTESIAN_POINT('Ctrl Pts',(31.4094506590971,0.550436181771672,16.4680797878762));
#60414=CARTESIAN_POINT('Ctrl Pts',(31.4699049158396,0.359005410515039,16.4574447450286));
#60415=CARTESIAN_POINT('Ctrl Pts',(31.5122933091642,-0.0326520383467692,
16.4356859978696));
#60416=CARTESIAN_POINT('Ctrl Pts',(31.4952196858866,-0.228959953862231,
16.4247800025632));
#60417=CARTESIAN_POINT('Ctrl Pts',(31.3881172406464,-0.599526626811694,
16.4041929651771));
#60418=CARTESIAN_POINT('Ctrl Pts',(31.300844426577,-0.770779121647004,16.3953430421646));
#60419=CARTESIAN_POINT('Ctrl Pts',(31.0690211851343,-1.06871793972269,16.3759133629805));
#60420=CARTESIAN_POINT('Ctrl Pts',(30.9276174608134,-1.1935139431374,16.3656435174717));
#60421=CARTESIAN_POINT('Ctrl Pts',(30.6058972740411,-1.3849221656676,16.3448478526983));
#60422=CARTESIAN_POINT('Ctrl Pts',(30.4282952255496,-1.44972308953241,16.3345029444933));
#60423=CARTESIAN_POINT('Ctrl Pts',(30.2433378840032,-1.48013062741398,16.3247595264191));
#60424=CARTESIAN_POINT('Ctrl Pts',(31.2041934952953,-0.894381364904531,
16.3247595264192));
#60425=CARTESIAN_POINT('Ctrl Pts',(31.2978308567217,-0.768308186313297,
16.33276668881));
#60426=CARTESIAN_POINT('Ctrl Pts',(31.3710758402094,-0.628345765505124,
16.3400919019164));
#60427=CARTESIAN_POINT('Ctrl Pts',(31.4735871865681,-0.324510524004584,
16.3569716375553));
#60428=CARTESIAN_POINT('Ctrl Pts',(31.5001727925959,-0.161986730686535,
16.3660007371841));
#60429=CARTESIAN_POINT('Ctrl Pts',(31.4997859079869,0.202485940247452,16.3862492189027));
#60430=CARTESIAN_POINT('Ctrl Pts',(31.4592164909323,0.401327421311596,16.3972959678507));
#60431=CARTESIAN_POINT('Ctrl Pts',(31.3063109849155,0.761415726638002,16.4173008737022));
#60432=CARTESIAN_POINT('Ctrl Pts',(31.1993149527403,0.920789441682028,16.4262087502572));
#60433=CARTESIAN_POINT('Ctrl Pts',(30.927737201713,1.19478997630558,16.4468861668575));
#60434=CARTESIAN_POINT('Ctrl Pts',(30.7642938567671,1.30539963746525,16.4578223290454));
#60435=CARTESIAN_POINT('Ctrl Pts',(30.4012071029328,1.45894804482998,16.4795565821721));
#60436=CARTESIAN_POINT('Ctrl Pts',(30.2045613271838,1.49922584611532,16.4901365342825));
#60437=CARTESIAN_POINT('Ctrl Pts',(29.8153532439137,1.50071981302521,16.5089038160006));
#60438=CARTESIAN_POINT('Ctrl Pts',(29.6264615866043,1.46518905889,16.5189388458803));
#60439=CARTESIAN_POINT('Ctrl Pts',(29.2652001883276,1.32257698188105,16.5402814895924));
#60440=CARTESIAN_POINT('Ctrl Pts',(29.0973517156097,1.21423683760981,16.5513665514533));
#60441=CARTESIAN_POINT('Ctrl Pts',(28.8152158635768,0.940440031832944,16.5725462857904));
#60442=CARTESIAN_POINT('Ctrl Pts',(28.7029935775965,0.778399491568193,16.5817555838018));
#60443=CARTESIAN_POINT('Ctrl Pts',(28.5479560175053,0.422736814401416,16.6015146214222));
#60444=CARTESIAN_POINT('Ctrl Pts',(28.5057189580682,0.232905312381588,16.6120608159788));
#60445=CARTESIAN_POINT('Ctrl Pts',(28.4951590610144,-0.159927799856357,
16.6338848777698));
#60446=CARTESIAN_POINT('Ctrl Pts',(28.5299387266544,-0.359247208886169,
16.6449581782715));
#60447=CARTESIAN_POINT('Ctrl Pts',(28.6722713443677,-0.723556115441905,
16.665197561969));
#60448=CARTESIAN_POINT('Ctrl Pts',(28.7749427214916,-0.886360478602884,
16.6740138619457));
#60449=CARTESIAN_POINT('Ctrl Pts',(29.0386829229376,-1.16785093047933,16.6945222475229));
#60450=CARTESIAN_POINT('Ctrl Pts',(29.1984334219549,-1.28276611305493,16.7054003353954));
#60451=CARTESIAN_POINT('Ctrl Pts',(29.5564186818177,-1.44663336596446,16.7271757773774));
#60452=CARTESIAN_POINT('Ctrl Pts',(29.7518446854206,-1.49263399091841,16.7378560104973));
#60453=CARTESIAN_POINT('Ctrl Pts',(29.9670564156215,-1.49972884223086,16.7484074688974));
#60454=CARTESIAN_POINT('Ctrl Pts',(29.9835330897433,-1.50000000000001,16.7492077354109));
#60455=CARTESIAN_POINT('Ctrl Pts',(30.,-1.50000000000001,16.75));
#60456=CARTESIAN_POINT('Origin',(27.4975425688509,1.03655180724329,15.7235432561772));
#60457=CARTESIAN_POINT('',(27.507537153458,1.0459948352816,31.5905494329235));
#60458=CARTESIAN_POINT('',(27.4979325782409,1.02280733953167,31.5905494329235));
#60459=CARTESIAN_POINT('Origin',(27.4975191258909,1.03656151763528,31.5962151370756));
#60460=CARTESIAN_POINT('',(27.4979325782409,1.02280733953167,33.8969505670765));
#60461=CARTESIAN_POINT('',(27.4979325782409,1.02280733953167,15.7235432561772));
#60462=CARTESIAN_POINT('',(27.507537153458,1.0459948352816,33.8969505670765));
#60463=CARTESIAN_POINT('Origin',(27.4975191258914,1.03656151763504,33.891284862925));
#60464=CARTESIAN_POINT('',(27.507537153458,1.0459948352816,15.7235432561772));
#60465=CARTESIAN_POINT('Origin',(27.4239298924869,0.837015916807854,15.7235432561772));
#60466=CARTESIAN_POINT('',(27.4331527756843,0.847214001212616,31.5905494329235));
#60467=CARTESIAN_POINT('',(27.4253970781159,0.823344418487269,31.5905494329235));
#60468=CARTESIAN_POINT('Origin',(27.4239057599253,0.837023757952457,31.5962151370753));
#60469=CARTESIAN_POINT('',(27.4253970781159,0.823344418487269,33.8969505670765));
#60470=CARTESIAN_POINT('',(27.4253970781159,0.823344418487269,15.7235432561772));
#60471=CARTESIAN_POINT('',(27.4331527756843,0.847214001212616,33.8969505670765));
#60472=CARTESIAN_POINT('Origin',(27.4239057599256,0.837023757952334,33.8912848629251));
#60473=CARTESIAN_POINT('',(27.4331527756843,0.847214001212616,15.7235432561772));
#60474=CARTESIAN_POINT('Origin',(27.3661995449658,0.632319544909263,15.7235432561772));
#60475=CARTESIAN_POINT('',(27.3745938646118,0.643209811098917,31.5905494329235));
#60476=CARTESIAN_POINT('',(27.3687348611468,0.618805305313091,31.5905494329235));
#60477=CARTESIAN_POINT('Origin',(27.3661748715877,0.632325468463276,31.5962151370755));
#60478=CARTESIAN_POINT('',(27.3687348611468,0.618805305313091,33.8969505670765));
#60479=CARTESIAN_POINT('',(27.3687348611468,0.618805305313091,15.7235432561772));
#60480=CARTESIAN_POINT('',(27.3745938646118,0.643209811098917,33.8969505670765));
#60481=CARTESIAN_POINT('Origin',(27.3661748715881,0.632325468463155,33.891284862925));
#60482=CARTESIAN_POINT('',(27.3745938646118,0.643209811098917,15.7235432561772));
#60483=CARTESIAN_POINT('Origin',(27.3247074530776,0.423724712748722,15.7235432561772));
#60484=CARTESIAN_POINT('',(27.3322214554001,0.435240018610828,31.5905494329235));
#60485=CARTESIAN_POINT('',(27.328295268743,0.410451051658016,31.5905494329235));
#60486=CARTESIAN_POINT('Origin',(27.3246823910025,0.423728682191457,31.5962151370754));
#60487=CARTESIAN_POINT('',(27.328295268743,0.410451051658016,33.8969505670765));
#60488=CARTESIAN_POINT('',(27.328295268743,0.410451051658016,15.7235432561772));
#60489=CARTESIAN_POINT('',(27.3322214554001,0.435240018610828,33.8969505670765));
#60490=CARTESIAN_POINT('Origin',(27.3246823910029,0.423728682191396,33.891284862925));
#60491=CARTESIAN_POINT('',(27.3322214554001,0.435240018610828,15.7235432561772));
#60492=CARTESIAN_POINT('Origin',(27.2997094293662,0.212517476831317,15.7235432561772));
#60493=CARTESIAN_POINT('',(27.3062967880422,0.224586826676008,31.5905494329235));
#60494=CARTESIAN_POINT('',(27.3043276244395,0.199566230780642,31.5905494329235));
#60495=CARTESIAN_POINT('Origin',(27.2996841331102,0.212519467689854,31.5962151370755));
#60496=CARTESIAN_POINT('',(27.3043276244395,0.199566230780642,33.8969505670765));
#60497=CARTESIAN_POINT('',(27.3043276244395,0.199566230780642,15.7235432561772));
#60498=CARTESIAN_POINT('',(27.3062967880422,0.224586826676008,33.8969505670765));
#60499=CARTESIAN_POINT('Origin',(27.2996841331108,0.212519467689809,33.8912848629251));
#60500=CARTESIAN_POINT('',(27.3062967880422,0.224586826676008,15.7235432561772));
#60501=CARTESIAN_POINT('Origin',(27.2913595949605,1.54398896472578E-14,
15.7235432561772));
#60502=CARTESIAN_POINT('',(27.2969796967333,0.0125489822720319,31.5905494329235));
#60503=CARTESIAN_POINT('',(27.2969796967333,-0.0125489822720016,31.5905494329235));
#60504=CARTESIAN_POINT('Origin',(27.2913342204835,1.66533453693773E-14,
31.5962151370755));
#60505=CARTESIAN_POINT('',(27.2969796967333,-0.0125489822720016,33.8969505670765));
#60506=CARTESIAN_POINT('',(27.2969796967333,-0.0125489822720016,15.7235432561772));
#60507=CARTESIAN_POINT('',(27.2969796967333,0.0125489822720319,33.8969505670765));
#60508=CARTESIAN_POINT('Origin',(27.2913342204839,1.44047100636424E-14,
33.891284862925));
#60509=CARTESIAN_POINT('',(27.2969796967333,0.0125489822720319,15.7235432561772));
#60510=CARTESIAN_POINT('Origin',(27.5865837274296,1.22969701109861,15.7235432561772));
#60511=CARTESIAN_POINT('',(27.5972883935087,1.23832676336248,31.5905494329235));
#60512=CARTESIAN_POINT('',(27.5858941560429,1.2159643132099,31.5905494329235));
#60513=CARTESIAN_POINT('Origin',(27.586561118605,1.22970853087013,31.5962151370754));
#60514=CARTESIAN_POINT('',(27.5858941560429,1.2159643132099,33.8969505670765));
#60515=CARTESIAN_POINT('',(27.5858941560429,1.2159643132099,15.7235432561772));
#60516=CARTESIAN_POINT('',(27.5972883935087,1.23832676336248,33.8969505670765));
#60517=CARTESIAN_POINT('Origin',(27.5865611186055,1.22970853086989,33.891284862925));
#60518=CARTESIAN_POINT('',(27.5972883935087,1.23832676336248,15.7235432561772));
#60519=CARTESIAN_POINT('Origin',(27.690504399871,1.41526072396476,15.7235432561772));
#60520=CARTESIAN_POINT('',(27.701853149596,1.42302399516181,31.5905494329235));
#60521=CARTESIAN_POINT('',(27.6887394991445,1.40162446254803,31.5905494329235));
#60522=CARTESIAN_POINT('Origin',(27.6904827645727,1.41527398209261,31.5962151370755));
#60523=CARTESIAN_POINT('',(27.6887394991445,1.40162446254803,33.8969505670765));
#60524=CARTESIAN_POINT('',(27.6887394991445,1.40162446254803,15.7235432561772));
#60525=CARTESIAN_POINT('',(27.701853149596,1.42302399516181,33.8969505670765));
#60526=CARTESIAN_POINT('Origin',(27.6904827645732,1.41527398209234,33.891284862925));
#60527=CARTESIAN_POINT('',(27.701853149596,1.42302399516181,15.7235432561772));
#60528=CARTESIAN_POINT('Origin',(27.8086638806724,1.59209888384573,15.7235432561772));
#60529=CARTESIAN_POINT('',(27.8205867452275,1.59894781082746,31.5905494329235));
#60530=CARTESIAN_POINT('',(27.805834531806,1.57864313098712,31.5905494329235));
#60531=CARTESIAN_POINT('Origin',(27.8086433522893,1.59211379858911,31.5962151370755));
#60532=CARTESIAN_POINT('',(27.805834531806,1.57864313098712,33.8969505670765));
#60533=CARTESIAN_POINT('',(27.805834531806,1.57864313098712,15.7235432561772));
#60534=CARTESIAN_POINT('',(27.8205867452275,1.59894781082746,33.8969505670765));
#60535=CARTESIAN_POINT('Origin',(27.8086433522896,1.59211379858882,33.8912848629251));
#60536=CARTESIAN_POINT('',(27.8205867452275,1.59894781082746,15.7235432561772));
#60537=CARTESIAN_POINT('Origin',(27.9403336773427,1.75912122468118,15.7235432561772));
#60538=CARTESIAN_POINT('',(27.9527571483031,1.76501358153527,31.5905494329235));
#60539=CARTESIAN_POINT('',(27.9364573242129,1.74592893957157,31.5905494329235));
#60540=CARTESIAN_POINT('Origin',(27.9403143824389,1.75913770408581,31.5962151370755));
#60541=CARTESIAN_POINT('',(27.9364573242129,1.74592893957157,33.8969505670765));
#60542=CARTESIAN_POINT('',(27.9364573242129,1.74592893957157,15.7235432561772));
#60543=CARTESIAN_POINT('',(27.9527571483031,1.76501358153527,33.8969505670765));
#60544=CARTESIAN_POINT('Origin',(27.9403143824393,1.75913770408551,33.891284862925));
#60545=CARTESIAN_POINT('',(27.9527571483031,1.76501358153527,15.7235432561772));
#60546=CARTESIAN_POINT('Origin',(28.0847020018007,1.9152979981993,15.7235432561772));
#60547=CARTESIAN_POINT('',(28.0975494843367,1.92019745658633,31.5905494329235));
#60548=CARTESIAN_POINT('',(28.0798025434137,1.90245051566326,31.5905494329235));
#60549=CARTESIAN_POINT('Origin',(28.0846840593359,1.9153159406641,31.5962151370755));
#60550=CARTESIAN_POINT('',(28.0798025434137,1.90245051566326,33.8969505670765));
#60551=CARTESIAN_POINT('',(28.0798025434137,1.90245051566326,15.7235432561772));
#60552=CARTESIAN_POINT('',(28.0975494843367,1.92019745658633,33.8969505670765));
#60553=CARTESIAN_POINT('Origin',(28.0846840593363,1.91531594066375,33.891284862925));
#60554=CARTESIAN_POINT('',(28.0975494843367,1.92019745658633,15.7235432561772));
#60555=CARTESIAN_POINT('Origin',(28.2408787753188,2.05966632265731,15.7235432561772));
#60556=CARTESIAN_POINT('',(28.2540710604285,2.06354267578708,31.5905494329235));
#60557=CARTESIAN_POINT('',(28.2349864184648,2.0472428516969,31.5905494329235));
#60558=CARTESIAN_POINT('Origin',(28.2408622959143,2.05968561756092,31.5962151370754));
#60559=CARTESIAN_POINT('',(28.2349864184648,2.0472428516969,33.8969505670765));
#60560=CARTESIAN_POINT('',(28.2349864184648,2.0472428516969,15.7235432561772));
#60561=CARTESIAN_POINT('',(28.2540710604285,2.06354267578708,33.8969505670765));
#60562=CARTESIAN_POINT('Origin',(28.2408622959145,2.05968561756065,33.891284862925));
#60563=CARTESIAN_POINT('',(28.2540710604285,2.06354267578708,15.7235432561772));
#60564=CARTESIAN_POINT('Origin',(28.4079011161543,2.19133611932758,15.7235432561772));
#60565=CARTESIAN_POINT('',(28.4213568690129,2.19416546819404,31.5905494329235));
#60566=CARTESIAN_POINT('',(28.4010521891726,2.1794132547725,31.5905494329235));
#60567=CARTESIAN_POINT('Origin',(28.407886201411,2.19135664771063,31.5962151370753));
#60568=CARTESIAN_POINT('',(28.4010521891726,2.1794132547725,33.8969505670765));
#60569=CARTESIAN_POINT('',(28.4010521891726,2.1794132547725,15.7235432561772));
#60570=CARTESIAN_POINT('',(28.4213568690129,2.19416546819404,33.8969505670765));
#60571=CARTESIAN_POINT('Origin',(28.4078862014112,2.19135664771024,33.8912848629252));
#60572=CARTESIAN_POINT('',(28.4213568690129,2.19416546819404,15.7235432561772));
#60573=CARTESIAN_POINT('Origin',(28.5847392760353,2.309495600129,15.7235432561772));
#60574=CARTESIAN_POINT('',(28.598375537452,2.31126050085552,31.5905494329235));
#60575=CARTESIAN_POINT('',(28.5769760048382,2.29814685040398,31.5905494329235));
#60576=CARTESIAN_POINT('Origin',(28.5847260179075,2.30951723542729,31.5962151370754));
#60577=CARTESIAN_POINT('',(28.5769760048382,2.29814685040398,33.8969505670765));
#60578=CARTESIAN_POINT('',(28.5769760048382,2.29814685040398,15.7235432561772));
#60579=CARTESIAN_POINT('',(28.598375537452,2.31126050085552,33.8969505670765));
#60580=CARTESIAN_POINT('Origin',(28.5847260179077,2.30951723542689,33.891284862925));
#60581=CARTESIAN_POINT('',(28.598375537452,2.31126050085552,15.7235432561772));
#60582=CARTESIAN_POINT('Origin',(28.7703029889014,2.4134162725704,15.7235432561772));
#60583=CARTESIAN_POINT('',(28.7840356867901,2.41410584395713,31.5905494329235));
#60584=CARTESIAN_POINT('',(28.7616732366375,2.40271160649133,31.5905494329235));
#60585=CARTESIAN_POINT('Origin',(28.7702914691299,2.41343888139489,31.5962151370753));
#60586=CARTESIAN_POINT('',(28.7616732366375,2.40271160649133,33.8969505670765));
#60587=CARTESIAN_POINT('',(28.7616732366375,2.40271160649133,15.7235432561772));
#60588=CARTESIAN_POINT('',(28.7840356867901,2.41410584395713,33.8969505670765));
#60589=CARTESIAN_POINT('Origin',(28.7702914691301,2.41343888139455,33.8912848629251));
#60590=CARTESIAN_POINT('',(28.7840356867901,2.41410584395713,15.7235432561772));
#60591=CARTESIAN_POINT('Origin',(30.,-1.32966554433622E-14,34.));
#60592=CARTESIAN_POINT('',(28.75,0.721687836487017,33.8917468245269));
#60593=CARTESIAN_POINT('',(28.75,-1.44824191072421E-14,33.6983711515529));
#60594=CARTESIAN_POINT('Ctrl Pts',(28.75,0.72168783648698,33.8917468245269));
#60595=CARTESIAN_POINT('Ctrl Pts',(28.75,0.334936490538873,33.6983711515529));
#60596=CARTESIAN_POINT('Ctrl Pts',(28.75,-1.55145598201422E-14,33.6983711515529));
#60597=CARTESIAN_POINT('',(30.,1.44337567297405,33.8917468245269));
#60598=CARTESIAN_POINT('Ctrl Pts',(30.,1.44337567297404,33.8917468245269));
#60599=CARTESIAN_POINT('Ctrl Pts',(29.375,1.08253175473053,33.5309029062834));
#60600=CARTESIAN_POINT('Ctrl Pts',(28.75,0.721687836487025,33.8917468245269));
#60601=CARTESIAN_POINT('',(31.25,0.721687836487017,33.891746824527));
#60602=CARTESIAN_POINT('Ctrl Pts',(31.25,0.721687836487027,33.8917468245269));
#60603=CARTESIAN_POINT('Ctrl Pts',(30.625,1.08253175473053,33.5309029062834));
#60604=CARTESIAN_POINT('Ctrl Pts',(30.,1.44337567297404,33.8917468245269));
#60605=CARTESIAN_POINT('',(31.25,-0.72168783648704,33.8917468245269));
#60606=CARTESIAN_POINT('Ctrl Pts',(31.25,-0.721687836487026,33.8917468245269));
#60607=CARTESIAN_POINT('Ctrl Pts',(31.25,-1.26287869051112E-14,33.5309029062834));
#60608=CARTESIAN_POINT('Ctrl Pts',(31.25,0.721687836487001,33.8917468245269));
#60609=CARTESIAN_POINT('',(30.,-1.44337567297407,33.8917468245269));
#60610=CARTESIAN_POINT('Ctrl Pts',(30.,-1.44337567297406,33.8917468245269));
#60611=CARTESIAN_POINT('Ctrl Pts',(30.625,-1.08253175473056,33.5309029062834));
#60612=CARTESIAN_POINT('Ctrl Pts',(31.25,-0.721687836487049,33.8917468245269));
#60613=CARTESIAN_POINT('',(28.75,-0.721687836487044,33.8917468245269));
#60614=CARTESIAN_POINT('Ctrl Pts',(28.75,-0.721687836487053,33.8917468245269));
#60615=CARTESIAN_POINT('Ctrl Pts',(29.375,-1.08253175473056,33.5309029062834));
#60616=CARTESIAN_POINT('Ctrl Pts',(30.,-1.44337567297406,33.8917468245269));
#60617=CARTESIAN_POINT('Ctrl Pts',(28.75,-1.55145598201422E-14,33.6983711515529));
#60618=CARTESIAN_POINT('Ctrl Pts',(28.75,-0.334936490538901,33.6983711515529));
#60619=CARTESIAN_POINT('Ctrl Pts',(28.75,-0.721687836487005,33.8917468245269));
#60620=CARTESIAN_POINT('',(28.4483711515529,-1.34873480853811E-14,34.));
#60621=CARTESIAN_POINT('',(28.4483711515529,-1.34873480853811E-14,34.));
#60622=CARTESIAN_POINT('Origin',(30.,-1.32966554433622E-14,34.));
#60623=CARTESIAN_POINT('Origin',(30.,-1.32966554433622E-14,33.953125));
#60624=CARTESIAN_POINT('',(30.,-2.6137293696319,33.9862706303681));
#60625=CARTESIAN_POINT('Origin',(30.,-1.32966554433622E-14,33.9862706303681));
#60626=CARTESIAN_POINT('',(30.,-2.58058373926378,34.));
#60627=CARTESIAN_POINT('Origin',(30.,-2.58058373926378,33.953125));
#60628=CARTESIAN_POINT('Origin',(30.,-1.32966554433622E-14,34.));
#60629=CARTESIAN_POINT('Origin',(30.,-1.32966554433622E-14,33.8637293696319));
#60630=CARTESIAN_POINT('',(30.012548982272,-2.70302030326669,33.8969505670765));
#60631=CARTESIAN_POINT('',(30.,-2.69489040503949,33.9051095949605));
#60632=CARTESIAN_POINT('Ctrl Pts',(30.012548982272,-2.70302030326672,33.8969505670765));
#60633=CARTESIAN_POINT('Ctrl Pts',(30.0117595027242,-2.70125749446881,33.8987170220581));
#60634=CARTESIAN_POINT('Ctrl Pts',(30.0105608813139,-2.69960157002983,33.9003782103613));
#60635=CARTESIAN_POINT('Ctrl Pts',(30.0079476416933,-2.69733049287042,33.9026580100842));
#60636=CARTESIAN_POINT('Ctrl Pts',(30.0065751610721,-2.69644647069985,33.9035459832655));
#60637=CARTESIAN_POINT('Ctrl Pts',(30.0034509360646,-2.69522714758869,33.9047710768107));
#60638=CARTESIAN_POINT('Ctrl Pts',(30.0017003028408,-2.69489040503949,33.9051095949605));
#60639=CARTESIAN_POINT('Ctrl Pts',(30.,-2.69489040503949,33.9051095949605));
#60640=CARTESIAN_POINT('',(30.027378900953,-2.73613365141358,33.8637293696319));
#60641=CARTESIAN_POINT('Ctrl Pts',(30.0273789009518,-2.73613365141079,33.8637293696347));
#60642=CARTESIAN_POINT('Ctrl Pts',(30.019918653996,-2.71947585577342,33.8804609779984));
#60643=CARTESIAN_POINT('Ctrl Pts',(30.0125489822686,-2.70302030325915,33.8969505670841));
#60644=CARTESIAN_POINT('',(30.1873800711417,-2.72984718831552,33.8637293696319));
#60645=CARTESIAN_POINT('Origin',(30.,-1.32966554433622E-14,33.8637293696319));
#60646=CARTESIAN_POINT('',(30.1995662307806,-2.69567237556051,33.8969505670765));
#60647=CARTESIAN_POINT('Ctrl Pts',(30.1995662307834,-2.69567237555272,33.8969505670841));
#60648=CARTESIAN_POINT('Ctrl Pts',(30.1935103650644,-2.71265541886991,33.8804609779983));
#60649=CARTESIAN_POINT('Ctrl Pts',(30.1873800711428,-2.72984718831265,33.8637293696347));
#60650=CARTESIAN_POINT('',(30.224586826676,-2.69370321195777,33.8969505670765));
#60651=CARTESIAN_POINT('Origin',(30.2125187883694,-2.70030745889015,33.8912937927563));
#60652=CARTESIAN_POINT('',(30.241969073019,-2.72555094069392,33.8637293696319));
#60653=CARTESIAN_POINT('Ctrl Pts',(30.2419690730176,-2.72555094069121,33.8637293696347));
#60654=CARTESIAN_POINT('Ctrl Pts',(30.233224867931,-2.70952981970859,33.8804609779984));
#60655=CARTESIAN_POINT('Ctrl Pts',(30.2245868266721,-2.69370321195052,33.8969505670841));
#60656=CARTESIAN_POINT('',(30.4009837827878,-2.70673030953518,33.8637293696319));
#60657=CARTESIAN_POINT('Origin',(30.,-1.32966554433622E-14,33.8637293696319));
#60658=CARTESIAN_POINT('',(30.410451051658,-2.67170473125697,33.8969505670765));
#60659=CARTESIAN_POINT('Ctrl Pts',(30.4104510516601,-2.67170473124899,33.8969505670841));
#60660=CARTESIAN_POINT('Ctrl Pts',(30.4057463283755,-2.68911055925959,33.8804609779983));
#60661=CARTESIAN_POINT('Ctrl Pts',(30.4009837827886,-2.70673030953223,33.8637293696347));
#60662=CARTESIAN_POINT('',(30.4352400186108,-2.66777854459992,33.8969505670765));
#60663=CARTESIAN_POINT('Origin',(30.4237273077484,-2.67530902338216,33.8912940899387));
#60664=CARTESIAN_POINT('',(30.455067425287,-2.69816430208722,33.8637293696319));
#60665=CARTESIAN_POINT('Ctrl Pts',(30.4550674252854,-2.69816430208464,33.8637293696347));
#60666=CARTESIAN_POINT('Ctrl Pts',(30.445093173,-2.68287863129519,33.8804609779983));
#60667=CARTESIAN_POINT('Ctrl Pts',(30.4352400186063,-2.667778544593,33.8969505670841));
#60668=CARTESIAN_POINT('',(30.6121152960723,-2.66692553831739,33.8637293696319));
#60669=CARTESIAN_POINT('Origin',(30.,-1.32966554433622E-14,33.8637293696319));
#60670=CARTESIAN_POINT('',(30.618805305313,-2.63126513885325,33.8969505670765));
#60671=CARTESIAN_POINT('Ctrl Pts',(30.6188053053145,-2.63126513884514,33.8969505670841));
#60672=CARTESIAN_POINT('Ctrl Pts',(30.6154807306477,-2.64898643883144,33.8804609779984));
#60673=CARTESIAN_POINT('Ctrl Pts',(30.6121152960728,-2.66692553831439,33.8637293696347));
#60674=CARTESIAN_POINT('',(30.6432098110989,-2.62540613538822,33.8969505670765));
#60675=CARTESIAN_POINT('Origin',(30.6323233823986,-2.63381649164655,33.8912943077151));
#60676=CARTESIAN_POINT('',(30.6653601355529,-2.65414258332748,33.8637293696319));
#60677=CARTESIAN_POINT('Ctrl Pts',(30.665360135551,-2.65414258332505,33.8637293696347));
#60678=CARTESIAN_POINT('Ctrl Pts',(30.6542173306489,-2.63968660397218,33.8804609779983));
#60679=CARTESIAN_POINT('Ctrl Pts',(30.6432098110939,-2.62540613538168,33.8969505670841));
#60680=CARTESIAN_POINT('',(30.8194729150075,-2.61067828431314,33.8637293696319));
#60681=CARTESIAN_POINT('Origin',(30.,-1.32966554433622E-14,33.8637293696319));
#60682=CARTESIAN_POINT('',(30.8233444184872,-2.57460292188405,33.8969505670765));
#60683=CARTESIAN_POINT('Ctrl Pts',(30.8233444184881,-2.57460292187584,33.8969505670841));
#60684=CARTESIAN_POINT('Ctrl Pts',(30.8214204895475,-2.59253043613051,33.8804609779984));
#60685=CARTESIAN_POINT('Ctrl Pts',(30.8194729150079,-2.61067828431011,33.8637293696347));
#60686=CARTESIAN_POINT('',(30.8472140012126,-2.56684722431573,33.8969505670765));
#60687=CARTESIAN_POINT('Origin',(30.837020957759,-2.57608565616367,33.891294472568));
#60688=CARTESIAN_POINT('',(30.8715506793283,-2.59375719294955,33.8637293696319));
#60689=CARTESIAN_POINT('Ctrl Pts',(30.8715506793263,-2.59375719294726,33.8637293696347));
#60690=CARTESIAN_POINT('Ctrl Pts',(30.8593080209051,-2.58022003095079,33.8804609779983));
#60691=CARTESIAN_POINT('Ctrl Pts',(30.8472140012071,-2.5668472243096,33.8969505670841));
#60692=CARTESIAN_POINT('',(31.0217782109194,-2.53833533054748,33.8637293696319));
#60693=CARTESIAN_POINT('Origin',(30.,-1.32966554433622E-14,33.8637293696319));
#60694=CARTESIAN_POINT('',(31.0228073395316,-2.5020674217591,33.8969505670765));
#60695=CARTESIAN_POINT('Ctrl Pts',(31.0228073395319,-2.50206742175084,33.8969505670841));
#60696=CARTESIAN_POINT('Ctrl Pts',(31.0222959179792,-2.52009062118698,33.8804609779983));
#60697=CARTESIAN_POINT('Ctrl Pts',(31.0217782109195,-2.53833533054442,33.8637293696347));
#60698=CARTESIAN_POINT('',(31.0459948352815,-2.49246284654201,33.8969505670765));
#60699=CARTESIAN_POINT('Origin',(31.0365580110689,-2.50247243285094,33.8912946002427));
#60700=CARTESIAN_POINT('',(31.0723678233457,-2.51738042696529,33.8637293696319));
#60701=CARTESIAN_POINT('Ctrl Pts',(31.0723678233435,-2.51738042696321,33.8637293696347));
#60702=CARTESIAN_POINT('Ctrl Pts',(31.0591007914634,-2.5048455434284,33.8804609779984));
#60703=CARTESIAN_POINT('Ctrl Pts',(31.0459948352755,-2.49246284653634,33.8969505670841));
#60704=CARTESIAN_POINT('',(31.2177839043851,-2.45034269538684,33.8637293696319));
#60705=CARTESIAN_POINT('Origin',(30.,-1.32966554433622E-14,33.8637293696319));
#60706=CARTESIAN_POINT('',(31.2159643132098,-2.41410584395714,33.8969505670765));
#60707=CARTESIAN_POINT('Ctrl Pts',(31.2159643132094,-2.4141058439489,33.8969505670841));
#60708=CARTESIAN_POINT('Ctrl Pts',(31.2168685521286,-2.43211360954869,33.8804609779984));
#60709=CARTESIAN_POINT('Ctrl Pts',(31.2177839043849,-2.4503426953838,33.8637293696347));
#60710=CARTESIAN_POINT('',(31.2383267633624,-2.40271160649135,33.8969505670765));
#60711=CARTESIAN_POINT('Origin',(31.2297043338602,-2.41343066267494,33.891294700665));
#60712=CARTESIAN_POINT('',(31.2665734631337,-2.42548317353486,33.8637293696319));
#60713=CARTESIAN_POINT('Ctrl Pts',(31.2665734631313,-2.42548317353296,33.8637293696347));
#60714=CARTESIAN_POINT('Ctrl Pts',(31.2523638534557,-2.41402785018508,33.8804609779983));
#60715=CARTESIAN_POINT('Ctrl Pts',(31.238326763356,-2.40271160648617,33.8969505670841));
#60716=CARTESIAN_POINT('',(31.4062815551261,-2.34724288268751,33.8637293696319));
#60717=CARTESIAN_POINT('Origin',(30.,-1.32966554433622E-14,33.8637293696319));
#60718=CARTESIAN_POINT('',(31.401624462548,-2.31126050085554,33.8969505670765));
#60719=CARTESIAN_POINT('Ctrl Pts',(31.4016244625469,-2.31126050084735,33.8969505670841));
#60720=CARTESIAN_POINT('Ctrl Pts',(31.4039387870044,-2.32914180874765,33.8804609779983));
#60721=CARTESIAN_POINT('Ctrl Pts',(31.4062815551258,-2.34724288268448,33.8637293696347));
#60722=CARTESIAN_POINT('',(31.4230239951618,-2.29814685040399,33.8969505670765));
#60723=CARTESIAN_POINT('Origin',(31.4152691174526,-2.30950931155476,33.8912947803757));
#60724=CARTESIAN_POINT('',(31.452970256343,-2.31863200978458,33.8637293696319));
#60725=CARTESIAN_POINT('Ctrl Pts',(31.4529702563405,-2.31863200978284,33.8637293696347));
#60726=CARTESIAN_POINT('Ctrl Pts',(31.4379056758382,-2.30832687249962,33.8804609779984));
#60727=CARTESIAN_POINT('Ctrl Pts',(31.423023995155,-2.29814685039932,33.8969505670841));
#60728=CARTESIAN_POINT('',(31.5861090124437,-2.22967153707895,33.8637293696319));
#60729=CARTESIAN_POINT('Origin',(30.,-1.32966554433622E-14,33.8637293696319));
#60730=CARTESIAN_POINT('',(31.5786431309871,-2.19416546819406,33.8969505670765));
#60731=CARTESIAN_POINT('Ctrl Pts',(31.5786431309854,-2.19416546818597,33.8969505670841));
#60732=CARTESIAN_POINT('Ctrl Pts',(31.5823532724012,-2.21181007417745,33.8804609779984));
#60733=CARTESIAN_POINT('Ctrl Pts',(31.5861090124431,-2.22967153707596,33.8637293696347));
#60734=CARTESIAN_POINT('',(31.5989478108274,-2.17941325477251,33.8969505670765));
#60735=CARTESIAN_POINT('Origin',(31.5921082951429,-2.19134908471607,33.891294843835));
#60736=CARTESIAN_POINT('',(31.6304090047603,-2.1974857086706,33.8637293696319));
#60737=CARTESIAN_POINT('Ctrl Pts',(31.6304090047577,-2.19748570866908,33.8637293696347));
#60738=CARTESIAN_POINT('Ctrl Pts',(31.6145823315769,-2.18839429204867,33.8804609779984));
#60739=CARTESIAN_POINT('Ctrl Pts',(31.5989478108202,-2.1794132547684,33.8969505670841));
#60740=CARTESIAN_POINT('',(31.7561575802648,-2.09835352500328,33.8637293696319));
#60741=CARTESIAN_POINT('Origin',(30.,-1.32966554433622E-14,33.8637293696319));
#60742=CARTESIAN_POINT('',(31.7459289395715,-2.0635426757871,33.8969505670765));
#60743=CARTESIAN_POINT('Ctrl Pts',(31.7459289395692,-2.06354267577917,33.8969505670841));
#60744=CARTESIAN_POINT('Ctrl Pts',(31.7510120236878,-2.08084179499847,33.8804609779983));
#60745=CARTESIAN_POINT('Ctrl Pts',(31.7561575802639,-2.09835352500035,33.8637293696347));
#60746=CARTESIAN_POINT('',(31.7650135815352,-2.04724285169692,33.8969505670765));
#60747=CARTESIAN_POINT('Origin',(31.7591315960217,-2.05967847590834,33.8912948941586));
#60748=CARTESIAN_POINT('',(31.7977957394973,-2.06279117742452,33.8637293696319));
#60749=CARTESIAN_POINT('Ctrl Pts',(31.7977957394945,-2.06279117742322,33.8637293696347));
#60750=CARTESIAN_POINT('Ctrl Pts',(31.7813045503384,-2.05496953307228,33.8804609779984));
#60751=CARTESIAN_POINT('Ctrl Pts',(31.7650135815277,-2.04724285169338,33.8969505670841));
#60752=CARTESIAN_POINT('',(31.9153788526219,-1.9540984656726,33.8637293696319));
#60753=CARTESIAN_POINT('Origin',(30.,-1.32966554433622E-14,33.8637293696319));
#60754=CARTESIAN_POINT('',(31.9024505156632,-1.92019745658634,33.8969505670765));
#60755=CARTESIAN_POINT('Ctrl Pts',(31.9024505156603,-1.92019745657863,33.8969505670841));
#60756=CARTESIAN_POINT('Ctrl Pts',(31.9088752035777,-1.93704443420321,33.8804609779984));
#60757=CARTESIAN_POINT('Ctrl Pts',(31.9153788526208,-1.95409846566976,33.8637293696347));
#60758=CARTESIAN_POINT('',(31.9201974565863,-1.90245051566327,33.8969505670765));
#60759=CARTESIAN_POINT('Origin',(31.9153092670123,-1.91530927561705,33.891294933562));
#60760=CARTESIAN_POINT('',(31.9540984656725,-1.91537885262194,33.8637293696319));
#60761=CARTESIAN_POINT('Ctrl Pts',(31.9540984656697,-1.91537885262084,33.8637293696347));
#60762=CARTESIAN_POINT('Ctrl Pts',(31.9370444342032,-1.90887520357777,33.8804609779984));
#60763=CARTESIAN_POINT('Ctrl Pts',(31.9201974565786,-1.90245051566033,33.8969505670841));
#60764=CARTESIAN_POINT('',(32.0627911774245,-1.79779573949737,33.8637293696319));
#60765=CARTESIAN_POINT('Origin',(30.,-1.32966554433622E-14,33.8637293696319));
#60766=CARTESIAN_POINT('',(32.0472428516969,-1.76501358153528,33.8969505670765));
#60767=CARTESIAN_POINT('Ctrl Pts',(32.0472428516934,-1.76501358152781,33.8969505670841));
#60768=CARTESIAN_POINT('Ctrl Pts',(32.0549695330723,-1.78130455033843,33.8804609779983));
#60769=CARTESIAN_POINT('Ctrl Pts',(32.0627911774232,-1.7977957394946,33.8637293696347));
#60770=CARTESIAN_POINT('',(32.063542675787,-1.74592893957158,33.8969505670765));
#60771=CARTESIAN_POINT('Origin',(32.0596784217459,-1.75913156587025,33.8912949636253));
#60772=CARTESIAN_POINT('',(32.0983535250032,-1.75615758026484,33.8637293696319));
#60773=CARTESIAN_POINT('Ctrl Pts',(32.0983535250003,-1.75615758026399,33.8637293696347));
#60774=CARTESIAN_POINT('Ctrl Pts',(32.0808417949984,-1.75101202368781,33.8804609779984));
#60775=CARTESIAN_POINT('Ctrl Pts',(32.0635426757791,-1.74592893956926,33.8969505670841));
#60776=CARTESIAN_POINT('',(32.1974857086705,-1.63040900476039,33.8637293696319));
#60777=CARTESIAN_POINT('Origin',(30.,-1.32966554433622E-14,33.8637293696319));
#60778=CARTESIAN_POINT('',(32.1794132547725,-1.59894781082747,33.8969505670765));
#60779=CARTESIAN_POINT('Ctrl Pts',(32.1794132547683,-1.59894781082035,33.8969505670841));
#60780=CARTESIAN_POINT('Ctrl Pts',(32.1883942920486,-1.61458233157699,33.8804609779984));
#60781=CARTESIAN_POINT('Ctrl Pts',(32.197485708669,-1.63040900475776,33.8637293696347));
#60782=CARTESIAN_POINT('',(32.194165468194,-1.57864313098713,33.8969505670765));
#60783=CARTESIAN_POINT('Origin',(32.1913489771416,-1.59210823242541,33.8912949854673));
#60784=CARTESIAN_POINT('',(32.2296715370789,-1.58610901244375,33.8637293696319));
#60785=CARTESIAN_POINT('Ctrl Pts',(32.2296715370759,-1.58610901244313,33.8637293696347));
#60786=CARTESIAN_POINT('Ctrl Pts',(32.2118100741774,-1.58235327240121,33.8804609779984));
#60787=CARTESIAN_POINT('Ctrl Pts',(32.1941654681859,-1.57864313098543,33.8969505670841));
#60788=CARTESIAN_POINT('',(32.3186320097845,-1.45297025634306,33.8637293696319));
#60789=CARTESIAN_POINT('Origin',(30.,-1.32966554433622E-14,33.8637293696319));
#60790=CARTESIAN_POINT('',(32.2981468504039,-1.42302399516182,33.8969505670765));
#60791=CARTESIAN_POINT('Ctrl Pts',(32.2981468503993,-1.42302399515499,33.8969505670841));
#60792=CARTESIAN_POINT('Ctrl Pts',(32.3083268724996,-1.4379056758382,33.8804609779984));
#60793=CARTESIAN_POINT('Ctrl Pts',(32.3186320097828,-1.45297025634053,33.8637293696347));
#60794=CARTESIAN_POINT('',(32.3112605008555,-1.40162446254804,33.8969505670765));
#60795=CARTESIAN_POINT('Origin',(32.3095091411127,-1.41526902814879,33.891294999854));
#60796=CARTESIAN_POINT('',(32.3472428826875,-1.40628155512619,33.8637293696319));
#60797=CARTESIAN_POINT('Ctrl Pts',(32.3472428826845,-1.4062815551258,33.8637293696347));
#60798=CARTESIAN_POINT('Ctrl Pts',(32.3291418087476,-1.4039387870044,33.8804609779983));
#60799=CARTESIAN_POINT('Ctrl Pts',(32.3112605008473,-1.40162446254698,33.8969505670841));
#60800=CARTESIAN_POINT('',(32.4254831735348,-1.26657346313373,33.8637293696319));
#60801=CARTESIAN_POINT('Origin',(30.,-1.32966554433622E-14,33.8637293696319));
#60802=CARTESIAN_POINT('',(32.4027116064913,-1.2383267633625,33.8969505670765));
#60803=CARTESIAN_POINT('Ctrl Pts',(32.4027116064861,-1.23832676335608,33.8969505670841));
#60804=CARTESIAN_POINT('Ctrl Pts',(32.414027850185,-1.25236385345577,33.8804609779983));
#60805=CARTESIAN_POINT('Ctrl Pts',(32.4254831735329,-1.26657346313137,33.8637293696347));
#60806=CARTESIAN_POINT('',(32.4141058439571,-1.21596431320991,33.8969505670765));
#60807=CARTESIAN_POINT('Origin',(32.4134304175703,-1.22970422416536,33.8912950072666));
#60808=CARTESIAN_POINT('',(32.4503426953868,-1.21778390438519,33.8637293696319));
#60809=CARTESIAN_POINT('Ctrl Pts',(32.4503426953838,-1.21778390438504,33.8637293696347));
#60810=CARTESIAN_POINT('Ctrl Pts',(32.4321136095486,-1.21686855212869,33.8804609779984));
#60811=CARTESIAN_POINT('Ctrl Pts',(32.4141058439489,-1.2159643132095,33.8969505670841));
#60812=CARTESIAN_POINT('',(32.5173804269652,-1.07236782334576,33.8637293696319));
#60813=CARTESIAN_POINT('Origin',(30.,-1.32966554433622E-14,33.8637293696319));
#60814=CARTESIAN_POINT('',(32.492462846542,-1.0459948352816,33.8969505670765));
#60815=CARTESIAN_POINT('Ctrl Pts',(32.4924628465363,-1.04599483527564,33.8969505670841));
#60816=CARTESIAN_POINT('Ctrl Pts',(32.5048455434283,-1.05910079146353,33.8804609779984));
#60817=CARTESIAN_POINT('Ctrl Pts',(32.5173804269631,-1.07236782334356,33.8637293696347));
#60818=CARTESIAN_POINT('',(32.5020674217591,-1.02280733953168,33.8969505670765));
#60819=CARTESIAN_POINT('Origin',(32.5024720978725,-1.03655788791108,33.8912950079413));
#60820=CARTESIAN_POINT('',(32.5383353305474,-1.02177821091943,33.8637293696319));
#60821=CARTESIAN_POINT('Ctrl Pts',(32.5383353305444,-1.02177821091952,33.8637293696347));
#60822=CARTESIAN_POINT('Ctrl Pts',(32.5200906211869,-1.02229591797926,33.8804609779983));
#60823=CARTESIAN_POINT('Ctrl Pts',(32.5020674217508,-1.02280733953191,33.8969505670841));
#60824=CARTESIAN_POINT('',(32.5937571929495,-0.871550679328387,33.8637293696319));
#60825=CARTESIAN_POINT('Origin',(30.,-1.32966554433622E-14,33.8637293696319));
#60826=CARTESIAN_POINT('',(32.5668472243157,-0.847214001212625,33.8969505670765));
#60827=CARTESIAN_POINT('Ctrl Pts',(32.5668472243096,-0.847214001207098,
33.8969505670841));
#60828=CARTESIAN_POINT('Ctrl Pts',(32.5802200309508,-0.859308020905142,
33.8804609779983));
#60829=CARTESIAN_POINT('Ctrl Pts',(32.5937571929472,-0.871550679326345,
33.8637293696347));
#60830=CARTESIAN_POINT('',(32.574602921884,-0.823344418487278,33.8969505670765));
#60831=CARTESIAN_POINT('Origin',(32.5760852110325,-0.837020829522246,33.8912950018862));
#60832=CARTESIAN_POINT('',(32.6106782843131,-0.819472915007605,33.8637293696319));
#60833=CARTESIAN_POINT('Ctrl Pts',(32.6106782843101,-0.819472915007929,
33.8637293696347));
#60834=CARTESIAN_POINT('Ctrl Pts',(32.5925304361305,-0.821420489547588,
33.8804609779984));
#60835=CARTESIAN_POINT('Ctrl Pts',(32.5746029218758,-0.823344418488157,
33.8969505670841));
#60836=CARTESIAN_POINT('',(32.6541425833274,-0.665360135552938,33.8637293696319));
#60837=CARTESIAN_POINT('Origin',(30.,-1.32966554433622E-14,33.8637293696319));
#60838=CARTESIAN_POINT('',(32.6254061353882,-0.643209811098926,33.8969505670765));
#60839=CARTESIAN_POINT('Ctrl Pts',(32.6254061353816,-0.643209811093906,
33.8969505670841));
#60840=CARTESIAN_POINT('Ctrl Pts',(32.6396866039721,-0.65421733064898,33.8804609779984));
#60841=CARTESIAN_POINT('Ctrl Pts',(32.654142583325,-0.665360135551083,33.8637293696347));
#60842=CARTESIAN_POINT('',(32.6312651388532,-0.6188053053131,33.8969505670765));
#60843=CARTESIAN_POINT('Origin',(32.633815908334,-0.632323260043048,33.8912949888765));
#60844=CARTESIAN_POINT('',(32.6669255383174,-0.612115296072366,33.8637293696319));
#60845=CARTESIAN_POINT('Ctrl Pts',(32.6669255383144,-0.612115296072921,
33.8637293696347));
#60846=CARTESIAN_POINT('Ctrl Pts',(32.6489864388314,-0.615480730647825,
33.8804609779983));
#60847=CARTESIAN_POINT('Ctrl Pts',(32.6312651388451,-0.618805305314621,
33.8969505670841));
#60848=CARTESIAN_POINT('',(32.6981643020872,-0.455067425287109,33.8637293696319));
#60849=CARTESIAN_POINT('Origin',(30.,-1.32966554433622E-14,33.8637293696319));
#60850=CARTESIAN_POINT('',(32.6677785445999,-0.435240018610835,33.8969505670765));
#60851=CARTESIAN_POINT('Ctrl Pts',(32.667778544593,-0.43524001860635,33.8969505670841));
#60852=CARTESIAN_POINT('Ctrl Pts',(32.6828786312952,-0.445093173000037,
33.8804609779984));
#60853=CARTESIAN_POINT('Ctrl Pts',(32.6981643020846,-0.45506742528547,33.8637293696347));
#60854=CARTESIAN_POINT('',(32.6717047312569,-0.410451051658023,33.8969505670765));
#60855=CARTESIAN_POINT('Origin',(32.6753082614924,-0.423727206709312,33.8912949684251));
#60856=CARTESIAN_POINT('',(32.7067303095351,-0.400983782787849,33.8637293696319));
#60857=CARTESIAN_POINT('Ctrl Pts',(32.7067303095322,-0.400983782788643,
33.8637293696347));
#60858=CARTESIAN_POINT('Ctrl Pts',(32.6891105592595,-0.405746328375509,
33.8804609779984));
#60859=CARTESIAN_POINT('Ctrl Pts',(32.6717047312489,-0.410451051660171,
33.8969505670841));
#60860=CARTESIAN_POINT('',(32.7255509406939,-0.241969073019109,33.8637293696319));
#60861=CARTESIAN_POINT('Origin',(30.,-1.32966554433622E-14,33.8637293696319));
#60862=CARTESIAN_POINT('',(32.6937032119577,-0.224586826676015,33.8969505670765));
#60863=CARTESIAN_POINT('Ctrl Pts',(32.6937032119505,-0.224586826672072,
33.8969505670841));
#60864=CARTESIAN_POINT('Ctrl Pts',(32.7095298197086,-0.233224867931026,
33.8804609779984));
#60865=CARTESIAN_POINT('Ctrl Pts',(32.7255509406912,-0.241969073017673,
33.8637293696347));
#60866=CARTESIAN_POINT('',(32.6956723755605,-0.199566230780649,33.8969505670765));
#60867=CARTESIAN_POINT('Origin',(32.7003064571198,-0.212518732061269,33.8912949397143));
#60868=CARTESIAN_POINT('',(32.7298471883155,-0.187380071141808,33.8637293696319));
#60869=CARTESIAN_POINT('Ctrl Pts',(32.7298471883126,-0.187380071142835,
33.8637293696347));
#60870=CARTESIAN_POINT('Ctrl Pts',(32.7126554188699,-0.19351036506442,33.8804609779983));
#60871=CARTESIAN_POINT('Ctrl Pts',(32.6956723755527,-0.199566230783424,
33.8969505670841));
#60872=CARTESIAN_POINT('',(32.7361336514135,-0.0273789009530657,33.8637293696319));
#60873=CARTESIAN_POINT('Origin',(30.,-1.32966554433622E-14,33.8637293696319));
#60874=CARTESIAN_POINT('',(32.7030203032667,-0.0125489822720396,33.8969505670765));
#60875=CARTESIAN_POINT('Ctrl Pts',(32.7030203032592,-0.0125489822686859,
33.8969505670841));
#60876=CARTESIAN_POINT('Ctrl Pts',(32.7194758557734,-0.0199186539960853,
33.8804609779984));
#60877=CARTESIAN_POINT('Ctrl Pts',(32.7361336514107,-0.0273789009518218,
33.8637293696347));
#60878=CARTESIAN_POINT('',(32.7030203032667,0.0125489822719939,33.8969505670765));
#60879=CARTESIAN_POINT('Origin',(32.7086563646857,-6.24428584025816E-9,
33.8912949140187));
#60880=CARTESIAN_POINT('',(32.7361336514135,0.0273789009530202,33.8637293696319));
#60881=CARTESIAN_POINT('Ctrl Pts',(32.7361336514108,0.027378900951751,33.8637293696347));
#60882=CARTESIAN_POINT('Ctrl Pts',(32.7194758557734,0.0199186539960142,
33.8804609779984));
#60883=CARTESIAN_POINT('Ctrl Pts',(32.7030203032592,0.0125489822686146,
33.8969505670841));
#60884=CARTESIAN_POINT('',(32.7298471883155,0.187380071141762,33.8637293696319));
#60885=CARTESIAN_POINT('Origin',(30.,-1.32966554433622E-14,33.8637293696319));
#60886=CARTESIAN_POINT('',(32.6956723755605,0.199566230780603,33.8969505670765));
#60887=CARTESIAN_POINT('Ctrl Pts',(32.6956723755527,0.199566230783364,33.8969505670841));
#60888=CARTESIAN_POINT('Ctrl Pts',(32.7126554188699,0.193510365064359,33.8804609779983));
#60889=CARTESIAN_POINT('Ctrl Pts',(32.7298471883126,0.187380071142775,33.8637293696347));
#60890=CARTESIAN_POINT('',(32.6937032119577,0.224586826675969,33.8969505670765));
#60891=CARTESIAN_POINT('Origin',(32.7003074588901,0.212518788369426,33.8912937927563));
#60892=CARTESIAN_POINT('',(32.7255509406939,0.241969073019064,33.8637293696319));
#60893=CARTESIAN_POINT('Ctrl Pts',(32.7255509406912,0.241969073017624,33.8637293696347));
#60894=CARTESIAN_POINT('Ctrl Pts',(32.7095298197086,0.233224867930978,33.8804609779984));
#60895=CARTESIAN_POINT('Ctrl Pts',(32.6937032119505,0.224586826672025,33.8969505670841));
#60896=CARTESIAN_POINT('',(32.7067303095351,0.400983782787804,33.8637293696319));
#60897=CARTESIAN_POINT('Origin',(30.,-1.32966554433622E-14,33.8637293696319));
#60898=CARTESIAN_POINT('',(32.6717047312569,0.410451051657977,33.8969505670765));
#60899=CARTESIAN_POINT('Ctrl Pts',(32.6717047312489,0.410451051660138,33.8969505670841));
#60900=CARTESIAN_POINT('Ctrl Pts',(32.6891105592595,0.405746328375475,33.8804609779984));
#60901=CARTESIAN_POINT('Ctrl Pts',(32.7067303095322,0.400983782788608,33.8637293696347));
#60902=CARTESIAN_POINT('',(32.6677785445999,0.435240018610789,33.8969505670765));
#60903=CARTESIAN_POINT('Origin',(32.6753090233822,0.423727307748461,33.8912940899386));
#60904=CARTESIAN_POINT('',(32.6981643020872,0.455067425287063,33.8637293696319));
#60905=CARTESIAN_POINT('Ctrl Pts',(32.6981643020846,0.455067425285395,33.8637293696347));
#60906=CARTESIAN_POINT('Ctrl Pts',(32.6828786312952,0.445093172999962,33.8804609779983));
#60907=CARTESIAN_POINT('Ctrl Pts',(32.667778544593,0.435240018606276,33.8969505670841));
#60908=CARTESIAN_POINT('',(32.6669255383174,0.61211529607232,33.8637293696319));
#60909=CARTESIAN_POINT('Origin',(30.,-1.32966554433622E-14,33.8637293696319));
#60910=CARTESIAN_POINT('',(32.6312651388532,0.618805305313054,33.8969505670765));
#60911=CARTESIAN_POINT('Ctrl Pts',(32.6312651388451,0.618805305314574,33.8969505670841));
#60912=CARTESIAN_POINT('Ctrl Pts',(32.6489864388314,0.615480730647778,33.8804609779983));
#60913=CARTESIAN_POINT('Ctrl Pts',(32.6669255383144,0.612115296072874,33.8637293696347));
#60914=CARTESIAN_POINT('',(32.6254061353882,0.64320981109888,33.8969505670765));
#60915=CARTESIAN_POINT('Origin',(32.6338164916465,0.632323382398585,33.8912943077151));
#60916=CARTESIAN_POINT('',(32.6541425833274,0.665360135552893,33.8637293696319));
#60917=CARTESIAN_POINT('Ctrl Pts',(32.654142583325,0.665360135551018,33.8637293696347));
#60918=CARTESIAN_POINT('Ctrl Pts',(32.6396866039721,0.654217330648915,33.8804609779984));
#60919=CARTESIAN_POINT('Ctrl Pts',(32.6254061353817,0.643209811093841,33.8969505670841));
#60920=CARTESIAN_POINT('',(32.6106782843131,0.81947291500756,33.8637293696319));
#60921=CARTESIAN_POINT('Origin',(30.,-1.32966554433622E-14,33.8637293696319));
#60922=CARTESIAN_POINT('',(32.574602921884,0.823344418487232,33.8969505670765));
#60923=CARTESIAN_POINT('Ctrl Pts',(32.5746029218758,0.823344418488117,33.8969505670841));
#60924=CARTESIAN_POINT('Ctrl Pts',(32.5925304361305,0.821420489547548,33.8804609779984));
#60925=CARTESIAN_POINT('Ctrl Pts',(32.6106782843101,0.819472915007888,33.8637293696347));
#60926=CARTESIAN_POINT('',(32.5668472243157,0.84721400121258,33.8969505670765));
#60927=CARTESIAN_POINT('Origin',(32.5760856561636,0.83702095775897,33.891294472568));
#60928=CARTESIAN_POINT('',(32.5937571929495,0.871550679328342,33.8637293696319));
#60929=CARTESIAN_POINT('Ctrl Pts',(32.5937571929473,0.871550679326287,33.8637293696347));
#60930=CARTESIAN_POINT('Ctrl Pts',(32.5802200309508,0.859308020905083,33.8804609779984));
#60931=CARTESIAN_POINT('Ctrl Pts',(32.5668472243096,0.847214001207037,33.8969505670841));
#60932=CARTESIAN_POINT('',(32.5383353305474,1.02177821091938,33.8637293696319));
#60933=CARTESIAN_POINT('Origin',(30.,-1.32966554433622E-14,33.8637293696319));
#60934=CARTESIAN_POINT('',(32.5020674217591,1.02280733953163,33.8969505670765));
#60935=CARTESIAN_POINT('Ctrl Pts',(32.5020674217508,1.02280733953187,33.8969505670841));
#60936=CARTESIAN_POINT('Ctrl Pts',(32.520090621187,1.02229591797922,33.8804609779984));
#60937=CARTESIAN_POINT('Ctrl Pts',(32.5383353305444,1.02177821091947,33.8637293696347));
#60938=CARTESIAN_POINT('',(32.492462846542,1.04599483528156,33.8969505670765));
#60939=CARTESIAN_POINT('Origin',(32.5024724328509,1.03655801106889,33.8912946002427));
#60940=CARTESIAN_POINT('',(32.5173804269653,1.07236782334572,33.8637293696319));
#60941=CARTESIAN_POINT('Ctrl Pts',(32.5173804269632,1.0723678233435,33.8637293696347));
#60942=CARTESIAN_POINT('Ctrl Pts',(32.5048455434284,1.05910079146346,33.8804609779983));
#60943=CARTESIAN_POINT('Ctrl Pts',(32.4924628465363,1.04599483527555,33.8969505670841));
#60944=CARTESIAN_POINT('',(32.4503426953868,1.21778390438515,33.8637293696319));
#60945=CARTESIAN_POINT('Origin',(30.,-1.32966554433622E-14,33.8637293696319));
#60946=CARTESIAN_POINT('',(32.4141058439571,1.21596431320987,33.8969505670765));
#60947=CARTESIAN_POINT('Ctrl Pts',(32.4141058439489,1.21596431320946,33.8969505670841));
#60948=CARTESIAN_POINT('Ctrl Pts',(32.4321136095487,1.21686855212866,33.8804609779984));
#60949=CARTESIAN_POINT('Ctrl Pts',(32.4503426953838,1.217783904385,33.8637293696347));
#60950=CARTESIAN_POINT('',(32.4027116064913,1.23832676336245,33.8969505670765));
#60951=CARTESIAN_POINT('Origin',(32.4134306626749,1.22970433386022,33.891294700665));
#60952=CARTESIAN_POINT('',(32.4254831735348,1.26657346313369,33.8637293696319));
#60953=CARTESIAN_POINT('Ctrl Pts',(32.4254831735329,1.26657346313132,33.8637293696347));
#60954=CARTESIAN_POINT('Ctrl Pts',(32.414027850185,1.25236385345572,33.8804609779984));
#60955=CARTESIAN_POINT('Ctrl Pts',(32.4027116064861,1.23832676335603,33.8969505670841));
#60956=CARTESIAN_POINT('',(32.3472428826875,1.40628155512614,33.8637293696319));
#60957=CARTESIAN_POINT('Origin',(30.,-1.32966554433622E-14,33.8637293696319));
#60958=CARTESIAN_POINT('',(32.3112605008555,1.401624462548,33.8969505670765));
#60959=CARTESIAN_POINT('Ctrl Pts',(32.3112605008473,1.40162446254694,33.8969505670841));
#60960=CARTESIAN_POINT('Ctrl Pts',(32.3291418087476,1.40393878700437,33.8804609779984));
#60961=CARTESIAN_POINT('Ctrl Pts',(32.3472428826845,1.40628155512576,33.8637293696347));
#60962=CARTESIAN_POINT('',(32.298146850404,1.42302399516178,33.8969505670765));
#60963=CARTESIAN_POINT('Origin',(32.3095093115547,1.41526911745259,33.8912947803757));
#60964=CARTESIAN_POINT('',(32.3186320097845,1.45297025634302,33.8637293696319));
#60965=CARTESIAN_POINT('Ctrl Pts',(32.3186320097828,1.45297025634046,33.8637293696347));
#60966=CARTESIAN_POINT('Ctrl Pts',(32.3083268724996,1.43790567583815,33.8804609779983));
#60967=CARTESIAN_POINT('Ctrl Pts',(32.2981468503993,1.42302399515495,33.8969505670841));
#60968=CARTESIAN_POINT('',(32.2296715370789,1.58610901244371,33.8637293696319));
#60969=CARTESIAN_POINT('Origin',(30.,-1.32966554433622E-14,33.8637293696319));
#60970=CARTESIAN_POINT('',(32.194165468194,1.57864313098709,33.8969505670765));
#60971=CARTESIAN_POINT('Ctrl Pts',(32.1941654681859,1.57864313098539,33.8969505670841));
#60972=CARTESIAN_POINT('Ctrl Pts',(32.2118100741774,1.58235327240116,33.8804609779984));
#60973=CARTESIAN_POINT('Ctrl Pts',(32.2296715370759,1.58610901244308,33.8637293696347));
#60974=CARTESIAN_POINT('',(32.1794132547725,1.59894781082743,33.8969505670765));
#60975=CARTESIAN_POINT('Origin',(32.191349084716,1.59210829514292,33.891294843835));
#60976=CARTESIAN_POINT('',(32.1974857086706,1.63040900476035,33.8637293696319));
#60977=CARTESIAN_POINT('Ctrl Pts',(32.1974857086691,1.6304090047577,33.8637293696347));
#60978=CARTESIAN_POINT('Ctrl Pts',(32.1883942920486,1.61458233157692,33.8804609779983));
#60979=CARTESIAN_POINT('Ctrl Pts',(32.1794132547684,1.59894781082026,33.8969505670841));
#60980=CARTESIAN_POINT('',(32.0983535250032,1.7561575802648,33.8637293696319));
#60981=CARTESIAN_POINT('Origin',(30.,-1.32966554433622E-14,33.8637293696319));
#60982=CARTESIAN_POINT('',(32.0635426757871,1.74592893957153,33.8969505670765));
#60983=CARTESIAN_POINT('Ctrl Pts',(32.0635426757792,1.74592893956921,33.8969505670841));
#60984=CARTESIAN_POINT('Ctrl Pts',(32.0808417949984,1.75101202368776,33.8804609779983));
#60985=CARTESIAN_POINT('Ctrl Pts',(32.0983535250003,1.75615758026393,33.8637293696347));
#60986=CARTESIAN_POINT('',(32.0472428516969,1.76501358153524,33.8969505670765));
#60987=CARTESIAN_POINT('Origin',(32.0596784759083,1.75913159602166,33.8912948941586));
#60988=CARTESIAN_POINT('',(32.0627911774245,1.79779573949733,33.8637293696319));
#60989=CARTESIAN_POINT('Ctrl Pts',(32.0627911774232,1.79779573949457,33.8637293696347));
#60990=CARTESIAN_POINT('Ctrl Pts',(32.0549695330723,1.78130455033839,33.8804609779984));
#60991=CARTESIAN_POINT('Ctrl Pts',(32.0472428516934,1.76501358152777,33.8969505670841));
#60992=CARTESIAN_POINT('',(31.9540984656726,1.9153788526219,33.8637293696319));
#60993=CARTESIAN_POINT('Origin',(30.,-1.32966554433622E-14,33.8637293696319));
#60994=CARTESIAN_POINT('',(31.9201974565863,1.90245051566323,33.8969505670765));
#60995=CARTESIAN_POINT('Ctrl Pts',(31.9201974565786,1.90245051566028,33.8969505670841));
#60996=CARTESIAN_POINT('Ctrl Pts',(31.9370444342032,1.90887520357773,33.8804609779983));
#60997=CARTESIAN_POINT('Ctrl Pts',(31.9540984656697,1.91537885262081,33.8637293696347));
#60998=CARTESIAN_POINT('',(31.9024505156632,1.9201974565863,33.8969505670765));
#60999=CARTESIAN_POINT('Origin',(31.915309275617,1.91530926701235,33.891294933562));
#61000=CARTESIAN_POINT('',(31.9153788526219,1.95409846567256,33.8637293696319));
#61001=CARTESIAN_POINT('Ctrl Pts',(31.9153788526208,1.95409846566973,33.8637293696347));
#61002=CARTESIAN_POINT('Ctrl Pts',(31.9088752035777,1.93704443420319,33.8804609779984));
#61003=CARTESIAN_POINT('Ctrl Pts',(31.9024505156603,1.9201974565786,33.8969505670841));
#61004=CARTESIAN_POINT('',(31.7977957394973,2.06279117742448,33.8637293696319));
#61005=CARTESIAN_POINT('Origin',(30.,-1.32966554433622E-14,33.8637293696319));
#61006=CARTESIAN_POINT('',(31.7650135815352,2.04724285169688,33.8969505670765));
#61007=CARTESIAN_POINT('Ctrl Pts',(31.7650135815278,2.04724285169333,33.8969505670841));
#61008=CARTESIAN_POINT('Ctrl Pts',(31.7813045503384,2.05496953307223,33.8804609779984));
#61009=CARTESIAN_POINT('Ctrl Pts',(31.7977957394946,2.06279117742316,33.8637293696347));
#61010=CARTESIAN_POINT('',(31.7459289395715,2.06354267578706,33.8969505670765));
#61011=CARTESIAN_POINT('Origin',(31.7591315658702,2.05967842174595,33.8912949636253));
#61012=CARTESIAN_POINT('',(31.7561575802648,2.09835352500324,33.8637293696319));
#61013=CARTESIAN_POINT('Ctrl Pts',(31.7561575802639,2.09835352500033,33.8637293696347));
#61014=CARTESIAN_POINT('Ctrl Pts',(31.7510120236877,2.08084179499845,33.8804609779984));
#61015=CARTESIAN_POINT('Ctrl Pts',(31.7459289395692,2.06354267577915,33.8969505670841));
#61016=CARTESIAN_POINT('',(31.6304090047604,2.19748570867057,33.8637293696319));
#61017=CARTESIAN_POINT('Origin',(30.,-1.32966554433622E-14,33.8637293696319));
#61018=CARTESIAN_POINT('',(31.5989478108274,2.17941325477248,33.8969505670765));
#61019=CARTESIAN_POINT('Ctrl Pts',(31.5989478108202,2.17941325476838,33.8969505670841));
#61020=CARTESIAN_POINT('Ctrl Pts',(31.6145823315769,2.18839429204865,33.8804609779983));
#61021=CARTESIAN_POINT('Ctrl Pts',(31.6304090047577,2.19748570866908,33.8637293696347));
#61022=CARTESIAN_POINT('',(31.5786431309871,2.19416546819402,33.8969505670765));
#61023=CARTESIAN_POINT('Origin',(31.5921082324254,2.19134897714166,33.8912949854673));
#61024=CARTESIAN_POINT('',(31.5861090124437,2.22967153707891,33.8637293696319));
#61025=CARTESIAN_POINT('Ctrl Pts',(31.5861090124431,2.22967153707593,33.8637293696347));
#61026=CARTESIAN_POINT('Ctrl Pts',(31.5823532724012,2.21181007417742,33.8804609779984));
#61027=CARTESIAN_POINT('Ctrl Pts',(31.5786431309854,2.19416546818594,33.8969505670841));
#61028=CARTESIAN_POINT('',(31.452970256343,2.31863200978455,33.8637293696319));
#61029=CARTESIAN_POINT('Origin',(30.,-1.32966554433622E-14,33.8637293696319));
#61030=CARTESIAN_POINT('',(31.4230239951618,2.29814685040396,33.8969505670765));
#61031=CARTESIAN_POINT('Ctrl Pts',(31.423023995155,2.29814685039929,33.8969505670841));
#61032=CARTESIAN_POINT('Ctrl Pts',(31.4379056758382,2.30832687249959,33.8804609779983));
#61033=CARTESIAN_POINT('Ctrl Pts',(31.4529702563405,2.31863200978281,33.8637293696347));
#61034=CARTESIAN_POINT('',(31.401624462548,2.3112605008555,33.8969505670765));
#61035=CARTESIAN_POINT('Origin',(31.4152690281487,2.30950914111275,33.891294999854));
#61036=CARTESIAN_POINT('',(31.4062815551261,2.34724288268748,33.8637293696319));
#61037=CARTESIAN_POINT('Ctrl Pts',(31.4062815551258,2.34724288268445,33.8637293696347));
#61038=CARTESIAN_POINT('Ctrl Pts',(31.4039387870044,2.32914180874762,33.8804609779983));
#61039=CARTESIAN_POINT('Ctrl Pts',(31.4016244625469,2.31126050084732,33.8969505670841));
#61040=CARTESIAN_POINT('',(31.2665734631337,2.42548317353483,33.8637293696319));
#61041=CARTESIAN_POINT('Origin',(30.,-1.32966554433622E-14,33.8637293696319));
#61042=CARTESIAN_POINT('',(31.2383267633625,2.40271160649132,33.8969505670765));
#61043=CARTESIAN_POINT('Ctrl Pts',(31.2383267633561,2.40271160648613,33.8969505670841));
#61044=CARTESIAN_POINT('Ctrl Pts',(31.2523638534557,2.41402785018503,33.8804609779983));
#61045=CARTESIAN_POINT('Ctrl Pts',(31.2665734631313,2.4254831735329,33.8637293696347));
#61046=CARTESIAN_POINT('',(31.2159643132099,2.41410584395711,33.8969505670765));
#61047=CARTESIAN_POINT('Origin',(31.2297042241653,2.41343041757031,33.8912950072666));
#61048=CARTESIAN_POINT('',(31.2177839043851,2.45034269538681,33.8637293696319));
#61049=CARTESIAN_POINT('Ctrl Pts',(31.217783904385,2.45034269538375,33.8637293696347));
#61050=CARTESIAN_POINT('Ctrl Pts',(31.2168685521287,2.43211360954864,33.8804609779984));
#61051=CARTESIAN_POINT('Ctrl Pts',(31.2159643132095,2.41410584394886,33.8969505670841));
#61052=CARTESIAN_POINT('',(31.0723678233457,2.51738042696526,33.8637293696319));
#61053=CARTESIAN_POINT('Origin',(30.,-1.32966554433622E-14,33.8637293696319));
#61054=CARTESIAN_POINT('',(31.0459948352816,2.49246284654197,33.8969505670765));
#61055=CARTESIAN_POINT('Ctrl Pts',(31.0459948352756,2.4924628465363,33.8969505670841));
#61056=CARTESIAN_POINT('Ctrl Pts',(31.0591007914635,2.50484554342835,33.8804609779983));
#61057=CARTESIAN_POINT('Ctrl Pts',(31.0723678233435,2.51738042696315,33.8637293696347));
#61058=CARTESIAN_POINT('',(31.0228073395316,2.50206742175906,33.8969505670765));
#61059=CARTESIAN_POINT('Origin',(31.036557887911,2.50247209787251,33.8912950079413));
#61060=CARTESIAN_POINT('',(31.0217782109194,2.53833533054745,33.8637293696319));
#61061=CARTESIAN_POINT('Ctrl Pts',(31.0217782109194,2.5383353305444,33.8637293696347));
#61062=CARTESIAN_POINT('Ctrl Pts',(31.0222959179792,2.52009062118696,33.8804609779984));
#61063=CARTESIAN_POINT('Ctrl Pts',(31.0228073395318,2.50206742175081,33.8969505670841));
#61064=CARTESIAN_POINT('',(30.8715506793283,2.59375719294951,33.8637293696319));
#61065=CARTESIAN_POINT('Origin',(30.,-1.32966554433622E-14,33.8637293696319));
#61066=CARTESIAN_POINT('',(30.8472140012126,2.5668472243157,33.8969505670765));
#61067=CARTESIAN_POINT('Ctrl Pts',(30.847214001207,2.56684722430959,33.8969505670841));
#61068=CARTESIAN_POINT('Ctrl Pts',(30.8593080209051,2.58022003095078,33.8804609779984));
#61069=CARTESIAN_POINT('Ctrl Pts',(30.8715506793263,2.59375719294725,33.8637293696347));
#61070=CARTESIAN_POINT('',(30.8233444184872,2.57460292188402,33.8969505670765));
#61071=CARTESIAN_POINT('Origin',(30.8370208295222,2.57608521103255,33.8912950018862));
#61072=CARTESIAN_POINT('',(30.8194729150076,2.61067828431311,33.8637293696319));
#61073=CARTESIAN_POINT('Ctrl Pts',(30.8194729150079,2.61067828431008,33.8637293696347));
#61074=CARTESIAN_POINT('Ctrl Pts',(30.8214204895475,2.59253043613048,33.8804609779984));
#61075=CARTESIAN_POINT('Ctrl Pts',(30.8233444184881,2.57460292187581,33.8969505670841));
#61076=CARTESIAN_POINT('',(30.6653601355529,2.65414258332745,33.8637293696319));
#61077=CARTESIAN_POINT('Origin',(30.,-1.32966554433622E-14,33.8637293696319));
#61078=CARTESIAN_POINT('',(30.6432098110989,2.62540613538819,33.8969505670765));
#61079=CARTESIAN_POINT('Ctrl Pts',(30.6432098110938,2.62540613538167,33.8969505670841));
#61080=CARTESIAN_POINT('Ctrl Pts',(30.6542173306489,2.63968660397217,33.8804609779983));
#61081=CARTESIAN_POINT('Ctrl Pts',(30.665360135551,2.65414258332504,33.8637293696347));
#61082=CARTESIAN_POINT('',(30.6188053053131,2.63126513885322,33.8969505670765));
#61083=CARTESIAN_POINT('Origin',(30.632323260043,2.633815908334,33.8912949888765));
#61084=CARTESIAN_POINT('',(30.6121152960723,2.66692553831736,33.8637293696319));
#61085=CARTESIAN_POINT('Ctrl Pts',(30.6121152960729,2.66692553831437,33.8637293696347));
#61086=CARTESIAN_POINT('Ctrl Pts',(30.6154807306478,2.6489864388314,33.8804609779983));
#61087=CARTESIAN_POINT('Ctrl Pts',(30.6188053053146,2.63126513884509,33.8969505670841));
#61088=CARTESIAN_POINT('',(30.4550674252871,2.69816430208719,33.8637293696319));
#61089=CARTESIAN_POINT('Origin',(30.,-1.32966554433622E-14,33.8637293696319));
#61090=CARTESIAN_POINT('',(30.4352400186108,2.66777854459989,33.8969505670765));
#61091=CARTESIAN_POINT('Ctrl Pts',(30.4352400186063,2.66777854459299,33.8969505670841));
#61092=CARTESIAN_POINT('Ctrl Pts',(30.4450931729999,2.68287863129519,33.8804609779983));
#61093=CARTESIAN_POINT('Ctrl Pts',(30.4550674252854,2.69816430208465,33.8637293696347));
#61094=CARTESIAN_POINT('',(30.410451051658,2.67170473125694,33.8969505670765));
#61095=CARTESIAN_POINT('Origin',(30.4237272067093,2.67530826149246,33.891294968425));
#61096=CARTESIAN_POINT('',(30.4009837827878,2.70673030953515,33.8637293696319));
#61097=CARTESIAN_POINT('Ctrl Pts',(30.4009837827886,2.7067303095322,33.8637293696347));
#61098=CARTESIAN_POINT('Ctrl Pts',(30.4057463283755,2.68911055925956,33.8804609779984));
#61099=CARTESIAN_POINT('Ctrl Pts',(30.4104510516602,2.67170473124897,33.8969505670841));
#61100=CARTESIAN_POINT('',(30.2419690730191,2.72555094069389,33.8637293696319));
#61101=CARTESIAN_POINT('Origin',(30.,-1.32966554433622E-14,33.8637293696319));
#61102=CARTESIAN_POINT('',(30.224586826676,2.69370321195774,33.8969505670765));
#61103=CARTESIAN_POINT('Ctrl Pts',(30.224586826672,2.6937032119505,33.8969505670841));
#61104=CARTESIAN_POINT('Ctrl Pts',(30.233224867931,2.70952981970859,33.8804609779983));
#61105=CARTESIAN_POINT('Ctrl Pts',(30.2419690730176,2.72555094069122,33.8637293696347));
#61106=CARTESIAN_POINT('',(30.1995662307806,2.69567237556048,33.8969505670765));
#61107=CARTESIAN_POINT('Origin',(30.2125187320612,2.70030645711979,33.8912949397143));
#61108=CARTESIAN_POINT('',(30.1873800711418,2.72984718831549,33.8637293696319));
#61109=CARTESIAN_POINT('Ctrl Pts',(30.1873800711428,2.7298471883126,33.8637293696347));
#61110=CARTESIAN_POINT('Ctrl Pts',(30.1935103650644,2.71265541886987,33.8804609779983));
#61111=CARTESIAN_POINT('Ctrl Pts',(30.1995662307834,2.6956723755527,33.8969505670841));
#61112=CARTESIAN_POINT('',(30.027378900953,2.73613365141356,33.8637293696319));
#61113=CARTESIAN_POINT('Origin',(30.,-1.32966554433622E-14,33.8637293696319));
#61114=CARTESIAN_POINT('',(30.012548982272,2.70302030326666,33.8969505670765));
#61115=CARTESIAN_POINT('Ctrl Pts',(30.0125489822686,2.70302030325912,33.8969505670841));
#61116=CARTESIAN_POINT('Ctrl Pts',(30.019918653996,2.71947585577339,33.8804609779983));
#61117=CARTESIAN_POINT('Ctrl Pts',(30.0273789009518,2.73613365141076,33.8637293696347));
#61118=CARTESIAN_POINT('',(29.987451017728,2.70302030326666,33.8969505670765));
#61119=CARTESIAN_POINT('Origin',(30.,2.70866577951602,33.891284862925));
#61120=CARTESIAN_POINT('',(29.9726210990469,2.73613365141356,33.8637293696319));
#61121=CARTESIAN_POINT('Ctrl Pts',(29.9726210990482,2.73613365141079,33.8637293696347));
#61122=CARTESIAN_POINT('Ctrl Pts',(29.980081346004,2.7194758557734,33.8804609779983));
#61123=CARTESIAN_POINT('Ctrl Pts',(29.9874510177314,2.70302030325912,33.8969505670841));
#61124=CARTESIAN_POINT('',(29.8126199288582,2.72984718831549,33.8637293696319));
#61125=CARTESIAN_POINT('Origin',(30.,-1.32966554433622E-14,33.8637293696319));
#61126=CARTESIAN_POINT('',(29.8004337692194,2.69567237556048,33.8969505670765));
#61127=CARTESIAN_POINT('Ctrl Pts',(29.8004337692166,2.6956723755527,33.8969505670841));
#61128=CARTESIAN_POINT('Ctrl Pts',(29.8064896349356,2.71265541886987,33.8804609779983));
#61129=CARTESIAN_POINT('Ctrl Pts',(29.8126199288572,2.7298471883126,33.8637293696347));
#61130=CARTESIAN_POINT('',(29.775413173324,2.69370321195775,33.8969505670765));
#61131=CARTESIAN_POINT('Origin',(29.7874812116306,2.70030745889017,33.8912937927563));
#61132=CARTESIAN_POINT('',(29.7580309269809,2.72555094069389,33.8637293696319));
#61133=CARTESIAN_POINT('Ctrl Pts',(29.7580309269824,2.72555094069121,33.8637293696347));
#61134=CARTESIAN_POINT('Ctrl Pts',(29.766775132069,2.70952981970858,33.8804609779983));
#61135=CARTESIAN_POINT('Ctrl Pts',(29.775413173328,2.69370321195049,33.8969505670841));
#61136=CARTESIAN_POINT('',(29.5990162172122,2.70673030953515,33.8637293696319));
#61137=CARTESIAN_POINT('Origin',(30.,-1.32966554433622E-14,33.8637293696319));
#61138=CARTESIAN_POINT('',(29.589548948342,2.67170473125694,33.8969505670765));
#61139=CARTESIAN_POINT('Ctrl Pts',(29.5895489483398,2.67170473124897,33.8969505670841));
#61140=CARTESIAN_POINT('Ctrl Pts',(29.5942536716245,2.68911055925956,33.8804609779983));
#61141=CARTESIAN_POINT('Ctrl Pts',(29.5990162172114,2.7067303095322,33.8637293696347));
#61142=CARTESIAN_POINT('',(29.5647599813892,2.6677785445999,33.8969505670765));
#61143=CARTESIAN_POINT('Origin',(29.5762726922515,2.67530902338217,33.8912940899386));
#61144=CARTESIAN_POINT('',(29.5449325747129,2.6981643020872,33.8637293696319));
#61145=CARTESIAN_POINT('Ctrl Pts',(29.5449325747146,2.69816430208465,33.8637293696347));
#61146=CARTESIAN_POINT('Ctrl Pts',(29.554906827,2.68287863129518,33.8804609779983));
#61147=CARTESIAN_POINT('Ctrl Pts',(29.5647599813937,2.66777854459298,33.8969505670841));
#61148=CARTESIAN_POINT('',(29.3878847039277,2.66692553831737,33.8637293696319));
#61149=CARTESIAN_POINT('Origin',(30.,-1.32966554433622E-14,33.8637293696319));
#61150=CARTESIAN_POINT('',(29.3811946946869,2.63126513885323,33.8969505670765));
#61151=CARTESIAN_POINT('Ctrl Pts',(29.3811946946854,2.6312651388451,33.8969505670841));
#61152=CARTESIAN_POINT('Ctrl Pts',(29.3845192693522,2.64898643883141,33.8804609779983));
#61153=CARTESIAN_POINT('Ctrl Pts',(29.3878847039271,2.66692553831437,33.8637293696347));
#61154=CARTESIAN_POINT('',(29.3567901889011,2.6254061353882,33.8969505670765));
#61155=CARTESIAN_POINT('Origin',(29.3676766176014,2.6338164916465,33.8912943077151));
#61156=CARTESIAN_POINT('',(29.3346398644471,2.65414258332745,33.8637293696319));
#61157=CARTESIAN_POINT('Ctrl Pts',(29.334639864449,2.65414258332502,33.8637293696347));
#61158=CARTESIAN_POINT('Ctrl Pts',(29.3457826693511,2.63968660397215,33.8804609779983));
#61159=CARTESIAN_POINT('Ctrl Pts',(29.3567901889061,2.62540613538165,33.8969505670841));
#61160=CARTESIAN_POINT('',(29.1805270849924,2.61067828431312,33.8637293696319));
#61161=CARTESIAN_POINT('Origin',(30.,-1.32966554433622E-14,33.8637293696319));
#61162=CARTESIAN_POINT('',(29.1766555815128,2.57460292188403,33.8969505670765));
#61163=CARTESIAN_POINT('Ctrl Pts',(29.1766555815118,2.57460292187581,33.8969505670841));
#61164=CARTESIAN_POINT('Ctrl Pts',(29.1785795104524,2.59253043613048,33.8804609779983));
#61165=CARTESIAN_POINT('Ctrl Pts',(29.1805270849921,2.61067828431008,33.8637293696347));
#61166=CARTESIAN_POINT('',(29.1527859987874,2.56684722431571,33.8969505670765));
#61167=CARTESIAN_POINT('Origin',(29.162979042241,2.57608565616365,33.891294472568));
#61168=CARTESIAN_POINT('',(29.1284493206716,2.59375719294953,33.8637293696319));
#61169=CARTESIAN_POINT('Ctrl Pts',(29.1284493206737,2.59375719294727,33.8637293696347));
#61170=CARTESIAN_POINT('Ctrl Pts',(29.1406919790949,2.58022003095078,33.8804609779983));
#61171=CARTESIAN_POINT('Ctrl Pts',(29.1527859987929,2.56684722430958,33.8969505670841));
#61172=CARTESIAN_POINT('',(28.9782217890806,2.53833533054746,33.8637293696319));
#61173=CARTESIAN_POINT('Origin',(30.,-1.32966554433622E-14,33.8637293696319));
#61174=CARTESIAN_POINT('',(28.9771926604684,2.50206742175908,33.8969505670765));
#61175=CARTESIAN_POINT('Ctrl Pts',(28.9771926604681,2.50206742175082,33.8969505670841));
#61176=CARTESIAN_POINT('Ctrl Pts',(28.9777040820208,2.52009062118696,33.8804609779983));
#61177=CARTESIAN_POINT('Ctrl Pts',(28.9782217890805,2.5383353305444,33.8637293696347));
#61178=CARTESIAN_POINT('',(28.9540051647184,2.49246284654199,33.8969505670765));
#61179=CARTESIAN_POINT('Origin',(28.9634419889311,2.50247243285091,33.8912946002427));
#61180=CARTESIAN_POINT('',(28.9276321766543,2.51738042696527,33.8637293696319));
#61181=CARTESIAN_POINT('Ctrl Pts',(28.9276321766565,2.51738042696315,33.8637293696347));
#61182=CARTESIAN_POINT('Ctrl Pts',(28.9408992085365,2.50484554342835,33.8804609779983));
#61183=CARTESIAN_POINT('Ctrl Pts',(28.9540051647244,2.49246284653631,33.8969505670841));
#61184=CARTESIAN_POINT('',(28.7822160956148,2.45034269538683,33.8637293696319));
#61185=CARTESIAN_POINT('Origin',(30.,-1.32966554433622E-14,33.8637293696319));
#61186=CARTESIAN_POINT('Ctrl Pts',(28.7840356867905,2.41410584394887,33.8969505670841));
#61187=CARTESIAN_POINT('Ctrl Pts',(28.7831314478713,2.43211360954865,33.8804609779983));
#61188=CARTESIAN_POINT('Ctrl Pts',(28.782216095615,2.45034269538377,33.8637293696347));
#61189=CARTESIAN_POINT('',(28.7334265368663,2.42548317353484,33.8637293696319));
#61190=CARTESIAN_POINT('Ctrl Pts',(28.7334265368687,2.42548317353291,33.8637293696347));
#61191=CARTESIAN_POINT('Ctrl Pts',(28.7476361465443,2.41402785018503,33.8804609779983));
#61192=CARTESIAN_POINT('Ctrl Pts',(28.7616732366439,2.40271160648614,33.8969505670841));
#61193=CARTESIAN_POINT('',(28.5937184448738,2.3472428826875,33.8637293696319));
#61194=CARTESIAN_POINT('Origin',(30.,-1.32966554433622E-14,33.8637293696319));
#61195=CARTESIAN_POINT('Ctrl Pts',(28.5983755374531,2.31126050084732,33.8969505670841));
#61196=CARTESIAN_POINT('Ctrl Pts',(28.5960612129956,2.32914180874763,33.8804609779983));
#61197=CARTESIAN_POINT('Ctrl Pts',(28.5937184448742,2.34724288268447,33.8637293696347));
#61198=CARTESIAN_POINT('',(28.547029743657,2.31863200978457,33.8637293696319));
#61199=CARTESIAN_POINT('Ctrl Pts',(28.5470297436595,2.31863200978283,33.8637293696347));
#61200=CARTESIAN_POINT('Ctrl Pts',(28.5620943241618,2.30832687249961,33.8804609779983));
#61201=CARTESIAN_POINT('Ctrl Pts',(28.576976004845,2.29814685039931,33.8969505670841));
#61202=CARTESIAN_POINT('',(28.4138909875563,2.22967153707894,33.8637293696319));
#61203=CARTESIAN_POINT('Origin',(30.,-1.32966554433622E-14,33.8637293696319));
#61204=CARTESIAN_POINT('Ctrl Pts',(28.4213568690146,2.19416546818595,33.8969505670841));
#61205=CARTESIAN_POINT('Ctrl Pts',(28.4176467275988,2.21181007417744,33.8804609779983));
#61206=CARTESIAN_POINT('Ctrl Pts',(28.4138909875569,2.22967153707594,33.8637293696347));
#61207=CARTESIAN_POINT('',(28.3695909952396,2.19748570867059,33.8637293696319));
#61208=CARTESIAN_POINT('Ctrl Pts',(28.3695909952423,2.19748570866909,33.8637293696347));
#61209=CARTESIAN_POINT('Ctrl Pts',(28.3854176684231,2.18839429204867,33.8804609779983));
#61210=CARTESIAN_POINT('Ctrl Pts',(28.4010521891798,2.17941325476839,33.8969505670841));
#61211=CARTESIAN_POINT('',(28.2438424197352,2.09835352500326,33.8637293696319));
#61212=CARTESIAN_POINT('Origin',(30.,-1.32966554433622E-14,33.8637293696319));
#61213=CARTESIAN_POINT('Ctrl Pts',(28.2540710604308,2.06354267577915,33.8969505670841));
#61214=CARTESIAN_POINT('Ctrl Pts',(28.2489879763122,2.08084179499845,33.8804609779983));
#61215=CARTESIAN_POINT('Ctrl Pts',(28.2438424197361,2.09835352500033,33.8637293696347));
#61216=CARTESIAN_POINT('',(28.2022042605027,2.0627911774245,33.8637293696319));
#61217=CARTESIAN_POINT('Ctrl Pts',(28.2022042605055,2.0627911774232,33.8637293696347));
#61218=CARTESIAN_POINT('Ctrl Pts',(28.2186954496616,2.05496953307227,33.8804609779984));
#61219=CARTESIAN_POINT('Ctrl Pts',(28.2349864184722,2.04724285169337,33.8969505670841));
#61220=CARTESIAN_POINT('',(28.0846211473781,1.95409846567259,33.8637293696319));
#61221=CARTESIAN_POINT('Origin',(30.,-1.32966554433622E-14,33.8637293696319));
#61222=CARTESIAN_POINT('Ctrl Pts',(28.0975494843397,1.92019745657863,33.8969505670841));
#61223=CARTESIAN_POINT('Ctrl Pts',(28.0911247964223,1.9370444342032,33.8804609779983));
#61224=CARTESIAN_POINT('Ctrl Pts',(28.0846211473792,1.95409846566974,33.8637293696347));
#61225=CARTESIAN_POINT('',(28.0459015343274,1.91537885262192,33.8637293696319));
#61226=CARTESIAN_POINT('Ctrl Pts',(28.0459015343303,1.91537885262084,33.8637293696347));
#61227=CARTESIAN_POINT('Ctrl Pts',(28.0629555657968,1.90887520357776,33.8804609779983));
#61228=CARTESIAN_POINT('Ctrl Pts',(28.0798025434214,1.90245051566032,33.8969505670841));
#61229=CARTESIAN_POINT('',(27.9372088225755,1.79779573949736,33.8637293696319));
#61230=CARTESIAN_POINT('Origin',(30.,-1.32966554433622E-14,33.8637293696319));
#61231=CARTESIAN_POINT('Ctrl Pts',(27.9527571483066,1.76501358152779,33.8969505670841));
#61232=CARTESIAN_POINT('Ctrl Pts',(27.9450304669277,1.78130455033841,33.8804609779983));
#61233=CARTESIAN_POINT('Ctrl Pts',(27.9372088225768,1.79779573949458,33.8637293696347));
#61234=CARTESIAN_POINT('',(27.9016464749967,1.75615758026483,33.8637293696319));
#61235=CARTESIAN_POINT('Ctrl Pts',(27.9016464749997,1.75615758026397,33.8637293696347));
#61236=CARTESIAN_POINT('Ctrl Pts',(27.9191582050016,1.75101202368779,33.8804609779983));
#61237=CARTESIAN_POINT('Ctrl Pts',(27.9364573242208,1.74592893956924,33.8969505670841));
#61238=CARTESIAN_POINT('',(27.8025142913294,1.63040900476038,33.8637293696319));
#61239=CARTESIAN_POINT('Origin',(30.,-1.32966554433622E-14,33.8637293696319));
#61240=CARTESIAN_POINT('Ctrl Pts',(27.8205867452316,1.59894781082027,33.8969505670841));
#61241=CARTESIAN_POINT('Ctrl Pts',(27.8116057079513,1.61458233157693,33.8804609779983));
#61242=CARTESIAN_POINT('Ctrl Pts',(27.8025142913309,1.63040900475771,33.8637293696347));
#61243=CARTESIAN_POINT('',(27.7703284629211,1.58610901244374,33.8637293696319));
#61244=CARTESIAN_POINT('Ctrl Pts',(27.7703284629241,1.58610901244311,33.8637293696347));
#61245=CARTESIAN_POINT('Ctrl Pts',(27.7881899258226,1.5823532724012,33.8804609779984));
#61246=CARTESIAN_POINT('Ctrl Pts',(27.8058345318141,1.57864313098542,33.8969505670841));
#61247=CARTESIAN_POINT('',(27.6813679902154,1.45297025634305,33.8637293696319));
#61248=CARTESIAN_POINT('Origin',(30.,-1.32966554433622E-14,33.8637293696319));
#61249=CARTESIAN_POINT('Ctrl Pts',(27.7018531496007,1.423023995155,33.8969505670841));
#61250=CARTESIAN_POINT('Ctrl Pts',(27.6916731275004,1.43790567583821,33.8804609779983));
#61251=CARTESIAN_POINT('Ctrl Pts',(27.6813679902172,1.45297025634054,33.8637293696347));
#61252=CARTESIAN_POINT('',(27.6527571173125,1.40628155512618,33.8637293696319));
#61253=CARTESIAN_POINT('Ctrl Pts',(27.6527571173155,1.40628155512578,33.8637293696347));
#61254=CARTESIAN_POINT('Ctrl Pts',(27.6708581912524,1.40393878700439,33.8804609779983));
#61255=CARTESIAN_POINT('Ctrl Pts',(27.6887394991527,1.40162446254697,33.8969505670841));
#61256=CARTESIAN_POINT('',(27.5745168264652,1.26657346313372,33.8637293696319));
#61257=CARTESIAN_POINT('Origin',(30.,-1.32966554433622E-14,33.8637293696319));
#61258=CARTESIAN_POINT('Ctrl Pts',(27.5972883935138,1.23832676335601,33.8969505670841));
#61259=CARTESIAN_POINT('Ctrl Pts',(27.5859721498149,1.2523638534557,33.8804609779984));
#61260=CARTESIAN_POINT('Ctrl Pts',(27.5745168264671,1.26657346313129,33.8637293696347));
#61261=CARTESIAN_POINT('',(27.5496573046132,1.21778390438518,33.8637293696319));
#61262=CARTESIAN_POINT('Ctrl Pts',(27.5496573046163,1.21778390438503,33.8637293696347));
#61263=CARTESIAN_POINT('Ctrl Pts',(27.5678863904514,1.21686855212868,33.8804609779984));
#61264=CARTESIAN_POINT('Ctrl Pts',(27.5858941560511,1.21596431320949,33.8969505670841));
#61265=CARTESIAN_POINT('',(27.4826195730347,1.07236782334576,33.8637293696319));
#61266=CARTESIAN_POINT('Origin',(30.,-1.32966554433622E-14,33.8637293696319));
#61267=CARTESIAN_POINT('Ctrl Pts',(27.5075371534637,1.04599483527557,33.8969505670841));
#61268=CARTESIAN_POINT('Ctrl Pts',(27.4951544565716,1.05910079146348,33.8804609779983));
#61269=CARTESIAN_POINT('Ctrl Pts',(27.4826195730368,1.07236782334352,33.8637293696347));
#61270=CARTESIAN_POINT('',(27.4616646694525,1.02177821091942,33.8637293696319));
#61271=CARTESIAN_POINT('Ctrl Pts',(27.4616646694556,1.0217782109195,33.8637293696347));
#61272=CARTESIAN_POINT('Ctrl Pts',(27.479909378813,1.02229591797925,33.8804609779983));
#61273=CARTESIAN_POINT('Ctrl Pts',(27.4979325782492,1.0228073395319,33.8969505670841));
#61274=CARTESIAN_POINT('',(27.4062428070505,0.871550679328378,33.8637293696319));
#61275=CARTESIAN_POINT('Origin',(30.,-1.32966554433622E-14,33.8637293696319));
#61276=CARTESIAN_POINT('Ctrl Pts',(27.4331527756904,0.847214001207086,33.8969505670841));
#61277=CARTESIAN_POINT('Ctrl Pts',(27.4197799690492,0.859308020905129,33.8804609779984));
#61278=CARTESIAN_POINT('Ctrl Pts',(27.4062428070528,0.871550679326332,33.8637293696347));
#61279=CARTESIAN_POINT('',(27.3893217156869,0.819472915007596,33.8637293696319));
#61280=CARTESIAN_POINT('Ctrl Pts',(27.3893217156899,0.819472915007932,33.8637293696347));
#61281=CARTESIAN_POINT('Ctrl Pts',(27.4074695638695,0.821420489547589,33.8804609779983));
#61282=CARTESIAN_POINT('Ctrl Pts',(27.4253970781241,0.823344418488154,33.8969505670841));
#61283=CARTESIAN_POINT('',(27.3458574166725,0.665360135552929,33.8637293696319));
#61284=CARTESIAN_POINT('Origin',(30.,-1.32966554433622E-14,33.8637293696319));
#61285=CARTESIAN_POINT('Ctrl Pts',(27.3745938646183,0.643209811093841,33.8969505670841));
#61286=CARTESIAN_POINT('Ctrl Pts',(27.3603133960278,0.654217330648928,33.8804609779983));
#61287=CARTESIAN_POINT('Ctrl Pts',(27.3458574166749,0.665360135551045,33.8637293696347));
#61288=CARTESIAN_POINT('',(27.3330744616826,0.612115296072357,33.8637293696319));
#61289=CARTESIAN_POINT('Ctrl Pts',(27.3330744616856,0.612115296072913,33.8637293696347));
#61290=CARTESIAN_POINT('Ctrl Pts',(27.3510135611686,0.615480730647817,33.8804609779983));
#61291=CARTESIAN_POINT('Ctrl Pts',(27.3687348611549,0.618805305314613,33.8969505670841));
#61292=CARTESIAN_POINT('',(27.3018356979128,0.455067425287102,33.8637293696319));
#61293=CARTESIAN_POINT('Origin',(30.,-1.32966554433622E-14,33.8637293696319));
#61294=CARTESIAN_POINT('Ctrl Pts',(27.332221455407,0.435240018606297,33.8969505670841));
#61295=CARTESIAN_POINT('Ctrl Pts',(27.3171213687048,0.445093172999983,33.8804609779983));
#61296=CARTESIAN_POINT('Ctrl Pts',(27.3018356979154,0.455067425285416,33.8637293696347));
#61297=CARTESIAN_POINT('',(27.2932696904648,0.400983782787843,33.8637293696319));
#61298=CARTESIAN_POINT('Ctrl Pts',(27.2932696904678,0.40098378278865,33.8637293696347));
#61299=CARTESIAN_POINT('Ctrl Pts',(27.3108894407404,0.405746328375518,33.8804609779983));
#61300=CARTESIAN_POINT('Ctrl Pts',(27.328295268751,0.410451051660182,33.8969505670841));
#61301=CARTESIAN_POINT('',(27.2744490593061,0.241969073019103,33.8637293696319));
#61302=CARTESIAN_POINT('Origin',(30.,-1.32966554433622E-14,33.8637293696319));
#61303=CARTESIAN_POINT('Ctrl Pts',(27.3062967880495,0.224586826672042,33.8969505670841));
#61304=CARTESIAN_POINT('Ctrl Pts',(27.2904701802914,0.233224867930985,33.8804609779983));
#61305=CARTESIAN_POINT('Ctrl Pts',(27.2744490593088,0.24196907301762,33.8637293696347));
#61306=CARTESIAN_POINT('',(27.2701528116845,0.1873800711418,33.8637293696319));
#61307=CARTESIAN_POINT('Ctrl Pts',(27.2701528116874,0.187380071142834,33.8637293696347));
#61308=CARTESIAN_POINT('Ctrl Pts',(27.2873445811301,0.193510365064418,33.8804609779983));
#61309=CARTESIAN_POINT('Ctrl Pts',(27.3043276244473,0.199566230783421,33.8969505670841));
#61310=CARTESIAN_POINT('',(27.2638663485864,0.0273789009530583,33.8637293696319));
#61311=CARTESIAN_POINT('Origin',(30.,-1.32966554433622E-14,33.8637293696319));
#61312=CARTESIAN_POINT('Ctrl Pts',(27.2969796967408,0.0125489822686371,
33.8969505670841));
#61313=CARTESIAN_POINT('Ctrl Pts',(27.2805241442266,0.0199186539960461,
33.8804609779983));
#61314=CARTESIAN_POINT('Ctrl Pts',(27.2638663485892,0.0273789009517924,
33.8637293696347));
#61315=CARTESIAN_POINT('',(27.2638663485864,-0.0273789009530277,33.8637293696319));
#61316=CARTESIAN_POINT('Ctrl Pts',(27.2638663485892,-0.0273789009517733,
33.8637293696347));
#61317=CARTESIAN_POINT('Ctrl Pts',(27.2805241442266,-0.0199186539960275,
33.8804609779983));
#61318=CARTESIAN_POINT('Ctrl Pts',(27.2969796967409,-0.012548982268619,
33.8969505670841));
#61319=CARTESIAN_POINT('',(27.2701528116845,-0.18738007114177,33.8637293696319));
#61320=CARTESIAN_POINT('Origin',(30.,-1.32966554433622E-14,33.8637293696319));
#61321=CARTESIAN_POINT('',(27.3043276244395,-0.199566230780611,33.8969505670765));
#61322=CARTESIAN_POINT('Ctrl Pts',(27.3043276244473,-0.199566230783401,
33.8969505670841));
#61323=CARTESIAN_POINT('Ctrl Pts',(27.2873445811301,-0.193510365064398,
33.8804609779983));
#61324=CARTESIAN_POINT('Ctrl Pts',(27.2701528116874,-0.187380071142813,
33.8637293696347));
#61325=CARTESIAN_POINT('',(27.3062967880422,-0.224586826675978,33.8969505670765));
#61326=CARTESIAN_POINT('Origin',(27.2996925411099,-0.212518788369432,33.8912937927564));
#61327=CARTESIAN_POINT('',(27.2744490593061,-0.241969073019072,33.8637293696319));
#61328=CARTESIAN_POINT('Ctrl Pts',(27.2744490593088,-0.241969073017592,
33.8637293696347));
#61329=CARTESIAN_POINT('Ctrl Pts',(27.2904701802914,-0.233224867930958,
33.8804609779983));
#61330=CARTESIAN_POINT('Ctrl Pts',(27.3062967880495,-0.224586826672017,
33.8969505670841));
#61331=CARTESIAN_POINT('',(27.2932696904648,-0.400983782787811,33.8637293696319));
#61332=CARTESIAN_POINT('Origin',(30.,-1.32966554433622E-14,33.8637293696319));
#61333=CARTESIAN_POINT('',(27.328295268743,-0.410451051657984,33.8969505670765));
#61334=CARTESIAN_POINT('Ctrl Pts',(27.328295268751,-0.410451051660133,33.8969505670841));
#61335=CARTESIAN_POINT('Ctrl Pts',(27.3108894407404,-0.40574632837547,33.8804609779983));
#61336=CARTESIAN_POINT('Ctrl Pts',(27.2932696904678,-0.400983782788603,
33.8637293696347));
#61337=CARTESIAN_POINT('',(27.3322214554001,-0.435240018610796,33.8969505670765));
#61338=CARTESIAN_POINT('Origin',(27.3246909766178,-0.423727307748468,33.8912940899386));
#61339=CARTESIAN_POINT('',(27.3018356979128,-0.45506742528707,33.8637293696319));
#61340=CARTESIAN_POINT('Ctrl Pts',(27.3018356979154,-0.455067425285398,
33.8637293696347));
#61341=CARTESIAN_POINT('Ctrl Pts',(27.3171213687048,-0.445093172999969,
33.8804609779984));
#61342=CARTESIAN_POINT('Ctrl Pts',(27.332221455407,-0.435240018606285,33.8969505670841));
#61343=CARTESIAN_POINT('',(27.3330744616826,-0.612115296072328,33.8637293696319));
#61344=CARTESIAN_POINT('Origin',(30.,-1.32966554433622E-14,33.8637293696319));
#61345=CARTESIAN_POINT('',(27.3687348611467,-0.618805305313063,33.8969505670765));
#61346=CARTESIAN_POINT('Ctrl Pts',(27.3687348611549,-0.618805305314591,
33.8969505670841));
#61347=CARTESIAN_POINT('Ctrl Pts',(27.3510135611686,-0.615480730647799,
33.8804609779983));
#61348=CARTESIAN_POINT('Ctrl Pts',(27.3330744616856,-0.6121152960729,33.8637293696347));
#61349=CARTESIAN_POINT('',(27.3745938646118,-0.643209811098888,33.8969505670765));
#61350=CARTESIAN_POINT('Origin',(27.3661835083535,-0.632323382398592,33.8912943077151));
#61351=CARTESIAN_POINT('',(27.3458574166725,-0.665360135552901,33.8637293696319));
#61352=CARTESIAN_POINT('Ctrl Pts',(27.345857416675,-0.665360135551053,33.8637293696347));
#61353=CARTESIAN_POINT('Ctrl Pts',(27.3603133960278,-0.654217330648938,
33.8804609779984));
#61354=CARTESIAN_POINT('Ctrl Pts',(27.3745938646183,-0.643209811093851,
33.8969505670841));
#61355=CARTESIAN_POINT('',(27.3893217156868,-0.819472915007569,33.8637293696319));
#61356=CARTESIAN_POINT('Origin',(30.,-1.32966554433622E-14,33.8637293696319));
#61357=CARTESIAN_POINT('',(27.4253970781159,-0.823344418487241,33.8969505670765));
#61358=CARTESIAN_POINT('Ctrl Pts',(27.4253970781241,-0.823344418488121,
33.8969505670841));
#61359=CARTESIAN_POINT('Ctrl Pts',(27.4074695638695,-0.821420489547552,
33.8804609779983));
#61360=CARTESIAN_POINT('Ctrl Pts',(27.3893217156899,-0.819472915007892,
33.8637293696347));
#61361=CARTESIAN_POINT('',(27.4331527756843,-0.847214001212589,33.8969505670765));
#61362=CARTESIAN_POINT('Origin',(27.4239143438363,-0.837020957758988,33.8912944725679));
#61363=CARTESIAN_POINT('',(27.4062428070504,-0.871550679328351,33.8637293696319));
#61364=CARTESIAN_POINT('Ctrl Pts',(27.4062428070527,-0.871550679326329,
33.8637293696347));
#61365=CARTESIAN_POINT('Ctrl Pts',(27.4197799690492,-0.859308020905111,
33.8804609779983));
#61366=CARTESIAN_POINT('Ctrl Pts',(27.4331527756904,-0.847214001207053,
33.8969505670841));
#61367=CARTESIAN_POINT('',(27.4616646694525,-1.02177821091939,33.8637293696319));
#61368=CARTESIAN_POINT('Origin',(30.,-1.32966554433622E-14,33.8637293696319));
#61369=CARTESIAN_POINT('',(27.4979325782409,-1.02280733953164,33.8969505670765));
#61370=CARTESIAN_POINT('Ctrl Pts',(27.4979325782492,-1.02280733953187,33.8969505670841));
#61371=CARTESIAN_POINT('Ctrl Pts',(27.479909378813,-1.02229591797922,33.8804609779983));
#61372=CARTESIAN_POINT('Ctrl Pts',(27.4616646694556,-1.02177821091947,33.8637293696347));
#61373=CARTESIAN_POINT('',(27.507537153458,-1.04599483528157,33.8969505670765));
#61374=CARTESIAN_POINT('Origin',(27.4975275671491,-1.03655801106889,33.8912946002427));
#61375=CARTESIAN_POINT('',(27.4826195730347,-1.07236782334573,33.8637293696319));
#61376=CARTESIAN_POINT('Ctrl Pts',(27.4826195730368,-1.07236782334351,33.8637293696347));
#61377=CARTESIAN_POINT('Ctrl Pts',(27.4951544565716,-1.05910079146347,33.8804609779983));
#61378=CARTESIAN_POINT('Ctrl Pts',(27.5075371534637,-1.04599483527557,33.8969505670841));
#61379=CARTESIAN_POINT('',(27.5496573046131,-1.21778390438516,33.8637293696319));
#61380=CARTESIAN_POINT('Origin',(30.,-1.32966554433622E-14,33.8637293696319));
#61381=CARTESIAN_POINT('',(27.5858941560428,-1.21596431320988,33.8969505670765));
#61382=CARTESIAN_POINT('Ctrl Pts',(27.5858941560511,-1.21596431320946,33.8969505670841));
#61383=CARTESIAN_POINT('Ctrl Pts',(27.5678863904513,-1.21686855212866,33.8804609779983));
#61384=CARTESIAN_POINT('Ctrl Pts',(27.5496573046162,-1.217783904385,33.8637293696347));
#61385=CARTESIAN_POINT('',(27.5972883935086,-1.23832676336246,33.8969505670765));
#61386=CARTESIAN_POINT('Origin',(27.5865693373251,-1.22970433386023,33.891294700665));
#61387=CARTESIAN_POINT('',(27.5745168264651,-1.2665734631337,33.8637293696319));
#61388=CARTESIAN_POINT('Ctrl Pts',(27.574516826467,-1.26657346313129,33.8637293696347));
#61389=CARTESIAN_POINT('Ctrl Pts',(27.5859721498149,-1.2523638534557,33.8804609779983));
#61390=CARTESIAN_POINT('Ctrl Pts',(27.5972883935138,-1.23832676335601,33.8969505670841));
#61391=CARTESIAN_POINT('',(27.6527571173125,-1.40628155512615,33.8637293696319));
#61392=CARTESIAN_POINT('Origin',(30.,-1.32966554433622E-14,33.8637293696319));
#61393=CARTESIAN_POINT('',(27.6887394991444,-1.40162446254801,33.8969505670765));
#61394=CARTESIAN_POINT('Ctrl Pts',(27.6887394991526,-1.40162446254695,33.8969505670841));
#61395=CARTESIAN_POINT('Ctrl Pts',(27.6708581912523,-1.40393878700437,33.8804609779983));
#61396=CARTESIAN_POINT('Ctrl Pts',(27.6527571173155,-1.40628155512576,33.8637293696347));
#61397=CARTESIAN_POINT('',(27.701853149596,-1.42302399516179,33.8969505670765));
#61398=CARTESIAN_POINT('Origin',(27.6904906884452,-1.4152691174526,33.8912947803756));
#61399=CARTESIAN_POINT('',(27.6813679902154,-1.45297025634303,33.8637293696319));
#61400=CARTESIAN_POINT('Ctrl Pts',(27.6813679902171,-1.4529702563405,33.8637293696347));
#61401=CARTESIAN_POINT('Ctrl Pts',(27.6916731275004,-1.43790567583818,33.8804609779983));
#61402=CARTESIAN_POINT('Ctrl Pts',(27.7018531496007,-1.42302399515497,33.8969505670841));
#61403=CARTESIAN_POINT('',(27.770328462921,-1.58610901244372,33.8637293696319));
#61404=CARTESIAN_POINT('Origin',(30.,-1.32966554433622E-14,33.8637293696319));
#61405=CARTESIAN_POINT('',(27.8058345318059,-1.5786431309871,33.8969505670765));
#61406=CARTESIAN_POINT('Ctrl Pts',(27.805834531814,-1.5786431309854,33.8969505670841));
#61407=CARTESIAN_POINT('Ctrl Pts',(27.7881899258225,-1.58235327240118,33.8804609779983));
#61408=CARTESIAN_POINT('Ctrl Pts',(27.770328462924,-1.5861090124431,33.8637293696347));
#61409=CARTESIAN_POINT('',(27.8205867452275,-1.59894781082744,33.8969505670765));
#61410=CARTESIAN_POINT('Origin',(27.8086509152839,-1.59210829514295,33.8912948438349));
#61411=CARTESIAN_POINT('',(27.8025142913294,-1.63040900476036,33.8637293696319));
#61412=CARTESIAN_POINT('Ctrl Pts',(27.8025142913309,-1.63040900475772,33.8637293696347));
#61413=CARTESIAN_POINT('Ctrl Pts',(27.8116057079513,-1.61458233157693,33.8804609779984));
#61414=CARTESIAN_POINT('Ctrl Pts',(27.8205867452316,-1.59894781082027,33.8969505670841));
#61415=CARTESIAN_POINT('',(27.9016464749967,-1.75615758026481,33.8637293696319));
#61416=CARTESIAN_POINT('Origin',(30.,-1.32966554433622E-14,33.8637293696319));
#61417=CARTESIAN_POINT('',(27.9364573242129,-1.74592893957155,33.8969505670765));
#61418=CARTESIAN_POINT('Ctrl Pts',(27.9364573242208,-1.74592893956922,33.8969505670841));
#61419=CARTESIAN_POINT('Ctrl Pts',(27.9191582050015,-1.75101202368778,33.8804609779983));
#61420=CARTESIAN_POINT('Ctrl Pts',(27.9016464749996,-1.75615758026396,33.8637293696347));
#61421=CARTESIAN_POINT('',(27.9527571483031,-1.76501358153525,33.8969505670765));
#61422=CARTESIAN_POINT('Origin',(27.9403215240917,-1.75913159602167,33.8912948941586));
#61423=CARTESIAN_POINT('',(27.9372088225755,-1.79779573949734,33.8637293696319));
#61424=CARTESIAN_POINT('Ctrl Pts',(27.9372088225768,-1.79779573949458,33.8637293696347));
#61425=CARTESIAN_POINT('Ctrl Pts',(27.9450304669278,-1.78130455033841,33.8804609779984));
#61426=CARTESIAN_POINT('Ctrl Pts',(27.9527571483066,-1.76501358152779,33.8969505670841));
#61427=CARTESIAN_POINT('',(28.0459015343274,-1.91537885262191,33.8637293696319));
#61428=CARTESIAN_POINT('Origin',(30.,-1.32966554433622E-14,33.8637293696319));
#61429=CARTESIAN_POINT('',(28.0798025434136,-1.90245051566325,33.8969505670765));
#61430=CARTESIAN_POINT('Ctrl Pts',(28.0798025434214,-1.90245051566032,33.8969505670841));
#61431=CARTESIAN_POINT('Ctrl Pts',(28.0629555657968,-1.90887520357775,33.8804609779983));
#61432=CARTESIAN_POINT('Ctrl Pts',(28.0459015343303,-1.91537885262082,33.8637293696347));
#61433=CARTESIAN_POINT('',(28.0975494843367,-1.92019745658631,33.8969505670765));
#61434=CARTESIAN_POINT('Origin',(28.0846907243829,-1.91530926701236,33.891294933562));
#61435=CARTESIAN_POINT('',(28.084621147378,-1.95409846567257,33.8637293696319));
#61436=CARTESIAN_POINT('Ctrl Pts',(28.0846211473791,-1.9540984656697,33.8637293696347));
#61437=CARTESIAN_POINT('Ctrl Pts',(28.0911247964222,-1.93704443420316,33.8804609779983));
#61438=CARTESIAN_POINT('Ctrl Pts',(28.0975494843396,-1.92019745657857,33.8969505670841));
#61439=CARTESIAN_POINT('',(28.2022042605026,-2.06279117742449,33.8637293696319));
#61440=CARTESIAN_POINT('Origin',(30.,-1.32966554433622E-14,33.8637293696319));
#61441=CARTESIAN_POINT('',(28.2349864184647,-2.04724285169689,33.8969505670765));
#61442=CARTESIAN_POINT('Ctrl Pts',(28.2349864184722,-2.04724285169334,33.8969505670841));
#61443=CARTESIAN_POINT('Ctrl Pts',(28.2186954496616,-2.05496953307223,33.8804609779983));
#61444=CARTESIAN_POINT('Ctrl Pts',(28.2022042605054,-2.06279117742317,33.8637293696347));
#61445=CARTESIAN_POINT('',(28.2540710604284,-2.06354267578707,33.8969505670765));
#61446=CARTESIAN_POINT('Origin',(28.2408684341297,-2.05967842174595,33.8912949636253));
#61447=CARTESIAN_POINT('',(28.2438424197351,-2.09835352500325,33.8637293696319));
#61448=CARTESIAN_POINT('Ctrl Pts',(28.243842419736,-2.09835352500031,33.8637293696347));
#61449=CARTESIAN_POINT('Ctrl Pts',(28.2489879763122,-2.08084179499844,33.8804609779983));
#61450=CARTESIAN_POINT('Ctrl Pts',(28.2540710604307,-2.06354267577914,33.8969505670841));
#61451=CARTESIAN_POINT('',(28.3695909952396,-2.19748570867058,33.8637293696319));
#61452=CARTESIAN_POINT('Origin',(30.,-1.32966554433622E-14,33.8637293696319));
#61453=CARTESIAN_POINT('',(28.4010521891725,-2.17941325477249,33.8969505670765));
#61454=CARTESIAN_POINT('Ctrl Pts',(28.4010521891797,-2.17941325476838,33.8969505670841));
#61455=CARTESIAN_POINT('Ctrl Pts',(28.385417668423,-2.18839429204864,33.8804609779983));
#61456=CARTESIAN_POINT('Ctrl Pts',(28.3695909952423,-2.19748570866905,33.8637293696347));
#61457=CARTESIAN_POINT('',(28.4213568690129,-2.19416546819403,33.8969505670765));
#61458=CARTESIAN_POINT('Origin',(28.4078917675746,-2.19134897714168,33.8912949854673));
#61459=CARTESIAN_POINT('',(28.4138909875562,-2.22967153707893,33.8637293696319));
#61460=CARTESIAN_POINT('Ctrl Pts',(28.4138909875569,-2.22967153707595,33.8637293696347));
#61461=CARTESIAN_POINT('Ctrl Pts',(28.4176467275988,-2.21181007417744,33.8804609779984));
#61462=CARTESIAN_POINT('Ctrl Pts',(28.4213568690146,-2.19416546818595,33.8969505670841));
#61463=CARTESIAN_POINT('',(28.5470297436569,-2.31863200978456,33.8637293696319));
#61464=CARTESIAN_POINT('Origin',(30.,-1.32966554433622E-14,33.8637293696319));
#61465=CARTESIAN_POINT('',(28.5769760048382,-2.29814685040397,33.8969505670765));
#61466=CARTESIAN_POINT('Ctrl Pts',(28.576976004845,-2.29814685039931,33.8969505670841));
#61467=CARTESIAN_POINT('Ctrl Pts',(28.5620943241618,-2.30832687249962,33.8804609779983));
#61468=CARTESIAN_POINT('Ctrl Pts',(28.5470297436595,-2.31863200978285,33.8637293696347));
#61469=CARTESIAN_POINT('',(28.5983755374519,-2.31126050085552,33.8969505670765));
#61470=CARTESIAN_POINT('Origin',(28.5847309718512,-2.30950914111276,33.891294999854));
#61471=CARTESIAN_POINT('',(28.5937184448738,-2.3472428826875,33.8637293696319));
#61472=CARTESIAN_POINT('Ctrl Pts',(28.5937184448742,-2.34724288268445,33.8637293696347));
#61473=CARTESIAN_POINT('Ctrl Pts',(28.5960612129955,-2.32914180874762,33.8804609779983));
#61474=CARTESIAN_POINT('Ctrl Pts',(28.598375537453,-2.31126050084731,33.8969505670841));
#61475=CARTESIAN_POINT('',(28.7334265368663,-2.42548317353484,33.8637293696319));
#61476=CARTESIAN_POINT('Origin',(30.,-1.32966554433622E-14,33.8637293696319));
#61477=CARTESIAN_POINT('',(28.7616732366375,-2.40271160649133,33.8969505670765));
#61478=CARTESIAN_POINT('Ctrl Pts',(28.761673236644,-2.40271160648615,33.8969505670841));
#61479=CARTESIAN_POINT('Ctrl Pts',(28.7476361465443,-2.41402785018505,33.8804609779983));
#61480=CARTESIAN_POINT('Ctrl Pts',(28.7334265368687,-2.42548317353292,33.8637293696347));
#61481=CARTESIAN_POINT('',(28.7840356867901,-2.41410584395713,33.8969505670765));
#61482=CARTESIAN_POINT('Origin',(28.7702957758346,-2.41343041757033,33.8912950072666));
#61483=CARTESIAN_POINT('',(28.7822160956148,-2.45034269538683,33.8637293696319));
#61484=CARTESIAN_POINT('Ctrl Pts',(28.782216095615,-2.45034269538378,33.8637293696347));
#61485=CARTESIAN_POINT('Ctrl Pts',(28.7831314478713,-2.43211360954867,33.8804609779983));
#61486=CARTESIAN_POINT('Ctrl Pts',(28.7840356867905,-2.41410584394888,33.8969505670841));
#61487=CARTESIAN_POINT('',(28.9276321766542,-2.51738042696528,33.8637293696319));
#61488=CARTESIAN_POINT('Origin',(30.,-1.32966554433622E-14,33.8637293696319));
#61489=CARTESIAN_POINT('',(28.9540051647184,-2.49246284654199,33.8969505670765));
#61490=CARTESIAN_POINT('Ctrl Pts',(28.9540051647244,-2.49246284653629,33.8969505670841));
#61491=CARTESIAN_POINT('Ctrl Pts',(28.9408992085365,-2.50484554342835,33.8804609779984));
#61492=CARTESIAN_POINT('Ctrl Pts',(28.9276321766564,-2.51738042696316,33.8637293696347));
#61493=CARTESIAN_POINT('',(28.9771926604683,-2.50206742175908,33.8969505670765));
#61494=CARTESIAN_POINT('Origin',(28.9634421120889,-2.50247209787259,33.8912950079413));
#61495=CARTESIAN_POINT('',(28.9782217890806,-2.53833533054747,33.8637293696319));
#61496=CARTESIAN_POINT('Ctrl Pts',(28.9782217890805,-2.53833533054441,33.8637293696347));
#61497=CARTESIAN_POINT('Ctrl Pts',(28.9777040820207,-2.52009062118697,33.8804609779983));
#61498=CARTESIAN_POINT('Ctrl Pts',(28.9771926604681,-2.50206742175082,33.8969505670841));
#61499=CARTESIAN_POINT('',(29.1284493206716,-2.59375719294953,33.8637293696319));
#61500=CARTESIAN_POINT('Origin',(30.,-1.32966554433622E-14,33.8637293696319));
#61501=CARTESIAN_POINT('',(29.1527859987874,-2.56684722431572,33.8969505670765));
#61502=CARTESIAN_POINT('Ctrl Pts',(29.1527859987929,-2.56684722430957,33.8969505670841));
#61503=CARTESIAN_POINT('Ctrl Pts',(29.1406919790949,-2.58022003095078,33.8804609779984));
#61504=CARTESIAN_POINT('Ctrl Pts',(29.1284493206736,-2.59375719294726,33.8637293696347));
#61505=CARTESIAN_POINT('',(29.1766555815127,-2.57460292188404,33.8969505670765));
#61506=CARTESIAN_POINT('Origin',(29.1629791704777,-2.57608521103258,33.8912950018861));
#61507=CARTESIAN_POINT('',(29.1805270849924,-2.61067828431313,33.8637293696319));
#61508=CARTESIAN_POINT('Ctrl Pts',(29.1805270849921,-2.61067828431009,33.8637293696347));
#61509=CARTESIAN_POINT('Ctrl Pts',(29.1785795104524,-2.59253043613049,33.8804609779983));
#61510=CARTESIAN_POINT('Ctrl Pts',(29.1766555815118,-2.57460292187582,33.8969505670841));
#61511=CARTESIAN_POINT('',(29.334639864447,-2.65414258332747,33.8637293696319));
#61512=CARTESIAN_POINT('Origin',(30.,-1.32966554433622E-14,33.8637293696319));
#61513=CARTESIAN_POINT('',(29.3567901889011,-2.62540613538822,33.8969505670765));
#61514=CARTESIAN_POINT('Ctrl Pts',(29.3567901889061,-2.62540613538166,33.8969505670841));
#61515=CARTESIAN_POINT('Ctrl Pts',(29.345782669351,-2.63968660397217,33.8804609779983));
#61516=CARTESIAN_POINT('Ctrl Pts',(29.3346398644489,-2.65414258332506,33.8637293696347));
#61517=CARTESIAN_POINT('',(29.3811946946869,-2.63126513885324,33.8969505670765));
#61518=CARTESIAN_POINT('Origin',(29.3676767399569,-2.63381590833404,33.8912949888765));
#61519=CARTESIAN_POINT('',(29.3878847039276,-2.66692553831738,33.8637293696319));
#61520=CARTESIAN_POINT('Ctrl Pts',(29.3878847039271,-2.66692553831437,33.8637293696347));
#61521=CARTESIAN_POINT('Ctrl Pts',(29.3845192693522,-2.64898643883142,33.8804609779983));
#61522=CARTESIAN_POINT('Ctrl Pts',(29.3811946946854,-2.63126513884512,33.8969505670841));
#61523=CARTESIAN_POINT('',(29.5449325747129,-2.69816430208721,33.8637293696319));
#61524=CARTESIAN_POINT('Origin',(30.,-1.32966554433622E-14,33.8637293696319));
#61525=CARTESIAN_POINT('',(29.5647599813891,-2.66777854459992,33.8969505670765));
#61526=CARTESIAN_POINT('Ctrl Pts',(29.5647599813936,-2.667778544593,33.8969505670841));
#61527=CARTESIAN_POINT('Ctrl Pts',(29.554906827,-2.68287863129519,33.8804609779983));
#61528=CARTESIAN_POINT('Ctrl Pts',(29.5449325747145,-2.69816430208464,33.8637293696347));
#61529=CARTESIAN_POINT('',(29.589548948342,-2.67170473125696,33.8969505670765));
#61530=CARTESIAN_POINT('Origin',(29.5762727932907,-2.67530826149246,33.8912949684251));
#61531=CARTESIAN_POINT('',(29.5990162172121,-2.70673030953517,33.8637293696319));
#61532=CARTESIAN_POINT('Ctrl Pts',(29.5990162172114,-2.70673030953221,33.8637293696347));
#61533=CARTESIAN_POINT('Ctrl Pts',(29.5942536716245,-2.68911055925957,33.8804609779984));
#61534=CARTESIAN_POINT('Ctrl Pts',(29.5895489483398,-2.67170473124899,33.8969505670841));
#61535=CARTESIAN_POINT('',(29.7580309269809,-2.72555094069392,33.8637293696319));
#61536=CARTESIAN_POINT('Origin',(30.,-1.32966554433622E-14,33.8637293696319));
#61537=CARTESIAN_POINT('',(29.775413173324,-2.69370321195777,33.8969505670765));
#61538=CARTESIAN_POINT('Ctrl Pts',(29.7754131733279,-2.6937032119505,33.8969505670841));
#61539=CARTESIAN_POINT('Ctrl Pts',(29.766775132069,-2.70952981970859,33.8804609779984));
#61540=CARTESIAN_POINT('Ctrl Pts',(29.7580309269823,-2.72555094069122,33.8637293696347));
#61541=CARTESIAN_POINT('',(29.8004337692193,-2.6956723755605,33.8969505670765));
#61542=CARTESIAN_POINT('Origin',(29.7874812679387,-2.70030645711978,33.8912949397144));
#61543=CARTESIAN_POINT('',(29.8126199288582,-2.72984718831551,33.8637293696319));
#61544=CARTESIAN_POINT('Ctrl Pts',(29.8126199288571,-2.72984718831264,33.8637293696347));
#61545=CARTESIAN_POINT('Ctrl Pts',(29.8064896349355,-2.7126554188699,33.8804609779983));
#61546=CARTESIAN_POINT('Ctrl Pts',(29.8004337692165,-2.69567237555272,33.8969505670841));
#61547=CARTESIAN_POINT('',(29.9726210990469,-2.73613365141358,33.8637293696319));
#61548=CARTESIAN_POINT('Origin',(30.,-1.32966554433622E-14,33.8637293696319));
#61549=CARTESIAN_POINT('',(29.987451017728,-2.70302030326669,33.8969505670765));
#61550=CARTESIAN_POINT('Ctrl Pts',(29.9874510177314,-2.70302030325915,33.8969505670841));
#61551=CARTESIAN_POINT('Ctrl Pts',(29.980081346004,-2.71947585577343,33.8804609779983));
#61552=CARTESIAN_POINT('Ctrl Pts',(29.9726210990482,-2.73613365141081,33.8637293696347));
#61553=CARTESIAN_POINT('Ctrl Pts',(30.,-2.69489040503949,33.9051095949605));
#61554=CARTESIAN_POINT('Ctrl Pts',(29.9982996971592,-2.69489040503949,33.9051095949605));
#61555=CARTESIAN_POINT('Ctrl Pts',(29.9965490639354,-2.69522714758869,33.9047710768107));
#61556=CARTESIAN_POINT('Ctrl Pts',(29.9934248389279,-2.69644647069985,33.9035459832655));
#61557=CARTESIAN_POINT('Ctrl Pts',(29.9920523583067,-2.69733049287042,33.9026580100842));
#61558=CARTESIAN_POINT('Ctrl Pts',(29.9894391186861,-2.69960157002983,33.9003782103613));
#61559=CARTESIAN_POINT('Ctrl Pts',(29.9882404972758,-2.7012574944688,33.8987170220582));
#61560=CARTESIAN_POINT('Ctrl Pts',(29.987451017728,-2.7030203032667,33.8969505670765));
#61561=CARTESIAN_POINT('',(30.,-2.73627063036813,33.8637293696319));
#61562=CARTESIAN_POINT('Origin',(30.,-1.32966554433622E-14,31.5762293696319));
#61563=CARTESIAN_POINT('',(30.012548982272,2.70302030326666,31.5905494329235));
#61564=CARTESIAN_POINT('',(30.,2.69489040503946,31.5823904050395));
#61565=CARTESIAN_POINT('Ctrl Pts',(30.012548982272,2.70302030326668,31.5905494329235));
#61566=CARTESIAN_POINT('Ctrl Pts',(30.0117595027242,2.70125749446877,31.5887829779419));
#61567=CARTESIAN_POINT('Ctrl Pts',(30.0105608813139,2.6996015700298,31.5871217896387));
#61568=CARTESIAN_POINT('Ctrl Pts',(30.0079476416933,2.69733049287039,31.5848419899159));
#61569=CARTESIAN_POINT('Ctrl Pts',(30.0065751610721,2.69644647069982,31.5839540167345));
#61570=CARTESIAN_POINT('Ctrl Pts',(30.0034509360646,2.69522714758867,31.5827289231894));
#61571=CARTESIAN_POINT('Ctrl Pts',(30.0017003028408,2.69489040503946,31.5823904050395));
#61572=CARTESIAN_POINT('Ctrl Pts',(30.,2.69489040503946,31.5823904050395));
#61573=CARTESIAN_POINT('',(30.0273789009535,2.73613365141461,31.6237706303691));
#61574=CARTESIAN_POINT('Ctrl Pts',(30.0273789009505,2.73613365140797,31.6237706303625));
#61575=CARTESIAN_POINT('Ctrl Pts',(30.0199186539932,2.71947585576695,31.6070390219952));
#61576=CARTESIAN_POINT('Ctrl Pts',(30.0125489822642,2.70302030324912,31.5905494329059));
#61577=CARTESIAN_POINT('',(30.1873800711414,2.72984718831658,31.6237706303691));
#61578=CARTESIAN_POINT('Origin',(30.,-1.32966554433622E-14,31.6237706303681));
#61579=CARTESIAN_POINT('',(30.1995662307806,2.69567237556048,31.5905494329235));
#61580=CARTESIAN_POINT('Ctrl Pts',(30.1995662307774,2.69567237556935,31.5905494329321));
#61581=CARTESIAN_POINT('Ctrl Pts',(30.1935103650619,2.71265541887687,31.6070390220085));
#61582=CARTESIAN_POINT('Ctrl Pts',(30.1873800711438,2.72984718830972,31.6237706303625));
#61583=CARTESIAN_POINT('',(30.224586826676,2.69370321195774,31.5905494329235));
#61584=CARTESIAN_POINT('Origin',(30.2125187883694,2.70030745889013,31.5962062072437));
#61585=CARTESIAN_POINT('',(30.2419690730196,2.72555094069491,31.6237706303691));
#61586=CARTESIAN_POINT('Ctrl Pts',(30.2419690730161,2.72555094068852,31.6237706303625));
#61587=CARTESIAN_POINT('Ctrl Pts',(30.2332248679276,2.70952981970239,31.6070390219952));
#61588=CARTESIAN_POINT('Ctrl Pts',(30.2245868266668,2.69370321194088,31.5905494329059));
#61589=CARTESIAN_POINT('',(30.4009837827875,2.70673030953627,31.6237706303691));
#61590=CARTESIAN_POINT('Origin',(30.,-1.32966554433622E-14,31.6237706303681));
#61591=CARTESIAN_POINT('',(30.410451051658,2.67170473125694,31.5905494329235));
#61592=CARTESIAN_POINT('Ctrl Pts',(30.4104510516555,2.67170473126603,31.5905494329321));
#61593=CARTESIAN_POINT('Ctrl Pts',(30.4057463283736,2.68911055926674,31.6070390220085));
#61594=CARTESIAN_POINT('Ctrl Pts',(30.4009837827894,2.70673030952925,31.6237706303625));
#61595=CARTESIAN_POINT('',(30.4352400186108,2.66777854459989,31.5905494329235));
#61596=CARTESIAN_POINT('Origin',(30.4237273077485,2.6753090233822,31.5962059100614));
#61597=CARTESIAN_POINT('',(30.4550674252877,2.69816430208816,31.6237706303691));
#61598=CARTESIAN_POINT('Ctrl Pts',(30.4550674252837,2.69816430208208,31.6237706303625));
#61599=CARTESIAN_POINT('Ctrl Pts',(30.4450931729961,2.68287863128927,31.6070390219952));
#61600=CARTESIAN_POINT('Ctrl Pts',(30.4352400186003,2.66777854458381,31.5905494329059));
#61601=CARTESIAN_POINT('',(30.6121152960721,2.6669255383185,31.6237706303691));
#61602=CARTESIAN_POINT('Origin',(30.,-1.32966554433622E-14,31.6237706303681));
#61603=CARTESIAN_POINT('',(30.6188053053131,2.63126513885322,31.5905494329235));
#61604=CARTESIAN_POINT('Ctrl Pts',(30.6188053053114,2.63126513886247,31.5905494329321));
#61605=CARTESIAN_POINT('Ctrl Pts',(30.6154807306465,2.64898643883871,31.6070390220085));
#61606=CARTESIAN_POINT('Ctrl Pts',(30.6121152960735,2.66692553831135,31.6237706303626));
#61607=CARTESIAN_POINT('',(30.6432098110989,2.62540613538819,31.5905494329235));
#61608=CARTESIAN_POINT('Origin',(30.6323233823986,2.63381649164648,31.5962056922849));
#61609=CARTESIAN_POINT('',(30.6653601355536,2.65414258332836,31.6237706303691));
#61610=CARTESIAN_POINT('Ctrl Pts',(30.6653601355491,2.65414258332261,31.6237706303625));
#61611=CARTESIAN_POINT('Ctrl Pts',(30.6542173306446,2.63968660396658,31.6070390219952));
#61612=CARTESIAN_POINT('Ctrl Pts',(30.6432098110871,2.62540613537299,31.5905494329059));
#61613=CARTESIAN_POINT('',(30.8194729150074,2.61067828431427,31.6237706303691));
#61614=CARTESIAN_POINT('Origin',(30.,-1.32966554433622E-14,31.6237706303681));
#61615=CARTESIAN_POINT('',(30.8233444184872,2.57460292188402,31.5905494329235));
#61616=CARTESIAN_POINT('Ctrl Pts',(30.8233444184862,2.57460292189339,31.5905494329321));
#61617=CARTESIAN_POINT('Ctrl Pts',(30.8214204895467,2.59253043613788,31.6070390220085));
#61618=CARTESIAN_POINT('Ctrl Pts',(30.8194729150082,2.61067828430704,31.6237706303625));
#61619=CARTESIAN_POINT('',(30.8472140012126,2.5668472243157,31.5905494329235));
#61620=CARTESIAN_POINT('Origin',(30.837020957759,2.57608565616362,31.596205527432));
#61621=CARTESIAN_POINT('',(30.8715506793291,2.59375719295037,31.6237706303691));
#61622=CARTESIAN_POINT('Ctrl Pts',(30.8715506793242,2.59375719294498,31.6237706303625));
#61623=CARTESIAN_POINT('Ctrl Pts',(30.8593080209003,2.58022003094555,31.6070390219952));
#61624=CARTESIAN_POINT('Ctrl Pts',(30.8472140011997,2.56684722430147,31.5905494329059));
#61625=CARTESIAN_POINT('',(31.0217782109193,2.53833533054861,31.6237706303691));
#61626=CARTESIAN_POINT('Origin',(30.,-1.32966554433622E-14,31.6237706303681));
#61627=CARTESIAN_POINT('',(31.0228073395316,2.50206742175906,31.5905494329235));
#61628=CARTESIAN_POINT('Ctrl Pts',(31.0228073395313,2.50206742176848,31.5905494329321));
#61629=CARTESIAN_POINT('Ctrl Pts',(31.022295917979,2.52009062119439,31.6070390220085));
#61630=CARTESIAN_POINT('Ctrl Pts',(31.0217782109195,2.53833533054134,31.6237706303625));
#61631=CARTESIAN_POINT('',(31.0459948352816,2.49246284654197,31.5905494329235));
#61632=CARTESIAN_POINT('Origin',(31.0365580110689,2.5024724328509,31.5962053997573));
#61633=CARTESIAN_POINT('',(31.0723678233466,2.51738042696606,31.6237706303691));
#61634=CARTESIAN_POINT('Ctrl Pts',(31.0723678233413,2.51738042696106,31.6237706303625));
#61635=CARTESIAN_POINT('Ctrl Pts',(31.0591007914584,2.50484554342351,31.6070390219952));
#61636=CARTESIAN_POINT('Ctrl Pts',(31.0459948352676,2.49246284652878,31.5905494329059));
#61637=CARTESIAN_POINT('',(31.2177839043852,2.45034269538797,31.6237706303691));
#61638=CARTESIAN_POINT('Origin',(30.,-1.32966554433622E-14,31.6237706303681));
#61639=CARTESIAN_POINT('',(31.2159643132099,2.41410584395711,31.5905494329235));
#61640=CARTESIAN_POINT('Ctrl Pts',(31.2159643132104,2.41410584396651,31.5905494329321));
#61641=CARTESIAN_POINT('Ctrl Pts',(31.216868552129,2.43211360955606,31.6070390220085));
#61642=CARTESIAN_POINT('Ctrl Pts',(31.2177839043849,2.4503426953807,31.6237706303625));
#61643=CARTESIAN_POINT('',(31.2383267633625,2.40271160649132,31.5905494329235));
#61644=CARTESIAN_POINT('Origin',(31.2297043338602,2.41343066267493,31.5962052993351));
#61645=CARTESIAN_POINT('',(31.2665734631346,2.42548317353555,31.6237706303691));
#61646=CARTESIAN_POINT('Ctrl Pts',(31.266573463129,2.42548317353098,31.6237706303625));
#61647=CARTESIAN_POINT('Ctrl Pts',(31.2523638534503,2.4140278501806,31.6070390219952));
#61648=CARTESIAN_POINT('Ctrl Pts',(31.2383267633475,2.40271160647926,31.5905494329059));
#61649=CARTESIAN_POINT('',(31.4062815551263,2.34724288268863,31.6237706303691));
#61650=CARTESIAN_POINT('Origin',(30.,-1.32966554433622E-14,31.6237706303681));
#61651=CARTESIAN_POINT('',(31.401624462548,2.3112605008555,31.5905494329235));
#61652=CARTESIAN_POINT('Ctrl Pts',(31.4016244625492,2.31126050086484,31.5905494329321));
#61653=CARTESIAN_POINT('Ctrl Pts',(31.4039387870053,2.32914180875499,31.6070390220085));
#61654=CARTESIAN_POINT('Ctrl Pts',(31.4062815551254,2.34724288268141,31.6237706303625));
#61655=CARTESIAN_POINT('',(31.4230239951618,2.29814685040396,31.5905494329235));
#61656=CARTESIAN_POINT('Origin',(31.4152691174526,2.30950931155475,31.5962052196244));
#61657=CARTESIAN_POINT('',(31.452970256344,2.3186320097852,31.6237706303691));
#61658=CARTESIAN_POINT('Ctrl Pts',(31.452970256338,2.31863200978109,31.6237706303625));
#61659=CARTESIAN_POINT('Ctrl Pts',(31.4379056758324,2.30832687249561,31.6070390219952));
#61660=CARTESIAN_POINT('Ctrl Pts',(31.4230239951459,2.2981468503931,31.5905494329059));
#61661=CARTESIAN_POINT('',(31.5861090124439,2.22967153708005,31.6237706303691));
#61662=CARTESIAN_POINT('Origin',(30.,-1.32966554433622E-14,31.6237706303681));
#61663=CARTESIAN_POINT('',(31.5786431309871,2.19416546819402,31.5905494329235));
#61664=CARTESIAN_POINT('Ctrl Pts',(31.578643130989,2.19416546820324,31.5905494329321));
#61665=CARTESIAN_POINT('Ctrl Pts',(31.5823532724027,2.21181007418469,31.6070390220085));
#61666=CARTESIAN_POINT('Ctrl Pts',(31.5861090124425,2.22967153707293,31.6237706303625));
#61667=CARTESIAN_POINT('',(31.5989478108274,2.17941325477248,31.5905494329235));
#61668=CARTESIAN_POINT('Origin',(31.5921082951429,2.19134908471604,31.596205156165));
#61669=CARTESIAN_POINT('',(31.6304090047614,2.19748570867114,31.6237706303691));
#61670=CARTESIAN_POINT('Ctrl Pts',(31.6304090047551,2.19748570866755,31.6237706303626));
#61671=CARTESIAN_POINT('Ctrl Pts',(31.6145823315708,2.18839429204514,31.6070390219952));
#61672=CARTESIAN_POINT('Ctrl Pts',(31.5989478108108,2.17941325476293,31.5905494329059));
#61673=CARTESIAN_POINT('',(31.7561575802651,2.09835352500435,31.6237706303691));
#61674=CARTESIAN_POINT('Origin',(30.,-1.32966554433622E-14,31.6237706303681));
#61675=CARTESIAN_POINT('',(31.7459289395715,2.06354267578706,31.5905494329235));
#61676=CARTESIAN_POINT('Ctrl Pts',(31.7459289395742,2.06354267579611,31.5905494329321));
#61677=CARTESIAN_POINT('Ctrl Pts',(31.7510120236898,2.08084179500558,31.6070390220085));
#61678=CARTESIAN_POINT('Ctrl Pts',(31.7561575802631,2.09835352499738,31.6237706303625));
#61679=CARTESIAN_POINT('',(31.7650135815352,2.04724285169688,31.5905494329235));
#61680=CARTESIAN_POINT('Origin',(31.7591315960216,2.05967847590828,31.5962051058414));
#61681=CARTESIAN_POINT('',(31.7977957394984,2.06279117742498,31.6237706303691));
#61682=CARTESIAN_POINT('Ctrl Pts',(31.7977957394918,2.06279117742187,31.6237706303625));
#61683=CARTESIAN_POINT('Ctrl Pts',(31.781304550332,2.05496953306921,31.6070390219952));
#61684=CARTESIAN_POINT('Ctrl Pts',(31.7650135815179,2.04724285168864,31.5905494329059));
#61685=CARTESIAN_POINT('',(31.9153788526223,1.95409846567364,31.6237706303691));
#61686=CARTESIAN_POINT('Origin',(30.,-1.32966554433622E-14,31.6237706303681));
#61687=CARTESIAN_POINT('',(31.9024505156632,1.9201974565863,31.5905494329235));
#61688=CARTESIAN_POINT('Ctrl Pts',(31.9024505156666,1.92019745659511,31.5905494329321));
#61689=CARTESIAN_POINT('Ctrl Pts',(31.9088752035804,1.93704443421013,31.6070390220085));
#61690=CARTESIAN_POINT('Ctrl Pts',(31.9153788526197,1.95409846566686,31.6237706303625));
#61691=CARTESIAN_POINT('',(31.9201974565863,1.90245051566323,31.5905494329235));
#61692=CARTESIAN_POINT('Origin',(31.9153092670123,1.91530927561703,31.596205066438));
#61693=CARTESIAN_POINT('',(31.9540984656736,1.91537885262231,31.6237706303691));
#61694=CARTESIAN_POINT('Ctrl Pts',(31.9540984656668,1.9153788526197,31.6237706303625));
#61695=CARTESIAN_POINT('Ctrl Pts',(31.9370444341966,1.90887520357521,31.6070390219952));
#61696=CARTESIAN_POINT('Ctrl Pts',(31.9201974565683,1.90245051565638,31.5905494329059));
#61697=CARTESIAN_POINT('',(32.062791177425,1.79779573949838,31.6237706303691));
#61698=CARTESIAN_POINT('Origin',(30.,-1.32966554433622E-14,31.6237706303681));
#61699=CARTESIAN_POINT('',(32.0472428516969,1.76501358153524,31.5905494329235));
#61700=CARTESIAN_POINT('Ctrl Pts',(32.0472428517009,1.76501358154374,31.5905494329321));
#61701=CARTESIAN_POINT('Ctrl Pts',(32.0549695330754,1.78130455034511,31.6070390220085));
#61702=CARTESIAN_POINT('Ctrl Pts',(32.0627911774219,1.7977957394918,31.6237706303625));
#61703=CARTESIAN_POINT('',(32.0635426757871,1.74592893957153,31.5905494329235));
#61704=CARTESIAN_POINT('Origin',(32.059678421746,1.75913156587022,31.5962050363748));
#61705=CARTESIAN_POINT('',(32.0983535250043,1.75615758026513,31.6237706303691));
#61706=CARTESIAN_POINT('Ctrl Pts',(32.0983535249974,1.75615758026307,31.6237706303625));
#61707=CARTESIAN_POINT('Ctrl Pts',(32.0808417949917,1.75101202368577,31.6070390219952));
#61708=CARTESIAN_POINT('Ctrl Pts',(32.0635426757687,1.74592893956612,31.5905494329059));
#61709=CARTESIAN_POINT('',(32.1974857086711,1.63040900476136,31.6237706303691));
#61710=CARTESIAN_POINT('Origin',(30.,-1.32966554433622E-14,31.6237706303681));
#61711=CARTESIAN_POINT('',(32.1794132547725,1.59894781082743,31.5905494329235));
#61712=CARTESIAN_POINT('Ctrl Pts',(32.1794132547772,1.59894781083559,31.5905494329321));
#61713=CARTESIAN_POINT('Ctrl Pts',(32.1883942920524,1.61458233158336,31.6070390220085));
#61714=CARTESIAN_POINT('Ctrl Pts',(32.1974857086675,1.63040900475503,31.6237706303625));
#61715=CARTESIAN_POINT('',(32.194165468194,1.57864313098709,31.5905494329235));
#61716=CARTESIAN_POINT('Origin',(32.1913489771416,1.59210823242537,31.5962050145327));
#61717=CARTESIAN_POINT('',(32.22967153708,1.58610901244395,31.6237706303691));
#61718=CARTESIAN_POINT('Ctrl Pts',(32.2296715370729,1.58610901244245,31.6237706303625));
#61719=CARTESIAN_POINT('Ctrl Pts',(32.2118100741705,1.58235327239971,31.6070390219952));
#61720=CARTESIAN_POINT('Ctrl Pts',(32.1941654681752,1.57864313098313,31.5905494329059));
#61721=CARTESIAN_POINT('',(32.3186320097852,1.45297025634397,31.6237706303691));
#61722=CARTESIAN_POINT('Origin',(30.,-1.32966554433622E-14,31.6237706303681));
#61723=CARTESIAN_POINT('',(32.298146850404,1.42302399516178,31.5905494329235));
#61724=CARTESIAN_POINT('Ctrl Pts',(32.2981468504093,1.42302399516954,31.5905494329321));
#61725=CARTESIAN_POINT('Ctrl Pts',(32.3083268725038,1.43790567584429,31.6070390220085));
#61726=CARTESIAN_POINT('Ctrl Pts',(32.3186320097811,1.45297025633794,31.6237706303625));
#61727=CARTESIAN_POINT('',(32.3112605008555,1.401624462548,31.5905494329235));
#61728=CARTESIAN_POINT('Origin',(32.3095091411128,1.41526902814876,31.596205000146));
#61729=CARTESIAN_POINT('',(32.3472428826886,1.40628155512629,31.6237706303691));
#61730=CARTESIAN_POINT('Ctrl Pts',(32.3472428826814,1.40628155512536,31.6237706303625));
#61731=CARTESIAN_POINT('Ctrl Pts',(32.3291418087406,1.40393878700346,31.6070390219952));
#61732=CARTESIAN_POINT('Ctrl Pts',(32.3112605008365,1.40162446254554,31.5905494329059));
#61733=CARTESIAN_POINT('',(32.4254831735355,1.26657346313459,31.6237706303691));
#61734=CARTESIAN_POINT('Origin',(30.,-1.32966554433622E-14,31.6237706303681));
#61735=CARTESIAN_POINT('',(32.4027116064913,1.23832676336245,31.5905494329235));
#61736=CARTESIAN_POINT('Ctrl Pts',(32.4027116064972,1.23832676336979,31.5905494329321));
#61737=CARTESIAN_POINT('Ctrl Pts',(32.4140278501897,1.2523638534615,31.6070390220085));
#61738=CARTESIAN_POINT('Ctrl Pts',(32.425483173531,1.26657346312893,31.6237706303625));
#61739=CARTESIAN_POINT('',(32.4141058439571,1.21596431320987,31.5905494329235));
#61740=CARTESIAN_POINT('Origin',(32.4134304175703,1.22970422416531,31.5962049927334));
#61741=CARTESIAN_POINT('',(32.450342695388,1.21778390438521,31.6237706303691));
#61742=CARTESIAN_POINT('Ctrl Pts',(32.4503426953807,1.21778390438485,31.6237706303625));
#61743=CARTESIAN_POINT('Ctrl Pts',(32.4321136095416,1.2168685521283,31.6070390219952));
#61744=CARTESIAN_POINT('Ctrl Pts',(32.4141058439379,1.21596431320891,31.5905494329059));
#61745=CARTESIAN_POINT('',(32.517380426966,1.07236782334656,31.6237706303691));
#61746=CARTESIAN_POINT('Origin',(30.,-1.32966554433622E-14,31.6237706303681));
#61747=CARTESIAN_POINT('',(32.492462846542,1.04599483528156,31.5905494329235));
#61748=CARTESIAN_POINT('Ctrl Pts',(32.4924628465485,1.04599483528841,31.5905494329321));
#61749=CARTESIAN_POINT('Ctrl Pts',(32.5048455434335,1.05910079146886,31.6070390220085));
#61750=CARTESIAN_POINT('Ctrl Pts',(32.5173804269611,1.07236782334125,31.6237706303625));
#61751=CARTESIAN_POINT('',(32.5020674217591,1.02280733953163,31.5905494329235));
#61752=CARTESIAN_POINT('Origin',(32.5024720978725,1.03655788791103,31.5962049920587));
#61753=CARTESIAN_POINT('',(32.5383353305486,1.02177821091935,31.6237706303691));
#61754=CARTESIAN_POINT('Ctrl Pts',(32.5383353305413,1.02177821091956,31.6237706303625));
#61755=CARTESIAN_POINT('Ctrl Pts',(32.5200906211799,1.02229591797942,31.6070390219952));
#61756=CARTESIAN_POINT('Ctrl Pts',(32.5020674217399,1.02280733953218,31.5905494329059));
#61757=CARTESIAN_POINT('',(32.5937571929504,0.87155067932912,31.6237706303691));
#61758=CARTESIAN_POINT('Origin',(30.,-1.32966554433622E-14,31.6237706303681));
#61759=CARTESIAN_POINT('',(32.5668472243157,0.84721400121258,31.5905494329235));
#61760=CARTESIAN_POINT('Ctrl Pts',(32.5668472243227,0.847214001218895,31.5905494329321));
#61761=CARTESIAN_POINT('Ctrl Pts',(32.5802200309563,0.859308020910075,31.6070390220085));
#61762=CARTESIAN_POINT('Ctrl Pts',(32.593757192945,0.871550679324244,31.6237706303625));
#61763=CARTESIAN_POINT('',(32.574602921884,0.823344418487232,31.5905494329235));
#61764=CARTESIAN_POINT('Origin',(32.5760852110325,0.837020829522203,31.5962049981138));
#61765=CARTESIAN_POINT('',(32.6106782843143,0.819472915007436,31.6237706303691));
#61766=CARTESIAN_POINT('Ctrl Pts',(32.6106782843071,0.819472915008212,31.6237706303625));
#61767=CARTESIAN_POINT('Ctrl Pts',(32.5925304361235,0.8214204895483,31.6070390219952));
#61768=CARTESIAN_POINT('Ctrl Pts',(32.5746029218649,0.823344418489286,31.5905494329059));
#61769=CARTESIAN_POINT('',(32.6541425833284,0.665360135553601,31.6237706303691));
#61770=CARTESIAN_POINT('Origin',(30.,-1.32966554433622E-14,31.6237706303681));
#61771=CARTESIAN_POINT('',(32.6254061353882,0.64320981109888,31.5905494329235));
#61772=CARTESIAN_POINT('Ctrl Pts',(32.6254061353957,0.643209811104633,31.5905494329321));
#61773=CARTESIAN_POINT('Ctrl Pts',(32.639686603978,0.654217330653466,31.6070390220085));
#61774=CARTESIAN_POINT('Ctrl Pts',(32.6541425833226,0.665360135549173,31.6237706303625));
#61775=CARTESIAN_POINT('',(32.6312651388532,0.618805305313054,31.5905494329235));
#61776=CARTESIAN_POINT('Origin',(32.633815908334,0.632323260043002,31.5962050111235));
#61777=CARTESIAN_POINT('',(32.6669255383185,0.612115296072106,31.6237706303691));
#61778=CARTESIAN_POINT('Ctrl Pts',(32.6669255383114,0.61211529607344,31.6237706303625));
#61779=CARTESIAN_POINT('Ctrl Pts',(32.6489864388245,0.61548073064908,31.6070390219952));
#61780=CARTESIAN_POINT('Ctrl Pts',(32.6312651388343,0.618805305316593,31.5905494329059));
#61781=CARTESIAN_POINT('',(32.6981643020882,0.455067425287697,31.6237706303691));
#61782=CARTESIAN_POINT('Origin',(30.,-1.32966554433622E-14,31.6237706303681));
#61783=CARTESIAN_POINT('',(32.6677785445999,0.435240018610789,31.5905494329235));
#61784=CARTESIAN_POINT('Ctrl Pts',(32.6677785446078,0.435240018615936,31.5905494329321));
#61785=CARTESIAN_POINT('Ctrl Pts',(32.6828786313014,0.44509317300403,31.6070390220085));
#61786=CARTESIAN_POINT('Ctrl Pts',(32.6981643020821,0.455067425283731,31.6237706303625));
#61787=CARTESIAN_POINT('',(32.6717047312569,0.410451051657977,31.5905494329235));
#61788=CARTESIAN_POINT('Origin',(32.6753082614925,0.423727206709275,31.596205031575));
#61789=CARTESIAN_POINT('',(32.7067303095363,0.400983782787501,31.6237706303691));
#61790=CARTESIAN_POINT('Ctrl Pts',(32.7067303095293,0.400983782789396,31.6237706303625));
#61791=CARTESIAN_POINT('Ctrl Pts',(32.6891105592528,0.405746328377311,31.6070390219952));
#61792=CARTESIAN_POINT('Ctrl Pts',(32.6717047312384,0.410451051662997,31.5905494329059));
#61793=CARTESIAN_POINT('',(32.7255509406949,0.24196907301962,31.6237706303691));
#61794=CARTESIAN_POINT('Origin',(30.,-1.32966554433622E-14,31.6237706303681));
#61795=CARTESIAN_POINT('',(32.6937032119577,0.224586826675969,31.5905494329235));
#61796=CARTESIAN_POINT('Ctrl Pts',(32.693703211966,0.224586826680493,31.5905494329321));
#61797=CARTESIAN_POINT('Ctrl Pts',(32.7095298197151,0.233224867934539,31.6070390220085));
#61798=CARTESIAN_POINT('Ctrl Pts',(32.7255509406885,0.241969073016156,31.6237706303625));
#61799=CARTESIAN_POINT('',(32.6956723755605,0.199566230780603,31.5905494329235));
#61800=CARTESIAN_POINT('Origin',(32.7003064571198,0.212518732061222,31.5962050602857));
#61801=CARTESIAN_POINT('',(32.7298471883166,0.187380071141372,31.6237706303691));
#61802=CARTESIAN_POINT('Ctrl Pts',(32.7298471883097,0.187380071143799,31.6237706303625));
#61803=CARTESIAN_POINT('Ctrl Pts',(32.7126554188632,0.193510365066728,31.6070390219952));
#61804=CARTESIAN_POINT('Ctrl Pts',(32.6956723755424,0.199566230787043,31.5905494329059));
#61805=CARTESIAN_POINT('',(32.7361336514146,0.0273789009534945,31.6237706303691));
#61806=CARTESIAN_POINT('Origin',(30.,-1.32966554433622E-14,31.6237706303681));
#61807=CARTESIAN_POINT('',(32.7030203032667,0.0125489822719939,31.5905494329235));
#61808=CARTESIAN_POINT('Ctrl Pts',(32.7030203032753,0.0125489822758371,
31.5905494329321));
#61809=CARTESIAN_POINT('Ctrl Pts',(32.7194758557802,0.0199186539990537,
31.6070390220085));
#61810=CARTESIAN_POINT('Ctrl Pts',(32.736133651408,0.0273789009505039,31.6237706303625));
#61811=CARTESIAN_POINT('',(32.7030203032667,-0.0125489822720396,31.5905494329235));
#61812=CARTESIAN_POINT('Origin',(32.7086563646858,6.24424376688964E-9,31.5962050859813));
#61813=CARTESIAN_POINT('',(32.7361336514146,-0.02737890095354,31.6237706303691));
#61814=CARTESIAN_POINT('Ctrl Pts',(32.736133651408,-0.0273789009505768,
31.6237706303625));
#61815=CARTESIAN_POINT('Ctrl Pts',(32.719475855767,-0.0199186539932038,
31.6070390219952));
#61816=CARTESIAN_POINT('Ctrl Pts',(32.7030203032491,-0.0125489822642076,
31.5905494329059));
#61817=CARTESIAN_POINT('',(32.7298471883166,-0.187380071141418,31.6237706303691));
#61818=CARTESIAN_POINT('Origin',(30.,-1.32966554433622E-14,31.6237706303681));
#61819=CARTESIAN_POINT('',(32.6956723755605,-0.199566230780649,31.5905494329235));
#61820=CARTESIAN_POINT('Ctrl Pts',(32.6956723755694,-0.199566230777489,
31.5905494329321));
#61821=CARTESIAN_POINT('Ctrl Pts',(32.7126554188769,-0.193510365061924,
31.6070390220085));
#61822=CARTESIAN_POINT('Ctrl Pts',(32.7298471883097,-0.187380071143864,
31.6237706303625));
#61823=CARTESIAN_POINT('',(32.6937032119577,-0.224586826676015,31.5905494329235));
#61824=CARTESIAN_POINT('Origin',(32.7003074588902,-0.212518788369472,31.5962062072437));
#61825=CARTESIAN_POINT('',(32.7255509406949,-0.241969073019665,31.6237706303691));
#61826=CARTESIAN_POINT('Ctrl Pts',(32.7255509406885,-0.241969073016199,
31.6237706303625));
#61827=CARTESIAN_POINT('Ctrl Pts',(32.7095298197024,-0.23322486792764,31.6070390219952));
#61828=CARTESIAN_POINT('Ctrl Pts',(32.6937032119408,-0.22458682666682,31.5905494329059));
#61829=CARTESIAN_POINT('',(32.7067303095363,-0.400983782787547,31.6237706303691));
#61830=CARTESIAN_POINT('Origin',(30.,-1.32966554433622E-14,31.6237706303681));
#61831=CARTESIAN_POINT('',(32.6717047312569,-0.410451051658023,31.5905494329235));
#61832=CARTESIAN_POINT('Ctrl Pts',(32.671704731266,-0.41045105165556,31.5905494329321));
#61833=CARTESIAN_POINT('Ctrl Pts',(32.6891105592667,-0.405746328373564,
31.6070390220085));
#61834=CARTESIAN_POINT('Ctrl Pts',(32.7067303095293,-0.40098378278943,31.6237706303625));
#61835=CARTESIAN_POINT('',(32.6677785445999,-0.435240018610835,31.5905494329235));
#61836=CARTESIAN_POINT('Origin',(32.6753090233822,-0.42372730774851,31.5962059100614));
#61837=CARTESIAN_POINT('',(32.6981643020882,-0.455067425287743,31.6237706303691));
#61838=CARTESIAN_POINT('Ctrl Pts',(32.6981643020821,-0.455067425283808,
31.6237706303625));
#61839=CARTESIAN_POINT('Ctrl Pts',(32.6828786312893,-0.445093172996188,
31.6070390219952));
#61840=CARTESIAN_POINT('Ctrl Pts',(32.6677785445838,-0.435240018600367,
31.5905494329059));
#61841=CARTESIAN_POINT('',(32.6669255383185,-0.612115296072152,31.6237706303691));
#61842=CARTESIAN_POINT('Origin',(30.,-1.32966554433622E-14,31.6237706303681));
#61843=CARTESIAN_POINT('',(32.6312651388532,-0.6188053053131,31.5905494329235));
#61844=CARTESIAN_POINT('Ctrl Pts',(32.6312651388625,-0.618805305311361,
31.5905494329321));
#61845=CARTESIAN_POINT('Ctrl Pts',(32.6489864388387,-0.615480730646455,
31.6070390220085));
#61846=CARTESIAN_POINT('Ctrl Pts',(32.6669255383114,-0.612115296073488,
31.6237706303625));
#61847=CARTESIAN_POINT('',(32.6254061353882,-0.643209811098926,31.5905494329235));
#61848=CARTESIAN_POINT('Origin',(32.6338164916465,-0.632323382398633,31.5962056922849));
#61849=CARTESIAN_POINT('',(32.6541425833284,-0.665360135553646,31.6237706303691));
#61850=CARTESIAN_POINT('Ctrl Pts',(32.6541425833226,-0.665360135549238,
31.6237706303625));
#61851=CARTESIAN_POINT('Ctrl Pts',(32.6396866039666,-0.654217330644686,
31.6070390219952));
#61852=CARTESIAN_POINT('Ctrl Pts',(32.625406135373,-0.643209811087222,31.5905494329059));
#61853=CARTESIAN_POINT('',(32.6106782843143,-0.819472915007481,31.6237706303691));
#61854=CARTESIAN_POINT('Origin',(30.,-1.32966554433622E-14,31.6237706303681));
#61855=CARTESIAN_POINT('',(32.574602921884,-0.823344418487278,31.5905494329235));
#61856=CARTESIAN_POINT('Ctrl Pts',(32.5746029218934,-0.823344418486272,
31.5905494329321));
#61857=CARTESIAN_POINT('Ctrl Pts',(32.5925304361379,-0.821420489546795,
31.6070390220085));
#61858=CARTESIAN_POINT('Ctrl Pts',(32.610678284307,-0.819472915008254,31.6237706303626));
#61859=CARTESIAN_POINT('',(32.5668472243157,-0.847214001212625,31.5905494329235));
#61860=CARTESIAN_POINT('Origin',(32.5760856561636,-0.837020957759021,31.596205527432));
#61861=CARTESIAN_POINT('',(32.5937571929504,-0.871550679329165,31.6237706303691));
#61862=CARTESIAN_POINT('Ctrl Pts',(32.593757192945,-0.871550679324299,31.6237706303625));
#61863=CARTESIAN_POINT('Ctrl Pts',(32.5802200309455,-0.859308020900409,
31.6070390219952));
#61864=CARTESIAN_POINT('Ctrl Pts',(32.5668472243014,-0.847214001199744,
31.5905494329059));
#61865=CARTESIAN_POINT('',(32.5383353305486,-1.02177821091939,31.6237706303691));
#61866=CARTESIAN_POINT('Origin',(30.,-1.32966554433622E-14,31.6237706303681));
#61867=CARTESIAN_POINT('',(32.5020674217591,-1.02280733953168,31.5905494329235));
#61868=CARTESIAN_POINT('Ctrl Pts',(32.5020674217685,-1.02280733953141,31.5905494329321));
#61869=CARTESIAN_POINT('Ctrl Pts',(32.5200906211944,-1.02229591797905,31.6070390220085));
#61870=CARTESIAN_POINT('Ctrl Pts',(32.5383353305413,-1.0217782109196,31.6237706303625));
#61871=CARTESIAN_POINT('',(32.492462846542,-1.0459948352816,31.5905494329235));
#61872=CARTESIAN_POINT('Origin',(32.5024724328509,-1.03655801106895,31.5962053997573));
#61873=CARTESIAN_POINT('',(32.517380426966,-1.07236782334661,31.6237706303691));
#61874=CARTESIAN_POINT('Ctrl Pts',(32.517380426961,-1.07236782334134,31.6237706303625));
#61875=CARTESIAN_POINT('Ctrl Pts',(32.5048455434235,-1.0591007914584,31.6070390219952));
#61876=CARTESIAN_POINT('Ctrl Pts',(32.4924628465288,-1.04599483526767,31.5905494329059));
#61877=CARTESIAN_POINT('',(32.450342695388,-1.21778390438525,31.6237706303691));
#61878=CARTESIAN_POINT('Origin',(30.,-1.32966554433622E-14,31.6237706303681));
#61879=CARTESIAN_POINT('',(32.4141058439571,-1.21596431320991,31.5905494329235));
#61880=CARTESIAN_POINT('Ctrl Pts',(32.4141058439665,-1.21596431321038,31.5905494329321));
#61881=CARTESIAN_POINT('Ctrl Pts',(32.4321136095561,-1.21686855212907,31.6070390220085));
#61882=CARTESIAN_POINT('Ctrl Pts',(32.4503426953807,-1.21778390438489,31.6237706303625));
#61883=CARTESIAN_POINT('',(32.4027116064913,-1.2383267633625,31.5905494329235));
#61884=CARTESIAN_POINT('Origin',(32.4134306626749,-1.2297043338603,31.5962052993351));
#61885=CARTESIAN_POINT('',(32.4254831735355,-1.26657346313463,31.6237706303691));
#61886=CARTESIAN_POINT('Ctrl Pts',(32.425483173531,-1.26657346312898,31.6237706303625));
#61887=CARTESIAN_POINT('Ctrl Pts',(32.4140278501806,-1.25236385345028,31.6070390219952));
#61888=CARTESIAN_POINT('Ctrl Pts',(32.4027116064792,-1.23832676334755,31.5905494329059));
#61889=CARTESIAN_POINT('',(32.3472428826886,-1.40628155512633,31.6237706303691));
#61890=CARTESIAN_POINT('Origin',(30.,-1.32966554433622E-14,31.6237706303681));
#61891=CARTESIAN_POINT('',(32.3112605008555,-1.40162446254804,31.5905494329235));
#61892=CARTESIAN_POINT('Ctrl Pts',(32.3112605008648,-1.40162446254925,31.5905494329321));
#61893=CARTESIAN_POINT('Ctrl Pts',(32.329141808755,-1.40393878700536,31.6070390220085));
#61894=CARTESIAN_POINT('Ctrl Pts',(32.3472428826814,-1.4062815551254,31.6237706303625));
#61895=CARTESIAN_POINT('',(32.2981468504039,-1.42302399516182,31.5905494329235));
#61896=CARTESIAN_POINT('Origin',(32.3095093115547,-1.41526911745265,31.5962052196244));
#61897=CARTESIAN_POINT('',(32.3186320097852,-1.45297025634402,31.6237706303691));
#61898=CARTESIAN_POINT('Ctrl Pts',(32.3186320097811,-1.45297025633802,31.6237706303625));
#61899=CARTESIAN_POINT('Ctrl Pts',(32.3083268724956,-1.43790567583238,31.6070390219952));
#61900=CARTESIAN_POINT('Ctrl Pts',(32.2981468503931,-1.42302399514595,31.5905494329059));
#61901=CARTESIAN_POINT('',(32.22967153708,-1.58610901244399,31.6237706303691));
#61902=CARTESIAN_POINT('Origin',(30.,-1.32966554433622E-14,31.6237706303681));
#61903=CARTESIAN_POINT('',(32.194165468194,-1.57864313098713,31.5905494329235));
#61904=CARTESIAN_POINT('Ctrl Pts',(32.1941654682032,-1.57864313098907,31.5905494329321));
#61905=CARTESIAN_POINT('Ctrl Pts',(32.2118100741847,-1.58235327240274,31.6070390220085));
#61906=CARTESIAN_POINT('Ctrl Pts',(32.2296715370729,-1.58610901244249,31.6237706303625));
#61907=CARTESIAN_POINT('',(32.1794132547725,-1.59894781082747,31.5905494329235));
#61908=CARTESIAN_POINT('Origin',(32.191349084716,-1.59210829514296,31.596205156165));
#61909=CARTESIAN_POINT('',(32.1974857086711,-1.6304090047614,31.6237706303691));
#61910=CARTESIAN_POINT('Ctrl Pts',(32.1974857086675,-1.63040900475512,31.6237706303625));
#61911=CARTESIAN_POINT('Ctrl Pts',(32.1883942920451,-1.61458233157088,31.6070390219952));
#61912=CARTESIAN_POINT('Ctrl Pts',(32.1794132547629,-1.59894781081085,31.5905494329059));
#61913=CARTESIAN_POINT('',(32.0983535250043,-1.75615758026517,31.6237706303691));
#61914=CARTESIAN_POINT('Origin',(30.,-1.32966554433622E-14,31.6237706303681));
#61915=CARTESIAN_POINT('',(32.063542675787,-1.74592893957158,31.5905494329235));
#61916=CARTESIAN_POINT('Ctrl Pts',(32.0635426757961,-1.74592893957424,31.5905494329321));
#61917=CARTESIAN_POINT('Ctrl Pts',(32.0808417950055,-1.75101202368991,31.6070390220085));
#61918=CARTESIAN_POINT('Ctrl Pts',(32.0983535249973,-1.75615758026313,31.6237706303625));
#61919=CARTESIAN_POINT('',(32.0472428516969,-1.76501358153528,31.5905494329235));
#61920=CARTESIAN_POINT('Origin',(32.0596784759083,-1.75913159602171,31.5962051058414));
#61921=CARTESIAN_POINT('',(32.062791177425,-1.79779573949842,31.6237706303691));
#61922=CARTESIAN_POINT('Ctrl Pts',(32.0627911774219,-1.79779573949184,31.6237706303625));
#61923=CARTESIAN_POINT('Ctrl Pts',(32.0549695330692,-1.78130455033205,31.6070390219952));
#61924=CARTESIAN_POINT('Ctrl Pts',(32.0472428516887,-1.76501358151791,31.5905494329059));
#61925=CARTESIAN_POINT('',(31.9540984656736,-1.91537885262235,31.6237706303691));
#61926=CARTESIAN_POINT('Origin',(30.,-1.32966554433622E-14,31.6237706303681));
#61927=CARTESIAN_POINT('',(31.9201974565863,-1.90245051566327,31.5905494329235));
#61928=CARTESIAN_POINT('Ctrl Pts',(31.9201974565951,-1.90245051566663,31.5905494329321));
#61929=CARTESIAN_POINT('Ctrl Pts',(31.9370444342101,-1.90887520358042,31.6070390220085));
#61930=CARTESIAN_POINT('Ctrl Pts',(31.9540984656668,-1.91537885261975,31.6237706303625));
#61931=CARTESIAN_POINT('',(31.9024505156632,-1.92019745658634,31.5905494329235));
#61932=CARTESIAN_POINT('Origin',(31.915309275617,-1.91530926701241,31.5962050664381));
#61933=CARTESIAN_POINT('',(31.9153788526223,-1.95409846567368,31.6237706303691));
#61934=CARTESIAN_POINT('Ctrl Pts',(31.9153788526197,-1.9540984656669,31.6237706303625));
#61935=CARTESIAN_POINT('Ctrl Pts',(31.9088752035752,-1.93704443419662,31.6070390219952));
#61936=CARTESIAN_POINT('Ctrl Pts',(31.9024505156564,-1.92019745656839,31.5905494329059));
#61937=CARTESIAN_POINT('',(31.7977957394984,-2.06279117742501,31.6237706303691));
#61938=CARTESIAN_POINT('Origin',(30.,-1.32966554433622E-14,31.6237706303681));
#61939=CARTESIAN_POINT('',(31.7650135815352,-2.04724285169692,31.5905494329235));
#61940=CARTESIAN_POINT('Ctrl Pts',(31.7650135815437,-2.04724285170096,31.5905494329321));
#61941=CARTESIAN_POINT('Ctrl Pts',(31.7813045503451,-2.05496953307547,31.6070390220085));
#61942=CARTESIAN_POINT('Ctrl Pts',(31.7977957394918,-2.06279117742192,31.6237706303625));
#61943=CARTESIAN_POINT('',(31.7459289395715,-2.0635426757871,31.5905494329235));
#61944=CARTESIAN_POINT('Origin',(31.7591315658702,-2.05967842174604,31.5962050363748));
#61945=CARTESIAN_POINT('',(31.7561575802651,-2.09835352500439,31.6237706303691));
#61946=CARTESIAN_POINT('Ctrl Pts',(31.7561575802631,-2.09835352499741,31.6237706303625));
#61947=CARTESIAN_POINT('Ctrl Pts',(31.7510120236858,-2.08084179499169,31.6070390219952));
#61948=CARTESIAN_POINT('Ctrl Pts',(31.7459289395661,-2.06354267576866,31.5905494329059));
#61949=CARTESIAN_POINT('',(31.6304090047613,-2.19748570867118,31.6237706303691));
#61950=CARTESIAN_POINT('Origin',(30.,-1.32966554433622E-14,31.6237706303681));
#61951=CARTESIAN_POINT('',(31.5989478108274,-2.17941325477251,31.5905494329235));
#61952=CARTESIAN_POINT('Ctrl Pts',(31.5989478108356,-2.17941325477721,31.5905494329321));
#61953=CARTESIAN_POINT('Ctrl Pts',(31.6145823315833,-2.18839429205237,31.6070390220085));
#61954=CARTESIAN_POINT('Ctrl Pts',(31.630409004755,-2.19748570866756,31.6237706303625));
#61955=CARTESIAN_POINT('',(31.5786431309871,-2.19416546819406,31.5905494329235));
#61956=CARTESIAN_POINT('Origin',(31.5921082324253,-2.19134897714169,31.5962050145327));
#61957=CARTESIAN_POINT('',(31.5861090124439,-2.22967153708009,31.6237706303691));
#61958=CARTESIAN_POINT('Ctrl Pts',(31.5861090124425,-2.22967153707296,31.6237706303625));
#61959=CARTESIAN_POINT('Ctrl Pts',(31.5823532723997,-2.21181007417054,31.6070390219952));
#61960=CARTESIAN_POINT('Ctrl Pts',(31.5786431309832,-2.19416546817524,31.5905494329059));
#61961=CARTESIAN_POINT('',(31.452970256344,-2.31863200978524,31.6237706303691));
#61962=CARTESIAN_POINT('Origin',(30.,-1.32966554433622E-14,31.6237706303681));
#61963=CARTESIAN_POINT('',(31.4230239951618,-2.29814685040399,31.5905494329235));
#61964=CARTESIAN_POINT('Ctrl Pts',(31.4230239951696,-2.2981468504093,31.5905494329321));
#61965=CARTESIAN_POINT('Ctrl Pts',(31.4379056758443,-2.30832687250383,31.6070390220085));
#61966=CARTESIAN_POINT('Ctrl Pts',(31.452970256338,-2.31863200978113,31.6237706303625));
#61967=CARTESIAN_POINT('',(31.401624462548,-2.31126050085554,31.5905494329235));
#61968=CARTESIAN_POINT('Origin',(31.4152690281487,-2.30950914111279,31.596205000146));
#61969=CARTESIAN_POINT('',(31.4062815551263,-2.34724288268866,31.6237706303691));
#61970=CARTESIAN_POINT('Ctrl Pts',(31.4062815551254,-2.34724288268144,31.6237706303625));
#61971=CARTESIAN_POINT('Ctrl Pts',(31.4039387870035,-2.32914180874065,31.6070390219952));
#61972=CARTESIAN_POINT('Ctrl Pts',(31.4016244625455,-2.31126050083648,31.5905494329059));
#61973=CARTESIAN_POINT('',(31.2665734631346,-2.42548317353559,31.6237706303691));
#61974=CARTESIAN_POINT('Origin',(30.,-1.32966554433622E-14,31.6237706303681));
#61975=CARTESIAN_POINT('',(31.2383267633624,-2.40271160649135,31.5905494329235));
#61976=CARTESIAN_POINT('Ctrl Pts',(31.2383267633697,-2.40271160649727,31.5905494329321));
#61977=CARTESIAN_POINT('Ctrl Pts',(31.2523638534615,-2.41402785018975,31.6070390220085));
#61978=CARTESIAN_POINT('Ctrl Pts',(31.2665734631289,-2.42548317353104,31.6237706303625));
#61979=CARTESIAN_POINT('',(31.2159643132098,-2.41410584395714,31.5905494329235));
#61980=CARTESIAN_POINT('Origin',(31.2297042241653,-2.41343041757036,31.5962049927334));
#61981=CARTESIAN_POINT('',(31.2177839043852,-2.450342695388,31.6237706303691));
#61982=CARTESIAN_POINT('Ctrl Pts',(31.2177839043848,-2.45034269538075,31.6237706303625));
#61983=CARTESIAN_POINT('Ctrl Pts',(31.2168685521282,-2.43211360954164,31.6070390219952));
#61984=CARTESIAN_POINT('Ctrl Pts',(31.2159643132088,-2.41410584393796,31.5905494329059));
#61985=CARTESIAN_POINT('',(31.0723678233465,-2.51738042696609,31.6237706303691));
#61986=CARTESIAN_POINT('Origin',(30.,-1.32966554433622E-14,31.6237706303681));
#61987=CARTESIAN_POINT('',(31.0459948352815,-2.49246284654201,31.5905494329235));
#61988=CARTESIAN_POINT('Ctrl Pts',(31.0459948352884,-2.49246284654849,31.5905494329321));
#61989=CARTESIAN_POINT('Ctrl Pts',(31.0591007914688,-2.5048455434335,31.6070390220085));
#61990=CARTESIAN_POINT('Ctrl Pts',(31.0723678233412,-2.51738042696111,31.6237706303625));
#61991=CARTESIAN_POINT('',(31.0228073395316,-2.5020674217591,31.5905494329235));
#61992=CARTESIAN_POINT('Origin',(31.036557887911,-2.50247209787259,31.5962049920587));
#61993=CARTESIAN_POINT('',(31.0217782109193,-2.53833533054864,31.6237706303691));
#61994=CARTESIAN_POINT('Ctrl Pts',(31.0217782109196,-2.53833533054137,31.6237706303625));
#61995=CARTESIAN_POINT('Ctrl Pts',(31.0222959179794,-2.52009062117993,31.6070390219952));
#61996=CARTESIAN_POINT('Ctrl Pts',(31.0228073395322,-2.50206742173989,31.5905494329059));
#61997=CARTESIAN_POINT('',(30.8715506793291,-2.59375719295041,31.6237706303691));
#61998=CARTESIAN_POINT('Origin',(30.,-1.32966554433622E-14,31.6237706303681));
#61999=CARTESIAN_POINT('',(30.8472140012126,-2.56684722431573,31.5905494329235));
#62000=CARTESIAN_POINT('Ctrl Pts',(30.8472140012189,-2.56684722432271,31.5905494329321));
#62001=CARTESIAN_POINT('Ctrl Pts',(30.8593080209101,-2.58022003095631,31.6070390220085));
#62002=CARTESIAN_POINT('Ctrl Pts',(30.8715506793242,-2.593757192945,31.6237706303625));
#62003=CARTESIAN_POINT('',(30.8233444184872,-2.57460292188405,31.5905494329235));
#62004=CARTESIAN_POINT('Origin',(30.8370208295222,-2.5760852110326,31.5962049981139));
#62005=CARTESIAN_POINT('',(30.8194729150074,-2.6106782843143,31.6237706303691));
#62006=CARTESIAN_POINT('Ctrl Pts',(30.8194729150082,-2.61067828430707,31.6237706303625));
#62007=CARTESIAN_POINT('Ctrl Pts',(30.8214204895483,-2.5925304361235,31.6070390219952));
#62008=CARTESIAN_POINT('Ctrl Pts',(30.8233444184892,-2.57460292186495,31.5905494329059));
#62009=CARTESIAN_POINT('',(30.6653601355536,-2.65414258332839,31.6237706303691));
#62010=CARTESIAN_POINT('Origin',(30.,-1.32966554433622E-14,31.6237706303681));
#62011=CARTESIAN_POINT('',(30.6432098110989,-2.62540613538822,31.5905494329235));
#62012=CARTESIAN_POINT('Ctrl Pts',(30.6432098111046,-2.62540613539568,31.5905494329321));
#62013=CARTESIAN_POINT('Ctrl Pts',(30.6542173306535,-2.63968660397806,31.6070390220085));
#62014=CARTESIAN_POINT('Ctrl Pts',(30.6653601355492,-2.65414258332262,31.6237706303625));
#62015=CARTESIAN_POINT('',(30.618805305313,-2.63126513885325,31.5905494329235));
#62016=CARTESIAN_POINT('Origin',(30.632323260043,-2.63381590833404,31.5962050111235));
#62017=CARTESIAN_POINT('',(30.6121152960721,-2.66692553831853,31.6237706303691));
#62018=CARTESIAN_POINT('Ctrl Pts',(30.6121152960734,-2.66692553831138,31.6237706303625));
#62019=CARTESIAN_POINT('Ctrl Pts',(30.615480730649,-2.6489864388245,31.6070390219952));
#62020=CARTESIAN_POINT('Ctrl Pts',(30.6188053053166,-2.63126513883437,31.5905494329059));
#62021=CARTESIAN_POINT('',(30.4550674252877,-2.69816430208819,31.6237706303691));
#62022=CARTESIAN_POINT('Origin',(30.,-1.32966554433622E-14,31.6237706303681));
#62023=CARTESIAN_POINT('',(30.4352400186108,-2.66777854459992,31.5905494329235));
#62024=CARTESIAN_POINT('Ctrl Pts',(30.435240018616,-2.6677785446078,31.5905494329321));
#62025=CARTESIAN_POINT('Ctrl Pts',(30.445093173004,-2.68287863130142,31.6070390220085));
#62026=CARTESIAN_POINT('Ctrl Pts',(30.4550674252837,-2.69816430208209,31.6237706303625));
#62027=CARTESIAN_POINT('',(30.410451051658,-2.67170473125697,31.5905494329235));
#62028=CARTESIAN_POINT('Origin',(30.4237272067093,-2.67530826149246,31.5962050315749));
#62029=CARTESIAN_POINT('',(30.4009837827875,-2.7067303095363,31.6237706303691));
#62030=CARTESIAN_POINT('Ctrl Pts',(30.4009837827894,-2.70673030952928,31.6237706303625));
#62031=CARTESIAN_POINT('Ctrl Pts',(30.4057463283773,-2.68911055925278,31.6070390219952));
#62032=CARTESIAN_POINT('Ctrl Pts',(30.410451051663,-2.67170473123841,31.5905494329059));
#62033=CARTESIAN_POINT('',(30.2419690730196,-2.72555094069494,31.6237706303691));
#62034=CARTESIAN_POINT('Origin',(30.,-1.32966554433622E-14,31.6237706303681));
#62035=CARTESIAN_POINT('',(30.224586826676,-2.69370321195777,31.5905494329235));
#62036=CARTESIAN_POINT('Ctrl Pts',(30.2245868266805,-2.69370321196604,31.5905494329321));
#62037=CARTESIAN_POINT('Ctrl Pts',(30.2332248679346,-2.70952981971513,31.6070390220085));
#62038=CARTESIAN_POINT('Ctrl Pts',(30.2419690730162,-2.72555094068854,31.6237706303625));
#62039=CARTESIAN_POINT('',(30.1995662307806,-2.69567237556051,31.5905494329235));
#62040=CARTESIAN_POINT('Origin',(30.2125187320612,-2.70030645711985,31.5962050602857));
#62041=CARTESIAN_POINT('',(30.1873800711414,-2.72984718831661,31.6237706303691));
#62042=CARTESIAN_POINT('Ctrl Pts',(30.1873800711438,-2.72984718830975,31.6237706303625));
#62043=CARTESIAN_POINT('Ctrl Pts',(30.1935103650667,-2.71265541886325,31.6070390219952));
#62044=CARTESIAN_POINT('Ctrl Pts',(30.199566230787,-2.6956723755424,31.5905494329059));
#62045=CARTESIAN_POINT('',(30.0273789009535,-2.73613365141464,31.6237706303691));
#62046=CARTESIAN_POINT('Origin',(30.,-1.32966554433622E-14,31.6237706303681));
#62047=CARTESIAN_POINT('',(30.012548982272,-2.70302030326669,31.5905494329235));
#62048=CARTESIAN_POINT('Ctrl Pts',(30.0125489822759,-2.70302030327528,31.5905494329321));
#62049=CARTESIAN_POINT('Ctrl Pts',(30.0199186539991,-2.7194758557802,31.6070390220085));
#62050=CARTESIAN_POINT('Ctrl Pts',(30.0273789009505,-2.736133651408,31.6237706303625));
#62051=CARTESIAN_POINT('',(29.987451017728,-2.70302030326669,31.5905494329235));
#62052=CARTESIAN_POINT('Origin',(30.,-2.7086657795165,31.5962151370754));
#62053=CARTESIAN_POINT('',(29.9726210990465,-2.73613365141464,31.6237706303691));
#62054=CARTESIAN_POINT('Ctrl Pts',(29.9726210990495,-2.73613365140799,31.6237706303625));
#62055=CARTESIAN_POINT('Ctrl Pts',(29.9800813460068,-2.71947585576697,31.6070390219952));
#62056=CARTESIAN_POINT('Ctrl Pts',(29.9874510177359,-2.70302030324915,31.5905494329059));
#62057=CARTESIAN_POINT('',(29.8126199288586,-2.72984718831661,31.6237706303691));
#62058=CARTESIAN_POINT('Origin',(30.,-1.32966554433622E-14,31.6237706303681));
#62059=CARTESIAN_POINT('',(29.8004337692193,-2.6956723755605,31.5905494329235));
#62060=CARTESIAN_POINT('Ctrl Pts',(29.8004337692225,-2.69567237556937,31.5905494329321));
#62061=CARTESIAN_POINT('Ctrl Pts',(29.806489634938,-2.71265541887691,31.6070390220085));
#62062=CARTESIAN_POINT('Ctrl Pts',(29.8126199288561,-2.72984718830976,31.6237706303625));
#62063=CARTESIAN_POINT('',(29.775413173324,-2.69370321195777,31.5905494329235));
#62064=CARTESIAN_POINT('Origin',(29.7874812116305,-2.70030745889015,31.5962062072437));
#62065=CARTESIAN_POINT('',(29.7580309269803,-2.72555094069494,31.6237706303691));
#62066=CARTESIAN_POINT('Ctrl Pts',(29.7580309269838,-2.72555094068855,31.6237706303625));
#62067=CARTESIAN_POINT('Ctrl Pts',(29.7667751320723,-2.7095298197024,31.6070390219952));
#62068=CARTESIAN_POINT('Ctrl Pts',(29.7754131733332,-2.69370321194088,31.5905494329059));
#62069=CARTESIAN_POINT('',(29.5990162172124,-2.70673030953629,31.6237706303691));
#62070=CARTESIAN_POINT('Origin',(30.,-1.32966554433622E-14,31.6237706303681));
#62071=CARTESIAN_POINT('',(29.589548948342,-2.67170473125696,31.5905494329235));
#62072=CARTESIAN_POINT('Ctrl Pts',(29.5895489483445,-2.67170473126605,31.5905494329321));
#62073=CARTESIAN_POINT('Ctrl Pts',(29.5942536716264,-2.68911055926676,31.6070390220085));
#62074=CARTESIAN_POINT('Ctrl Pts',(29.5990162172106,-2.70673030952926,31.6237706303625));
#62075=CARTESIAN_POINT('',(29.5647599813891,-2.66777854459992,31.5905494329235));
#62076=CARTESIAN_POINT('Origin',(29.5762726922515,-2.67530902338218,31.5962059100614));
#62077=CARTESIAN_POINT('',(29.5449325747122,-2.69816430208819,31.6237706303691));
#62078=CARTESIAN_POINT('Ctrl Pts',(29.5449325747162,-2.6981643020821,31.6237706303625));
#62079=CARTESIAN_POINT('Ctrl Pts',(29.5549068270038,-2.68287863128929,31.6070390219952));
#62080=CARTESIAN_POINT('Ctrl Pts',(29.5647599813996,-2.66777854458383,31.5905494329059));
#62081=CARTESIAN_POINT('',(29.3878847039278,-2.66692553831852,31.6237706303691));
#62082=CARTESIAN_POINT('Origin',(30.,-1.32966554433622E-14,31.6237706303681));
#62083=CARTESIAN_POINT('',(29.3811946946869,-2.63126513885324,31.5905494329235));
#62084=CARTESIAN_POINT('Ctrl Pts',(29.3811946946886,-2.63126513886249,31.5905494329321));
#62085=CARTESIAN_POINT('Ctrl Pts',(29.3845192693535,-2.64898643883873,31.6070390220085));
#62086=CARTESIAN_POINT('Ctrl Pts',(29.3878847039265,-2.66692553831137,31.6237706303625));
#62087=CARTESIAN_POINT('',(29.3567901889011,-2.62540613538822,31.5905494329235));
#62088=CARTESIAN_POINT('Origin',(29.3676766176013,-2.63381649164654,31.5962056922849));
#62089=CARTESIAN_POINT('',(29.3346398644463,-2.65414258332839,31.6237706303691));
#62090=CARTESIAN_POINT('Ctrl Pts',(29.3346398644508,-2.65414258332263,31.6237706303626));
#62091=CARTESIAN_POINT('Ctrl Pts',(29.3457826693553,-2.63968660396658,31.6070390219952));
#62092=CARTESIAN_POINT('Ctrl Pts',(29.3567901889128,-2.62540613537299,31.5905494329059));
#62093=CARTESIAN_POINT('',(29.1805270849925,-2.61067828431429,31.6237706303691));
#62094=CARTESIAN_POINT('Origin',(30.,-1.32966554433622E-14,31.6237706303681));
#62095=CARTESIAN_POINT('',(29.1766555815127,-2.57460292188404,31.5905494329235));
#62096=CARTESIAN_POINT('Ctrl Pts',(29.1766555815137,-2.5746029218934,31.5905494329321));
#62097=CARTESIAN_POINT('Ctrl Pts',(29.1785795104532,-2.59253043613788,31.6070390220085));
#62098=CARTESIAN_POINT('Ctrl Pts',(29.1805270849917,-2.61067828430705,31.6237706303625));
#62099=CARTESIAN_POINT('',(29.1527859987874,-2.56684722431572,31.5905494329235));
#62100=CARTESIAN_POINT('Origin',(29.162979042241,-2.57608565616368,31.5962055274321));
#62101=CARTESIAN_POINT('',(29.1284493206708,-2.59375719295039,31.6237706303691));
#62102=CARTESIAN_POINT('Ctrl Pts',(29.1284493206757,-2.593757192945,31.6237706303625));
#62103=CARTESIAN_POINT('Ctrl Pts',(29.1406919790996,-2.58022003094555,31.6070390219952));
#62104=CARTESIAN_POINT('Ctrl Pts',(29.1527859988003,-2.56684722430145,31.5905494329059));
#62105=CARTESIAN_POINT('',(28.9782217890806,-2.53833533054863,31.6237706303691));
#62106=CARTESIAN_POINT('Origin',(30.,-1.32966554433622E-14,31.6237706303681));
#62107=CARTESIAN_POINT('',(28.9771926604683,-2.50206742175908,31.5905494329235));
#62108=CARTESIAN_POINT('Ctrl Pts',(28.9771926604686,-2.50206742176849,31.5905494329321));
#62109=CARTESIAN_POINT('Ctrl Pts',(28.9777040820209,-2.5200906211944,31.6070390220085));
#62110=CARTESIAN_POINT('Ctrl Pts',(28.9782217890804,-2.53833533054136,31.6237706303625));
#62111=CARTESIAN_POINT('',(28.9540051647184,-2.49246284654199,31.5905494329235));
#62112=CARTESIAN_POINT('Origin',(28.963441988931,-2.50247243285095,31.5962053997573));
#62113=CARTESIAN_POINT('',(28.9276321766534,-2.51738042696608,31.6237706303691));
#62114=CARTESIAN_POINT('Ctrl Pts',(28.9276321766587,-2.51738042696105,31.6237706303625));
#62115=CARTESIAN_POINT('Ctrl Pts',(28.9408992085416,-2.5048455434235,31.6070390219952));
#62116=CARTESIAN_POINT('Ctrl Pts',(28.9540051647323,-2.49246284652876,31.5905494329059));
#62117=CARTESIAN_POINT('',(28.7822160956147,-2.45034269538798,31.6237706303691));
#62118=CARTESIAN_POINT('Origin',(30.,-1.32966554433622E-14,31.6237706303681));
#62119=CARTESIAN_POINT('',(28.7840356867901,-2.41410584395713,31.5905494329235));
#62120=CARTESIAN_POINT('Ctrl Pts',(28.7840356867896,-2.41410584396654,31.5905494329321));
#62121=CARTESIAN_POINT('Ctrl Pts',(28.783131447871,-2.43211360955609,31.6070390220085));
#62122=CARTESIAN_POINT('Ctrl Pts',(28.7822160956151,-2.45034269538072,31.6237706303625));
#62123=CARTESIAN_POINT('',(28.7616732366375,-2.40271160649133,31.5905494329235));
#62124=CARTESIAN_POINT('Origin',(28.7702956661397,-2.41343066267495,31.5962052993351));
#62125=CARTESIAN_POINT('',(28.7334265368654,-2.42548317353557,31.6237706303691));
#62126=CARTESIAN_POINT('Ctrl Pts',(28.7334265368711,-2.425483173531,31.6237706303625));
#62127=CARTESIAN_POINT('Ctrl Pts',(28.7476361465498,-2.41402785018062,31.6070390219952));
#62128=CARTESIAN_POINT('Ctrl Pts',(28.7616732366525,-2.40271160647928,31.5905494329059));
#62129=CARTESIAN_POINT('',(28.5937184448736,-2.34724288268865,31.6237706303691));
#62130=CARTESIAN_POINT('Origin',(30.,-1.32966554433622E-14,31.6237706303681));
#62131=CARTESIAN_POINT('',(28.5983755374519,-2.31126050085552,31.5905494329235));
#62132=CARTESIAN_POINT('Ctrl Pts',(28.5983755374507,-2.31126050086484,31.5905494329321));
#62133=CARTESIAN_POINT('Ctrl Pts',(28.5960612129946,-2.32914180875499,31.6070390220085));
#62134=CARTESIAN_POINT('Ctrl Pts',(28.5937184448745,-2.34724288268142,31.6237706303625));
#62135=CARTESIAN_POINT('',(28.5769760048382,-2.29814685040397,31.5905494329235));
#62136=CARTESIAN_POINT('Origin',(28.5847308825473,-2.30950931155478,31.5962052196244));
#62137=CARTESIAN_POINT('',(28.547029743656,-2.31863200978522,31.6237706303691));
#62138=CARTESIAN_POINT('Ctrl Pts',(28.547029743662,-2.31863200978111,31.6237706303625));
#62139=CARTESIAN_POINT('Ctrl Pts',(28.5620943241676,-2.30832687249563,31.6070390219952));
#62140=CARTESIAN_POINT('Ctrl Pts',(28.5769760048541,-2.29814685039312,31.5905494329059));
#62141=CARTESIAN_POINT('',(28.413890987556,-2.22967153708007,31.6237706303691));
#62142=CARTESIAN_POINT('Origin',(30.,-1.32966554433622E-14,31.6237706303681));
#62143=CARTESIAN_POINT('',(28.4213568690129,-2.19416546819403,31.5905494329235));
#62144=CARTESIAN_POINT('Ctrl Pts',(28.421356869011,-2.19416546820326,31.5905494329321));
#62145=CARTESIAN_POINT('Ctrl Pts',(28.4176467275973,-2.21181007418472,31.6070390220085));
#62146=CARTESIAN_POINT('Ctrl Pts',(28.4138909875575,-2.22967153707296,31.6237706303625));
#62147=CARTESIAN_POINT('',(28.4010521891725,-2.17941325477249,31.5905494329235));
#62148=CARTESIAN_POINT('Origin',(28.407891704857,-2.19134908471608,31.596205156165));
#62149=CARTESIAN_POINT('',(28.3695909952386,-2.19748570867116,31.6237706303691));
#62150=CARTESIAN_POINT('Ctrl Pts',(28.3695909952449,-2.19748570866753,31.6237706303625));
#62151=CARTESIAN_POINT('Ctrl Pts',(28.3854176684292,-2.18839429204513,31.6070390219952));
#62152=CARTESIAN_POINT('Ctrl Pts',(28.4010521891892,-2.17941325476292,31.5905494329059));
#62153=CARTESIAN_POINT('',(28.2438424197348,-2.09835352500436,31.6237706303691));
#62154=CARTESIAN_POINT('Origin',(30.,-1.32966554433622E-14,31.6237706303681));
#62155=CARTESIAN_POINT('',(28.2540710604284,-2.06354267578707,31.5905494329235));
#62156=CARTESIAN_POINT('Ctrl Pts',(28.2540710604258,-2.0635426757961,31.5905494329321));
#62157=CARTESIAN_POINT('Ctrl Pts',(28.2489879763101,-2.08084179500557,31.6070390220085));
#62158=CARTESIAN_POINT('Ctrl Pts',(28.2438424197369,-2.09835352499738,31.6237706303625));
#62159=CARTESIAN_POINT('',(28.2349864184647,-2.04724285169689,31.5905494329235));
#62160=CARTESIAN_POINT('Origin',(28.2408684039783,-2.05967847590829,31.5962051058414));
#62161=CARTESIAN_POINT('',(28.2022042605016,-2.06279117742499,31.6237706303691));
#62162=CARTESIAN_POINT('Ctrl Pts',(28.2022042605082,-2.06279117742185,31.6237706303625));
#62163=CARTESIAN_POINT('Ctrl Pts',(28.2186954496679,-2.0549695330692,31.6070390219952));
#62164=CARTESIAN_POINT('Ctrl Pts',(28.2349864184821,-2.04724285168864,31.5905494329059));
#62165=CARTESIAN_POINT('',(28.0846211473776,-1.95409846567366,31.6237706303691));
#62166=CARTESIAN_POINT('Origin',(30.,-1.32966554433622E-14,31.6237706303681));
#62167=CARTESIAN_POINT('',(28.0975494843367,-1.92019745658631,31.5905494329235));
#62168=CARTESIAN_POINT('Ctrl Pts',(28.0975494843333,-1.92019745659509,31.5905494329321));
#62169=CARTESIAN_POINT('Ctrl Pts',(28.0911247964195,-1.93704443421011,31.6070390220085));
#62170=CARTESIAN_POINT('Ctrl Pts',(28.0846211473802,-1.95409846566685,31.6237706303626));
#62171=CARTESIAN_POINT('',(28.0798025434136,-1.90245051566325,31.5905494329235));
#62172=CARTESIAN_POINT('Origin',(28.0846907329876,-1.91530927561707,31.5962050664381));
#62173=CARTESIAN_POINT('',(28.0459015343263,-1.91537885262232,31.6237706303691));
#62174=CARTESIAN_POINT('Ctrl Pts',(28.0459015343331,-1.91537885261973,31.6237706303625));
#62175=CARTESIAN_POINT('Ctrl Pts',(28.0629555658034,-1.90887520357524,31.6070390219952));
#62176=CARTESIAN_POINT('Ctrl Pts',(28.0798025434316,-1.90245051565641,31.5905494329059));
#62177=CARTESIAN_POINT('',(27.937208822575,-1.79779573949839,31.6237706303691));
#62178=CARTESIAN_POINT('Origin',(30.,-1.32966554433622E-14,31.6237706303681));
#62179=CARTESIAN_POINT('',(27.9527571483031,-1.76501358153525,31.5905494329235));
#62180=CARTESIAN_POINT('Ctrl Pts',(27.9527571482991,-1.76501358154376,31.5905494329321));
#62181=CARTESIAN_POINT('Ctrl Pts',(27.9450304669246,-1.78130455034514,31.6070390220085));
#62182=CARTESIAN_POINT('Ctrl Pts',(27.9372088225781,-1.79779573949183,31.6237706303625));
#62183=CARTESIAN_POINT('',(27.9364573242129,-1.74592893957155,31.5905494329235));
#62184=CARTESIAN_POINT('Origin',(27.940321578254,-1.75913156587022,31.5962050363747));
#62185=CARTESIAN_POINT('',(27.9016464749956,-1.75615758026514,31.6237706303691));
#62186=CARTESIAN_POINT('Ctrl Pts',(27.9016464750026,-1.75615758026309,31.6237706303625));
#62187=CARTESIAN_POINT('Ctrl Pts',(27.9191582050083,-1.75101202368579,31.6070390219952));
#62188=CARTESIAN_POINT('Ctrl Pts',(27.9364573242313,-1.74592893956614,31.5905494329059));
#62189=CARTESIAN_POINT('',(27.8025142913288,-1.63040900476137,31.6237706303691));
#62190=CARTESIAN_POINT('Origin',(30.,-1.32966554433622E-14,31.6237706303681));
#62191=CARTESIAN_POINT('',(27.8205867452275,-1.59894781082744,31.5905494329235));
#62192=CARTESIAN_POINT('Ctrl Pts',(27.8205867452228,-1.59894781083561,31.5905494329321));
#62193=CARTESIAN_POINT('Ctrl Pts',(27.8116057079476,-1.61458233158338,31.6070390220085));
#62194=CARTESIAN_POINT('Ctrl Pts',(27.8025142913325,-1.63040900475507,31.6237706303625));
#62195=CARTESIAN_POINT('',(27.8058345318059,-1.5786431309871,31.5905494329235));
#62196=CARTESIAN_POINT('Origin',(27.8086510228583,-1.5921082324254,31.5962050145327));
#62197=CARTESIAN_POINT('',(27.7703284629199,-1.58610901244396,31.6237706303691));
#62198=CARTESIAN_POINT('Ctrl Pts',(27.770328462927,-1.58610901244246,31.6237706303625));
#62199=CARTESIAN_POINT('Ctrl Pts',(27.7881899258294,-1.58235327239973,31.6070390219952));
#62200=CARTESIAN_POINT('Ctrl Pts',(27.8058345318247,-1.57864313098315,31.5905494329059));
#62201=CARTESIAN_POINT('',(27.6813679902147,-1.45297025634398,31.6237706303691));
#62202=CARTESIAN_POINT('Origin',(30.,-1.32966554433622E-14,31.6237706303681));
#62203=CARTESIAN_POINT('',(27.701853149596,-1.42302399516179,31.5905494329235));
#62204=CARTESIAN_POINT('Ctrl Pts',(27.7018531495907,-1.42302399516956,31.5905494329321));
#62205=CARTESIAN_POINT('Ctrl Pts',(27.6916731274962,-1.43790567584432,31.6070390220085));
#62206=CARTESIAN_POINT('Ctrl Pts',(27.6813679902189,-1.45297025633799,31.6237706303626));
#62207=CARTESIAN_POINT('',(27.6887394991444,-1.40162446254801,31.5905494329235));
#62208=CARTESIAN_POINT('Origin',(27.6904908588872,-1.41526902814876,31.596205000146));
#62209=CARTESIAN_POINT('',(27.6527571173113,-1.4062815551263,31.6237706303691));
#62210=CARTESIAN_POINT('Ctrl Pts',(27.6527571173185,-1.40628155512537,31.6237706303626));
#62211=CARTESIAN_POINT('Ctrl Pts',(27.6708581912593,-1.40393878700346,31.6070390219953));
#62212=CARTESIAN_POINT('Ctrl Pts',(27.6887394991635,-1.40162446254554,31.5905494329059));
#62213=CARTESIAN_POINT('',(27.5745168264644,-1.2665734631346,31.6237706303691));
#62214=CARTESIAN_POINT('Origin',(30.,-1.32966554433622E-14,31.6237706303681));
#62215=CARTESIAN_POINT('',(27.5972883935086,-1.23832676336246,31.5905494329235));
#62216=CARTESIAN_POINT('Ctrl Pts',(27.5972883935027,-1.23832676336977,31.5905494329321));
#62217=CARTESIAN_POINT('Ctrl Pts',(27.5859721498102,-1.25236385346148,31.6070390220085));
#62218=CARTESIAN_POINT('Ctrl Pts',(27.574516826469,-1.2665734631289,31.6237706303626));
#62219=CARTESIAN_POINT('',(27.5858941560428,-1.21596431320988,31.5905494329235));
#62220=CARTESIAN_POINT('Origin',(27.5865695824296,-1.22970422416533,31.5962049927334));
#62221=CARTESIAN_POINT('',(27.549657304612,-1.21778390438522,31.6237706303691));
#62222=CARTESIAN_POINT('Ctrl Pts',(27.5496573046193,-1.21778390438485,31.6237706303625));
#62223=CARTESIAN_POINT('Ctrl Pts',(27.5678863904584,-1.2168685521283,31.6070390219952));
#62224=CARTESIAN_POINT('Ctrl Pts',(27.585894156062,-1.21596431320891,31.5905494329059));
#62225=CARTESIAN_POINT('',(27.4826195730339,-1.07236782334657,31.6237706303691));
#62226=CARTESIAN_POINT('Origin',(30.,-1.32966554433622E-14,31.6237706303681));
#62227=CARTESIAN_POINT('',(27.507537153458,-1.04599483528157,31.5905494329235));
#62228=CARTESIAN_POINT('Ctrl Pts',(27.5075371534515,-1.04599483528841,31.5905494329321));
#62229=CARTESIAN_POINT('Ctrl Pts',(27.4951544565665,-1.05910079146888,31.6070390220085));
#62230=CARTESIAN_POINT('Ctrl Pts',(27.4826195730389,-1.07236782334129,31.6237706303626));
#62231=CARTESIAN_POINT('',(27.4979325782409,-1.02280733953164,31.5905494329235));
#62232=CARTESIAN_POINT('Origin',(27.4975279021274,-1.03655788791105,31.5962049920587));
#62233=CARTESIAN_POINT('',(27.4616646694513,-1.02177821091936,31.6237706303691));
#62234=CARTESIAN_POINT('Ctrl Pts',(27.4616646694586,-1.02177821091956,31.6237706303626));
#62235=CARTESIAN_POINT('Ctrl Pts',(27.4799093788201,-1.02229591797942,31.6070390219952));
#62236=CARTESIAN_POINT('Ctrl Pts',(27.4979325782601,-1.02280733953218,31.5905494329059));
#62237=CARTESIAN_POINT('',(27.4062428070496,-0.871550679329129,31.6237706303691));
#62238=CARTESIAN_POINT('Origin',(30.,-1.32966554433622E-14,31.6237706303681));
#62239=CARTESIAN_POINT('',(27.4331527756843,-0.847214001212589,31.5905494329235));
#62240=CARTESIAN_POINT('Ctrl Pts',(27.4331527756773,-0.847214001218912,
31.5905494329321));
#62241=CARTESIAN_POINT('Ctrl Pts',(27.4197799690437,-0.859308020910092,
31.6070390220085));
#62242=CARTESIAN_POINT('Ctrl Pts',(27.406242807055,-0.871550679324261,31.6237706303625));
#62243=CARTESIAN_POINT('',(27.4253970781159,-0.823344418487241,31.5905494329235));
#62244=CARTESIAN_POINT('Origin',(27.4239147889674,-0.837020829522197,31.5962049981138));
#62245=CARTESIAN_POINT('',(27.3893217156857,-0.819472915007445,31.6237706303691));
#62246=CARTESIAN_POINT('Ctrl Pts',(27.3893217156929,-0.819472915008222,
31.6237706303625));
#62247=CARTESIAN_POINT('Ctrl Pts',(27.4074695638765,-0.821420489548307,
31.6070390219952));
#62248=CARTESIAN_POINT('Ctrl Pts',(27.425397078135,-0.823344418489291,31.590549432906));
#62249=CARTESIAN_POINT('',(27.3458574166716,-0.665360135553609,31.6237706303691));
#62250=CARTESIAN_POINT('Origin',(30.,-1.32966554433622E-14,31.6237706303681));
#62251=CARTESIAN_POINT('',(27.3745938646118,-0.643209811098888,31.5905494329235));
#62252=CARTESIAN_POINT('Ctrl Pts',(27.3745938646043,-0.643209811104637,
31.5905494329321));
#62253=CARTESIAN_POINT('Ctrl Pts',(27.3603133960219,-0.65421733065347,31.6070390220085));
#62254=CARTESIAN_POINT('Ctrl Pts',(27.3458574166774,-0.665360135549176,
31.6237706303625));
#62255=CARTESIAN_POINT('',(27.3687348611467,-0.618805305313063,31.5905494329235));
#62256=CARTESIAN_POINT('Origin',(27.3661840916659,-0.632323260043008,31.5962050111235));
#62257=CARTESIAN_POINT('',(27.3330744616815,-0.612115296072114,31.6237706303691));
#62258=CARTESIAN_POINT('Ctrl Pts',(27.3330744616886,-0.612115296073467,
31.6237706303625));
#62259=CARTESIAN_POINT('Ctrl Pts',(27.3510135611755,-0.615480730649101,
31.6070390219952));
#62260=CARTESIAN_POINT('Ctrl Pts',(27.3687348611656,-0.61880530531661,31.590549432906));
#62261=CARTESIAN_POINT('',(27.3018356979118,-0.455067425287704,31.6237706303691));
#62262=CARTESIAN_POINT('Origin',(30.,-1.32966554433622E-14,31.6237706303681));
#62263=CARTESIAN_POINT('',(27.3322214554001,-0.435240018610796,31.5905494329235));
#62264=CARTESIAN_POINT('Ctrl Pts',(27.3322214553922,-0.435240018615941,
31.5905494329321));
#62265=CARTESIAN_POINT('Ctrl Pts',(27.3171213686986,-0.445093173004034,
31.6070390220085));
#62266=CARTESIAN_POINT('Ctrl Pts',(27.3018356979179,-0.455067425283735,
31.6237706303625));
#62267=CARTESIAN_POINT('',(27.328295268743,-0.410451051657984,31.5905494329235));
#62268=CARTESIAN_POINT('Origin',(27.3246917385075,-0.423727206709274,31.5962050315749));
#62269=CARTESIAN_POINT('',(27.2932696904637,-0.400983782787508,31.6237706303691));
#62270=CARTESIAN_POINT('Ctrl Pts',(27.2932696904707,-0.400983782789399,
31.6237706303625));
#62271=CARTESIAN_POINT('Ctrl Pts',(27.3108894407472,-0.405746328377308,
31.6070390219952));
#62272=CARTESIAN_POINT('Ctrl Pts',(27.3282952687616,-0.410451051662988,
31.5905494329059));
#62273=CARTESIAN_POINT('',(27.274449059305,-0.241969073019628,31.6237706303691));
#62274=CARTESIAN_POINT('Origin',(30.,-1.32966554433622E-14,31.6237706303681));
#62275=CARTESIAN_POINT('',(27.3062967880422,-0.224586826675978,31.5905494329235));
#62276=CARTESIAN_POINT('Ctrl Pts',(27.306296788034,-0.224586826680481,31.5905494329321));
#62277=CARTESIAN_POINT('Ctrl Pts',(27.2904701802848,-0.233224867934527,
31.6070390220085));
#62278=CARTESIAN_POINT('Ctrl Pts',(27.2744490593114,-0.241969073016143,
31.6237706303626));
#62279=CARTESIAN_POINT('',(27.3043276244395,-0.199566230780611,31.5905494329235));
#62280=CARTESIAN_POINT('Origin',(27.2996935428802,-0.212518732061225,31.5962050602856));
#62281=CARTESIAN_POINT('',(27.2701528116834,-0.18738007114138,31.6237706303691));
#62282=CARTESIAN_POINT('Ctrl Pts',(27.2701528116903,-0.187380071143839,
31.6237706303625));
#62283=CARTESIAN_POINT('Ctrl Pts',(27.2873445811368,-0.193510365066767,
31.6070390219952));
#62284=CARTESIAN_POINT('Ctrl Pts',(27.3043276244576,-0.199566230787083,
31.5905494329059));
#62285=CARTESIAN_POINT('',(27.2638663485853,-0.027378900953502,31.6237706303691));
#62286=CARTESIAN_POINT('Origin',(30.,-1.32966554433622E-14,31.6237706303681));
#62287=CARTESIAN_POINT('Ctrl Pts',(27.2969796967247,-0.0125489822758455,
31.5905494329321));
#62288=CARTESIAN_POINT('Ctrl Pts',(27.2805241442198,-0.0199186539990725,
31.6070390220085));
#62289=CARTESIAN_POINT('Ctrl Pts',(27.263866348592,-0.0273789009505331,
31.6237706303626));
#62290=CARTESIAN_POINT('',(27.2638663485853,0.0273789009535324,31.6237706303691));
#62291=CARTESIAN_POINT('Ctrl Pts',(27.263866348592,0.0273789009505529,31.6237706303626));
#62292=CARTESIAN_POINT('Ctrl Pts',(27.280524144233,0.0199186539931685,31.6070390219952));
#62293=CARTESIAN_POINT('Ctrl Pts',(27.2969796967508,0.012548982264161,31.5905494329059));
#62294=CARTESIAN_POINT('',(27.2701528116834,0.187380071141411,31.6237706303691));
#62295=CARTESIAN_POINT('Origin',(30.,-1.32966554433622E-14,31.6237706303681));
#62296=CARTESIAN_POINT('Ctrl Pts',(27.3043276244306,0.199566230777481,31.5905494329321));
#62297=CARTESIAN_POINT('Ctrl Pts',(27.2873445811231,0.193510365061917,31.6070390220085));
#62298=CARTESIAN_POINT('Ctrl Pts',(27.2701528116902,0.187380071143857,31.6237706303625));
#62299=CARTESIAN_POINT('',(27.2744490593051,0.241969073019658,31.6237706303691));
#62300=CARTESIAN_POINT('Ctrl Pts',(27.2744490593115,0.241969073016152,31.6237706303625));
#62301=CARTESIAN_POINT('Ctrl Pts',(27.2904701802976,0.233224867927605,31.6070390219952));
#62302=CARTESIAN_POINT('Ctrl Pts',(27.3062967880591,0.224586826666795,31.5905494329059));
#62303=CARTESIAN_POINT('',(27.2932696904637,0.40098378278754,31.6237706303691));
#62304=CARTESIAN_POINT('Origin',(30.,-1.32966554433622E-14,31.6237706303681));
#62305=CARTESIAN_POINT('Ctrl Pts',(27.3282952687339,0.410451051655568,31.5905494329321));
#62306=CARTESIAN_POINT('Ctrl Pts',(27.3108894407332,0.405746328373579,31.6070390220085));
#62307=CARTESIAN_POINT('Ctrl Pts',(27.2932696904707,0.400983782789452,31.6237706303626));
#62308=CARTESIAN_POINT('',(27.3018356979118,0.455067425287736,31.6237706303691));
#62309=CARTESIAN_POINT('Ctrl Pts',(27.3018356979179,0.455067425283746,31.6237706303626));
#62310=CARTESIAN_POINT('Ctrl Pts',(27.3171213687107,0.445093172996126,31.6070390219952));
#62311=CARTESIAN_POINT('Ctrl Pts',(27.3322214554162,0.435240018600305,31.5905494329059));
#62312=CARTESIAN_POINT('',(27.3330744616815,0.612115296072143,31.6237706303691));
#62313=CARTESIAN_POINT('Origin',(30.,-1.32966554433622E-14,31.6237706303681));
#62314=CARTESIAN_POINT('Ctrl Pts',(27.3687348611375,0.618805305311351,31.5905494329321));
#62315=CARTESIAN_POINT('Ctrl Pts',(27.3510135611613,0.615480730646445,31.6070390220085));
#62316=CARTESIAN_POINT('Ctrl Pts',(27.3330744616886,0.612115296073478,31.6237706303625));
#62317=CARTESIAN_POINT('',(27.3458574166716,0.665360135553637,31.6237706303691));
#62318=CARTESIAN_POINT('Ctrl Pts',(27.3458574166774,0.665360135549173,31.6237706303626));
#62319=CARTESIAN_POINT('Ctrl Pts',(27.3603133960334,0.65421733064462,31.6070390219952));
#62320=CARTESIAN_POINT('Ctrl Pts',(27.374593864627,0.643209811087154,31.5905494329059));
#62321=CARTESIAN_POINT('',(27.3893217156857,0.819472915007473,31.6237706303691));
#62322=CARTESIAN_POINT('Origin',(30.,-1.32966554433622E-14,31.6237706303681));
#62323=CARTESIAN_POINT('Ctrl Pts',(27.4253970781066,0.823344418486268,31.5905494329322));
#62324=CARTESIAN_POINT('Ctrl Pts',(27.4074695638621,0.821420489546793,31.6070390220085));
#62325=CARTESIAN_POINT('Ctrl Pts',(27.3893217156929,0.819472915008255,31.6237706303625));
#62326=CARTESIAN_POINT('',(27.4062428070496,0.871550679329156,31.6237706303691));
#62327=CARTESIAN_POINT('Ctrl Pts',(27.406242807055,0.87155067932429,31.6237706303625));
#62328=CARTESIAN_POINT('Ctrl Pts',(27.4197799690545,0.8593080209004,31.6070390219952));
#62329=CARTESIAN_POINT('Ctrl Pts',(27.4331527756986,0.847214001199735,31.5905494329059));
#62330=CARTESIAN_POINT('',(27.4616646694514,1.02177821091938,31.6237706303691));
#62331=CARTESIAN_POINT('Origin',(30.,-1.32966554433622E-14,31.6237706303681));
#62332=CARTESIAN_POINT('Ctrl Pts',(27.4979325782315,1.0228073395314,31.5905494329321));
#62333=CARTESIAN_POINT('Ctrl Pts',(27.4799093788056,1.02229591797904,31.6070390220085));
#62334=CARTESIAN_POINT('Ctrl Pts',(27.4616646694587,1.02177821091959,31.6237706303625));
#62335=CARTESIAN_POINT('',(27.4826195730339,1.0723678233466,31.6237706303691));
#62336=CARTESIAN_POINT('Ctrl Pts',(27.4826195730389,1.0723678233413,31.6237706303626));
#62337=CARTESIAN_POINT('Ctrl Pts',(27.4951544565765,1.05910079145835,31.6070390219952));
#62338=CARTESIAN_POINT('Ctrl Pts',(27.5075371534712,1.04599483526761,31.5905494329059));
#62339=CARTESIAN_POINT('',(27.549657304612,1.21778390438524,31.6237706303691));
#62340=CARTESIAN_POINT('Origin',(30.,-1.32966554433622E-14,31.6237706303681));
#62341=CARTESIAN_POINT('Ctrl Pts',(27.5858941560335,1.21596431321037,31.5905494329321));
#62342=CARTESIAN_POINT('Ctrl Pts',(27.5678863904439,1.21686855212906,31.6070390220085));
#62343=CARTESIAN_POINT('Ctrl Pts',(27.5496573046193,1.21778390438488,31.6237706303626));
#62344=CARTESIAN_POINT('',(27.5745168264644,1.26657346313462,31.6237706303691));
#62345=CARTESIAN_POINT('Ctrl Pts',(27.574516826469,1.26657346312892,31.6237706303626));
#62346=CARTESIAN_POINT('Ctrl Pts',(27.5859721498194,1.25236385345021,31.6070390219952));
#62347=CARTESIAN_POINT('Ctrl Pts',(27.5972883935207,1.23832676334747,31.5905494329059));
#62348=CARTESIAN_POINT('',(27.6527571173114,1.40628155512632,31.6237706303691));
#62349=CARTESIAN_POINT('Origin',(30.,-1.32966554433622E-14,31.6237706303681));
#62350=CARTESIAN_POINT('Ctrl Pts',(27.6887394991352,1.40162446254924,31.5905494329321));
#62351=CARTESIAN_POINT('Ctrl Pts',(27.670858191245,1.40393878700535,31.6070390220085));
#62352=CARTESIAN_POINT('Ctrl Pts',(27.6527571173186,1.40628155512539,31.6237706303625));
#62353=CARTESIAN_POINT('',(27.6813679902148,1.45297025634401,31.6237706303691));
#62354=CARTESIAN_POINT('Ctrl Pts',(27.6813679902189,1.452970256338,31.6237706303625));
#62355=CARTESIAN_POINT('Ctrl Pts',(27.6916731275044,1.43790567583238,31.6070390219952));
#62356=CARTESIAN_POINT('Ctrl Pts',(27.7018531496069,1.42302399514596,31.5905494329059));
#62357=CARTESIAN_POINT('',(27.7703284629199,1.58610901244398,31.6237706303691));
#62358=CARTESIAN_POINT('Origin',(30.,-1.32966554433622E-14,31.6237706303681));
#62359=CARTESIAN_POINT('Ctrl Pts',(27.8058345317968,1.57864313098906,31.5905494329321));
#62360=CARTESIAN_POINT('Ctrl Pts',(27.7881899258153,1.58235327240273,31.6070390220085));
#62361=CARTESIAN_POINT('Ctrl Pts',(27.770328462927,1.58610901244249,31.6237706303626));
#62362=CARTESIAN_POINT('',(27.8025142913288,1.63040900476139,31.6237706303691));
#62363=CARTESIAN_POINT('Ctrl Pts',(27.8025142913324,1.63040900475507,31.6237706303626));
#62364=CARTESIAN_POINT('Ctrl Pts',(27.8116057079549,1.61458233157081,31.6070390219952));
#62365=CARTESIAN_POINT('Ctrl Pts',(27.8205867452371,1.59894781081078,31.5905494329059));
#62366=CARTESIAN_POINT('',(27.9016464749956,1.75615758026516,31.6237706303691));
#62367=CARTESIAN_POINT('Origin',(30.,-1.32966554433622E-14,31.6237706303681));
#62368=CARTESIAN_POINT('Ctrl Pts',(27.9364573242039,1.74592893957422,31.5905494329321));
#62369=CARTESIAN_POINT('Ctrl Pts',(27.9191582049944,1.75101202368989,31.6070390220085));
#62370=CARTESIAN_POINT('Ctrl Pts',(27.9016464750026,1.7561575802631,31.6237706303626));
#62371=CARTESIAN_POINT('',(27.937208822575,1.79779573949841,31.6237706303691));
#62372=CARTESIAN_POINT('Ctrl Pts',(27.9372088225781,1.79779573949182,31.6237706303625));
#62373=CARTESIAN_POINT('Ctrl Pts',(27.9450304669308,1.78130455033204,31.6070390219952));
#62374=CARTESIAN_POINT('Ctrl Pts',(27.9527571483113,1.76501358151789,31.5905494329059));
#62375=CARTESIAN_POINT('',(28.0459015343263,1.91537885262234,31.6237706303691));
#62376=CARTESIAN_POINT('Origin',(30.,-1.32966554433622E-14,31.6237706303681));
#62377=CARTESIAN_POINT('Ctrl Pts',(28.0798025434049,1.90245051566662,31.5905494329321));
#62378=CARTESIAN_POINT('Ctrl Pts',(28.0629555657899,1.90887520358041,31.6070390220085));
#62379=CARTESIAN_POINT('Ctrl Pts',(28.0459015343331,1.91537885261975,31.6237706303626));
#62380=CARTESIAN_POINT('',(28.0846211473777,1.95409846567367,31.6237706303691));
#62381=CARTESIAN_POINT('Ctrl Pts',(28.0846211473803,1.95409846566688,31.6237706303625));
#62382=CARTESIAN_POINT('Ctrl Pts',(28.0911247964248,1.93704443419661,31.6070390219952));
#62383=CARTESIAN_POINT('Ctrl Pts',(28.0975494843436,1.9201974565684,31.5905494329059));
#62384=CARTESIAN_POINT('',(28.2022042605016,2.062791177425,31.6237706303691));
#62385=CARTESIAN_POINT('Origin',(30.,-1.32966554433622E-14,31.6237706303681));
#62386=CARTESIAN_POINT('Ctrl Pts',(28.2349864184563,2.04724285170094,31.5905494329321));
#62387=CARTESIAN_POINT('Ctrl Pts',(28.2186954496549,2.05496953307545,31.6070390220085));
#62388=CARTESIAN_POINT('Ctrl Pts',(28.2022042605082,2.0627911774219,31.6237706303626));
#62389=CARTESIAN_POINT('',(28.2438424197349,2.09835352500437,31.6237706303691));
#62390=CARTESIAN_POINT('Ctrl Pts',(28.2438424197369,2.09835352499738,31.6237706303625));
#62391=CARTESIAN_POINT('Ctrl Pts',(28.2489879763142,2.08084179499167,31.6070390219952));
#62392=CARTESIAN_POINT('Ctrl Pts',(28.2540710604339,2.06354267576863,31.5905494329059));
#62393=CARTESIAN_POINT('',(28.3695909952386,2.19748570867117,31.6237706303691));
#62394=CARTESIAN_POINT('Origin',(30.,-1.32966554433622E-14,31.6237706303681));
#62395=CARTESIAN_POINT('Ctrl Pts',(28.4010521891644,2.17941325477719,31.5905494329321));
#62396=CARTESIAN_POINT('Ctrl Pts',(28.3854176684167,2.18839429205237,31.6070390220085));
#62397=CARTESIAN_POINT('Ctrl Pts',(28.369590995245,2.19748570866756,31.6237706303626));
#62398=CARTESIAN_POINT('',(28.413890987556,2.22967153708007,31.6237706303691));
#62399=CARTESIAN_POINT('Ctrl Pts',(28.4138909875575,2.22967153707294,31.6237706303625));
#62400=CARTESIAN_POINT('Ctrl Pts',(28.4176467276003,2.21181007417053,31.6070390219952));
#62401=CARTESIAN_POINT('Ctrl Pts',(28.4213568690169,2.19416546817523,31.5905494329059));
#62402=CARTESIAN_POINT('',(28.547029743656,2.31863200978522,31.6237706303691));
#62403=CARTESIAN_POINT('Origin',(30.,-1.32966554433622E-14,31.6237706303681));
#62404=CARTESIAN_POINT('Ctrl Pts',(28.5769760048304,2.29814685040929,31.5905494329321));
#62405=CARTESIAN_POINT('Ctrl Pts',(28.5620943241557,2.30832687250382,31.6070390220085));
#62406=CARTESIAN_POINT('Ctrl Pts',(28.547029743662,2.31863200978111,31.6237706303625));
#62407=CARTESIAN_POINT('',(28.5937184448737,2.34724288268865,31.6237706303691));
#62408=CARTESIAN_POINT('Ctrl Pts',(28.5937184448746,2.34724288268143,31.6237706303626));
#62409=CARTESIAN_POINT('Ctrl Pts',(28.5960612129965,2.32914180874063,31.6070390219952));
#62410=CARTESIAN_POINT('Ctrl Pts',(28.5983755374545,2.31126050083645,31.5905494329059));
#62411=CARTESIAN_POINT('',(28.7334265368654,2.42548317353557,31.6237706303691));
#62412=CARTESIAN_POINT('Origin',(30.,-1.32966554433622E-14,31.6237706303681));
#62413=CARTESIAN_POINT('Ctrl Pts',(28.7616732366302,2.40271160649724,31.5905494329321));
#62414=CARTESIAN_POINT('Ctrl Pts',(28.7476361465385,2.4140278501897,31.6070390220085));
#62415=CARTESIAN_POINT('Ctrl Pts',(28.7334265368711,2.42548317353099,31.6237706303625));
#62416=CARTESIAN_POINT('',(28.7822160956148,2.45034269538798,31.6237706303691));
#62417=CARTESIAN_POINT('Ctrl Pts',(28.7822160956151,2.45034269538071,31.6237706303626));
#62418=CARTESIAN_POINT('Ctrl Pts',(28.7831314478717,2.4321136095416,31.6070390219952));
#62419=CARTESIAN_POINT('Ctrl Pts',(28.7840356867911,2.41410584393792,31.5905494329059));
#62420=CARTESIAN_POINT('',(28.9276321766534,2.51738042696607,31.6237706303691));
#62421=CARTESIAN_POINT('Origin',(30.,-1.32966554433622E-14,31.6237706303681));
#62422=CARTESIAN_POINT('',(28.9540051647184,2.49246284654199,31.5905494329235));
#62423=CARTESIAN_POINT('Ctrl Pts',(28.9540051647116,2.49246284654845,31.5905494329321));
#62424=CARTESIAN_POINT('Ctrl Pts',(28.9408992085311,2.50484554343346,31.6070390220085));
#62425=CARTESIAN_POINT('Ctrl Pts',(28.9276321766587,2.51738042696107,31.6237706303625));
#62426=CARTESIAN_POINT('',(28.9771926604684,2.50206742175908,31.5905494329235));
#62427=CARTESIAN_POINT('Origin',(28.9634421120889,2.50247209787257,31.5962049920587));
#62428=CARTESIAN_POINT('',(28.9782217890806,2.53833533054862,31.6237706303691));
#62429=CARTESIAN_POINT('Ctrl Pts',(28.9782217890804,2.53833533054134,31.6237706303625));
#62430=CARTESIAN_POINT('Ctrl Pts',(28.9777040820206,2.52009062117991,31.6070390219952));
#62431=CARTESIAN_POINT('Ctrl Pts',(28.9771926604678,2.50206742173986,31.5905494329059));
#62432=CARTESIAN_POINT('',(29.1284493206709,2.59375719295039,31.6237706303691));
#62433=CARTESIAN_POINT('Origin',(30.,-1.32966554433622E-14,31.6237706303681));
#62434=CARTESIAN_POINT('',(29.1527859987874,2.56684722431571,31.5905494329235));
#62435=CARTESIAN_POINT('Ctrl Pts',(29.1527859987811,2.56684722432269,31.5905494329321));
#62436=CARTESIAN_POINT('Ctrl Pts',(29.1406919790899,2.58022003095629,31.6070390220085));
#62437=CARTESIAN_POINT('Ctrl Pts',(29.1284493206758,2.59375719294498,31.6237706303625));
#62438=CARTESIAN_POINT('',(29.1766555815128,2.57460292188403,31.5905494329235));
#62439=CARTESIAN_POINT('Origin',(29.1629791704778,2.57608521103256,31.5962049981139));
#62440=CARTESIAN_POINT('',(29.1805270849926,2.61067828431428,31.6237706303691));
#62441=CARTESIAN_POINT('Ctrl Pts',(29.1805270849917,2.61067828430704,31.6237706303626));
#62442=CARTESIAN_POINT('Ctrl Pts',(29.1785795104516,2.59253043612347,31.6070390219952));
#62443=CARTESIAN_POINT('Ctrl Pts',(29.1766555815107,2.57460292186492,31.5905494329059));
#62444=CARTESIAN_POINT('',(29.3346398644464,2.65414258332837,31.6237706303691));
#62445=CARTESIAN_POINT('Origin',(30.,-1.32966554433622E-14,31.6237706303681));
#62446=CARTESIAN_POINT('',(29.3567901889011,2.6254061353882,31.5905494329235));
#62447=CARTESIAN_POINT('Ctrl Pts',(29.3567901888954,2.62540613539565,31.5905494329321));
#62448=CARTESIAN_POINT('Ctrl Pts',(29.3457826693465,2.63968660397804,31.6070390220085));
#62449=CARTESIAN_POINT('Ctrl Pts',(29.3346398644508,2.6541425833226,31.6237706303625));
#62450=CARTESIAN_POINT('',(29.3811946946869,2.63126513885323,31.5905494329235));
#62451=CARTESIAN_POINT('Origin',(29.367676739957,2.63381590833401,31.5962050111235));
#62452=CARTESIAN_POINT('',(29.3878847039279,2.66692553831851,31.6237706303691));
#62453=CARTESIAN_POINT('Ctrl Pts',(29.3878847039265,2.66692553831136,31.6237706303626));
#62454=CARTESIAN_POINT('Ctrl Pts',(29.3845192693509,2.64898643882447,31.6070390219952));
#62455=CARTESIAN_POINT('Ctrl Pts',(29.3811946946833,2.63126513883434,31.5905494329059));
#62456=CARTESIAN_POINT('',(29.5449325747123,2.69816430208817,31.6237706303691));
#62457=CARTESIAN_POINT('Origin',(30.,-1.32966554433622E-14,31.6237706303681));
#62458=CARTESIAN_POINT('',(29.5647599813892,2.6677785445999,31.5905494329235));
#62459=CARTESIAN_POINT('Ctrl Pts',(29.5647599813841,2.66777854460778,31.5905494329321));
#62460=CARTESIAN_POINT('Ctrl Pts',(29.554906826996,2.6828786313014,31.6070390220085));
#62461=CARTESIAN_POINT('Ctrl Pts',(29.5449325747163,2.69816430208207,31.6237706303625));
#62462=CARTESIAN_POINT('',(29.589548948342,2.67170473125694,31.5905494329235));
#62463=CARTESIAN_POINT('Origin',(29.5762727932907,2.67530826149244,31.5962050315749));
#62464=CARTESIAN_POINT('',(29.5990162172125,2.70673030953627,31.6237706303691));
#62465=CARTESIAN_POINT('Ctrl Pts',(29.5990162172106,2.70673030952925,31.6237706303625));
#62466=CARTESIAN_POINT('Ctrl Pts',(29.5942536716227,2.68911055925274,31.6070390219952));
#62467=CARTESIAN_POINT('Ctrl Pts',(29.589548948337,2.67170473123838,31.5905494329059));
#62468=CARTESIAN_POINT('',(29.7580309269804,2.72555094069491,31.6237706303691));
#62469=CARTESIAN_POINT('Origin',(30.,-1.32966554433622E-14,31.6237706303681));
#62470=CARTESIAN_POINT('',(29.775413173324,2.69370321195775,31.5905494329235));
#62471=CARTESIAN_POINT('Ctrl Pts',(29.7754131733195,2.69370321196601,31.5905494329321));
#62472=CARTESIAN_POINT('Ctrl Pts',(29.7667751320655,2.7095298197151,31.6070390220085));
#62473=CARTESIAN_POINT('Ctrl Pts',(29.7580309269838,2.72555094068851,31.6237706303625));
#62474=CARTESIAN_POINT('',(29.8004337692194,2.69567237556048,31.5905494329235));
#62475=CARTESIAN_POINT('Origin',(29.7874812679388,2.70030645711977,31.5962050602857));
#62476=CARTESIAN_POINT('',(29.8126199288586,2.72984718831658,31.6237706303691));
#62477=CARTESIAN_POINT('Ctrl Pts',(29.8126199288562,2.72984718830972,31.6237706303625));
#62478=CARTESIAN_POINT('Ctrl Pts',(29.8064896349333,2.71265541886322,31.6070390219952));
#62479=CARTESIAN_POINT('Ctrl Pts',(29.800433769213,2.69567237554238,31.5905494329059));
#62480=CARTESIAN_POINT('',(29.9726210990465,2.73613365141461,31.6237706303691));
#62481=CARTESIAN_POINT('Origin',(30.,-1.32966554433622E-14,31.6237706303681));
#62482=CARTESIAN_POINT('',(29.987451017728,2.70302030326666,31.5905494329235));
#62483=CARTESIAN_POINT('Ctrl Pts',(29.9874510177241,2.70302030327525,31.5905494329321));
#62484=CARTESIAN_POINT('Ctrl Pts',(29.9800813460009,2.71947585578017,31.6070390220085));
#62485=CARTESIAN_POINT('Ctrl Pts',(29.9726210990495,2.73613365140797,31.6237706303625));
#62486=CARTESIAN_POINT('Ctrl Pts',(30.,2.69489040503946,31.5823904050395));
#62487=CARTESIAN_POINT('Ctrl Pts',(29.9982996971592,2.69489040503946,31.5823904050395));
#62488=CARTESIAN_POINT('Ctrl Pts',(29.9965490639354,2.69522714758866,31.5827289231894));
#62489=CARTESIAN_POINT('Ctrl Pts',(29.9934248389279,2.69644647069982,31.5839540167345));
#62490=CARTESIAN_POINT('Ctrl Pts',(29.9920523583067,2.69733049287039,31.5848419899159));
#62491=CARTESIAN_POINT('Ctrl Pts',(29.9894391186861,2.6996015700298,31.5871217896387));
#62492=CARTESIAN_POINT('Ctrl Pts',(29.9882404972758,2.70125749446876,31.5887829779419));
#62493=CARTESIAN_POINT('Ctrl Pts',(29.987451017728,2.70302030326666,31.5905494329235));
#62494=CARTESIAN_POINT('',(30.,2.68872936963187,31.5762293696319));
#62495=CARTESIAN_POINT('',(30.,2.68872936963187,31.5762293696319));
#62496=CARTESIAN_POINT('',(30.,-2.68872936963189,31.5762293696319));
#62497=CARTESIAN_POINT('Origin',(30.,-1.32966554433622E-14,31.5762293696319));
#62498=CARTESIAN_POINT('Origin',(30.,-1.32966554433622E-14,31.5762293696319));
#62499=CARTESIAN_POINT('Origin',(30.,-1.32966554433622E-14,31.5430837392638));
#62500=CARTESIAN_POINT('',(30.,-2.67500000000001,31.5430837392638));
#62501=CARTESIAN_POINT('Origin',(30.,-1.32966554433622E-14,31.5430837392638));
#62502=CARTESIAN_POINT('Origin',(30.,-2.72187500000001,31.5430837392638));
#62503=CARTESIAN_POINT('Origin',(30.,-1.32966554433622E-14,16.));
#62504=CARTESIAN_POINT('',(30.,-2.67500000000001,31.06875));
#62505=CARTESIAN_POINT('Origin',(30.,-1.32966554433622E-14,31.06875));
#62506=CARTESIAN_POINT('',(30.,-2.67500000000001,16.));
#62507=CARTESIAN_POINT('Origin',(30.,-1.32966554433622E-14,31.06875));
#62508=CARTESIAN_POINT('',(30.,-2.60625000000001,31.));
#62509=CARTESIAN_POINT('Origin',(30.,-1.32966554433622E-14,31.));
#62510=CARTESIAN_POINT('Origin',(30.,-2.60625000000001,31.06875));
#62511=CARTESIAN_POINT('Origin',(30.,-1.32966554433622E-14,30.85));
#62512=CARTESIAN_POINT('',(30.,-1.65000000000002,31.));
#62513=CARTESIAN_POINT('Origin',(30.,-1.65000000000001,30.85));
#62514=CARTESIAN_POINT('Origin',(30.,-1.32966554433622E-14,31.));
#62515=CARTESIAN_POINT('Origin',(30.,-1.32966554433622E-14,31.6569162607362));
#62516=CARTESIAN_POINT('',(27.4723387620945,1.08324912480478,31.6569162607362));
#62517=CARTESIAN_POINT('Origin',(27.5075595450194,1.04598613791953,31.6570432561871));
#62518=CARTESIAN_POINT('',(27.5347062454699,1.21853465435945,31.6569162607362));
#62519=CARTESIAN_POINT('Origin',(30.,-1.32966554433622E-14,31.6569162607362));
#62520=CARTESIAN_POINT('Origin',(27.5859112932463,1.21595145595199,31.6570220656254));
#62521=CARTESIAN_POINT('Origin',(30.,-1.32966554433622E-14,31.6569162607362));
#62522=CARTESIAN_POINT('',(27.4467007962708,1.0213536000015,31.6569162607362));
#62523=CARTESIAN_POINT('Origin',(27.4979506713832,1.02279586647784,31.6570220656247));
#62524=CARTESIAN_POINT('',(27.3951399513465,0.881591814236737,31.6569162607362));
#62525=CARTESIAN_POINT('Origin',(27.4331757806072,0.847207087483285,31.6570432561871));
#62526=CARTESIAN_POINT('Origin',(30.,-1.32966554433622E-14,31.6569162607362));
#62527=CARTESIAN_POINT('Origin',(30.,-1.32966554433622E-14,31.6569162607362));
#62528=CARTESIAN_POINT('',(27.3744372857209,0.817875561065013,31.6569162607362));
#62529=CARTESIAN_POINT('Origin',(27.4254160156494,0.82333440037271,31.6570220656251));
#62530=CARTESIAN_POINT('',(27.3340009690024,0.674499196974899,31.6569162607362));
#62531=CARTESIAN_POINT('Origin',(27.3746173410621,0.643204723628532,31.6570432561866));
#62532=CARTESIAN_POINT('Origin',(30.,-1.32966554433622E-14,31.6569162607362));
#62533=CARTESIAN_POINT('Origin',(30.,-1.32966554433622E-14,31.6569162607362));
#62534=CARTESIAN_POINT('',(27.3183612423927,0.609355047323335,31.6569162607362));
#62535=CARTESIAN_POINT('Origin',(27.3687545263143,0.61879680390278,31.6570220656251));
#62536=CARTESIAN_POINT('',(27.2892987572189,0.463248067869971,31.6569162607362));
#62537=CARTESIAN_POINT('Origin',(27.3322452586394,0.435236788764015,31.6570432561869));
#62538=CARTESIAN_POINT('Origin',(30.,-1.32966554433622E-14,31.6569162607362));
#62539=CARTESIAN_POINT('Origin',(30.,-1.32966554433622E-14,31.6569162607362));
#62540=CARTESIAN_POINT('',(27.2788183937405,0.397077657083795,31.6569162607362));
#62541=CARTESIAN_POINT('Origin',(27.3283155403022,0.41044411936593,31.6570220656249));
#62542=CARTESIAN_POINT('',(27.2613089199969,0.249140860381007,31.6569162607362));
#62543=CARTESIAN_POINT('Origin',(27.3063207713152,0.224585474366194,31.6570432561871));
#62544=CARTESIAN_POINT('Origin',(30.,-1.32966554433622E-14,31.6569162607362));
#62545=CARTESIAN_POINT('Origin',(30.,-1.32966554433622E-14,31.6569162607362));
#62546=CARTESIAN_POINT('',(27.2560525345756,0.182352151046611,31.6569162607362));
#62547=CARTESIAN_POINT('Origin',(27.3043483774102,0.199560910346922,31.6570220656251));
#62548=CARTESIAN_POINT('',(27.2502040239902,0.0334976166400503,31.6569162607362));
#62549=CARTESIAN_POINT('Origin',(27.2970037121761,0.0125495158363338,31.6570432561875));
#62550=CARTESIAN_POINT('Origin',(30.,-1.32966554433622E-14,31.6569162607362));
#62551=CARTESIAN_POINT('Origin',(30.,-1.32966554433622E-14,31.6569162607362));
#62552=CARTESIAN_POINT('',(27.2502040239902,-0.0334976166400194,31.6569162607362));
#62553=CARTESIAN_POINT('Origin',(27.297000803166,-0.0125526580452972,31.6570220656252));
#62554=CARTESIAN_POINT('',(27.2560525345756,-0.18235215104658,31.6569162607362));
#62555=CARTESIAN_POINT('Origin',(27.3043515239857,-0.199563814630509,31.6570432561868));
#62556=CARTESIAN_POINT('Origin',(30.,-1.32966554433622E-14,31.6569162607362));
#62557=CARTESIAN_POINT('Origin',(30.,-1.32966554433622E-14,31.6569162607362));
#62558=CARTESIAN_POINT('',(27.2613089199969,-0.249140860380976,31.6569162607362));
#62559=CARTESIAN_POINT('Origin',(27.3063181178117,-0.22458883512474,31.6570220656265));
#62560=CARTESIAN_POINT('',(27.2788183937405,-0.397077657083763,31.6569162607362));
#62561=CARTESIAN_POINT('Origin',(27.3283189050458,-0.410446767819208,31.6570432561867));
#62562=CARTESIAN_POINT('Origin',(30.,-1.32966554433622E-14,31.6569162607362));
#62563=CARTESIAN_POINT('Origin',(30.,-1.32966554433622E-14,31.6569162607362));
#62564=CARTESIAN_POINT('',(27.2892987572189,-0.463248067869938,31.6569162607362));
#62565=CARTESIAN_POINT('Origin',(27.3322428769935,-0.4352403473568,31.6570220656245));
#62566=CARTESIAN_POINT('',(27.3183612423927,-0.609355047323306,31.6569162607362));
#62567=CARTESIAN_POINT('Origin',(27.3687580884808,-0.618799180197033,31.6570432561867));
#62568=CARTESIAN_POINT('Origin',(30.,-1.32966554433622E-14,31.6569162607362));
#62569=CARTESIAN_POINT('Origin',(30.,-1.32966554433622E-14,31.6569162607362));
#62570=CARTESIAN_POINT('',(27.3340009690024,-0.674499196974871,31.6569162607362));
#62571=CARTESIAN_POINT('Origin',(27.3746152459701,-0.643208458106799,31.6570220656281));
#62572=CARTESIAN_POINT('',(27.3744372857209,-0.817875561064986,31.6569162607362));
#62573=CARTESIAN_POINT('Origin',(27.4254197532793,-0.823336489857566,31.6570432561877));
#62574=CARTESIAN_POINT('Origin',(30.,-1.32966554433622E-14,31.6569162607362));
#62575=CARTESIAN_POINT('Origin',(30.,-1.32966554433622E-14,31.6569162607362));
#62576=CARTESIAN_POINT('',(27.3951399513465,-0.88159181423671,31.6569162607362));
#62577=CARTESIAN_POINT('Origin',(27.4331739849698,-0.847210974835381,31.6570220656246));
#62578=CARTESIAN_POINT('',(27.4467007962708,-1.02135360000148,31.6569162607362));
#62579=CARTESIAN_POINT('Origin',(27.4979545614299,-1.02279765627042,31.6570432561873));
#62580=CARTESIAN_POINT('Origin',(30.,-1.32966554433622E-14,31.6569162607362));
#62581=CARTESIAN_POINT('Origin',(30.,-1.32966554433622E-14,31.6569162607362));
#62582=CARTESIAN_POINT('',(27.4723387620945,-1.08324912480475,31.6569162607362));
#62583=CARTESIAN_POINT('Origin',(27.5075580599161,-1.04599015417175,31.657022065625));
#62584=CARTESIAN_POINT('',(27.5347062454699,-1.21853465435942,31.6569162607362));
#62585=CARTESIAN_POINT('Origin',(27.5859153117243,-1.21595293501783,31.6570432561869));
#62586=CARTESIAN_POINT('Origin',(30.,-1.32966554433622E-14,31.6569162607362));
#62587=CARTESIAN_POINT('Origin',(30.,-1.32966554433622E-14,31.6569162607362));
#62588=CARTESIAN_POINT('',(27.5651214449068,-1.27822784430149,31.6569162607362));
#62589=CARTESIAN_POINT('Origin',(27.5973088682438,-1.23832045638074,31.6570220656251));
#62590=CARTESIAN_POINT('',(27.637911050459,-1.40820303736935,31.6569162607362));
#62591=CARTESIAN_POINT('Origin',(27.6887596968882,-1.40161145957539,31.6570432561872));
#62592=CARTESIAN_POINT('Origin',(30.,-1.32966554433622E-14,31.6569162607362));
#62593=CARTESIAN_POINT('Origin',(30.,-1.32966554433622E-14,31.6569162607362));
#62594=CARTESIAN_POINT('',(27.6729159636906,-1.46532586408421,31.6569162607362));
#62595=CARTESIAN_POINT('Origin',(27.7018730663766,-1.42301610118967,31.6570220656267));
#62596=CARTESIAN_POINT('',(27.7556789192963,-1.58918938037887,31.6569162607362));
#62597=CARTESIAN_POINT('Origin',(27.8058536470839,-1.57862858340189,31.6570432561867));
#62598=CARTESIAN_POINT('Origin',(30.,-1.32966554433622E-14,31.6569162607362));
#62599=CARTESIAN_POINT('Origin',(30.,-1.32966554433622E-14,31.6569162607362));
#62600=CARTESIAN_POINT('',(27.7950577293922,-1.64338966264456,31.6569162607362));
#62601=CARTESIAN_POINT('Origin',(27.8206059812726,-1.59893837851,31.6570220656387));
#62602=CARTESIAN_POINT('',(27.8872837739086,-1.76037784239926,31.6569162607362));
#62603=CARTESIAN_POINT('Origin',(27.9364752391763,-1.7459129370637,31.6570432561874));
#62604=CARTESIAN_POINT('Origin',(30.,-1.32966554433622E-14,31.6569162607362));
#62605=CARTESIAN_POINT('Origin',(30.,-1.32966554433622E-14,31.6569162607362));
#62606=CARTESIAN_POINT('',(27.9307936974098,-1.81132141745219,31.6569162607362));
#62607=CARTESIAN_POINT('Origin',(27.9527755849842,-1.76500266908356,31.6570220656253));
#62608=CARTESIAN_POINT('',(28.0319142266042,-1.92071298963622,31.6569162607362));
#62609=CARTESIAN_POINT('Origin',(28.0798191476078,-1.90243315689441,31.657043256187));
#62610=CARTESIAN_POINT('Origin',(30.,-1.32966554433622E-14,31.6569162607362));
#62611=CARTESIAN_POINT('Origin',(30.,-1.32966554433622E-14,31.6569162607362));
#62612=CARTESIAN_POINT('',(28.0792870103637,-1.96808577339573,31.6569162607362));
#62613=CARTESIAN_POINT('Origin',(28.097567008002,-1.92018513125043,31.6570220656245));
#62614=CARTESIAN_POINT('',(28.1886785825478,-2.06920630259019,31.6569162607362));
#62615=CARTESIAN_POINT('Origin',(28.2350016095212,-2.0472242436889,31.6570432561873));
#62616=CARTESIAN_POINT('Origin',(30.,-1.32966554433622E-14,31.6569162607362));
#62617=CARTESIAN_POINT('Origin',(30.,-1.32966554433622E-14,31.6569162607362));
#62618=CARTESIAN_POINT('',(28.2396221576007,-2.11271622609136,31.6569162607362));
#62619=CARTESIAN_POINT('Origin',(28.2540875630401,-2.06352901355267,31.6570220656256));
#62620=CARTESIAN_POINT('',(28.3566103373554,-2.20494227060778,31.6569162607362));
#62621=CARTESIAN_POINT('Origin',(28.4010658734316,-2.17939351225073,31.6570432561869));
#62622=CARTESIAN_POINT('Origin',(30.,-1.32966554433622E-14,31.6569162607362));
#62623=CARTESIAN_POINT('Origin',(30.,-1.32966554433622E-14,31.6569162607362));
#62624=CARTESIAN_POINT('',(28.4108106196211,-2.2443210807037,31.6569162607362));
#62625=CARTESIAN_POINT('Origin',(28.4213722488256,-2.19415055329735,31.6570220656249));
#62626=CARTESIAN_POINT('',(28.5346741359157,-2.32708403630936,31.6569162607362));
#62627=CARTESIAN_POINT('Origin',(28.5769880979323,-2.29812609508764,31.6570432561867));
#62628=CARTESIAN_POINT('Origin',(30.,-1.32966554433622E-14,31.6569162607362));
#62629=CARTESIAN_POINT('Origin',(30.,-1.32966554433622E-14,31.6569162607362));
#62630=CARTESIAN_POINT('',(28.5917969626306,-2.362088949541,31.6569162607362));
#62631=CARTESIAN_POINT('Origin',(28.5983896996446,-2.31124442525031,31.6570220656249));
#62632=CARTESIAN_POINT('',(28.7217721556985,-2.43487855509312,31.6569162607362));
#62633=CARTESIAN_POINT('Origin',(28.7616836640096,-2.40268996634326,31.6570432561868));
#62634=CARTESIAN_POINT('Origin',(30.,-1.32966554433622E-14,31.6569162607362));
#62635=CARTESIAN_POINT('Origin',(30.,-1.32966554433622E-14,31.6569162607362));
#62636=CARTESIAN_POINT('',(28.7814653456405,-2.46529375453011,31.6569162607362));
#62637=CARTESIAN_POINT('Origin',(28.784048544048,-2.41408870675338,31.6570220656255));
#62638=CARTESIAN_POINT('',(28.9167508751952,-2.52766123790546,31.6569162607362));
#62639=CARTESIAN_POINT('Origin',(28.9540138620808,-2.49244045498024,31.6570432561872));
#62640=CARTESIAN_POINT('Origin',(30.,-1.32966554433622E-14,31.6569162607362));
#62641=CARTESIAN_POINT('Origin',(30.,-1.32966554433622E-14,31.6569162607362));
#62642=CARTESIAN_POINT('',(28.9786463999985,-2.55329920372917,31.6569162607362));
#62643=CARTESIAN_POINT('Origin',(28.9772041335221,-2.50204932861609,31.657022065625));
#62644=CARTESIAN_POINT('',(29.1184081857632,-2.60486004865345,31.6569162607362));
#62645=CARTESIAN_POINT('Origin',(29.1527929125168,-2.56682421939275,31.6570432561872));
#62646=CARTESIAN_POINT('Origin',(30.,-1.32966554433622E-14,31.6569162607362));
#62647=CARTESIAN_POINT('Origin',(30.,-1.32966554433622E-14,31.6569162607362));
#62648=CARTESIAN_POINT('',(29.182124438935,-2.6255627142791,31.6569162607362));
#62649=CARTESIAN_POINT('Origin',(29.1766655996274,-2.57458398435135,31.6570220656246));
#62650=CARTESIAN_POINT('',(29.3255008030251,-2.66599903099763,31.6569162607362));
#62651=CARTESIAN_POINT('Origin',(29.3567952763715,-2.62538265893786,31.6570432561866));
#62652=CARTESIAN_POINT('Origin',(30.,-1.32966554433622E-14,31.6569162607362));
#62653=CARTESIAN_POINT('Origin',(30.,-1.32966554433622E-14,31.6569162607362));
#62654=CARTESIAN_POINT('',(29.3906449526766,-2.6816387576073,31.6569162607362));
#62655=CARTESIAN_POINT('Origin',(29.3812031960972,-2.63124547368565,31.6570220656251));
#62656=CARTESIAN_POINT('',(29.53675193213,-2.71070124278106,31.6569162607362));
#62657=CARTESIAN_POINT('Origin',(29.5647632112362,-2.66775474136028,31.6570432561871));
#62658=CARTESIAN_POINT('Origin',(30.,-1.32966554433622E-14,31.6569162607362));
#62659=CARTESIAN_POINT('Origin',(30.,-1.32966554433622E-14,31.6569162607362));
#62660=CARTESIAN_POINT('',(29.6029223429162,-2.72118160625948,31.6569162607362));
#62661=CARTESIAN_POINT('Origin',(29.5895558806344,-2.67168445969898,31.6570220656245));
#62662=CARTESIAN_POINT('',(29.750859139619,-2.73869108000313,31.6569162607362));
#62663=CARTESIAN_POINT('Origin',(29.7754145256345,-2.69367922868347,31.6570432561876));
#62664=CARTESIAN_POINT('Origin',(30.,-1.32966554433622E-14,31.6569162607362));
#62665=CARTESIAN_POINT('Origin',(30.,-1.32966554433622E-14,31.6569162607362));
#62666=CARTESIAN_POINT('',(29.8176478489534,-2.74394746542436,31.6569162607362));
#62667=CARTESIAN_POINT('Origin',(29.800439089653,-2.69565162258972,31.6570220656252));
#62668=CARTESIAN_POINT('',(29.9665023833599,-2.74979597600977,31.6569162607362));
#62669=CARTESIAN_POINT('Origin',(29.9874504841626,-2.70299628782621,31.6570432561866));
#62670=CARTESIAN_POINT('Origin',(30.,-1.32966554433622E-14,31.6569162607362));
#62671=CARTESIAN_POINT('Origin',(30.,-1.32966554433622E-14,31.6569162607362));
#62672=CARTESIAN_POINT('',(30.03349761664,-2.74979597600977,31.6569162607362));
#62673=CARTESIAN_POINT('Origin',(30.0125526580435,-2.70299919683014,31.6570220656269));
#62674=CARTESIAN_POINT('',(30.1823521510466,-2.74394746542436,31.6569162607362));
#62675=CARTESIAN_POINT('Origin',(30.1995638146306,-2.69564847601399,31.6570432561868));
#62676=CARTESIAN_POINT('Origin',(30.,-1.32966554433622E-14,31.6569162607362));
#62677=CARTESIAN_POINT('Origin',(30.,-1.32966554433622E-14,31.6569162607362));
#62678=CARTESIAN_POINT('',(30.2491408603809,-2.73869108000313,31.6569162607362));
#62679=CARTESIAN_POINT('Origin',(30.2245888351274,-2.69368188219317,31.6570220656245));
#62680=CARTESIAN_POINT('',(30.3970776570837,-2.72118160625948,31.6569162607362));
#62681=CARTESIAN_POINT('Origin',(30.4104467678196,-2.67168109495285,31.6570432561872));
#62682=CARTESIAN_POINT('Origin',(30.,-1.32966554433622E-14,31.6569162607362));
#62683=CARTESIAN_POINT('Origin',(30.,-1.32966554433622E-14,31.6569162607362));
#62684=CARTESIAN_POINT('',(30.4632480678699,-2.71070124278107,31.6569162607362));
#62685=CARTESIAN_POINT('Origin',(30.4352403473562,-2.66775712300563,31.6570220656249));
#62686=CARTESIAN_POINT('',(30.6093550473233,-2.68163875760731,31.6569162607362));
#62687=CARTESIAN_POINT('Origin',(30.6187991801974,-2.63124191151731,31.6570432561874));
#62688=CARTESIAN_POINT('Origin',(30.,-1.32966554433622E-14,31.6569162607362));
#62689=CARTESIAN_POINT('Origin',(30.,-1.32966554433622E-14,31.6569162607362));
#62690=CARTESIAN_POINT('',(30.6744991969748,-2.66599903099764,31.6569162607362));
#62691=CARTESIAN_POINT('Origin',(30.6432084581108,-2.62538475403506,31.6570220656255));
#62692=CARTESIAN_POINT('',(30.817875561065,-2.62556271427912,31.6569162607362));
#62693=CARTESIAN_POINT('Origin',(30.8233364898573,-2.57458024672293,31.6570432561868));
#62694=CARTESIAN_POINT('Origin',(30.,-1.32966554433622E-14,31.6569162607362));
#62695=CARTESIAN_POINT('Origin',(30.,-1.32966554433622E-14,31.6569162607362));
#62696=CARTESIAN_POINT('',(30.8815918142367,-2.60486004865346,31.6569162607362));
#62697=CARTESIAN_POINT('Origin',(30.8472109748348,-2.56682601502956,31.6570220656249));
#62698=CARTESIAN_POINT('',(31.0213536000014,-2.55329920372919,31.6569162607362));
#62699=CARTESIAN_POINT('Origin',(31.0227976562703,-2.50204543857134,31.6570432561867));
#62700=CARTESIAN_POINT('Origin',(30.,-1.32966554433622E-14,31.6569162607362));
#62701=CARTESIAN_POINT('Origin',(30.,-1.32966554433622E-14,31.6569162607362));
#62702=CARTESIAN_POINT('',(31.0832491248047,-2.52766123790547,31.6569162607362));
#62703=CARTESIAN_POINT('Origin',(31.0459901541642,-2.49244194007693,31.6570220656289));
#62704=CARTESIAN_POINT('',(31.2185346543594,-2.46529375453013,31.6569162607362));
#62705=CARTESIAN_POINT('Origin',(31.2159529350178,-2.41408468827489,31.6570432561872));
#62706=CARTESIAN_POINT('Origin',(30.,-1.32966554433622E-14,31.6569162607362));
#62707=CARTESIAN_POINT('Origin',(30.,-1.32966554433622E-14,31.6569162607362));
#62708=CARTESIAN_POINT('',(31.2782278443015,-2.43487855509314,31.6569162607362));
#62709=CARTESIAN_POINT('Origin',(31.238320456382,-2.40269113175716,31.6570220656245));
#62710=CARTESIAN_POINT('',(31.4082030373693,-2.36208894954102,31.6569162607362));
#62711=CARTESIAN_POINT('Origin',(31.4016114595753,-2.31124030311134,31.6570432561875));
#62712=CARTESIAN_POINT('Origin',(30.,-1.32966554433622E-14,31.6569162607362));
#62713=CARTESIAN_POINT('Origin',(30.,-1.32966554433622E-14,31.6569162607362));
#62714=CARTESIAN_POINT('',(31.4653258640842,-2.32708403630938,31.6569162607362));
#62715=CARTESIAN_POINT('Origin',(31.4230161011935,-2.29812693362589,31.657022065625));
#62716=CARTESIAN_POINT('',(31.5891893803788,-2.24432108070372,31.6569162607362));
#62717=CARTESIAN_POINT('Origin',(31.5786285834021,-2.1941463529175,31.6570432561862));
#62718=CARTESIAN_POINT('Origin',(30.,-1.32966554433622E-14,31.6569162607362));
#62719=CARTESIAN_POINT('Origin',(30.,-1.32966554433622E-14,31.6569162607362));
#62720=CARTESIAN_POINT('',(31.6433896626445,-2.2049422706078,31.6569162607362));
#62721=CARTESIAN_POINT('Origin',(31.5989383785409,-2.17939401874466,31.6570220656252));
#62722=CARTESIAN_POINT('',(31.7603778423992,-2.11271622609138,31.6569162607362));
#62723=CARTESIAN_POINT('Origin',(31.7459129370641,-2.0635247608251,31.6570432561869));
#62724=CARTESIAN_POINT('Origin',(30.,-1.32966554433622E-14,31.6569162607362));
#62725=CARTESIAN_POINT('Origin',(30.,-1.32966554433622E-14,31.6569162607362));
#62726=CARTESIAN_POINT('',(31.8113214174522,-2.06920630259022,31.6569162607362));
#62727=CARTESIAN_POINT('Origin',(31.7650026690826,-2.04722441501533,31.6570220656257));
#62728=CARTESIAN_POINT('',(31.9207129896362,-1.96808577339576,31.6569162607362));
#62729=CARTESIAN_POINT('Origin',(31.9024331568943,-1.92018085239205,31.657043256187));
#62730=CARTESIAN_POINT('Origin',(30.,-1.32966554433622E-14,31.6569162607362));
#62731=CARTESIAN_POINT('Origin',(30.,-1.32966554433622E-14,31.6569162607362));
#62732=CARTESIAN_POINT('',(31.9680857733957,-1.92071298963625,31.6569162607362));
#62733=CARTESIAN_POINT('Origin',(31.9201851312437,-1.90243299199549,31.6570220656273));
#62734=CARTESIAN_POINT('',(32.0692063025902,-1.81132141745222,31.6569162607362));
#62735=CARTESIAN_POINT('Origin',(32.0472242436891,-1.76499839047944,31.6570432561871));
#62736=CARTESIAN_POINT('Origin',(30.,-1.32966554433622E-14,31.6569162607362));
#62737=CARTESIAN_POINT('Origin',(30.,-1.32966554433622E-14,31.6569162607362));
#62738=CARTESIAN_POINT('',(32.1127162260913,-1.76037784239929,31.6569162607362));
#62739=CARTESIAN_POINT('Origin',(32.0635290135546,-1.74591243696045,31.6570220656248));
#62740=CARTESIAN_POINT('',(32.2049422706077,-1.64338966264459,31.6569162607362));
#62741=CARTESIAN_POINT('Origin',(32.1793935122505,-1.59893412656801,31.6570432561871));
#62742=CARTESIAN_POINT('Origin',(30.,-1.32966554433622E-14,31.6569162607362));
#62743=CARTESIAN_POINT('Origin',(30.,-1.32966554433622E-14,31.6569162607362));
#62744=CARTESIAN_POINT('',(32.2443210807037,-1.5891893803789,31.6569162607362));
#62745=CARTESIAN_POINT('Origin',(32.1941505532956,-1.57862775117404,31.6570220656256));
#62746=CARTESIAN_POINT('',(32.3270840363093,-1.46532586408424,31.6569162607362));
#62747=CARTESIAN_POINT('Origin',(32.2981260950875,-1.42301190206755,31.6570432561867));
#62748=CARTESIAN_POINT('Origin',(30.,-1.32966554433622E-14,31.6569162607362));
#62749=CARTESIAN_POINT('Origin',(30.,-1.32966554433622E-14,31.6569162607362));
#62750=CARTESIAN_POINT('',(32.362088949541,-1.40820303736938,31.6569162607362));
#62751=CARTESIAN_POINT('Origin',(32.3112444252322,-1.40161030035328,31.657022065632));
#62752=CARTESIAN_POINT('',(32.4348785550931,-1.27822784430152,31.6569162607362));
#62753=CARTESIAN_POINT('Origin',(32.4026899663432,-1.23831633599041,31.6570432561868));
#62754=CARTESIAN_POINT('Origin',(30.,-1.32966554433622E-14,31.6569162607362));
#62755=CARTESIAN_POINT('Origin',(30.,-1.32966554433622E-14,31.6569162607362));
#62756=CARTESIAN_POINT('',(32.4652937545301,-1.21853465435946,31.6569162607362));
#62757=CARTESIAN_POINT('Origin',(32.414088706754,-1.21595145595202,31.6570220656252));
#62758=CARTESIAN_POINT('',(32.5276612379054,-1.08324912480479,31.6569162607362));
#62759=CARTESIAN_POINT('Origin',(32.4924404549811,-1.04598613792014,31.6570432561868));
#62760=CARTESIAN_POINT('Origin',(30.,-1.32966554433622E-14,31.6569162607362));
#62761=CARTESIAN_POINT('Origin',(30.,-1.32966554433622E-14,31.6569162607362));
#62762=CARTESIAN_POINT('',(32.5532992037291,-1.02135360000151,31.6569162607362));
#62763=CARTESIAN_POINT('Origin',(32.5020493286151,-1.0227958664779,31.6570220656254));
#62764=CARTESIAN_POINT('',(32.6048600486534,-0.881591814236746,31.6569162607362));
#62765=CARTESIAN_POINT('Origin',(32.5668242193914,-0.847207087482045,31.6570432561878));
#62766=CARTESIAN_POINT('Origin',(30.,-1.32966554433622E-14,31.6569162607362));
#62767=CARTESIAN_POINT('Origin',(30.,-1.32966554433622E-14,31.6569162607362));
#62768=CARTESIAN_POINT('',(32.6255627142791,-0.817875561065022,31.6569162607362));
#62769=CARTESIAN_POINT('Origin',(32.5745839843496,-0.82333440037284,31.6570220656255));
#62770=CARTESIAN_POINT('',(32.6659990309976,-0.674499196974908,31.6569162607362));
#62771=CARTESIAN_POINT('Origin',(32.6253826589374,-0.643204723628158,31.6570432561868));
#62772=CARTESIAN_POINT('Origin',(30.,-1.32966554433622E-14,31.6569162607362));
#62773=CARTESIAN_POINT('Origin',(30.,-1.32966554433622E-14,31.6569162607362));
#62774=CARTESIAN_POINT('',(32.6816387576073,-0.609355047323343,31.6569162607362));
#62775=CARTESIAN_POINT('Origin',(32.6312454736857,-0.618796803902764,31.657022065625));
#62776=CARTESIAN_POINT('',(32.710701242781,-0.463248067869977,31.6569162607362));
#62777=CARTESIAN_POINT('Origin',(32.6677547413593,-0.435236788763208,31.6570432561875));
#62778=CARTESIAN_POINT('Origin',(30.,-1.32966554433622E-14,31.6569162607362));
#62779=CARTESIAN_POINT('Origin',(30.,-1.32966554433622E-14,31.6569162607362));
#62780=CARTESIAN_POINT('',(32.7211816062594,-0.397077657083801,31.6569162607362));
#62781=CARTESIAN_POINT('Origin',(32.6716844596186,-0.410444119388296,31.6570220656567));
#62782=CARTESIAN_POINT('',(32.7386910800031,-0.249140860381013,31.6569162607362));
#62783=CARTESIAN_POINT('Origin',(32.6936792286845,-0.224585474366052,31.6570432561872));
#62784=CARTESIAN_POINT('Origin',(30.,-1.32966554433622E-14,31.6569162607362));
#62785=CARTESIAN_POINT('Origin',(30.,-1.32966554433622E-14,31.6569162607362));
#62786=CARTESIAN_POINT('',(32.7439474654243,-0.182352151046618,31.6569162607362));
#62787=CARTESIAN_POINT('Origin',(32.695651622591,-0.19956091034649,31.6570220656247));
#62788=CARTESIAN_POINT('',(32.7497959760097,-0.0334976166400576,31.6569162607362));
#62789=CARTESIAN_POINT('Origin',(32.702996287825,-0.0125495158368562,31.657043256187));
#62790=CARTESIAN_POINT('Origin',(30.,-1.32966554433622E-14,31.6569162607362));
#62791=CARTESIAN_POINT('Origin',(30.,-1.32966554433622E-14,31.6569162607362));
#62792=CARTESIAN_POINT('',(32.7497959760097,0.0334976166400122,31.6569162607362));
#62793=CARTESIAN_POINT('Origin',(32.7029991968315,0.0125526580441019,31.6570220656263));
#62794=CARTESIAN_POINT('',(32.7439474654243,0.182352151046572,31.6569162607362));
#62795=CARTESIAN_POINT('Origin',(32.695648476013,0.199563814630937,31.6570432561873));
#62796=CARTESIAN_POINT('Origin',(30.,-1.32966554433622E-14,31.6569162607362));
#62797=CARTESIAN_POINT('Origin',(30.,-1.32966554433622E-14,31.6569162607362));
#62798=CARTESIAN_POINT('',(32.7386910800031,0.249140860380968,31.6569162607362));
#62799=CARTESIAN_POINT('Origin',(32.6936818821912,0.224588835126342,31.6570220656253));
#62800=CARTESIAN_POINT('',(32.7211816062594,0.397077657083756,31.6569162607362));
#62801=CARTESIAN_POINT('Origin',(32.6716810949533,0.410446767819417,31.657043256187));
#62802=CARTESIAN_POINT('Origin',(30.,-1.32966554433622E-14,31.6569162607362));
#62803=CARTESIAN_POINT('Origin',(30.,-1.32966554433622E-14,31.6569162607362));
#62804=CARTESIAN_POINT('',(32.710701242781,0.463248067869931,31.6569162607362));
#62805=CARTESIAN_POINT('Origin',(32.6677571230054,0.435240347356078,31.6570220656249));
#62806=CARTESIAN_POINT('',(32.6816387576073,0.609355047323298,31.6569162607362));
#62807=CARTESIAN_POINT('Origin',(32.6312419115184,0.618799180197174,31.657043256187));
#62808=CARTESIAN_POINT('Origin',(30.,-1.32966554433622E-14,31.6569162607362));
#62809=CARTESIAN_POINT('Origin',(30.,-1.32966554433622E-14,31.6569162607362));
#62810=CARTESIAN_POINT('',(32.6659990309976,0.674499196974863,31.6569162607362));
#62811=CARTESIAN_POINT('Origin',(32.6253847539863,0.643208458072405,31.6570220656495));
#62812=CARTESIAN_POINT('',(32.6255627142791,0.817875561064977,31.6569162607362));
#62813=CARTESIAN_POINT('Origin',(32.574580246722,0.823336489857403,31.6570432561872));
#62814=CARTESIAN_POINT('Origin',(30.,-1.32966554433622E-14,31.6569162607362));
#62815=CARTESIAN_POINT('Origin',(30.,-1.32966554433622E-14,31.6569162607362));
#62816=CARTESIAN_POINT('',(32.6048600486534,0.881591814236701,31.6569162607362));
#62817=CARTESIAN_POINT('Origin',(32.5668260150295,0.847210974834854,31.6570220656249));
#62818=CARTESIAN_POINT('',(32.5532992037291,1.02135360000147,31.6569162607362));
#62819=CARTESIAN_POINT('Origin',(32.5020454385711,1.02279765627039,31.6570432561869));
#62820=CARTESIAN_POINT('Origin',(30.,-1.32966554433622E-14,31.6569162607362));
#62821=CARTESIAN_POINT('Origin',(30.,-1.32966554433622E-14,31.6569162607362));
#62822=CARTESIAN_POINT('',(32.5276612379054,1.08324912480474,31.6569162607362));
#62823=CARTESIAN_POINT('Origin',(32.4924419400839,1.04599015417185,31.6570220656248));
#62824=CARTESIAN_POINT('',(32.4652937545301,1.21853465435941,31.6569162607362));
#62825=CARTESIAN_POINT('Origin',(32.4140846882753,1.2159529350178,31.657043256187));
#62826=CARTESIAN_POINT('Origin',(30.,-1.32966554433622E-14,31.6569162607362));
#62827=CARTESIAN_POINT('Origin',(30.,-1.32966554433622E-14,31.6569162607362));
#62828=CARTESIAN_POINT('',(32.4348785550931,1.27822784430148,31.6569162607362));
#62829=CARTESIAN_POINT('Origin',(32.4026911317566,1.23832045638126,31.6570220656248));
#62830=CARTESIAN_POINT('',(32.362088949541,1.40820303736934,31.6569162607362));
#62831=CARTESIAN_POINT('Origin',(32.3112403031114,1.40161145957535,31.6570432561874));
#62832=CARTESIAN_POINT('Origin',(30.,-1.32966554433622E-14,31.6569162607362));
#62833=CARTESIAN_POINT('Origin',(30.,-1.32966554433622E-14,31.6569162607362));
#62834=CARTESIAN_POINT('',(32.3270840363093,1.4653258640842,31.6569162607362));
#62835=CARTESIAN_POINT('Origin',(32.2981269336259,1.42301610119356,31.657022065625));
#62836=CARTESIAN_POINT('',(32.2443210807037,1.58918938037886,31.6569162607362));
#62837=CARTESIAN_POINT('Origin',(32.1941463529162,1.57862858340189,31.6570432561866));
#62838=CARTESIAN_POINT('Origin',(30.,-1.32966554433622E-14,31.6569162607362));
#62839=CARTESIAN_POINT('Origin',(30.,-1.32966554433622E-14,31.6569162607362));
#62840=CARTESIAN_POINT('',(32.2049422706078,1.64338966264455,31.6569162607362));
#62841=CARTESIAN_POINT('Origin',(32.1793940187453,1.59893837854221,31.6570220656245));
#62842=CARTESIAN_POINT('',(32.1127162260913,1.76037784239925,31.6569162607362));
#62843=CARTESIAN_POINT('Origin',(32.0635247608241,1.74591293706383,31.6570432561872));
#62844=CARTESIAN_POINT('Origin',(30.,-1.32966554433622E-14,31.6569162607362));
#62845=CARTESIAN_POINT('Origin',(30.,-1.32966554433622E-14,31.6569162607362));
#62846=CARTESIAN_POINT('',(32.0692063025902,1.81132141745218,31.6569162607362));
#62847=CARTESIAN_POINT('Origin',(32.0472244150162,1.76500266908448,31.6570220656248));
#62848=CARTESIAN_POINT('',(31.9680857733957,1.92071298963621,31.6569162607362));
#62849=CARTESIAN_POINT('Origin',(31.9201808523931,1.90243315689474,31.6570432561866));
#62850=CARTESIAN_POINT('Origin',(30.,-1.32966554433622E-14,31.6569162607362));
#62851=CARTESIAN_POINT('Origin',(30.,-1.32966554433622E-14,31.6569162607362));
#62852=CARTESIAN_POINT('',(31.9207129896362,1.96808577339572,31.6569162607362));
#62853=CARTESIAN_POINT('Origin',(31.9024329919958,1.92018513124459,31.657022065627));
#62854=CARTESIAN_POINT('',(31.8113214174522,2.06920630259018,31.6569162607362));
#62855=CARTESIAN_POINT('Origin',(31.7649983904793,2.04722424368911,31.6570432561871));
#62856=CARTESIAN_POINT('Origin',(30.,-1.32966554433622E-14,31.6569162607362));
#62857=CARTESIAN_POINT('Origin',(30.,-1.32966554433622E-14,31.6569162607362));
#62858=CARTESIAN_POINT('',(31.7603778423992,2.11271622609134,31.6569162607362));
#62859=CARTESIAN_POINT('Origin',(31.7459124369604,2.06352901355459,31.6570220656248));
#62860=CARTESIAN_POINT('',(31.6433896626445,2.20494227060776,31.6569162607362));
#62861=CARTESIAN_POINT('Origin',(31.5989341265682,2.17939351225069,31.657043256187));
#62862=CARTESIAN_POINT('Origin',(30.,-1.32966554433622E-14,31.6569162607362));
#62863=CARTESIAN_POINT('Origin',(30.,-1.32966554433622E-14,31.6569162607362));
#62864=CARTESIAN_POINT('',(31.5891893803789,2.24432108070368,31.6569162607362));
#62865=CARTESIAN_POINT('Origin',(31.5786277511742,2.19415055329685,31.6570220656251));
#62866=CARTESIAN_POINT('',(31.4653258640842,2.32708403630934,31.6569162607362));
#62867=CARTESIAN_POINT('Origin',(31.4230119020666,2.29812609508688,31.6570432561872));
#62868=CARTESIAN_POINT('Origin',(30.,-1.32966554433622E-14,31.6569162607362));
#62869=CARTESIAN_POINT('Origin',(30.,-1.32966554433622E-14,31.6569162607362));
#62870=CARTESIAN_POINT('',(31.4082030373693,2.36208894954099,31.6569162607362));
#62871=CARTESIAN_POINT('Origin',(31.4016103003533,2.31124442523252,31.6570220656319));
#62872=CARTESIAN_POINT('',(31.2782278443015,2.4348785550931,31.6569162607362));
#62873=CARTESIAN_POINT('Origin',(31.2383163359906,2.4026899663434,31.6570432561867));
#62874=CARTESIAN_POINT('Origin',(30.,-1.32966554433622E-14,31.6569162607362));
#62875=CARTESIAN_POINT('Origin',(30.,-1.32966554433622E-14,31.6569162607362));
#62876=CARTESIAN_POINT('',(31.2185346543594,2.46529375453009,31.6569162607362));
#62877=CARTESIAN_POINT('Origin',(31.215951455952,2.4140887067551,31.6570220656248));
#62878=CARTESIAN_POINT('',(31.0832491248047,2.52766123790544,31.6569162607362));
#62879=CARTESIAN_POINT('Origin',(31.045986137919,2.49244045498011,31.6570432561873));
#62880=CARTESIAN_POINT('Origin',(30.,-1.32966554433622E-14,31.6569162607362));
#62881=CARTESIAN_POINT('Origin',(30.,-1.32966554433622E-14,31.6569162607362));
#62882=CARTESIAN_POINT('',(31.0213536000015,2.55329920372915,31.6569162607362));
#62883=CARTESIAN_POINT('Origin',(31.0227958664779,2.50204932861496,31.6570220656254));
#62884=CARTESIAN_POINT('',(30.8815918142367,2.60486004865343,31.6569162607362));
#62885=CARTESIAN_POINT('Origin',(30.8472070874836,2.56682421939316,31.6570432561869));
#62886=CARTESIAN_POINT('Origin',(30.,-1.32966554433622E-14,31.6569162607362));
#62887=CARTESIAN_POINT('Origin',(30.,-1.32966554433622E-14,31.6569162607362));
#62888=CARTESIAN_POINT('',(30.817875561065,2.62556271427908,31.6569162607362));
#62889=CARTESIAN_POINT('Origin',(30.8233344003728,2.5745839843498,31.6570220656254));
#62890=CARTESIAN_POINT('',(30.6744991969749,2.6659990309976,31.6569162607362));
#62891=CARTESIAN_POINT('Origin',(30.6432047236281,2.62538265893739,31.6570432561868));
#62892=CARTESIAN_POINT('Origin',(30.,-1.32966554433622E-14,31.6569162607362));
#62893=CARTESIAN_POINT('Origin',(30.,-1.32966554433622E-14,31.6569162607362));
#62894=CARTESIAN_POINT('',(30.6093550473233,2.68163875760728,31.6569162607362));
#62895=CARTESIAN_POINT('Origin',(30.6187968039028,2.63124547368537,31.6570220656252));
#62896=CARTESIAN_POINT('',(30.4632480678699,2.71070124278104,31.6569162607362));
#62897=CARTESIAN_POINT('Origin',(30.4352367887645,2.66775474136143,31.6570432561865));
#62898=CARTESIAN_POINT('Origin',(30.,-1.32966554433622E-14,31.6569162607362));
#62899=CARTESIAN_POINT('Origin',(30.,-1.32966554433622E-14,31.6569162607362));
#62900=CARTESIAN_POINT('',(27.5651214449069,1.27822784430151,31.6569162607362));
#62901=CARTESIAN_POINT('Origin',(27.5973100336575,1.23831633598946,31.6570432561873));
#62902=CARTESIAN_POINT('',(27.637911050459,1.40820303736937,31.6569162607362));
#62903=CARTESIAN_POINT('Origin',(30.,-1.32966554433622E-14,31.6569162607362));
#62904=CARTESIAN_POINT('Origin',(27.6887555747495,1.40161030035545,31.6570220656248));
#62905=CARTESIAN_POINT('Origin',(30.,-1.32966554433622E-14,31.6569162607362));
#62906=CARTESIAN_POINT('',(27.6729159636906,1.46532586408423,31.6569162607362));
#62907=CARTESIAN_POINT('Origin',(27.7018739049127,1.42301190206727,31.6570432561868));
#62908=CARTESIAN_POINT('',(27.7556789192963,1.58918938037889,31.6569162607362));
#62909=CARTESIAN_POINT('Origin',(30.,-1.32966554433622E-14,31.6569162607362));
#62910=CARTESIAN_POINT('Origin',(27.805849446702,1.5786277511745,31.6570220656247));
#62911=CARTESIAN_POINT('Origin',(30.,-1.32966554433622E-14,31.6569162607362));
#62912=CARTESIAN_POINT('',(27.7950577293922,1.64338966264458,31.6569162607362));
#62913=CARTESIAN_POINT('Origin',(27.8206064877494,1.59893412656804,31.6570432561871));
#62914=CARTESIAN_POINT('',(27.8872837739086,1.76037784239928,31.6569162607362));
#62915=CARTESIAN_POINT('Origin',(30.,-1.32966554433622E-14,31.6569162607362));
#62916=CARTESIAN_POINT('Origin',(27.936470986445,1.74591243696058,31.6570220656246));
#62917=CARTESIAN_POINT('Origin',(30.,-1.32966554433622E-14,31.6569162607362));
#62918=CARTESIAN_POINT('',(27.9307936974098,1.81132141745221,31.6569162607362));
#62919=CARTESIAN_POINT('Origin',(27.9527757563104,1.76499839048029,31.6570432561867));
#62920=CARTESIAN_POINT('',(28.0319142266043,1.92071298963623,31.6569162607362));
#62921=CARTESIAN_POINT('Origin',(30.,-1.32966554433622E-14,31.6569162607362));
#62922=CARTESIAN_POINT('Origin',(28.0798148687497,1.90243299199796,31.6570220656246));
#62923=CARTESIAN_POINT('Origin',(30.,-1.32966554433622E-14,31.6569162607362));
#62924=CARTESIAN_POINT('',(28.0792870103638,1.96808577339574,31.6569162607362));
#62925=CARTESIAN_POINT('Origin',(28.0975668431059,1.92018085239124,31.6570432561874));
#62926=CARTESIAN_POINT('',(28.1886785825478,2.0692063025902,31.6569162607362));
#62927=CARTESIAN_POINT('Origin',(30.,-1.32966554433622E-14,31.6569162607362));
#62928=CARTESIAN_POINT('Origin',(28.2349973309159,2.04722441501599,31.657022065625));
#62929=CARTESIAN_POINT('Origin',(30.,-1.32966554433622E-14,31.6569162607362));
#62930=CARTESIAN_POINT('',(28.2396221576007,2.11271622609137,31.6569162607362));
#62931=CARTESIAN_POINT('Origin',(28.2540870629359,2.06352476082518,31.6570432561869));
#62932=CARTESIAN_POINT('',(28.3566103373554,2.20494227060779,31.6569162607362));
#62933=CARTESIAN_POINT('Origin',(30.,-1.32966554433622E-14,31.6569162607362));
#62934=CARTESIAN_POINT('Origin',(28.4010616214895,2.17939401872761,31.6570220656385));
#62935=CARTESIAN_POINT('Origin',(30.,-1.32966554433622E-14,31.6569162607362));
#62936=CARTESIAN_POINT('',(28.4108106196211,2.2443210807037,31.6569162607362));
#62937=CARTESIAN_POINT('Origin',(28.4213714165984,2.19414635291463,31.6570432561873));
#62938=CARTESIAN_POINT('',(28.5346741359158,2.32708403630936,31.6569162607362));
#62939=CARTESIAN_POINT('Origin',(30.,-1.32966554433622E-14,31.6569162607362));
#62940=CARTESIAN_POINT('Origin',(28.5769838988101,2.29812693362349,31.6570220656266));
#62941=CARTESIAN_POINT('Origin',(30.,-1.32966554433622E-14,31.6569162607362));
#62942=CARTESIAN_POINT('',(28.5917969626306,2.36208894954101,31.6569162607362));
#62943=CARTESIAN_POINT('Origin',(28.5983885404246,2.31124030311217,31.6570432561871));
#62944=CARTESIAN_POINT('',(28.7217721556985,2.43487855509312,31.6569162607362));
#62945=CARTESIAN_POINT('Origin',(30.,-1.32966554433622E-14,31.6569162607362));
#62946=CARTESIAN_POINT('Origin',(28.7616795436181,2.40269113175706,31.6570220656245));
#62947=CARTESIAN_POINT('Origin',(30.,-1.32966554433622E-14,31.6569162607362));
#62948=CARTESIAN_POINT('',(28.7814653456406,2.46529375453011,31.6569162607362));
#62949=CARTESIAN_POINT('Origin',(28.7840470649822,2.41408468827519,31.6570432561871));
#62950=CARTESIAN_POINT('',(28.9167508751953,2.52766123790545,31.6569162607362));
#62951=CARTESIAN_POINT('Origin',(30.,-1.32966554433622E-14,31.6569162607362));
#62952=CARTESIAN_POINT('Origin',(28.9540098458282,2.49244194008388,31.6570220656249));
#62953=CARTESIAN_POINT('Origin',(30.,-1.32966554433622E-14,31.6569162607362));
#62954=CARTESIAN_POINT('',(28.9786463999985,2.55329920372917,31.6569162607362));
#62955=CARTESIAN_POINT('Origin',(28.9772023437296,2.50204543857058,31.657043256187));
#62956=CARTESIAN_POINT('',(29.1184081857633,2.60486004865344,31.6569162607362));
#62957=CARTESIAN_POINT('Origin',(30.,-1.32966554433622E-14,31.6569162607362));
#62958=CARTESIAN_POINT('Origin',(29.1527890251647,2.56682601503002,31.6570220656247));
#62959=CARTESIAN_POINT('Origin',(30.,-1.32966554433622E-14,31.6569162607362));
#62960=CARTESIAN_POINT('',(29.182124438935,2.62556271427909,31.6569162607362));
#62961=CARTESIAN_POINT('Origin',(29.1766635101426,2.57458024672254,31.657043256187));
#62962=CARTESIAN_POINT('',(29.3255008030251,2.66599903099761,31.6569162607362));
#62963=CARTESIAN_POINT('Origin',(30.,-1.32966554433622E-14,31.6569162607362));
#62964=CARTESIAN_POINT('Origin',(29.356791541893,2.62538475403008,31.657022065628));
#62965=CARTESIAN_POINT('Origin',(30.,-1.32966554433622E-14,31.6569162607362));
#62966=CARTESIAN_POINT('',(29.3906449526767,2.68163875760729,31.6569162607362));
#62967=CARTESIAN_POINT('Origin',(29.3812008198028,2.6312419115181,31.6570432561872));
#62968=CARTESIAN_POINT('',(29.5367519321301,2.71070124278105,31.6569162607362));
#62969=CARTESIAN_POINT('Origin',(30.,-1.32966554433622E-14,31.6569162607362));
#62970=CARTESIAN_POINT('Origin',(29.5647596526443,2.66775712300484,31.6570220656252));
#62971=CARTESIAN_POINT('Origin',(30.,-1.32966554433622E-14,31.6569162607362));
#62972=CARTESIAN_POINT('',(29.6029223429162,2.72118160625946,31.6569162607362));
#62973=CARTESIAN_POINT('Origin',(29.5895532321803,2.67168109495224,31.6570432561874));
#62974=CARTESIAN_POINT('',(29.750859139619,2.7386910800031,31.6569162607362));
#62975=CARTESIAN_POINT('Origin',(30.,-1.32966554433622E-14,31.6569162607362));
#62976=CARTESIAN_POINT('Origin',(29.7754111648735,2.69368188219135,31.6570220656252));
#62977=CARTESIAN_POINT('Origin',(30.,-1.32966554433622E-14,31.6569162607362));
#62978=CARTESIAN_POINT('',(29.8176478489534,2.74394746542433,31.6569162607362));
#62979=CARTESIAN_POINT('Origin',(29.8004361853695,2.6956484760142,31.6570432561868));
#62980=CARTESIAN_POINT('',(29.9665023833599,2.74979597600974,31.6569162607362));
#62981=CARTESIAN_POINT('Origin',(30.,-1.32966554433622E-14,31.6569162607362));
#62982=CARTESIAN_POINT('Origin',(29.9874473419551,2.70299919683309,31.6570220656256));
#62983=CARTESIAN_POINT('Origin',(30.,-1.32966554433622E-14,31.6569162607362));
#62984=CARTESIAN_POINT('',(30.3970776570838,2.72118160625945,31.6569162607362));
#62985=CARTESIAN_POINT('Origin',(30.4104441193885,2.67168445961759,31.6570220656571));
#62986=CARTESIAN_POINT('',(30.249140860381,2.7386910800031,31.6569162607362));
#62987=CARTESIAN_POINT('Origin',(30.2245854743662,2.69367922868485,31.657043256187));
#62988=CARTESIAN_POINT('Origin',(30.,-1.32966554433622E-14,31.6569162607362));
#62989=CARTESIAN_POINT('Origin',(30.,-1.32966554433622E-14,16.));
#62990=CARTESIAN_POINT('',(27.4723387620945,1.08324912480478,33.8305837392638));
#62991=CARTESIAN_POINT('',(27.4723387620945,1.08324912480478,16.));
#62992=CARTESIAN_POINT('',(27.5347062454699,1.21853465435945,33.8305837392638));
#62993=CARTESIAN_POINT('Origin',(30.,-1.32966554433622E-14,33.8305837392638));
#62994=CARTESIAN_POINT('',(27.5347062454699,1.21853465435945,16.));
#62995=CARTESIAN_POINT('Origin',(30.,-1.32966554433622E-14,16.));
#62996=CARTESIAN_POINT('',(27.4467007962708,1.0213536000015,33.8305837392638));
#62997=CARTESIAN_POINT('',(27.4467007962708,1.0213536000015,16.));
#62998=CARTESIAN_POINT('',(27.3951399513465,0.881591814236741,33.8305837392638));
#62999=CARTESIAN_POINT('',(27.3951399513465,0.881591814236737,16.));
#63000=CARTESIAN_POINT('Origin',(30.,-1.32966554433622E-14,33.8305837392638));
#63001=CARTESIAN_POINT('Origin',(30.,-1.32966554433622E-14,16.));
#63002=CARTESIAN_POINT('',(27.3744372857209,0.817875561065013,33.8305837392638));
#63003=CARTESIAN_POINT('',(27.3744372857209,0.817875561065013,16.));
#63004=CARTESIAN_POINT('',(27.3340009690024,0.674499196974903,33.8305837392638));
#63005=CARTESIAN_POINT('',(27.3340009690024,0.674499196974899,16.));
#63006=CARTESIAN_POINT('Origin',(30.,-1.32966554433622E-14,33.8305837392638));
#63007=CARTESIAN_POINT('Origin',(30.,-1.32966554433622E-14,16.));
#63008=CARTESIAN_POINT('',(27.3183612423927,0.609355047323334,33.8305837392638));
#63009=CARTESIAN_POINT('',(27.3183612423927,0.609355047323335,16.));
#63010=CARTESIAN_POINT('',(27.2892987572189,0.463248067869974,33.8305837392638));
#63011=CARTESIAN_POINT('',(27.2892987572189,0.463248067869971,16.));
#63012=CARTESIAN_POINT('Origin',(30.,-1.32966554433622E-14,33.8305837392638));
#63013=CARTESIAN_POINT('Origin',(30.,-1.32966554433622E-14,16.));
#63014=CARTESIAN_POINT('',(27.2788183937405,0.397077657083793,33.8305837392638));
#63015=CARTESIAN_POINT('',(27.2788183937405,0.397077657083795,16.));
#63016=CARTESIAN_POINT('',(27.2613089199969,0.24914086038101,33.8305837392638));
#63017=CARTESIAN_POINT('',(27.2613089199969,0.249140860381007,16.));
#63018=CARTESIAN_POINT('Origin',(30.,-1.32966554433622E-14,33.8305837392638));
#63019=CARTESIAN_POINT('Origin',(30.,-1.32966554433622E-14,16.));
#63020=CARTESIAN_POINT('',(27.2560525345756,0.182352151046609,33.8305837392638));
#63021=CARTESIAN_POINT('',(27.2560525345756,0.182352151046611,16.));
#63022=CARTESIAN_POINT('',(27.2502040239902,0.0334976166400525,33.8305837392638));
#63023=CARTESIAN_POINT('',(27.2502040239902,0.0334976166400503,16.));
#63024=CARTESIAN_POINT('Origin',(30.,-1.32966554433622E-14,33.8305837392638));
#63025=CARTESIAN_POINT('Origin',(30.,-1.32966554433622E-14,16.));
#63026=CARTESIAN_POINT('',(27.2502040239902,-0.0334976166400219,33.8305837392638));
#63027=CARTESIAN_POINT('',(27.2502040239902,-0.0334976166400194,16.));
#63028=CARTESIAN_POINT('',(27.2560525345756,-0.182352151046578,33.8305837392638));
#63029=CARTESIAN_POINT('',(27.2560525345756,-0.18235215104658,16.));
#63030=CARTESIAN_POINT('Origin',(30.,-1.32966554433622E-14,33.8305837392638));
#63031=CARTESIAN_POINT('Origin',(30.,-1.32966554433622E-14,16.));
#63032=CARTESIAN_POINT('',(27.2613089199969,-0.249140860380979,33.8305837392638));
#63033=CARTESIAN_POINT('',(27.2613089199969,-0.249140860380976,16.));
#63034=CARTESIAN_POINT('',(27.2788183937405,-0.397077657083761,33.8305837392638));
#63035=CARTESIAN_POINT('',(27.2788183937405,-0.397077657083763,16.));
#63036=CARTESIAN_POINT('Origin',(30.,-1.32966554433622E-14,33.8305837392638));
#63037=CARTESIAN_POINT('Origin',(30.,-1.32966554433622E-14,16.));
#63038=CARTESIAN_POINT('',(27.2892987572189,-0.463248067869942,33.8305837392638));
#63039=CARTESIAN_POINT('',(27.2892987572189,-0.463248067869938,16.));
#63040=CARTESIAN_POINT('',(27.3183612423927,-0.609355047323305,33.8305837392638));
#63041=CARTESIAN_POINT('',(27.3183612423927,-0.609355047323306,16.));
#63042=CARTESIAN_POINT('Origin',(30.,-1.32966554433622E-14,33.8305837392638));
#63043=CARTESIAN_POINT('Origin',(30.,-1.32966554433622E-14,16.));
#63044=CARTESIAN_POINT('',(27.3340009690023,-0.674499196974875,33.8305837392638));
#63045=CARTESIAN_POINT('',(27.3340009690024,-0.674499196974871,16.));
#63046=CARTESIAN_POINT('',(27.3744372857209,-0.817875561064985,33.8305837392638));
#63047=CARTESIAN_POINT('',(27.3744372857209,-0.817875561064986,16.));
#63048=CARTESIAN_POINT('Origin',(30.,-1.32966554433622E-14,33.8305837392638));
#63049=CARTESIAN_POINT('Origin',(30.,-1.32966554433622E-14,16.));
#63050=CARTESIAN_POINT('',(27.3951399513465,-0.881591814236714,33.8305837392638));
#63051=CARTESIAN_POINT('',(27.3951399513465,-0.88159181423671,16.));
#63052=CARTESIAN_POINT('',(27.4467007962708,-1.02135360000148,33.8305837392638));
#63053=CARTESIAN_POINT('',(27.4467007962708,-1.02135360000148,16.));
#63054=CARTESIAN_POINT('Origin',(30.,-1.32966554433622E-14,33.8305837392638));
#63055=CARTESIAN_POINT('Origin',(30.,-1.32966554433622E-14,16.));
#63056=CARTESIAN_POINT('',(27.4723387620945,-1.08324912480476,33.8305837392638));
#63057=CARTESIAN_POINT('',(27.4723387620945,-1.08324912480475,16.));
#63058=CARTESIAN_POINT('',(27.5347062454699,-1.21853465435942,33.8305837392638));
#63059=CARTESIAN_POINT('',(27.5347062454699,-1.21853465435942,16.));
#63060=CARTESIAN_POINT('Origin',(30.,-1.32966554433622E-14,33.8305837392638));
#63061=CARTESIAN_POINT('Origin',(30.,-1.32966554433622E-14,16.));
#63062=CARTESIAN_POINT('',(27.5651214449068,-1.27822784430149,33.8305837392638));
#63063=CARTESIAN_POINT('',(27.5651214449068,-1.27822784430149,16.));
#63064=CARTESIAN_POINT('',(27.637911050459,-1.40820303736935,33.8305837392638));
#63065=CARTESIAN_POINT('',(27.637911050459,-1.40820303736935,16.));
#63066=CARTESIAN_POINT('Origin',(30.,-1.32966554433622E-14,33.8305837392638));
#63067=CARTESIAN_POINT('Origin',(30.,-1.32966554433622E-14,16.));
#63068=CARTESIAN_POINT('',(27.6729159636906,-1.46532586408422,33.8305837392638));
#63069=CARTESIAN_POINT('',(27.6729159636906,-1.46532586408421,16.));
#63070=CARTESIAN_POINT('',(27.7556789192963,-1.58918938037887,33.8305837392638));
#63071=CARTESIAN_POINT('',(27.7556789192963,-1.58918938037887,16.));
#63072=CARTESIAN_POINT('Origin',(30.,-1.32966554433622E-14,33.8305837392638));
#63073=CARTESIAN_POINT('Origin',(30.,-1.32966554433622E-14,16.));
#63074=CARTESIAN_POINT('',(27.7950577293922,-1.64338966264456,33.8305837392638));
#63075=CARTESIAN_POINT('',(27.7950577293922,-1.64338966264456,16.));
#63076=CARTESIAN_POINT('',(27.8872837739086,-1.76037784239926,33.8305837392638));
#63077=CARTESIAN_POINT('',(27.8872837739086,-1.76037784239926,16.));
#63078=CARTESIAN_POINT('Origin',(30.,-1.32966554433622E-14,33.8305837392638));
#63079=CARTESIAN_POINT('Origin',(30.,-1.32966554433622E-14,16.));
#63080=CARTESIAN_POINT('',(27.9307936974098,-1.81132141745219,33.8305837392638));
#63081=CARTESIAN_POINT('',(27.9307936974098,-1.81132141745219,16.));
#63082=CARTESIAN_POINT('',(28.0319142266042,-1.92071298963622,33.8305837392638));
#63083=CARTESIAN_POINT('',(28.0319142266042,-1.92071298963622,16.));
#63084=CARTESIAN_POINT('Origin',(30.,-1.32966554433622E-14,33.8305837392638));
#63085=CARTESIAN_POINT('Origin',(30.,-1.32966554433622E-14,16.));
#63086=CARTESIAN_POINT('',(28.0792870103637,-1.96808577339574,33.8305837392638));
#63087=CARTESIAN_POINT('',(28.0792870103637,-1.96808577339573,16.));
#63088=CARTESIAN_POINT('',(28.1886785825478,-2.06920630259019,33.8305837392638));
#63089=CARTESIAN_POINT('',(28.1886785825478,-2.06920630259019,16.));
#63090=CARTESIAN_POINT('Origin',(30.,-1.32966554433622E-14,33.8305837392638));
#63091=CARTESIAN_POINT('Origin',(30.,-1.32966554433622E-14,16.));
#63092=CARTESIAN_POINT('',(28.2396221576007,-2.11271622609136,33.8305837392638));
#63093=CARTESIAN_POINT('',(28.2396221576007,-2.11271622609136,16.));
#63094=CARTESIAN_POINT('',(28.3566103373554,-2.20494227060778,33.8305837392638));
#63095=CARTESIAN_POINT('',(28.3566103373554,-2.20494227060778,16.));
#63096=CARTESIAN_POINT('Origin',(30.,-1.32966554433622E-14,33.8305837392638));
#63097=CARTESIAN_POINT('Origin',(30.,-1.32966554433622E-14,16.));
#63098=CARTESIAN_POINT('',(28.4108106196211,-2.2443210807037,33.8305837392638));
#63099=CARTESIAN_POINT('',(28.4108106196211,-2.2443210807037,16.));
#63100=CARTESIAN_POINT('',(28.5346741359157,-2.32708403630936,33.8305837392638));
#63101=CARTESIAN_POINT('',(28.5346741359157,-2.32708403630936,16.));
#63102=CARTESIAN_POINT('Origin',(30.,-1.32966554433622E-14,33.8305837392638));
#63103=CARTESIAN_POINT('Origin',(30.,-1.32966554433622E-14,16.));
#63104=CARTESIAN_POINT('',(28.5917969626306,-2.36208894954101,33.8305837392638));
#63105=CARTESIAN_POINT('',(28.5917969626306,-2.362088949541,16.));
#63106=CARTESIAN_POINT('',(28.7217721556985,-2.43487855509313,33.8305837392638));
#63107=CARTESIAN_POINT('',(28.7217721556985,-2.43487855509312,16.));
#63108=CARTESIAN_POINT('Origin',(30.,-1.32966554433622E-14,33.8305837392638));
#63109=CARTESIAN_POINT('Origin',(30.,-1.32966554433622E-14,16.));
#63110=CARTESIAN_POINT('',(28.7814653456405,-2.46529375453011,33.8305837392638));
#63111=CARTESIAN_POINT('',(28.7814653456405,-2.46529375453011,16.));
#63112=CARTESIAN_POINT('',(28.9167508751952,-2.52766123790546,33.8305837392638));
#63113=CARTESIAN_POINT('',(28.9167508751952,-2.52766123790546,16.));
#63114=CARTESIAN_POINT('Origin',(30.,-1.32966554433622E-14,33.8305837392638));
#63115=CARTESIAN_POINT('Origin',(30.,-1.32966554433622E-14,16.));
#63116=CARTESIAN_POINT('',(28.9786463999985,-2.55329920372918,33.8305837392638));
#63117=CARTESIAN_POINT('',(28.9786463999985,-2.55329920372917,16.));
#63118=CARTESIAN_POINT('',(29.1184081857632,-2.60486004865345,33.8305837392638));
#63119=CARTESIAN_POINT('',(29.1184081857632,-2.60486004865345,16.));
#63120=CARTESIAN_POINT('Origin',(30.,-1.32966554433622E-14,33.8305837392638));
#63121=CARTESIAN_POINT('Origin',(30.,-1.32966554433622E-14,16.));
#63122=CARTESIAN_POINT('',(29.182124438935,-2.62556271427911,33.8305837392638));
#63123=CARTESIAN_POINT('',(29.182124438935,-2.6255627142791,16.));
#63124=CARTESIAN_POINT('',(29.3255008030251,-2.66599903099763,33.8305837392638));
#63125=CARTESIAN_POINT('',(29.3255008030251,-2.66599903099763,16.));
#63126=CARTESIAN_POINT('Origin',(30.,-1.32966554433622E-14,33.8305837392638));
#63127=CARTESIAN_POINT('Origin',(30.,-1.32966554433622E-14,16.));
#63128=CARTESIAN_POINT('',(29.3906449526766,-2.68163875760731,33.8305837392638));
#63129=CARTESIAN_POINT('',(29.3906449526766,-2.6816387576073,16.));
#63130=CARTESIAN_POINT('',(29.53675193213,-2.71070124278107,33.8305837392638));
#63131=CARTESIAN_POINT('',(29.53675193213,-2.71070124278106,16.));
#63132=CARTESIAN_POINT('Origin',(30.,-1.32966554433622E-14,33.8305837392638));
#63133=CARTESIAN_POINT('Origin',(30.,-1.32966554433622E-14,16.));
#63134=CARTESIAN_POINT('',(29.6029223429162,-2.72118160625948,33.8305837392638));
#63135=CARTESIAN_POINT('',(29.6029223429162,-2.72118160625948,16.));
#63136=CARTESIAN_POINT('',(29.750859139619,-2.73869108000313,33.8305837392638));
#63137=CARTESIAN_POINT('',(29.750859139619,-2.73869108000313,16.));
#63138=CARTESIAN_POINT('Origin',(30.,-1.32966554433622E-14,33.8305837392638));
#63139=CARTESIAN_POINT('Origin',(30.,-1.32966554433622E-14,16.));
#63140=CARTESIAN_POINT('',(29.8176478489534,-2.74394746542436,33.8305837392638));
#63141=CARTESIAN_POINT('',(29.8176478489534,-2.74394746542436,16.));
#63142=CARTESIAN_POINT('',(29.9665023833599,-2.74979597600977,33.8305837392638));
#63143=CARTESIAN_POINT('',(29.9665023833599,-2.74979597600977,16.));
#63144=CARTESIAN_POINT('Origin',(30.,-1.32966554433622E-14,33.8305837392638));
#63145=CARTESIAN_POINT('Origin',(30.,-1.32966554433622E-14,16.));
#63146=CARTESIAN_POINT('',(30.03349761664,-2.74979597600977,33.8305837392638));
#63147=CARTESIAN_POINT('',(30.03349761664,-2.74979597600977,16.));
#63148=CARTESIAN_POINT('',(30.1823521510466,-2.74394746542436,33.8305837392638));
#63149=CARTESIAN_POINT('',(30.1823521510466,-2.74394746542436,16.));
#63150=CARTESIAN_POINT('Origin',(30.,-1.32966554433622E-14,33.8305837392638));
#63151=CARTESIAN_POINT('Origin',(30.,-1.32966554433622E-14,16.));
#63152=CARTESIAN_POINT('',(30.249140860381,-2.73869108000313,33.8305837392638));
#63153=CARTESIAN_POINT('',(30.2491408603809,-2.73869108000313,16.));
#63154=CARTESIAN_POINT('',(30.3970776570837,-2.72118160625949,33.8305837392638));
#63155=CARTESIAN_POINT('',(30.3970776570837,-2.72118160625948,16.));
#63156=CARTESIAN_POINT('Origin',(30.,-1.32966554433622E-14,33.8305837392638));
#63157=CARTESIAN_POINT('Origin',(30.,-1.32966554433622E-14,16.));
#63158=CARTESIAN_POINT('',(30.4632480678699,-2.71070124278108,33.8305837392638));
#63159=CARTESIAN_POINT('',(30.4632480678699,-2.71070124278107,16.));
#63160=CARTESIAN_POINT('',(30.6093550473233,-2.68163875760732,33.8305837392638));
#63161=CARTESIAN_POINT('',(30.6093550473233,-2.68163875760731,16.));
#63162=CARTESIAN_POINT('Origin',(30.,-1.32966554433622E-14,33.8305837392638));
#63163=CARTESIAN_POINT('Origin',(30.,-1.32966554433622E-14,16.));
#63164=CARTESIAN_POINT('',(30.6744991969748,-2.66599903099764,33.8305837392638));
#63165=CARTESIAN_POINT('',(30.6744991969748,-2.66599903099764,16.));
#63166=CARTESIAN_POINT('',(30.817875561065,-2.62556271427912,33.8305837392638));
#63167=CARTESIAN_POINT('',(30.817875561065,-2.62556271427912,16.));
#63168=CARTESIAN_POINT('Origin',(30.,-1.32966554433622E-14,33.8305837392638));
#63169=CARTESIAN_POINT('Origin',(30.,-1.32966554433622E-14,16.));
#63170=CARTESIAN_POINT('',(30.8815918142367,-2.60486004865346,33.8305837392638));
#63171=CARTESIAN_POINT('',(30.8815918142367,-2.60486004865346,16.));
#63172=CARTESIAN_POINT('',(31.0213536000014,-2.55329920372919,33.8305837392638));
#63173=CARTESIAN_POINT('',(31.0213536000014,-2.55329920372919,16.));
#63174=CARTESIAN_POINT('Origin',(30.,-1.32966554433622E-14,33.8305837392638));
#63175=CARTESIAN_POINT('Origin',(30.,-1.32966554433622E-14,16.));
#63176=CARTESIAN_POINT('',(31.0832491248047,-2.52766123790547,33.8305837392638));
#63177=CARTESIAN_POINT('',(31.0832491248047,-2.52766123790547,16.));
#63178=CARTESIAN_POINT('',(31.2185346543594,-2.46529375453013,33.8305837392638));
#63179=CARTESIAN_POINT('',(31.2185346543594,-2.46529375453013,16.));
#63180=CARTESIAN_POINT('Origin',(30.,-1.32966554433622E-14,33.8305837392638));
#63181=CARTESIAN_POINT('Origin',(30.,-1.32966554433622E-14,16.));
#63182=CARTESIAN_POINT('',(31.2782278443015,-2.43487855509314,33.8305837392638));
#63183=CARTESIAN_POINT('',(31.2782278443015,-2.43487855509314,16.));
#63184=CARTESIAN_POINT('',(31.4082030373693,-2.36208894954103,33.8305837392638));
#63185=CARTESIAN_POINT('',(31.4082030373693,-2.36208894954102,16.));
#63186=CARTESIAN_POINT('Origin',(30.,-1.32966554433622E-14,33.8305837392638));
#63187=CARTESIAN_POINT('Origin',(30.,-1.32966554433622E-14,16.));
#63188=CARTESIAN_POINT('',(31.4653258640842,-2.32708403630938,33.8305837392638));
#63189=CARTESIAN_POINT('',(31.4653258640842,-2.32708403630938,16.));
#63190=CARTESIAN_POINT('',(31.5891893803788,-2.24432108070372,33.8305837392638));
#63191=CARTESIAN_POINT('',(31.5891893803788,-2.24432108070372,16.));
#63192=CARTESIAN_POINT('Origin',(30.,-1.32966554433622E-14,33.8305837392638));
#63193=CARTESIAN_POINT('Origin',(30.,-1.32966554433622E-14,16.));
#63194=CARTESIAN_POINT('',(31.6433896626445,-2.2049422706078,33.8305837392638));
#63195=CARTESIAN_POINT('',(31.6433896626445,-2.2049422706078,16.));
#63196=CARTESIAN_POINT('',(31.7603778423992,-2.11271622609139,33.8305837392638));
#63197=CARTESIAN_POINT('',(31.7603778423992,-2.11271622609138,16.));
#63198=CARTESIAN_POINT('Origin',(30.,-1.32966554433622E-14,33.8305837392638));
#63199=CARTESIAN_POINT('Origin',(30.,-1.32966554433622E-14,16.));
#63200=CARTESIAN_POINT('',(31.8113214174522,-2.06920630259022,33.8305837392638));
#63201=CARTESIAN_POINT('',(31.8113214174522,-2.06920630259022,16.));
#63202=CARTESIAN_POINT('',(31.9207129896362,-1.96808577339576,33.8305837392638));
#63203=CARTESIAN_POINT('',(31.9207129896362,-1.96808577339576,16.));
#63204=CARTESIAN_POINT('Origin',(30.,-1.32966554433622E-14,33.8305837392638));
#63205=CARTESIAN_POINT('Origin',(30.,-1.32966554433622E-14,16.));
#63206=CARTESIAN_POINT('',(31.9680857733957,-1.92071298963625,33.8305837392638));
#63207=CARTESIAN_POINT('',(31.9680857733957,-1.92071298963625,16.));
#63208=CARTESIAN_POINT('',(32.0692063025902,-1.81132141745222,33.8305837392638));
#63209=CARTESIAN_POINT('',(32.0692063025902,-1.81132141745222,16.));
#63210=CARTESIAN_POINT('Origin',(30.,-1.32966554433622E-14,33.8305837392638));
#63211=CARTESIAN_POINT('Origin',(30.,-1.32966554433622E-14,16.));
#63212=CARTESIAN_POINT('',(32.1127162260913,-1.76037784239929,33.8305837392638));
#63213=CARTESIAN_POINT('',(32.1127162260913,-1.76037784239929,16.));
#63214=CARTESIAN_POINT('',(32.2049422706078,-1.6433896626446,33.8305837392638));
#63215=CARTESIAN_POINT('',(32.2049422706077,-1.64338966264459,16.));
#63216=CARTESIAN_POINT('Origin',(30.,-1.32966554433622E-14,33.8305837392638));
#63217=CARTESIAN_POINT('Origin',(30.,-1.32966554433622E-14,16.));
#63218=CARTESIAN_POINT('',(32.2443210807037,-1.5891893803789,33.8305837392638));
#63219=CARTESIAN_POINT('',(32.2443210807037,-1.5891893803789,16.));
#63220=CARTESIAN_POINT('',(32.3270840363093,-1.46532586408425,33.8305837392638));
#63221=CARTESIAN_POINT('',(32.3270840363093,-1.46532586408424,16.));
#63222=CARTESIAN_POINT('Origin',(30.,-1.32966554433622E-14,33.8305837392638));
#63223=CARTESIAN_POINT('Origin',(30.,-1.32966554433622E-14,16.));
#63224=CARTESIAN_POINT('',(32.362088949541,-1.40820303736938,33.8305837392638));
#63225=CARTESIAN_POINT('',(32.362088949541,-1.40820303736938,16.));
#63226=CARTESIAN_POINT('',(32.4348785550931,-1.27822784430152,33.8305837392638));
#63227=CARTESIAN_POINT('',(32.4348785550931,-1.27822784430152,16.));
#63228=CARTESIAN_POINT('Origin',(30.,-1.32966554433622E-14,33.8305837392638));
#63229=CARTESIAN_POINT('Origin',(30.,-1.32966554433622E-14,16.));
#63230=CARTESIAN_POINT('',(32.4652937545301,-1.21853465435946,33.8305837392638));
#63231=CARTESIAN_POINT('',(32.4652937545301,-1.21853465435946,16.));
#63232=CARTESIAN_POINT('',(32.5276612379054,-1.08324912480479,33.8305837392638));
#63233=CARTESIAN_POINT('',(32.5276612379054,-1.08324912480479,16.));
#63234=CARTESIAN_POINT('Origin',(30.,-1.32966554433622E-14,33.8305837392638));
#63235=CARTESIAN_POINT('Origin',(30.,-1.32966554433622E-14,16.));
#63236=CARTESIAN_POINT('',(32.5532992037291,-1.02135360000151,33.8305837392638));
#63237=CARTESIAN_POINT('',(32.5532992037291,-1.02135360000151,16.));
#63238=CARTESIAN_POINT('',(32.6048600486534,-0.88159181423675,33.8305837392638));
#63239=CARTESIAN_POINT('',(32.6048600486534,-0.881591814236746,16.));
#63240=CARTESIAN_POINT('Origin',(30.,-1.32966554433622E-14,33.8305837392638));
#63241=CARTESIAN_POINT('Origin',(30.,-1.32966554433622E-14,16.));
#63242=CARTESIAN_POINT('',(32.6255627142791,-0.817875561065022,33.8305837392638));
#63243=CARTESIAN_POINT('',(32.6255627142791,-0.817875561065022,16.));
#63244=CARTESIAN_POINT('',(32.6659990309976,-0.674499196974912,33.8305837392638));
#63245=CARTESIAN_POINT('',(32.6659990309976,-0.674499196974908,16.));
#63246=CARTESIAN_POINT('Origin',(30.,-1.32966554433622E-14,33.8305837392638));
#63247=CARTESIAN_POINT('Origin',(30.,-1.32966554433622E-14,16.));
#63248=CARTESIAN_POINT('',(32.6816387576073,-0.609355047323342,33.8305837392638));
#63249=CARTESIAN_POINT('',(32.6816387576073,-0.609355047323343,16.));
#63250=CARTESIAN_POINT('',(32.710701242781,-0.463248067869981,33.8305837392638));
#63251=CARTESIAN_POINT('',(32.710701242781,-0.463248067869977,16.));
#63252=CARTESIAN_POINT('Origin',(30.,-1.32966554433622E-14,33.8305837392638));
#63253=CARTESIAN_POINT('Origin',(30.,-1.32966554433622E-14,16.));
#63254=CARTESIAN_POINT('',(32.7211816062594,-0.3970776570838,33.8305837392638));
#63255=CARTESIAN_POINT('',(32.7211816062594,-0.397077657083801,16.));
#63256=CARTESIAN_POINT('',(32.7386910800031,-0.249140860381016,33.8305837392638));
#63257=CARTESIAN_POINT('',(32.7386910800031,-0.249140860381013,16.));
#63258=CARTESIAN_POINT('Origin',(30.,-1.32966554433622E-14,33.8305837392638));
#63259=CARTESIAN_POINT('Origin',(30.,-1.32966554433622E-14,16.));
#63260=CARTESIAN_POINT('',(32.7439474654243,-0.182352151046616,33.8305837392638));
#63261=CARTESIAN_POINT('',(32.7439474654243,-0.182352151046618,16.));
#63262=CARTESIAN_POINT('',(32.7497959760097,-0.03349761664006,33.8305837392638));
#63263=CARTESIAN_POINT('',(32.7497959760097,-0.0334976166400576,16.));
#63264=CARTESIAN_POINT('Origin',(30.,-1.32966554433622E-14,33.8305837392638));
#63265=CARTESIAN_POINT('Origin',(30.,-1.32966554433622E-14,16.));
#63266=CARTESIAN_POINT('',(32.7497959760097,0.0334976166400146,33.8305837392638));
#63267=CARTESIAN_POINT('',(32.7497959760097,0.0334976166400122,16.));
#63268=CARTESIAN_POINT('',(32.7439474654243,0.18235215104657,33.8305837392638));
#63269=CARTESIAN_POINT('',(32.7439474654243,0.182352151046572,16.));
#63270=CARTESIAN_POINT('Origin',(30.,-1.32966554433622E-14,33.8305837392638));
#63271=CARTESIAN_POINT('Origin',(30.,-1.32966554433622E-14,16.));
#63272=CARTESIAN_POINT('',(32.7386910800031,0.249140860380971,33.8305837392638));
#63273=CARTESIAN_POINT('',(32.7386910800031,0.249140860380968,16.));
#63274=CARTESIAN_POINT('',(32.7211816062594,0.397077657083754,33.8305837392638));
#63275=CARTESIAN_POINT('',(32.7211816062594,0.397077657083756,16.));
#63276=CARTESIAN_POINT('Origin',(30.,-1.32966554433622E-14,33.8305837392638));
#63277=CARTESIAN_POINT('Origin',(30.,-1.32966554433622E-14,16.));
#63278=CARTESIAN_POINT('',(32.710701242781,0.463248067869934,33.8305837392638));
#63279=CARTESIAN_POINT('',(32.710701242781,0.463248067869931,16.));
#63280=CARTESIAN_POINT('',(32.6816387576073,0.609355047323297,33.8305837392638));
#63281=CARTESIAN_POINT('',(32.6816387576073,0.609355047323298,16.));
#63282=CARTESIAN_POINT('Origin',(30.,-1.32966554433622E-14,33.8305837392638));
#63283=CARTESIAN_POINT('Origin',(30.,-1.32966554433622E-14,16.));
#63284=CARTESIAN_POINT('',(32.6659990309976,0.674499196974867,33.8305837392638));
#63285=CARTESIAN_POINT('',(32.6659990309976,0.674499196974863,16.));
#63286=CARTESIAN_POINT('',(32.6255627142791,0.817875561064977,33.8305837392638));
#63287=CARTESIAN_POINT('',(32.6255627142791,0.817875561064977,16.));
#63288=CARTESIAN_POINT('Origin',(30.,-1.32966554433622E-14,33.8305837392638));
#63289=CARTESIAN_POINT('Origin',(30.,-1.32966554433622E-14,16.));
#63290=CARTESIAN_POINT('',(32.6048600486534,0.881591814236705,33.8305837392638));
#63291=CARTESIAN_POINT('',(32.6048600486534,0.881591814236701,16.));
#63292=CARTESIAN_POINT('',(32.5532992037292,1.02135360000147,33.8305837392638));
#63293=CARTESIAN_POINT('',(32.5532992037291,1.02135360000147,16.));
#63294=CARTESIAN_POINT('Origin',(30.,-1.32966554433622E-14,33.8305837392638));
#63295=CARTESIAN_POINT('Origin',(30.,-1.32966554433622E-14,16.));
#63296=CARTESIAN_POINT('',(32.5276612379054,1.08324912480475,33.8305837392638));
#63297=CARTESIAN_POINT('',(32.5276612379054,1.08324912480474,16.));
#63298=CARTESIAN_POINT('',(32.4652937545301,1.21853465435941,33.8305837392638));
#63299=CARTESIAN_POINT('',(32.4652937545301,1.21853465435941,16.));
#63300=CARTESIAN_POINT('Origin',(30.,-1.32966554433622E-14,33.8305837392638));
#63301=CARTESIAN_POINT('Origin',(30.,-1.32966554433622E-14,16.));
#63302=CARTESIAN_POINT('',(32.4348785550931,1.27822784430148,33.8305837392638));
#63303=CARTESIAN_POINT('',(32.4348785550931,1.27822784430148,16.));
#63304=CARTESIAN_POINT('',(32.362088949541,1.40820303736934,33.8305837392638));
#63305=CARTESIAN_POINT('',(32.362088949541,1.40820303736934,16.));
#63306=CARTESIAN_POINT('Origin',(30.,-1.32966554433622E-14,33.8305837392638));
#63307=CARTESIAN_POINT('Origin',(30.,-1.32966554433622E-14,16.));
#63308=CARTESIAN_POINT('',(32.3270840363093,1.4653258640842,33.8305837392638));
#63309=CARTESIAN_POINT('',(32.3270840363093,1.4653258640842,16.));
#63310=CARTESIAN_POINT('',(32.2443210807037,1.58918938037886,33.8305837392638));
#63311=CARTESIAN_POINT('',(32.2443210807037,1.58918938037886,16.));
#63312=CARTESIAN_POINT('Origin',(30.,-1.32966554433622E-14,33.8305837392638));
#63313=CARTESIAN_POINT('Origin',(30.,-1.32966554433622E-14,16.));
#63314=CARTESIAN_POINT('',(32.2049422706078,1.64338966264455,33.8305837392638));
#63315=CARTESIAN_POINT('',(32.2049422706078,1.64338966264455,16.));
#63316=CARTESIAN_POINT('',(32.1127162260914,1.76037784239925,33.8305837392638));
#63317=CARTESIAN_POINT('',(32.1127162260913,1.76037784239925,16.));
#63318=CARTESIAN_POINT('Origin',(30.,-1.32966554433622E-14,33.8305837392638));
#63319=CARTESIAN_POINT('Origin',(30.,-1.32966554433622E-14,16.));
#63320=CARTESIAN_POINT('',(32.0692063025902,1.81132141745218,33.8305837392638));
#63321=CARTESIAN_POINT('',(32.0692063025902,1.81132141745218,16.));
#63322=CARTESIAN_POINT('',(31.9680857733957,1.92071298963621,33.8305837392638));
#63323=CARTESIAN_POINT('',(31.9680857733957,1.92071298963621,16.));
#63324=CARTESIAN_POINT('Origin',(30.,-1.32966554433622E-14,33.8305837392638));
#63325=CARTESIAN_POINT('Origin',(30.,-1.32966554433622E-14,16.));
#63326=CARTESIAN_POINT('',(31.9207129896362,1.96808577339572,33.8305837392638));
#63327=CARTESIAN_POINT('',(31.9207129896362,1.96808577339572,16.));
#63328=CARTESIAN_POINT('',(31.8113214174522,2.06920630259018,33.8305837392638));
#63329=CARTESIAN_POINT('',(31.8113214174522,2.06920630259018,16.));
#63330=CARTESIAN_POINT('Origin',(30.,-1.32966554433622E-14,33.8305837392638));
#63331=CARTESIAN_POINT('Origin',(30.,-1.32966554433622E-14,16.));
#63332=CARTESIAN_POINT('',(31.7603778423992,2.11271622609135,33.8305837392638));
#63333=CARTESIAN_POINT('',(31.7603778423992,2.11271622609134,16.));
#63334=CARTESIAN_POINT('',(31.6433896626446,2.20494227060777,33.8305837392638));
#63335=CARTESIAN_POINT('',(31.6433896626445,2.20494227060776,16.));
#63336=CARTESIAN_POINT('Origin',(30.,-1.32966554433622E-14,33.8305837392638));
#63337=CARTESIAN_POINT('Origin',(30.,-1.32966554433622E-14,16.));
#63338=CARTESIAN_POINT('',(31.5891893803789,2.24432108070369,33.8305837392638));
#63339=CARTESIAN_POINT('',(31.5891893803789,2.24432108070368,16.));
#63340=CARTESIAN_POINT('',(31.4653258640842,2.32708403630934,33.8305837392638));
#63341=CARTESIAN_POINT('',(31.4653258640842,2.32708403630934,16.));
#63342=CARTESIAN_POINT('Origin',(30.,-1.32966554433622E-14,33.8305837392638));
#63343=CARTESIAN_POINT('Origin',(30.,-1.32966554433622E-14,16.));
#63344=CARTESIAN_POINT('',(31.4082030373693,2.36208894954099,33.8305837392638));
#63345=CARTESIAN_POINT('',(31.4082030373693,2.36208894954099,16.));
#63346=CARTESIAN_POINT('',(31.2782278443015,2.43487855509311,33.8305837392638));
#63347=CARTESIAN_POINT('',(31.2782278443015,2.4348785550931,16.));
#63348=CARTESIAN_POINT('Origin',(30.,-1.32966554433622E-14,33.8305837392638));
#63349=CARTESIAN_POINT('Origin',(30.,-1.32966554433622E-14,16.));
#63350=CARTESIAN_POINT('',(31.2185346543594,2.4652937545301,33.8305837392638));
#63351=CARTESIAN_POINT('',(31.2185346543594,2.46529375453009,16.));
#63352=CARTESIAN_POINT('',(31.0832491248047,2.52766123790544,33.8305837392638));
#63353=CARTESIAN_POINT('',(31.0832491248047,2.52766123790544,16.));
#63354=CARTESIAN_POINT('Origin',(30.,-1.32966554433622E-14,33.8305837392638));
#63355=CARTESIAN_POINT('Origin',(30.,-1.32966554433622E-14,16.));
#63356=CARTESIAN_POINT('',(31.0213536000015,2.55329920372916,33.8305837392638));
#63357=CARTESIAN_POINT('',(31.0213536000015,2.55329920372915,16.));
#63358=CARTESIAN_POINT('',(30.8815918142367,2.60486004865343,33.8305837392638));
#63359=CARTESIAN_POINT('',(30.8815918142367,2.60486004865343,16.));
#63360=CARTESIAN_POINT('Origin',(30.,-1.32966554433622E-14,33.8305837392638));
#63361=CARTESIAN_POINT('Origin',(30.,-1.32966554433622E-14,16.));
#63362=CARTESIAN_POINT('',(30.817875561065,2.62556271427909,33.8305837392638));
#63363=CARTESIAN_POINT('',(30.817875561065,2.62556271427908,16.));
#63364=CARTESIAN_POINT('',(30.6744991969749,2.66599903099761,33.8305837392638));
#63365=CARTESIAN_POINT('',(30.6744991969749,2.6659990309976,16.));
#63366=CARTESIAN_POINT('Origin',(30.,-1.32966554433622E-14,33.8305837392638));
#63367=CARTESIAN_POINT('Origin',(30.,-1.32966554433622E-14,16.));
#63368=CARTESIAN_POINT('',(30.6093550473233,2.68163875760729,33.8305837392638));
#63369=CARTESIAN_POINT('',(30.6093550473233,2.68163875760728,16.));
#63370=CARTESIAN_POINT('',(30.4632480678699,2.71070124278105,33.8305837392638));
#63371=CARTESIAN_POINT('',(30.4632480678699,2.71070124278104,16.));
#63372=CARTESIAN_POINT('Origin',(30.,-1.32966554433622E-14,33.8305837392638));
#63373=CARTESIAN_POINT('Origin',(30.,-1.32966554433622E-14,16.));
#63374=CARTESIAN_POINT('',(27.5651214449069,1.27822784430151,33.8305837392638));
#63375=CARTESIAN_POINT('',(27.5651214449069,1.27822784430151,16.));
#63376=CARTESIAN_POINT('',(27.637911050459,1.40820303736937,33.8305837392638));
#63377=CARTESIAN_POINT('Origin',(30.,-1.32966554433622E-14,33.8305837392638));
#63378=CARTESIAN_POINT('',(27.637911050459,1.40820303736937,16.));
#63379=CARTESIAN_POINT('Origin',(30.,-1.32966554433622E-14,16.));
#63380=CARTESIAN_POINT('',(27.6729159636906,1.46532586408424,33.8305837392638));
#63381=CARTESIAN_POINT('',(27.6729159636906,1.46532586408423,16.));
#63382=CARTESIAN_POINT('',(27.7556789192963,1.58918938037889,33.8305837392638));
#63383=CARTESIAN_POINT('Origin',(30.,-1.32966554433622E-14,33.8305837392638));
#63384=CARTESIAN_POINT('',(27.7556789192963,1.58918938037889,16.));
#63385=CARTESIAN_POINT('Origin',(30.,-1.32966554433622E-14,16.));
#63386=CARTESIAN_POINT('',(27.7950577293922,1.64338966264458,33.8305837392638));
#63387=CARTESIAN_POINT('',(27.7950577293922,1.64338966264458,16.));
#63388=CARTESIAN_POINT('',(27.8872837739086,1.76037784239928,33.8305837392638));
#63389=CARTESIAN_POINT('Origin',(30.,-1.32966554433622E-14,33.8305837392638));
#63390=CARTESIAN_POINT('',(27.8872837739086,1.76037784239928,16.));
#63391=CARTESIAN_POINT('Origin',(30.,-1.32966554433622E-14,16.));
#63392=CARTESIAN_POINT('',(27.9307936974098,1.81132141745221,33.8305837392638));
#63393=CARTESIAN_POINT('',(27.9307936974098,1.81132141745221,16.));
#63394=CARTESIAN_POINT('',(28.0319142266043,1.92071298963624,33.8305837392638));
#63395=CARTESIAN_POINT('Origin',(30.,-1.32966554433622E-14,33.8305837392638));
#63396=CARTESIAN_POINT('',(28.0319142266043,1.92071298963623,16.));
#63397=CARTESIAN_POINT('Origin',(30.,-1.32966554433622E-14,16.));
#63398=CARTESIAN_POINT('',(28.0792870103638,1.96808577339575,33.8305837392638));
#63399=CARTESIAN_POINT('',(28.0792870103638,1.96808577339574,16.));
#63400=CARTESIAN_POINT('',(28.1886785825478,2.06920630259021,33.8305837392638));
#63401=CARTESIAN_POINT('Origin',(30.,-1.32966554433622E-14,33.8305837392638));
#63402=CARTESIAN_POINT('',(28.1886785825478,2.0692063025902,16.));
#63403=CARTESIAN_POINT('Origin',(30.,-1.32966554433622E-14,16.));
#63404=CARTESIAN_POINT('',(28.2396221576007,2.11271622609138,33.8305837392638));
#63405=CARTESIAN_POINT('',(28.2396221576007,2.11271622609137,16.));
#63406=CARTESIAN_POINT('',(28.3566103373554,2.20494227060779,33.8305837392638));
#63407=CARTESIAN_POINT('Origin',(30.,-1.32966554433622E-14,33.8305837392638));
#63408=CARTESIAN_POINT('',(28.3566103373554,2.20494227060779,16.));
#63409=CARTESIAN_POINT('Origin',(30.,-1.32966554433622E-14,16.));
#63410=CARTESIAN_POINT('',(28.4108106196211,2.24432108070371,33.8305837392638));
#63411=CARTESIAN_POINT('',(28.4108106196211,2.2443210807037,16.));
#63412=CARTESIAN_POINT('',(28.5346741359158,2.32708403630936,33.8305837392638));
#63413=CARTESIAN_POINT('Origin',(30.,-1.32966554433622E-14,33.8305837392638));
#63414=CARTESIAN_POINT('',(28.5346741359158,2.32708403630936,16.));
#63415=CARTESIAN_POINT('Origin',(30.,-1.32966554433622E-14,16.));
#63416=CARTESIAN_POINT('',(28.5917969626306,2.36208894954101,33.8305837392638));
#63417=CARTESIAN_POINT('',(28.5917969626306,2.36208894954101,16.));
#63418=CARTESIAN_POINT('',(28.7217721556985,2.43487855509313,33.8305837392638));
#63419=CARTESIAN_POINT('Origin',(30.,-1.32966554433622E-14,33.8305837392638));
#63420=CARTESIAN_POINT('',(28.7217721556985,2.43487855509312,16.));
#63421=CARTESIAN_POINT('Origin',(30.,-1.32966554433622E-14,16.));
#63422=CARTESIAN_POINT('',(28.7814653456406,2.46529375453011,33.8305837392638));
#63423=CARTESIAN_POINT('',(28.7814653456406,2.46529375453011,16.));
#63424=CARTESIAN_POINT('',(28.9167508751952,2.52766123790546,33.8305837392638));
#63425=CARTESIAN_POINT('Origin',(30.,-1.32966554433622E-14,33.8305837392638));
#63426=CARTESIAN_POINT('',(28.9167508751953,2.52766123790545,16.));
#63427=CARTESIAN_POINT('Origin',(30.,-1.32966554433622E-14,16.));
#63428=CARTESIAN_POINT('',(28.9786463999985,2.55329920372917,33.8305837392638));
#63429=CARTESIAN_POINT('',(28.9786463999985,2.55329920372917,16.));
#63430=CARTESIAN_POINT('',(29.1184081857633,2.60486004865344,33.8305837392638));
#63431=CARTESIAN_POINT('Origin',(30.,-1.32966554433622E-14,33.8305837392638));
#63432=CARTESIAN_POINT('',(29.1184081857633,2.60486004865344,16.));
#63433=CARTESIAN_POINT('Origin',(30.,-1.32966554433622E-14,16.));
#63434=CARTESIAN_POINT('',(29.182124438935,2.6255627142791,33.8305837392638));
#63435=CARTESIAN_POINT('',(29.182124438935,2.62556271427909,16.));
#63436=CARTESIAN_POINT('',(29.3255008030251,2.66599903099762,33.8305837392638));
#63437=CARTESIAN_POINT('Origin',(30.,-1.32966554433622E-14,33.8305837392638));
#63438=CARTESIAN_POINT('',(29.3255008030251,2.66599903099761,16.));
#63439=CARTESIAN_POINT('Origin',(30.,-1.32966554433622E-14,16.));
#63440=CARTESIAN_POINT('',(29.3906449526767,2.6816387576073,33.8305837392638));
#63441=CARTESIAN_POINT('',(29.3906449526767,2.68163875760729,16.));
#63442=CARTESIAN_POINT('',(29.5367519321301,2.71070124278105,33.8305837392638));
#63443=CARTESIAN_POINT('Origin',(30.,-1.32966554433622E-14,33.8305837392638));
#63444=CARTESIAN_POINT('',(29.5367519321301,2.71070124278105,16.));
#63445=CARTESIAN_POINT('Origin',(30.,-1.32966554433622E-14,16.));
#63446=CARTESIAN_POINT('',(29.6029223429162,2.72118160625947,33.8305837392638));
#63447=CARTESIAN_POINT('',(29.6029223429162,2.72118160625946,16.));
#63448=CARTESIAN_POINT('',(29.750859139619,2.73869108000311,33.8305837392638));
#63449=CARTESIAN_POINT('Origin',(30.,-1.32966554433622E-14,33.8305837392638));
#63450=CARTESIAN_POINT('',(29.750859139619,2.7386910800031,16.));
#63451=CARTESIAN_POINT('Origin',(30.,-1.32966554433622E-14,16.));
#63452=CARTESIAN_POINT('',(29.8176478489534,2.74394746542434,33.8305837392638));
#63453=CARTESIAN_POINT('',(29.8176478489534,2.74394746542433,16.));
#63454=CARTESIAN_POINT('',(29.9665023833599,2.74979597600975,33.8305837392638));
#63455=CARTESIAN_POINT('Origin',(30.,-1.32966554433622E-14,33.8305837392638));
#63456=CARTESIAN_POINT('',(29.9665023833599,2.74979597600974,16.));
#63457=CARTESIAN_POINT('Origin',(30.,-1.32966554433622E-14,16.));
#63458=CARTESIAN_POINT('',(30.3970776570838,2.72118160625946,33.8305837392638));
#63459=CARTESIAN_POINT('',(30.3970776570838,2.72118160625945,16.));
#63460=CARTESIAN_POINT('',(30.249140860381,2.73869108000311,33.8305837392638));
#63461=CARTESIAN_POINT('',(30.249140860381,2.7386910800031,16.));
#63462=CARTESIAN_POINT('Origin',(30.,-1.32966554433622E-14,33.8305837392638));
#63463=CARTESIAN_POINT('Origin',(30.,-1.32966554433622E-14,33.8305837392638));
#63464=CARTESIAN_POINT('Origin',(27.5075580599235,1.0459901541636,33.8304779343707));
#63465=CARTESIAN_POINT('Origin',(27.5859153117241,1.21595293501799,33.830456743813));
#63466=CARTESIAN_POINT('Origin',(30.,-1.32966554433622E-14,33.8305837392638));
#63467=CARTESIAN_POINT('Origin',(27.4979545614264,1.02279765627048,33.8304567438139));
#63468=CARTESIAN_POINT('Origin',(27.4331739849704,0.847210974834779,33.830477934375));
#63469=CARTESIAN_POINT('Origin',(30.,-1.32966554433622E-14,33.8305837392638));
#63470=CARTESIAN_POINT('Origin',(27.4254197532764,0.823336489857381,33.8304567438132));
#63471=CARTESIAN_POINT('Origin',(27.3746152459633,0.643208458112014,33.8304779343751));
#63472=CARTESIAN_POINT('Origin',(30.,-1.32966554433622E-14,33.8305837392638));
#63473=CARTESIAN_POINT('Origin',(27.368758088479,0.618799180196873,33.8304567438137));
#63474=CARTESIAN_POINT('Origin',(27.3322428769935,0.435240347356666,33.8304779343754));
#63475=CARTESIAN_POINT('Origin',(30.,-1.32966554433622E-14,33.8305837392638));
#63476=CARTESIAN_POINT('Origin',(27.3283189050469,0.410446767819665,33.8304567438127));
#63477=CARTESIAN_POINT('Origin',(27.3063181178076,0.224588835126915,33.8304779343751));
#63478=CARTESIAN_POINT('Origin',(30.,-1.32966554433622E-14,33.8305837392638));
#63479=CARTESIAN_POINT('Origin',(27.3043515239852,0.199563814630461,33.8304567438133));
#63480=CARTESIAN_POINT('Origin',(27.2970008031678,0.0125526580442922,33.8304779343738));
#63481=CARTESIAN_POINT('Origin',(30.,-1.32966554433622E-14,33.8305837392638));
#63482=CARTESIAN_POINT('Origin',(27.2970037121732,-0.012549515837469,33.8304567438135));
#63483=CARTESIAN_POINT('Origin',(27.3043483774083,-0.199560910346332,33.8304779343754));
#63484=CARTESIAN_POINT('Origin',(30.,-1.32966554433622E-14,33.8305837392638));
#63485=CARTESIAN_POINT('Origin',(27.3063207713147,-0.224585474366301,33.8304567438129));
#63486=CARTESIAN_POINT('Origin',(27.3283155403039,-0.410444119366497,33.8304779343742));
#63487=CARTESIAN_POINT('Origin',(30.,-1.32966554433622E-14,33.8305837392638));
#63488=CARTESIAN_POINT('Origin',(27.3322452586388,-0.435236788764194,33.8304567438132));
#63489=CARTESIAN_POINT('Origin',(27.3687545263134,-0.618796803902706,33.8304779343752));
#63490=CARTESIAN_POINT('Origin',(30.,-1.32966554433622E-14,33.8305837392638));
#63491=CARTESIAN_POINT('Origin',(27.3746173410614,-0.643204723628853,33.8304567438136));
#63492=CARTESIAN_POINT('Origin',(27.4254160156486,-0.823334400372707,33.8304779343751));
#63493=CARTESIAN_POINT('Origin',(30.,-1.32966554433622E-14,33.8305837392638));
#63494=CARTESIAN_POINT('Origin',(27.433175780606,-0.847207087484101,33.8304567438133));
#63495=CARTESIAN_POINT('Origin',(27.4979506713824,-1.02279586647791,33.8304779343754));
#63496=CARTESIAN_POINT('Origin',(30.,-1.32966554433622E-14,33.8305837392638));
#63497=CARTESIAN_POINT('Origin',(27.5075595450189,-1.04598613791989,33.830456743813));
#63498=CARTESIAN_POINT('Origin',(27.5859112932449,-1.21595145595217,33.830477934375));
#63499=CARTESIAN_POINT('Origin',(30.,-1.32966554433622E-14,33.8305837392638));
#63500=CARTESIAN_POINT('Origin',(27.5973100336554,-1.23831633599182,33.8304567438138));
#63501=CARTESIAN_POINT('Origin',(27.6887555747498,-1.40161030035549,33.8304779343749));
#63502=CARTESIAN_POINT('Origin',(30.,-1.32966554433622E-14,33.8305837392638));
#63503=CARTESIAN_POINT('Origin',(27.7018739049122,-1.42301190206769,33.8304567438132));
#63504=CARTESIAN_POINT('Origin',(27.8058494467036,-1.57862775117429,33.8304779343746));
#63505=CARTESIAN_POINT('Origin',(30.,-1.32966554433622E-14,33.8305837392638));
#63506=CARTESIAN_POINT('Origin',(27.8206064877493,-1.59893412656796,33.8304567438128));
#63507=CARTESIAN_POINT('Origin',(27.9364709864456,-1.74591243696051,33.830477934375));
#63508=CARTESIAN_POINT('Origin',(30.,-1.32966554433622E-14,33.8305837392638));
#63509=CARTESIAN_POINT('Origin',(27.9527757563098,-1.76499839048126,33.8304567438135));
#63510=CARTESIAN_POINT('Origin',(28.0798148687495,-1.90243299199812,33.8304779343753));
#63511=CARTESIAN_POINT('Origin',(30.,-1.32966554433622E-14,33.8305837392638));
#63512=CARTESIAN_POINT('Origin',(28.0975668431045,-1.92018085239454,33.8304567438138));
#63513=CARTESIAN_POINT('Origin',(28.234997330915,-2.04722441501659,33.8304779343752));
#63514=CARTESIAN_POINT('Origin',(30.,-1.32966554433622E-14,33.8305837392638));
#63515=CARTESIAN_POINT('Origin',(28.2540870629355,-2.06352476082575,33.8304567438132));
#63516=CARTESIAN_POINT('Origin',(28.4010616214883,-2.1793940187284,33.8304779343619));
#63517=CARTESIAN_POINT('Origin',(30.,-1.32966554433622E-14,33.8305837392638));
#63518=CARTESIAN_POINT('Origin',(28.4213714165976,-2.19414635291788,33.8304567438138));
#63519=CARTESIAN_POINT('Origin',(28.5769838988107,-2.29812693362319,33.8304779343729));
#63520=CARTESIAN_POINT('Origin',(30.,-1.32966554433622E-14,33.8305837392638));
#63521=CARTESIAN_POINT('Origin',(28.5983885404242,-2.31124030311337,33.8304567438133));
#63522=CARTESIAN_POINT('Origin',(28.7616795436178,-2.40269113175742,33.8304779343754));
#63523=CARTESIAN_POINT('Origin',(30.,-1.32966554433622E-14,33.8305837392638));
#63524=CARTESIAN_POINT('Origin',(28.7840470649819,-2.41408468827727,33.8304567438135));
#63525=CARTESIAN_POINT('Origin',(28.9540098458287,-2.49244194008352,33.8304779343747));
#63526=CARTESIAN_POINT('Origin',(30.,-1.32966554433622E-14,33.8305837392638));
#63527=CARTESIAN_POINT('Origin',(28.9772023437295,-2.50204543857419,33.8304567438141));
#63528=CARTESIAN_POINT('Origin',(29.1527890251654,-2.5668260150294,33.8304779343748));
#63529=CARTESIAN_POINT('Origin',(30.,-1.32966554433622E-14,33.8305837392638));
#63530=CARTESIAN_POINT('Origin',(29.1766635101425,-2.57458024672298,33.8304567438129));
#63531=CARTESIAN_POINT('Origin',(29.3567915418921,-2.62538475403142,33.8304779343725));
#63532=CARTESIAN_POINT('Origin',(30.,-1.32966554433622E-14,33.8305837392638));
#63533=CARTESIAN_POINT('Origin',(29.3812008198029,-2.63124191151983,33.8304567438133));
#63534=CARTESIAN_POINT('Origin',(29.5647596526443,-2.66775712300496,33.8304779343746));
#63535=CARTESIAN_POINT('Origin',(30.,-1.32966554433622E-14,33.8305837392638));
#63536=CARTESIAN_POINT('Origin',(29.589553232181,-2.67168109495555,33.8304567438136));
#63537=CARTESIAN_POINT('Origin',(29.7754111648755,-2.69368188218804,33.8304779343731));
#63538=CARTESIAN_POINT('Origin',(30.,-1.32966554433622E-14,33.8305837392638));
#63539=CARTESIAN_POINT('Origin',(29.8004361853699,-2.69564847601571,33.8304567438137));
#63540=CARTESIAN_POINT('Origin',(29.9874473419542,-2.70299919683539,33.8304779343752));
#63541=CARTESIAN_POINT('Origin',(30.,-1.32966554433622E-14,33.8305837392638));
#63542=CARTESIAN_POINT('Origin',(30.0125495158367,-2.70299628782517,33.8304567438128));
#63543=CARTESIAN_POINT('Origin',(30.199560910346,-2.6956516225925,33.8304779343757));
#63544=CARTESIAN_POINT('Origin',(30.,-1.32966554433622E-14,33.8305837392638));
#63545=CARTESIAN_POINT('Origin',(30.2245854743665,-2.69367922868563,33.8304567438131));
#63546=CARTESIAN_POINT('Origin',(30.4104441193657,-2.67168445969903,33.8304779343754));
#63547=CARTESIAN_POINT('Origin',(30.,-1.32966554433622E-14,33.8305837392638));
#63548=CARTESIAN_POINT('Origin',(30.4352367887642,-2.66775474136125,33.8304567438132));
#63549=CARTESIAN_POINT('Origin',(30.6187968039027,-2.63124547368644,33.8304779343751));
#63550=CARTESIAN_POINT('Origin',(30.,-1.32966554433622E-14,33.8305837392638));
#63551=CARTESIAN_POINT('Origin',(30.6432047236274,-2.6253826589367,33.8304567438126));
#63552=CARTESIAN_POINT('Origin',(30.8233344003726,-2.57458398435223,33.8304779343755));
#63553=CARTESIAN_POINT('Origin',(30.,-1.32966554433622E-14,33.8305837392638));
#63554=CARTESIAN_POINT('Origin',(30.8472070874839,-2.5668242193938,33.8304567438132));
#63555=CARTESIAN_POINT('Origin',(31.0227958664778,-2.50204932861793,33.8304779343756));
#63556=CARTESIAN_POINT('Origin',(30.,-1.32966554433622E-14,33.8305837392638));
#63557=CARTESIAN_POINT('Origin',(31.0459861379201,-2.49244045498134,33.8304567438131));
#63558=CARTESIAN_POINT('Origin',(31.2159514559521,-2.41408870675381,33.8304779343746));
#63559=CARTESIAN_POINT('Origin',(30.,-1.32966554433622E-14,33.8305837392638));
#63560=CARTESIAN_POINT('Origin',(31.2383163359911,-2.402689966344,33.8304567438135));
#63561=CARTESIAN_POINT('Origin',(31.4016103003557,-2.3112444252517,33.8304779343755));
#63562=CARTESIAN_POINT('Origin',(30.,-1.32966554433622E-14,33.8305837392638));
#63563=CARTESIAN_POINT('Origin',(31.4230119020685,-2.29812609508837,33.8304567438136));
#63564=CARTESIAN_POINT('Origin',(31.5786277511746,-2.19415055329817,33.8304779343753));
#63565=CARTESIAN_POINT('Origin',(30.,-1.32966554433622E-14,33.8305837392638));
#63566=CARTESIAN_POINT('Origin',(31.5989341265715,-2.17939351225268,33.8304567438143));
#63567=CARTESIAN_POINT('Origin',(31.7459124369605,-2.06352901355452,33.8304779343751));
#63568=CARTESIAN_POINT('Origin',(30.,-1.32966554433622E-14,33.8305837392638));
#63569=CARTESIAN_POINT('Origin',(31.764998390482,-2.04722424369058,33.8304567438139));
#63570=CARTESIAN_POINT('Origin',(31.9024329919978,-1.92018513124985,33.8304779343751));
#63571=CARTESIAN_POINT('Origin',(30.,-1.32966554433622E-14,33.8305837392638));
#63572=CARTESIAN_POINT('Origin',(31.9201808523926,-1.90243315689474,33.8304567438131));
#63573=CARTESIAN_POINT('Origin',(32.0472244150163,-1.76500266908446,33.830477934375));
#63574=CARTESIAN_POINT('Origin',(30.,-1.32966554433622E-14,33.8305837392638));
#63575=CARTESIAN_POINT('Origin',(32.0635247608254,-1.74591293706441,33.8304567438131));
#63576=CARTESIAN_POINT('Origin',(32.1793940187282,-1.59893837851134,33.8304779343617));
#63577=CARTESIAN_POINT('Origin',(30.,-1.32966554433622E-14,33.8305837392638));
#63578=CARTESIAN_POINT('Origin',(32.1941463529172,-1.57862858340229,33.8304567438136));
#63579=CARTESIAN_POINT('Origin',(32.2981269336233,-1.42301610118952,33.830477934373));
#63580=CARTESIAN_POINT('Origin',(30.,-1.32966554433622E-14,33.8305837392638));
#63581=CARTESIAN_POINT('Origin',(32.311240303114,-1.40161145957583,33.8304567438134));
#63582=CARTESIAN_POINT('Origin',(32.4026911317571,-1.23832045638176,33.8304779343753));
#63583=CARTESIAN_POINT('Origin',(30.,-1.32966554433622E-14,33.8305837392638));
#63584=CARTESIAN_POINT('Origin',(32.4140846882749,-1.21595293501797,33.8304567438127));
#63585=CARTESIAN_POINT('Origin',(32.4924419400838,-1.04599015417152,33.8304779343749));
#63586=CARTESIAN_POINT('Origin',(30.,-1.32966554433622E-14,33.8305837392638));
#63587=CARTESIAN_POINT('Origin',(32.5020454385714,-1.02279765627054,33.8304567438132));
#63588=CARTESIAN_POINT('Origin',(32.56682601503,-0.847210974835106,33.8304779343751));
#63589=CARTESIAN_POINT('Origin',(30.,-1.32966554433622E-14,33.8305837392638));
#63590=CARTESIAN_POINT('Origin',(32.5745802467237,-0.823336489857386,33.8304567438133));
#63591=CARTESIAN_POINT('Origin',(32.6253847540299,-0.643208458106727,33.8304779343718));
#63592=CARTESIAN_POINT('Origin',(30.,-1.32966554433622E-14,33.8305837392638));
#63593=CARTESIAN_POINT('Origin',(32.6312419115182,-0.618799180197391,33.8304567438127));
#63594=CARTESIAN_POINT('Origin',(32.6677571230055,-0.435240347356057,33.830477934375));
#63595=CARTESIAN_POINT('Origin',(30.,-1.32966554433622E-14,33.8305837392638));
#63596=CARTESIAN_POINT('Origin',(32.6716810949544,-0.410446767819313,33.8304567438133));
#63597=CARTESIAN_POINT('Origin',(32.6936818821919,-0.224588835126652,33.8304779343749));
#63598=CARTESIAN_POINT('Origin',(30.,-1.32966554433622E-14,33.8305837392638));
#63599=CARTESIAN_POINT('Origin',(32.6956484760151,-0.199563814630355,33.8304567438134));
#63600=CARTESIAN_POINT('Origin',(32.7029991968333,-0.0125526580448477,33.8304779343743));
#63601=CARTESIAN_POINT('Origin',(30.,-1.32966554433622E-14,33.8305837392638));
#63602=CARTESIAN_POINT('Origin',(32.7029962878262,0.0125495158371826,33.8304567438133));
#63603=CARTESIAN_POINT('Origin',(32.6956516225903,0.19956091034681,33.8304779343749));
#63604=CARTESIAN_POINT('Origin',(30.,-1.32966554433622E-14,33.8305837392638));
#63605=CARTESIAN_POINT('Origin',(32.6936792286859,0.22458547436666,33.8304567438133));
#63606=CARTESIAN_POINT('Origin',(32.6716844596177,0.410444119388619,33.8304779343428));
#63607=CARTESIAN_POINT('Origin',(30.,-1.32966554433622E-14,33.8305837392638));
#63608=CARTESIAN_POINT('Origin',(32.6677547413622,0.435236788764869,33.8304567438136));
#63609=CARTESIAN_POINT('Origin',(32.6312454736863,0.618796803902747,33.8304779343751));
#63610=CARTESIAN_POINT('Origin',(30.,-1.32966554433622E-14,33.8305837392638));
#63611=CARTESIAN_POINT('Origin',(32.625382658939,0.643204723629168,33.8304567438138));
#63612=CARTESIAN_POINT('Origin',(32.5745839843506,0.823334400372804,33.8304779343749));
#63613=CARTESIAN_POINT('Origin',(30.,-1.32966554433622E-14,33.8305837392638));
#63614=CARTESIAN_POINT('Origin',(32.5668242193939,0.847207087484111,33.8304567438133));
#63615=CARTESIAN_POINT('Origin',(32.5020493286164,1.02279586647793,33.830477934375));
#63616=CARTESIAN_POINT('Origin',(30.,-1.32966554433622E-14,33.8305837392638));
#63617=CARTESIAN_POINT('Origin',(32.4924404549818,1.04598613792066,33.8304567438134));
#63618=CARTESIAN_POINT('Origin',(32.4140887067556,1.21595145595219,33.8304779343752));
#63619=CARTESIAN_POINT('Origin',(30.,-1.32966554433622E-14,33.8305837392638));
#63620=CARTESIAN_POINT('Origin',(32.4026899663445,1.2383163359917,33.8304567438137));
#63621=CARTESIAN_POINT('Origin',(32.3112444252326,1.40161030035344,33.830477934368));
#63622=CARTESIAN_POINT('Origin',(30.,-1.32966554433622E-14,33.8305837392638));
#63623=CARTESIAN_POINT('Origin',(32.2981260950878,1.42301190206775,33.8304567438133));
#63624=CARTESIAN_POINT('Origin',(32.1941505532983,1.57862775117468,33.8304779343753));
#63625=CARTESIAN_POINT('Origin',(30.,-1.32966554433622E-14,33.8305837392638));
#63626=CARTESIAN_POINT('Origin',(32.1793935122518,1.59893412656992,33.8304567438136));
#63627=CARTESIAN_POINT('Origin',(32.0635290135536,1.74591243696026,33.8304779343747));
#63628=CARTESIAN_POINT('Origin',(30.,-1.32966554433622E-14,33.8305837392638));
#63629=CARTESIAN_POINT('Origin',(32.04722424369,1.76499839048088,33.8304567438134));
#63630=CARTESIAN_POINT('Origin',(31.9201851312459,1.90243299199643,33.8304779343734));
#63631=CARTESIAN_POINT('Origin',(30.,-1.32966554433622E-14,33.8305837392638));
#63632=CARTESIAN_POINT('Origin',(31.9024331568948,1.92018085239292,33.8304567438132));
#63633=CARTESIAN_POINT('Origin',(31.7650026690842,2.0472244150162,33.8304779343749));
#63634=CARTESIAN_POINT('Origin',(30.,-1.32966554433622E-14,33.8305837392638));
#63635=CARTESIAN_POINT('Origin',(31.7459129370645,2.06352476082576,33.8304567438132));
#63636=CARTESIAN_POINT('Origin',(31.5989383785419,2.17939401874533,33.8304779343753));
#63637=CARTESIAN_POINT('Origin',(30.,-1.32966554433622E-14,33.8305837392638));
#63638=CARTESIAN_POINT('Origin',(31.5786285834019,2.1941463529156,33.830456743813));
#63639=CARTESIAN_POINT('Origin',(31.4230161011941,2.29812693362645,33.8304779343752));
#63640=CARTESIAN_POINT('Origin',(30.,-1.32966554433622E-14,33.8305837392638));
#63641=CARTESIAN_POINT('Origin',(31.4016114595758,2.31124030311394,33.8304567438134));
#63642=CARTESIAN_POINT('Origin',(31.2383204563814,2.40269113175683,33.8304779343751));
#63643=CARTESIAN_POINT('Origin',(30.,-1.32966554433622E-14,33.8305837392638));
#63644=CARTESIAN_POINT('Origin',(31.215952935018,2.41408468827632,33.8304567438131));
#63645=CARTESIAN_POINT('Origin',(31.0459901541714,2.49244194008366,33.8304779343748));
#63646=CARTESIAN_POINT('Origin',(30.,-1.32966554433622E-14,33.8305837392638));
#63647=CARTESIAN_POINT('Origin',(31.0227976562705,2.50204543857161,33.8304567438132));
#63648=CARTESIAN_POINT('Origin',(30.8472109748356,2.56682601503055,33.8304779343754));
#63649=CARTESIAN_POINT('Origin',(30.,-1.32966554433622E-14,33.8305837392638));
#63650=CARTESIAN_POINT('Origin',(30.8233364898573,2.574580246724,33.8304567438134));
#63651=CARTESIAN_POINT('Origin',(30.6432084580721,2.62538475398616,33.8304779343503));
#63652=CARTESIAN_POINT('Origin',(30.,-1.32966554433622E-14,33.8305837392638));
#63653=CARTESIAN_POINT('Origin',(30.6187991801972,2.63124191151918,33.8304567438131));
#63654=CARTESIAN_POINT('Origin',(30.4352403473569,2.66775712300684,33.8304779343755));
#63655=CARTESIAN_POINT('Origin',(30.,-1.32966554433622E-14,33.8305837392638));
#63656=CARTESIAN_POINT('Origin',(27.5973088682432,1.23832045638137,33.8304779343751));
#63657=CARTESIAN_POINT('Origin',(27.6887596968862,1.40161145957579,33.8304567438134));
#63658=CARTESIAN_POINT('Origin',(30.,-1.32966554433622E-14,33.8305837392638));
#63659=CARTESIAN_POINT('Origin',(27.7018730663741,1.4230161011934,33.8304779343749));
#63660=CARTESIAN_POINT('Origin',(27.8058536470835,1.57862858340213,33.8304567438133));
#63661=CARTESIAN_POINT('Origin',(30.,-1.32966554433622E-14,33.8305837392638));
#63662=CARTESIAN_POINT('Origin',(27.8206059812548,1.59893837854177,33.8304779343751));
#63663=CARTESIAN_POINT('Origin',(27.9364752391745,1.7459129370644,33.8304567438132));
#63664=CARTESIAN_POINT('Origin',(30.,-1.32966554433622E-14,33.8305837392638));
#63665=CARTESIAN_POINT('Origin',(27.952775584984,1.76500266908388,33.8304779343747));
#63666=CARTESIAN_POINT('Origin',(28.0798191476065,1.90243315689505,33.8304567438134));
#63667=CARTESIAN_POINT('Origin',(30.,-1.32966554433622E-14,33.8305837392638));
#63668=CARTESIAN_POINT('Origin',(28.0975670080041,1.92018513124447,33.8304779343728));
#63669=CARTESIAN_POINT('Origin',(28.23500160952,2.04722424368963,33.830456743813));
#63670=CARTESIAN_POINT('Origin',(30.,-1.32966554433622E-14,33.8305837392638));
#63671=CARTESIAN_POINT('Origin',(28.2540875630398,2.06352901355343,33.8304779343746));
#63672=CARTESIAN_POINT('Origin',(28.4010658734306,2.17939351225149,33.8304567438134));
#63673=CARTESIAN_POINT('Origin',(30.,-1.32966554433622E-14,33.8305837392638));
#63674=CARTESIAN_POINT('Origin',(28.4213722488255,2.19415055329726,33.8304779343749));
#63675=CARTESIAN_POINT('Origin',(28.5769880979325,2.29812609508769,33.8304567438131));
#63676=CARTESIAN_POINT('Origin',(30.,-1.32966554433622E-14,33.8305837392638));
#63677=CARTESIAN_POINT('Origin',(28.5983896996467,2.31124442523142,33.8304779343677));
#63678=CARTESIAN_POINT('Origin',(28.7616836640084,2.40268996634441,33.8304567438137));
#63679=CARTESIAN_POINT('Origin',(30.,-1.32966554433622E-14,33.8305837392638));
#63680=CARTESIAN_POINT('Origin',(28.7840485440478,2.41408870675589,33.8304779343753));
#63681=CARTESIAN_POINT('Origin',(28.9540138620795,2.49244045498167,33.8304567438133));
#63682=CARTESIAN_POINT('Origin',(30.,-1.32966554433622E-14,33.8305837392638));
#63683=CARTESIAN_POINT('Origin',(28.9772041335221,2.50204932861683,33.8304779343752));
#63684=CARTESIAN_POINT('Origin',(29.1527929125161,2.56682421939371,33.8304567438132));
#63685=CARTESIAN_POINT('Origin',(30.,-1.32966554433622E-14,33.8305837392638));
#63686=CARTESIAN_POINT('Origin',(29.1766655996273,2.57458398435145,33.8304779343752));
#63687=CARTESIAN_POINT('Origin',(29.3567952763716,2.62538265893797,33.8304567438133));
#63688=CARTESIAN_POINT('Origin',(30.,-1.32966554433622E-14,33.8305837392638));
#63689=CARTESIAN_POINT('Origin',(29.3812031960975,2.63124547368767,33.8304779343756));
#63690=CARTESIAN_POINT('Origin',(29.5647632112354,2.66775474136179,33.8304567438135));
#63691=CARTESIAN_POINT('Origin',(30.,-1.32966554433622E-14,33.8305837392638));
#63692=CARTESIAN_POINT('Origin',(29.5895558806117,2.67168445961877,33.8304779343432));
#63693=CARTESIAN_POINT('Origin',(29.775414525633,2.69367922868643,33.8304567438135));
#63694=CARTESIAN_POINT('Origin',(30.,-1.32966554433622E-14,33.8305837392638));
#63695=CARTESIAN_POINT('Origin',(29.8004390896529,2.69565162258947,33.8304779343745));
#63696=CARTESIAN_POINT('Origin',(29.9874504841622,2.70299628782743,33.8304567438137));
#63697=CARTESIAN_POINT('Origin',(30.,-1.32966554433622E-14,33.8305837392638));
#63698=CARTESIAN_POINT('Origin',(30.4104467678198,2.67168109495229,33.8304567438124));
#63699=CARTESIAN_POINT('Origin',(30.2245888351268,2.69368188219228,33.830477934375));
#63700=CARTESIAN_POINT('Origin',(30.,1.17524047358083,16.));
#63701=CARTESIAN_POINT('Origin',(30.,2.60624999999999,31.));
#63702=CARTESIAN_POINT('Origin',(30.,-1.32966554433622E-14,31.6569162607362));
#63703=CARTESIAN_POINT('',(30.1823521510466,2.74394746542433,31.6569162607362));
#63704=CARTESIAN_POINT('Origin',(30.1995609103462,2.69565162259179,31.6570220656244));
#63705=CARTESIAN_POINT('',(30.03349761664,2.74979597600974,31.6569162607362));
#63706=CARTESIAN_POINT('Origin',(30.0125495158372,2.70299628782596,31.6570432561867));
#63707=CARTESIAN_POINT('Origin',(30.,-1.32966554433622E-14,31.6569162607362));
#63708=CARTESIAN_POINT('Origin',(30.,-1.32966554433622E-14,16.));
#63709=CARTESIAN_POINT('',(30.1823521510466,2.74394746542434,33.8305837392638));
#63710=CARTESIAN_POINT('',(30.1823521510466,2.74394746542433,16.));
#63711=CARTESIAN_POINT('',(30.03349761664,2.74979597600975,33.8305837392638));
#63712=CARTESIAN_POINT('',(30.03349761664,2.74979597600974,16.));
#63713=CARTESIAN_POINT('Origin',(30.,-1.32966554433622E-14,33.8305837392638));
#63714=CARTESIAN_POINT('Origin',(30.,-1.32966554433622E-14,33.8305837392638));
#63715=CARTESIAN_POINT('Origin',(30.1995638146302,2.69564847601544,33.8304567438135));
#63716=CARTESIAN_POINT('Origin',(30.0125526580447,2.70299919683307,33.8304779343742));
#63717=CARTESIAN_POINT('Origin',(30.,-1.32966554433622E-14,34.));
#63718=CARTESIAN_POINT('Origin',(30.,-1.32966554433622E-14,32.5));
#63719=CARTESIAN_POINT('',(30.,-1.44337567297407,32.5));
#63720=CARTESIAN_POINT('',(31.25,-0.72168783648704,32.5));
#63721=CARTESIAN_POINT('',(30.,-1.44337567297407,32.5));
#63722=CARTESIAN_POINT('',(31.25,0.721687836487017,32.5));
#63723=CARTESIAN_POINT('',(31.25,-0.72168783648704,32.5));
#63724=CARTESIAN_POINT('',(30.,1.44337567297405,32.5));
#63725=CARTESIAN_POINT('',(31.25,0.721687836487017,32.5));
#63726=CARTESIAN_POINT('',(28.75,0.721687836487017,32.5));
#63727=CARTESIAN_POINT('',(30.,1.44337567297405,32.5));
#63728=CARTESIAN_POINT('',(28.75,-0.721687836487044,32.5));
#63729=CARTESIAN_POINT('',(28.75,0.721687836487017,32.5));
#63730=CARTESIAN_POINT('',(28.75,-0.721687836487044,32.5));
#63731=CARTESIAN_POINT('Origin',(31.25,-0.72168783648704,32.5));
#63732=CARTESIAN_POINT('',(31.25,-0.72168783648704,32.5));
#63733=CARTESIAN_POINT('',(31.25,0.721687836487017,32.5));
#63734=CARTESIAN_POINT('Origin',(31.25,0.721687836487017,32.5));
#63735=CARTESIAN_POINT('',(30.,1.44337567297405,32.5));
#63736=CARTESIAN_POINT('Origin',(30.,1.44337567297405,32.5));
#63737=CARTESIAN_POINT('',(28.75,0.721687836487017,32.5));
#63738=CARTESIAN_POINT('Origin',(28.75,0.721687836487017,32.5));
#63739=CARTESIAN_POINT('',(28.75,-0.721687836487044,32.5));
#63740=CARTESIAN_POINT('Origin',(28.75,-0.721687836487044,32.5));
#63741=CARTESIAN_POINT('',(30.,-1.44337567297407,32.5));
#63742=CARTESIAN_POINT('Origin',(30.,-1.44337567297407,32.5));
#63743=CARTESIAN_POINT('Ctrl Pts',(30.,1.17523237272422,15.7500046770317));
#63744=CARTESIAN_POINT('Ctrl Pts',(29.3214792732473,1.17523237272422,15.7916713436984));
#63745=CARTESIAN_POINT('Ctrl Pts',(28.9822189098709,0.587616186362105,15.8333380103651));
#63746=CARTESIAN_POINT('Ctrl Pts',(28.6429585464946,-1.32141491426617E-14,
15.8750046770317));
#63747=CARTESIAN_POINT('Ctrl Pts',(28.9822189098709,-0.587616186362132,
15.9166713436984));
#63748=CARTESIAN_POINT('Ctrl Pts',(29.3214792732473,-1.17523237272425,15.9583380103651));
#63749=CARTESIAN_POINT('Ctrl Pts',(30.,-1.17523237272425,16.0000046770317));
#63750=CARTESIAN_POINT('Ctrl Pts',(30.6785207267527,-1.17523237272425,16.0416713436984));
#63751=CARTESIAN_POINT('Ctrl Pts',(31.017781090129,-0.587616186362132,16.0833380103651));
#63752=CARTESIAN_POINT('Ctrl Pts',(31.3570414535054,-1.35453513912972E-14,
16.1250046770317));
#63753=CARTESIAN_POINT('Ctrl Pts',(31.017781090129,0.587616186362104,16.1666713436984));
#63754=CARTESIAN_POINT('Ctrl Pts',(30.6785207267527,1.17523237272422,16.2083380103651));
#63755=CARTESIAN_POINT('Ctrl Pts',(30.,1.17523237272422,16.2500046770317));
#63756=CARTESIAN_POINT('Ctrl Pts',(29.3214792732473,1.17523237272422,16.2916713436984));
#63757=CARTESIAN_POINT('Ctrl Pts',(28.9822189098709,0.587616186362105,16.3333380103651));
#63758=CARTESIAN_POINT('Ctrl Pts',(28.6429585464946,-1.32141491426617E-14,
16.3750046770317));
#63759=CARTESIAN_POINT('Ctrl Pts',(28.9822189098709,-0.587616186362132,
16.4166713436984));
#63760=CARTESIAN_POINT('Ctrl Pts',(29.3214792732473,-1.17523237272425,16.4583380103651));
#63761=CARTESIAN_POINT('Ctrl Pts',(30.,-1.17523237272425,16.5000046770317));
#63762=CARTESIAN_POINT('Ctrl Pts',(30.6785207267527,-1.17523237272425,16.5416713436984));
#63763=CARTESIAN_POINT('Ctrl Pts',(31.017781090129,-0.587616186362132,16.5833380103651));
#63764=CARTESIAN_POINT('Ctrl Pts',(31.3570414535054,-1.35453513912972E-14,
16.6250046770317));
#63765=CARTESIAN_POINT('Ctrl Pts',(31.017781090129,0.587616186362104,16.6666713436984));
#63766=CARTESIAN_POINT('Ctrl Pts',(30.6785207267527,1.17523237272422,16.7083380103651));
#63767=CARTESIAN_POINT('Ctrl Pts',(30.,1.17523237272422,16.7500046770317));
#63768=CARTESIAN_POINT('Ctrl Pts',(29.3214792732473,1.17523237272422,16.7916713436984));
#63769=CARTESIAN_POINT('Ctrl Pts',(28.9822189098709,0.587616186362105,16.8333380103651));
#63770=CARTESIAN_POINT('Ctrl Pts',(28.6429585464946,-1.32141491426617E-14,
16.8750046770317));
#63771=CARTESIAN_POINT('Ctrl Pts',(28.9822189098709,-0.587616186362132,
16.9166713436984));
#63772=CARTESIAN_POINT('Ctrl Pts',(29.3214792732473,-1.17523237272425,16.9583380103651));
#63773=CARTESIAN_POINT('Ctrl Pts',(30.,-1.17523237272425,17.0000046770317));
#63774=CARTESIAN_POINT('Ctrl Pts',(30.6785207267527,-1.17523237272425,17.0416713436984));
#63775=CARTESIAN_POINT('Ctrl Pts',(31.017781090129,-0.587616186362132,17.0833380103651));
#63776=CARTESIAN_POINT('Ctrl Pts',(31.3570414535054,-1.35453513912972E-14,
17.1250046770317));
#63777=CARTESIAN_POINT('Ctrl Pts',(31.017781090129,0.587616186362104,17.1666713436984));
#63778=CARTESIAN_POINT('Ctrl Pts',(30.6785207267527,1.17523237272422,17.2083380103651));
#63779=CARTESIAN_POINT('Ctrl Pts',(30.,1.17523237272422,17.2500046770317));
#63780=CARTESIAN_POINT('Ctrl Pts',(29.3214792732473,1.17523237272422,17.2916713436984));
#63781=CARTESIAN_POINT('Ctrl Pts',(28.9822189098709,0.587616186362105,17.3333380103651));
#63782=CARTESIAN_POINT('Ctrl Pts',(28.6429585464946,-1.32141491426617E-14,
17.3750046770317));
#63783=CARTESIAN_POINT('Ctrl Pts',(28.9822189098709,-0.587616186362132,
17.4166713436984));
#63784=CARTESIAN_POINT('Ctrl Pts',(29.3214792732473,-1.17523237272425,17.4583380103651));
#63785=CARTESIAN_POINT('Ctrl Pts',(30.,-1.17523237272425,17.5000046770317));
#63786=CARTESIAN_POINT('Ctrl Pts',(30.6785207267527,-1.17523237272425,17.5416713436984));
#63787=CARTESIAN_POINT('Ctrl Pts',(31.017781090129,-0.587616186362132,17.5833380103651));
#63788=CARTESIAN_POINT('Ctrl Pts',(31.3570414535054,-1.35453513912972E-14,
17.6250046770317));
#63789=CARTESIAN_POINT('Ctrl Pts',(31.017781090129,0.587616186362104,17.6666713436984));
#63790=CARTESIAN_POINT('Ctrl Pts',(30.6785207267527,1.17523237272422,17.7083380103651));
#63791=CARTESIAN_POINT('Ctrl Pts',(30.,1.17523237272422,17.7500046770317));
#63792=CARTESIAN_POINT('Ctrl Pts',(29.3214792732473,1.17523237272422,17.7916713436984));
#63793=CARTESIAN_POINT('Ctrl Pts',(28.9822189098709,0.587616186362105,17.8333380103651));
#63794=CARTESIAN_POINT('Ctrl Pts',(28.6429585464946,-1.32141491426617E-14,
17.8750046770317));
#63795=CARTESIAN_POINT('Ctrl Pts',(28.9822189098709,-0.587616186362132,
17.9166713436984));
#63796=CARTESIAN_POINT('Ctrl Pts',(29.3214792732473,-1.17523237272425,17.9583380103651));
#63797=CARTESIAN_POINT('Ctrl Pts',(30.,-1.17523237272425,18.0000046770317));
#63798=CARTESIAN_POINT('Ctrl Pts',(30.6785207267527,-1.17523237272425,18.0416713436984));
#63799=CARTESIAN_POINT('Ctrl Pts',(31.017781090129,-0.587616186362132,18.0833380103651));
#63800=CARTESIAN_POINT('Ctrl Pts',(31.3570414535054,-1.35453513912972E-14,
18.1250046770317));
#63801=CARTESIAN_POINT('Ctrl Pts',(31.017781090129,0.587616186362104,18.1666713436984));
#63802=CARTESIAN_POINT('Ctrl Pts',(30.6785207267527,1.17523237272422,18.2083380103651));
#63803=CARTESIAN_POINT('Ctrl Pts',(30.,1.17523237272422,18.2500046770317));
#63804=CARTESIAN_POINT('Ctrl Pts',(29.3214792732473,1.17523237272422,18.2916713436984));
#63805=CARTESIAN_POINT('Ctrl Pts',(28.9822189098709,0.587616186362105,18.3333380103651));
#63806=CARTESIAN_POINT('Ctrl Pts',(28.6429585464946,-1.32141491426617E-14,
18.3750046770317));
#63807=CARTESIAN_POINT('Ctrl Pts',(28.9822189098709,-0.587616186362132,
18.4166713436984));
#63808=CARTESIAN_POINT('Ctrl Pts',(29.3214792732473,-1.17523237272425,18.4583380103651));
#63809=CARTESIAN_POINT('Ctrl Pts',(30.,-1.17523237272425,18.5000046770317));
#63810=CARTESIAN_POINT('Ctrl Pts',(30.6785207267527,-1.17523237272425,18.5416713436984));
#63811=CARTESIAN_POINT('Ctrl Pts',(31.017781090129,-0.587616186362132,18.5833380103651));
#63812=CARTESIAN_POINT('Ctrl Pts',(31.3570414535054,-1.35453513912972E-14,
18.6250046770317));
#63813=CARTESIAN_POINT('Ctrl Pts',(31.017781090129,0.587616186362104,18.6666713436984));
#63814=CARTESIAN_POINT('Ctrl Pts',(30.6785207267527,1.17523237272422,18.7083380103651));
#63815=CARTESIAN_POINT('Ctrl Pts',(30.,1.17523237272422,18.7500046770317));
#63816=CARTESIAN_POINT('Ctrl Pts',(29.3214792732473,1.17523237272422,18.7916713436984));
#63817=CARTESIAN_POINT('Ctrl Pts',(28.9822189098709,0.587616186362105,18.8333380103651));
#63818=CARTESIAN_POINT('Ctrl Pts',(28.6429585464946,-1.32141491426617E-14,
18.8750046770317));
#63819=CARTESIAN_POINT('Ctrl Pts',(28.9822189098709,-0.587616186362132,
18.9166713436984));
#63820=CARTESIAN_POINT('Ctrl Pts',(29.3214792732473,-1.17523237272425,18.9583380103651));
#63821=CARTESIAN_POINT('Ctrl Pts',(30.,-1.17523237272425,19.0000046770317));
#63822=CARTESIAN_POINT('Ctrl Pts',(30.6785207267527,-1.17523237272425,19.0416713436984));
#63823=CARTESIAN_POINT('Ctrl Pts',(31.017781090129,-0.587616186362132,19.0833380103651));
#63824=CARTESIAN_POINT('Ctrl Pts',(31.3570414535054,-1.35453513912972E-14,
19.1250046770317));
#63825=CARTESIAN_POINT('Ctrl Pts',(31.017781090129,0.587616186362104,19.1666713436984));
#63826=CARTESIAN_POINT('Ctrl Pts',(30.6785207267527,1.17523237272422,19.2083380103651));
#63827=CARTESIAN_POINT('Ctrl Pts',(30.,1.17523237272422,19.2500046770317));
#63828=CARTESIAN_POINT('Ctrl Pts',(29.3214792732473,1.17523237272422,19.2916713436984));
#63829=CARTESIAN_POINT('Ctrl Pts',(28.9822189098709,0.587616186362105,19.3333380103651));
#63830=CARTESIAN_POINT('Ctrl Pts',(28.6429585464946,-1.32141491426617E-14,
19.3750046770317));
#63831=CARTESIAN_POINT('Ctrl Pts',(28.9822189098709,-0.587616186362132,
19.4166713436984));
#63832=CARTESIAN_POINT('Ctrl Pts',(29.3214792732473,-1.17523237272425,19.4583380103651));
#63833=CARTESIAN_POINT('Ctrl Pts',(30.,-1.17523237272425,19.5000046770317));
#63834=CARTESIAN_POINT('Ctrl Pts',(30.6785207267527,-1.17523237272425,19.5416713436984));
#63835=CARTESIAN_POINT('Ctrl Pts',(31.017781090129,-0.587616186362132,19.5833380103651));
#63836=CARTESIAN_POINT('Ctrl Pts',(31.3570414535054,-1.35453513912972E-14,
19.6250046770317));
#63837=CARTESIAN_POINT('Ctrl Pts',(31.017781090129,0.587616186362104,19.6666713436984));
#63838=CARTESIAN_POINT('Ctrl Pts',(30.6785207267527,1.17523237272422,19.7083380103651));
#63839=CARTESIAN_POINT('Ctrl Pts',(30.,1.17523237272422,19.7500046770317));
#63840=CARTESIAN_POINT('Ctrl Pts',(29.3214792732473,1.17523237272422,19.7916713436984));
#63841=CARTESIAN_POINT('Ctrl Pts',(28.9822189098709,0.587616186362105,19.8333380103651));
#63842=CARTESIAN_POINT('Ctrl Pts',(28.6429585464946,-1.32141491426617E-14,
19.8750046770317));
#63843=CARTESIAN_POINT('Ctrl Pts',(28.9822189098709,-0.587616186362132,
19.9166713436984));
#63844=CARTESIAN_POINT('Ctrl Pts',(29.3214792732473,-1.17523237272425,19.9583380103651));
#63845=CARTESIAN_POINT('Ctrl Pts',(30.,-1.17523237272425,20.0000046770317));
#63846=CARTESIAN_POINT('Ctrl Pts',(30.6785207267527,-1.17523237272425,20.0416713436984));
#63847=CARTESIAN_POINT('Ctrl Pts',(31.017781090129,-0.587616186362132,20.0833380103651));
#63848=CARTESIAN_POINT('Ctrl Pts',(31.3570414535054,-1.35453513912972E-14,
20.1250046770317));
#63849=CARTESIAN_POINT('Ctrl Pts',(31.017781090129,0.587616186362104,20.1666713436984));
#63850=CARTESIAN_POINT('Ctrl Pts',(30.6785207267527,1.17523237272422,20.2083380103651));
#63851=CARTESIAN_POINT('Ctrl Pts',(30.,1.17523237272422,20.2500046770317));
#63852=CARTESIAN_POINT('Ctrl Pts',(29.3214792732473,1.17523237272422,20.2916713436984));
#63853=CARTESIAN_POINT('Ctrl Pts',(28.9822189098709,0.587616186362105,20.3333380103651));
#63854=CARTESIAN_POINT('Ctrl Pts',(28.6429585464946,-1.32141491426617E-14,
20.3750046770317));
#63855=CARTESIAN_POINT('Ctrl Pts',(28.9822189098709,-0.587616186362132,
20.4166713436984));
#63856=CARTESIAN_POINT('Ctrl Pts',(29.3214792732473,-1.17523237272425,20.4583380103651));
#63857=CARTESIAN_POINT('Ctrl Pts',(30.,-1.17523237272425,20.5000046770317));
#63858=CARTESIAN_POINT('Ctrl Pts',(30.6785207267527,-1.17523237272425,20.5416713436984));
#63859=CARTESIAN_POINT('Ctrl Pts',(31.017781090129,-0.587616186362132,20.5833380103651));
#63860=CARTESIAN_POINT('Ctrl Pts',(31.3570414535054,-1.35453513912972E-14,
20.6250046770317));
#63861=CARTESIAN_POINT('Ctrl Pts',(31.017781090129,0.587616186362104,20.6666713436984));
#63862=CARTESIAN_POINT('Ctrl Pts',(30.6785207267527,1.17523237272422,20.7083380103651));
#63863=CARTESIAN_POINT('Ctrl Pts',(30.,1.17523237272422,20.7500046770317));
#63864=CARTESIAN_POINT('Ctrl Pts',(29.3214792732473,1.17523237272422,20.7916713436984));
#63865=CARTESIAN_POINT('Ctrl Pts',(28.9822189098709,0.587616186362105,20.8333380103651));
#63866=CARTESIAN_POINT('Ctrl Pts',(28.6429585464946,-1.32141491426617E-14,
20.8750046770317));
#63867=CARTESIAN_POINT('Ctrl Pts',(28.9822189098709,-0.587616186362132,
20.9166713436984));
#63868=CARTESIAN_POINT('Ctrl Pts',(29.3214792732473,-1.17523237272425,20.9583380103651));
#63869=CARTESIAN_POINT('Ctrl Pts',(30.,-1.17523237272425,21.0000046770317));
#63870=CARTESIAN_POINT('Ctrl Pts',(30.6785207267527,-1.17523237272425,21.0416713436984));
#63871=CARTESIAN_POINT('Ctrl Pts',(31.017781090129,-0.587616186362132,21.0833380103651));
#63872=CARTESIAN_POINT('Ctrl Pts',(31.3570414535054,-1.35453513912972E-14,
21.1250046770317));
#63873=CARTESIAN_POINT('Ctrl Pts',(31.017781090129,0.587616186362104,21.1666713436984));
#63874=CARTESIAN_POINT('Ctrl Pts',(30.6785207267527,1.17523237272422,21.2083380103651));
#63875=CARTESIAN_POINT('Ctrl Pts',(30.,1.17523237272422,21.2500046770317));
#63876=CARTESIAN_POINT('Ctrl Pts',(29.3214792732473,1.17523237272422,21.2916713436984));
#63877=CARTESIAN_POINT('Ctrl Pts',(28.9822189098709,0.587616186362105,21.3333380103651));
#63878=CARTESIAN_POINT('Ctrl Pts',(28.6429585464946,-1.32141491426617E-14,
21.3750046770317));
#63879=CARTESIAN_POINT('Ctrl Pts',(28.9822189098709,-0.587616186362132,
21.4166713436984));
#63880=CARTESIAN_POINT('Ctrl Pts',(29.3214792732473,-1.17523237272425,21.4583380103651));
#63881=CARTESIAN_POINT('Ctrl Pts',(30.,-1.17523237272425,21.5000046770317));
#63882=CARTESIAN_POINT('Ctrl Pts',(30.6785207267527,-1.17523237272425,21.5416713436984));
#63883=CARTESIAN_POINT('Ctrl Pts',(31.017781090129,-0.587616186362132,21.5833380103651));
#63884=CARTESIAN_POINT('Ctrl Pts',(31.3570414535054,-1.35453513912972E-14,
21.6250046770317));
#63885=CARTESIAN_POINT('Ctrl Pts',(31.017781090129,0.587616186362104,21.6666713436984));
#63886=CARTESIAN_POINT('Ctrl Pts',(30.6785207267527,1.17523237272422,21.7083380103651));
#63887=CARTESIAN_POINT('Ctrl Pts',(30.,1.17523237272422,21.7500046770317));
#63888=CARTESIAN_POINT('Ctrl Pts',(29.3214792732473,1.17523237272422,21.7916713436984));
#63889=CARTESIAN_POINT('Ctrl Pts',(28.9822189098709,0.587616186362105,21.8333380103651));
#63890=CARTESIAN_POINT('Ctrl Pts',(28.6429585464946,-1.32141491426617E-14,
21.8750046770317));
#63891=CARTESIAN_POINT('Ctrl Pts',(28.9822189098709,-0.587616186362132,
21.9166713436984));
#63892=CARTESIAN_POINT('Ctrl Pts',(29.3214792732473,-1.17523237272425,21.9583380103651));
#63893=CARTESIAN_POINT('Ctrl Pts',(30.,-1.17523237272425,22.0000046770317));
#63894=CARTESIAN_POINT('Ctrl Pts',(30.6785207267527,-1.17523237272425,22.0416713436984));
#63895=CARTESIAN_POINT('Ctrl Pts',(31.017781090129,-0.587616186362132,22.0833380103651));
#63896=CARTESIAN_POINT('Ctrl Pts',(31.3570414535054,-1.35453513912972E-14,
22.1250046770317));
#63897=CARTESIAN_POINT('Ctrl Pts',(31.017781090129,0.587616186362104,22.1666713436984));
#63898=CARTESIAN_POINT('Ctrl Pts',(30.6785207267527,1.17523237272422,22.2083380103651));
#63899=CARTESIAN_POINT('Ctrl Pts',(30.,1.17523237272422,22.2500046770317));
#63900=CARTESIAN_POINT('Ctrl Pts',(29.3214792732473,1.17523237272422,22.2916713436984));
#63901=CARTESIAN_POINT('Ctrl Pts',(28.9822189098709,0.587616186362105,22.3333380103651));
#63902=CARTESIAN_POINT('Ctrl Pts',(28.6429585464946,-1.32141491426617E-14,
22.3750046770317));
#63903=CARTESIAN_POINT('Ctrl Pts',(28.9822189098709,-0.587616186362132,
22.4166713436984));
#63904=CARTESIAN_POINT('Ctrl Pts',(29.3214792732473,-1.17523237272425,22.4583380103651));
#63905=CARTESIAN_POINT('Ctrl Pts',(30.,-1.17523237272425,22.5000046770317));
#63906=CARTESIAN_POINT('Ctrl Pts',(30.6785207267527,-1.17523237272425,22.5416713436984));
#63907=CARTESIAN_POINT('Ctrl Pts',(31.017781090129,-0.587616186362132,22.5833380103651));
#63908=CARTESIAN_POINT('Ctrl Pts',(31.3570414535054,-1.35453513912972E-14,
22.6250046770317));
#63909=CARTESIAN_POINT('Ctrl Pts',(31.017781090129,0.587616186362104,22.6666713436984));
#63910=CARTESIAN_POINT('Ctrl Pts',(30.6785207267527,1.17523237272422,22.7083380103651));
#63911=CARTESIAN_POINT('Ctrl Pts',(30.,1.17523237272422,22.7500046770317));
#63912=CARTESIAN_POINT('Ctrl Pts',(29.3214792732473,1.17523237272422,22.7916713436984));
#63913=CARTESIAN_POINT('Ctrl Pts',(28.9822189098709,0.587616186362105,22.8333380103651));
#63914=CARTESIAN_POINT('Ctrl Pts',(28.6429585464946,-1.32141491426617E-14,
22.8750046770317));
#63915=CARTESIAN_POINT('Ctrl Pts',(28.9822189098709,-0.587616186362132,
22.9166713436984));
#63916=CARTESIAN_POINT('Ctrl Pts',(29.3214792732473,-1.17523237272425,22.9583380103651));
#63917=CARTESIAN_POINT('Ctrl Pts',(30.,-1.17523237272425,23.0000046770317));
#63918=CARTESIAN_POINT('Ctrl Pts',(30.6785207267527,-1.17523237272425,23.0416713436984));
#63919=CARTESIAN_POINT('Ctrl Pts',(31.017781090129,-0.587616186362132,23.0833380103651));
#63920=CARTESIAN_POINT('Ctrl Pts',(31.3570414535054,-1.35453513912972E-14,
23.1250046770317));
#63921=CARTESIAN_POINT('Ctrl Pts',(31.017781090129,0.587616186362104,23.1666713436984));
#63922=CARTESIAN_POINT('Ctrl Pts',(30.6785207267527,1.17523237272422,23.2083380103651));
#63923=CARTESIAN_POINT('Ctrl Pts',(30.,1.17523237272422,23.2500046770317));
#63924=CARTESIAN_POINT('Ctrl Pts',(29.3214792732473,1.17523237272422,23.2916713436984));
#63925=CARTESIAN_POINT('Ctrl Pts',(28.9822189098709,0.587616186362105,23.3333380103651));
#63926=CARTESIAN_POINT('Ctrl Pts',(28.6429585464946,-1.32141491426617E-14,
23.3750046770317));
#63927=CARTESIAN_POINT('Ctrl Pts',(28.9822189098709,-0.587616186362132,
23.4166713436984));
#63928=CARTESIAN_POINT('Ctrl Pts',(29.3214792732473,-1.17523237272425,23.4583380103651));
#63929=CARTESIAN_POINT('Ctrl Pts',(30.,-1.17523237272425,23.5000046770317));
#63930=CARTESIAN_POINT('Ctrl Pts',(30.6785207267527,-1.17523237272425,23.5416713436984));
#63931=CARTESIAN_POINT('Ctrl Pts',(31.017781090129,-0.587616186362132,23.5833380103651));
#63932=CARTESIAN_POINT('Ctrl Pts',(31.3570414535054,-1.35453513912972E-14,
23.6250046770317));
#63933=CARTESIAN_POINT('Ctrl Pts',(31.017781090129,0.587616186362104,23.6666713436984));
#63934=CARTESIAN_POINT('Ctrl Pts',(30.6785207267527,1.17523237272422,23.7083380103651));
#63935=CARTESIAN_POINT('Ctrl Pts',(30.,1.17523237272422,23.7500046770317));
#63936=CARTESIAN_POINT('Ctrl Pts',(29.3214792732473,1.17523237272422,23.7916713436984));
#63937=CARTESIAN_POINT('Ctrl Pts',(28.9822189098709,0.587616186362105,23.8333380103651));
#63938=CARTESIAN_POINT('Ctrl Pts',(28.6429585464946,-1.32141491426617E-14,
23.8750046770317));
#63939=CARTESIAN_POINT('Ctrl Pts',(28.9822189098709,-0.587616186362132,
23.9166713436984));
#63940=CARTESIAN_POINT('Ctrl Pts',(29.3214792732473,-1.17523237272425,23.9583380103651));
#63941=CARTESIAN_POINT('Ctrl Pts',(30.,-1.17523237272425,24.0000046770317));
#63942=CARTESIAN_POINT('Ctrl Pts',(30.6785207267527,-1.17523237272425,24.0416713436984));
#63943=CARTESIAN_POINT('Ctrl Pts',(31.017781090129,-0.587616186362132,24.0833380103651));
#63944=CARTESIAN_POINT('Ctrl Pts',(31.3570414535054,-1.35453513912972E-14,
24.1250046770317));
#63945=CARTESIAN_POINT('Ctrl Pts',(31.017781090129,0.587616186362104,24.1666713436984));
#63946=CARTESIAN_POINT('Ctrl Pts',(30.6785207267527,1.17523237272422,24.2083380103651));
#63947=CARTESIAN_POINT('Ctrl Pts',(30.,1.17523237272422,24.2500046770317));
#63948=CARTESIAN_POINT('Ctrl Pts',(29.3214792732473,1.17523237272422,24.2916713436984));
#63949=CARTESIAN_POINT('Ctrl Pts',(28.9822189098709,0.587616186362105,24.3333380103651));
#63950=CARTESIAN_POINT('Ctrl Pts',(28.6429585464946,-1.32141491426617E-14,
24.3750046770317));
#63951=CARTESIAN_POINT('Ctrl Pts',(28.9822189098709,-0.587616186362132,
24.4166713436984));
#63952=CARTESIAN_POINT('Ctrl Pts',(29.3214792732473,-1.17523237272425,24.4583380103651));
#63953=CARTESIAN_POINT('Ctrl Pts',(30.,-1.17523237272425,24.5000046770317));
#63954=CARTESIAN_POINT('Ctrl Pts',(30.6785207267527,-1.17523237272425,24.5416713436984));
#63955=CARTESIAN_POINT('Ctrl Pts',(31.017781090129,-0.587616186362132,24.5833380103651));
#63956=CARTESIAN_POINT('Ctrl Pts',(31.3570414535054,-1.35453513912972E-14,
24.6250046770317));
#63957=CARTESIAN_POINT('Ctrl Pts',(31.017781090129,0.587616186362104,24.6666713436984));
#63958=CARTESIAN_POINT('Ctrl Pts',(30.6785207267527,1.17523237272422,24.7083380103651));
#63959=CARTESIAN_POINT('Ctrl Pts',(30.,1.17523237272422,24.7500046770317));
#63960=CARTESIAN_POINT('Ctrl Pts',(29.3214792732473,1.17523237272422,24.7916713436984));
#63961=CARTESIAN_POINT('Ctrl Pts',(28.9822189098709,0.587616186362105,24.8333380103651));
#63962=CARTESIAN_POINT('Ctrl Pts',(28.6429585464946,-1.32141491426617E-14,
24.8750046770317));
#63963=CARTESIAN_POINT('Ctrl Pts',(28.9822189098709,-0.587616186362132,
24.9166713436984));
#63964=CARTESIAN_POINT('Ctrl Pts',(29.3214792732473,-1.17523237272425,24.9583380103651));
#63965=CARTESIAN_POINT('Ctrl Pts',(30.,-1.17523237272425,25.0000046770317));
#63966=CARTESIAN_POINT('Ctrl Pts',(30.6785207267527,-1.17523237272425,25.0416713436984));
#63967=CARTESIAN_POINT('Ctrl Pts',(31.017781090129,-0.587616186362132,25.0833380103651));
#63968=CARTESIAN_POINT('Ctrl Pts',(31.3570414535054,-1.35453513912972E-14,
25.1250046770317));
#63969=CARTESIAN_POINT('Ctrl Pts',(31.017781090129,0.587616186362104,25.1666713436984));
#63970=CARTESIAN_POINT('Ctrl Pts',(30.6785207267527,1.17523237272422,25.2083380103651));
#63971=CARTESIAN_POINT('Ctrl Pts',(30.,1.17523237272422,25.2500046770317));
#63972=CARTESIAN_POINT('Ctrl Pts',(29.3214792732473,1.17523237272422,25.2916713436984));
#63973=CARTESIAN_POINT('Ctrl Pts',(28.9822189098709,0.587616186362105,25.3333380103651));
#63974=CARTESIAN_POINT('Ctrl Pts',(28.6429585464946,-1.32141491426617E-14,
25.3750046770317));
#63975=CARTESIAN_POINT('Ctrl Pts',(28.9822189098709,-0.587616186362132,
25.4166713436984));
#63976=CARTESIAN_POINT('Ctrl Pts',(29.3214792732473,-1.17523237272425,25.4583380103651));
#63977=CARTESIAN_POINT('Ctrl Pts',(30.,-1.17523237272425,25.5000046770317));
#63978=CARTESIAN_POINT('Ctrl Pts',(30.6785207267527,-1.17523237272425,25.5416713436984));
#63979=CARTESIAN_POINT('Ctrl Pts',(31.017781090129,-0.587616186362132,25.5833380103651));
#63980=CARTESIAN_POINT('Ctrl Pts',(31.3570414535054,-1.35453513912972E-14,
25.6250046770317));
#63981=CARTESIAN_POINT('Ctrl Pts',(31.017781090129,0.587616186362104,25.6666713436984));
#63982=CARTESIAN_POINT('Ctrl Pts',(30.6785207267527,1.17523237272422,25.7083380103651));
#63983=CARTESIAN_POINT('Ctrl Pts',(30.,1.17523237272422,25.7500046770317));
#63984=CARTESIAN_POINT('Ctrl Pts',(29.3214792732473,1.17523237272422,25.7916713436984));
#63985=CARTESIAN_POINT('Ctrl Pts',(28.9822189098709,0.587616186362105,25.8333380103651));
#63986=CARTESIAN_POINT('Ctrl Pts',(28.6429585464946,-1.32141491426617E-14,
25.8750046770317));
#63987=CARTESIAN_POINT('Ctrl Pts',(28.9822189098709,-0.587616186362132,
25.9166713436984));
#63988=CARTESIAN_POINT('Ctrl Pts',(29.3214792732473,-1.17523237272425,25.9583380103651));
#63989=CARTESIAN_POINT('Ctrl Pts',(30.,-1.17523237272425,26.0000046770317));
#63990=CARTESIAN_POINT('Ctrl Pts',(30.6785207267527,-1.17523237272425,26.0416713436984));
#63991=CARTESIAN_POINT('Ctrl Pts',(31.017781090129,-0.587616186362132,26.0833380103651));
#63992=CARTESIAN_POINT('Ctrl Pts',(31.3570414535054,-1.35453513912972E-14,
26.1250046770317));
#63993=CARTESIAN_POINT('Ctrl Pts',(31.017781090129,0.587616186362104,26.1666713436984));
#63994=CARTESIAN_POINT('Ctrl Pts',(30.6785207267527,1.17523237272422,26.2083380103651));
#63995=CARTESIAN_POINT('Ctrl Pts',(30.,1.17523237272422,26.2500046770317));
#63996=CARTESIAN_POINT('Ctrl Pts',(29.3214792732473,1.17523237272422,26.2916713436984));
#63997=CARTESIAN_POINT('Ctrl Pts',(28.9822189098709,0.587616186362105,26.3333380103651));
#63998=CARTESIAN_POINT('Ctrl Pts',(28.6429585464946,-1.32141491426617E-14,
26.3750046770317));
#63999=CARTESIAN_POINT('Ctrl Pts',(28.9822189098709,-0.587616186362132,
26.4166713436984));
#64000=CARTESIAN_POINT('Ctrl Pts',(29.3214792732473,-1.17523237272425,26.4583380103651));
#64001=CARTESIAN_POINT('Ctrl Pts',(30.,-1.17523237272425,26.5000046770317));
#64002=CARTESIAN_POINT('Ctrl Pts',(30.6785207267527,-1.17523237272425,26.5416713436984));
#64003=CARTESIAN_POINT('Ctrl Pts',(31.017781090129,-0.587616186362132,26.5833380103651));
#64004=CARTESIAN_POINT('Ctrl Pts',(31.3570414535054,-1.35453513912972E-14,
26.6250046770317));
#64005=CARTESIAN_POINT('Ctrl Pts',(31.017781090129,0.587616186362104,26.6666713436984));
#64006=CARTESIAN_POINT('Ctrl Pts',(30.6785207267527,1.17523237272422,26.7083380103651));
#64007=CARTESIAN_POINT('Ctrl Pts',(30.,1.17523237272422,26.7500046770317));
#64008=CARTESIAN_POINT('Ctrl Pts',(29.3214792732473,1.17523237272422,26.7916713436984));
#64009=CARTESIAN_POINT('Ctrl Pts',(28.9822189098709,0.587616186362105,26.8333380103651));
#64010=CARTESIAN_POINT('Ctrl Pts',(28.6429585464946,-1.32141491426617E-14,
26.8750046770317));
#64011=CARTESIAN_POINT('Ctrl Pts',(28.9822189098709,-0.587616186362132,
26.9166713436984));
#64012=CARTESIAN_POINT('Ctrl Pts',(29.3214792732473,-1.17523237272425,26.9583380103651));
#64013=CARTESIAN_POINT('Ctrl Pts',(30.,-1.17523237272425,27.0000046770317));
#64014=CARTESIAN_POINT('Ctrl Pts',(30.6785207267527,-1.17523237272425,27.0416713436984));
#64015=CARTESIAN_POINT('Ctrl Pts',(31.017781090129,-0.587616186362132,27.0833380103651));
#64016=CARTESIAN_POINT('Ctrl Pts',(31.3570414535054,-1.35453513912972E-14,
27.1250046770317));
#64017=CARTESIAN_POINT('Ctrl Pts',(31.017781090129,0.587616186362104,27.1666713436984));
#64018=CARTESIAN_POINT('Ctrl Pts',(30.6785207267527,1.17523237272422,27.2083380103651));
#64019=CARTESIAN_POINT('Ctrl Pts',(30.,1.17523237272422,27.2500046770317));
#64020=CARTESIAN_POINT('Ctrl Pts',(29.3214792732473,1.17523237272422,27.2916713436984));
#64021=CARTESIAN_POINT('Ctrl Pts',(28.9822189098709,0.587616186362105,27.3333380103651));
#64022=CARTESIAN_POINT('Ctrl Pts',(28.6429585464946,-1.32141491426617E-14,
27.3750046770317));
#64023=CARTESIAN_POINT('Ctrl Pts',(28.9822189098709,-0.587616186362132,
27.4166713436984));
#64024=CARTESIAN_POINT('Ctrl Pts',(29.3214792732473,-1.17523237272425,27.4583380103651));
#64025=CARTESIAN_POINT('Ctrl Pts',(30.,-1.17523237272425,27.5000046770317));
#64026=CARTESIAN_POINT('Ctrl Pts',(30.6785207267527,-1.17523237272425,27.5416713436984));
#64027=CARTESIAN_POINT('Ctrl Pts',(31.017781090129,-0.587616186362132,27.5833380103651));
#64028=CARTESIAN_POINT('Ctrl Pts',(31.3570414535054,-1.35453513912972E-14,
27.6250046770317));
#64029=CARTESIAN_POINT('Ctrl Pts',(31.017781090129,0.587616186362104,27.6666713436984));
#64030=CARTESIAN_POINT('Ctrl Pts',(30.6785207267527,1.17523237272422,27.7083380103651));
#64031=CARTESIAN_POINT('Ctrl Pts',(30.,1.17523237272422,27.7500046770317));
#64032=CARTESIAN_POINT('Ctrl Pts',(29.3214792732473,1.17523237272422,27.7916713436984));
#64033=CARTESIAN_POINT('Ctrl Pts',(28.9822189098709,0.587616186362105,27.8333380103651));
#64034=CARTESIAN_POINT('Ctrl Pts',(28.6429585464946,-1.32141491426617E-14,
27.8750046770317));
#64035=CARTESIAN_POINT('Ctrl Pts',(28.9822189098709,-0.587616186362132,
27.9166713436984));
#64036=CARTESIAN_POINT('Ctrl Pts',(29.3214792732473,-1.17523237272425,27.9583380103651));
#64037=CARTESIAN_POINT('Ctrl Pts',(30.,-1.17523237272425,28.0000046770317));
#64038=CARTESIAN_POINT('Ctrl Pts',(30.6785207267527,-1.17523237272425,28.0416713436984));
#64039=CARTESIAN_POINT('Ctrl Pts',(31.017781090129,-0.587616186362132,28.0833380103651));
#64040=CARTESIAN_POINT('Ctrl Pts',(31.3570414535054,-1.35453513912972E-14,
28.1250046770317));
#64041=CARTESIAN_POINT('Ctrl Pts',(31.017781090129,0.587616186362104,28.1666713436984));
#64042=CARTESIAN_POINT('Ctrl Pts',(30.6785207267527,1.17523237272422,28.2083380103651));
#64043=CARTESIAN_POINT('Ctrl Pts',(30.,1.17523237272422,28.2500046770317));
#64044=CARTESIAN_POINT('Ctrl Pts',(29.3214792732473,1.17523237272422,28.2916713436984));
#64045=CARTESIAN_POINT('Ctrl Pts',(28.9822189098709,0.587616186362105,28.3333380103651));
#64046=CARTESIAN_POINT('Ctrl Pts',(28.6429585464946,-1.32141491426617E-14,
28.3750046770317));
#64047=CARTESIAN_POINT('Ctrl Pts',(28.9822189098709,-0.587616186362132,
28.4166713436984));
#64048=CARTESIAN_POINT('Ctrl Pts',(29.3214792732473,-1.17523237272425,28.4583380103651));
#64049=CARTESIAN_POINT('Ctrl Pts',(30.,-1.17523237272425,28.5000046770317));
#64050=CARTESIAN_POINT('Ctrl Pts',(30.6785207267527,-1.17523237272425,28.5416713436984));
#64051=CARTESIAN_POINT('Ctrl Pts',(31.017781090129,-0.587616186362132,28.5833380103651));
#64052=CARTESIAN_POINT('Ctrl Pts',(31.3570414535054,-1.35453513912972E-14,
28.6250046770317));
#64053=CARTESIAN_POINT('Ctrl Pts',(31.017781090129,0.587616186362104,28.6666713436984));
#64054=CARTESIAN_POINT('Ctrl Pts',(30.6785207267527,1.17523237272422,28.7083380103651));
#64055=CARTESIAN_POINT('Ctrl Pts',(30.,1.17523237272422,28.7500046770317));
#64056=CARTESIAN_POINT('Ctrl Pts',(29.3214792732473,1.17523237272422,28.7916713436984));
#64057=CARTESIAN_POINT('Ctrl Pts',(28.9822189098709,0.587616186362105,28.8333380103651));
#64058=CARTESIAN_POINT('Ctrl Pts',(28.6429585464946,-1.32141491426617E-14,
28.8750046770317));
#64059=CARTESIAN_POINT('Ctrl Pts',(28.9822189098709,-0.587616186362132,
28.9166713436984));
#64060=CARTESIAN_POINT('Ctrl Pts',(29.3214792732473,-1.17523237272425,28.9583380103651));
#64061=CARTESIAN_POINT('Ctrl Pts',(30.,-1.17523237272425,29.0000046770317));
#64062=CARTESIAN_POINT('Ctrl Pts',(30.6785207267527,-1.17523237272425,29.0416713436984));
#64063=CARTESIAN_POINT('Ctrl Pts',(31.017781090129,-0.587616186362132,29.0833380103651));
#64064=CARTESIAN_POINT('Ctrl Pts',(31.3570414535054,-1.35453513912972E-14,
29.1250046770317));
#64065=CARTESIAN_POINT('Ctrl Pts',(31.017781090129,0.587616186362104,29.1666713436984));
#64066=CARTESIAN_POINT('Ctrl Pts',(30.6785207267527,1.17523237272422,29.2083380103651));
#64067=CARTESIAN_POINT('Ctrl Pts',(30.,1.17523237272422,29.2500046770317));
#64068=CARTESIAN_POINT('Ctrl Pts',(29.3214792732473,1.17523237272422,29.2916713436984));
#64069=CARTESIAN_POINT('Ctrl Pts',(28.9822189098709,0.587616186362105,29.3333380103651));
#64070=CARTESIAN_POINT('Ctrl Pts',(28.6429585464946,-1.32141491426617E-14,
29.3750046770317));
#64071=CARTESIAN_POINT('Ctrl Pts',(28.9822189098709,-0.587616186362132,
29.4166713436984));
#64072=CARTESIAN_POINT('Ctrl Pts',(29.3214792732473,-1.17523237272425,29.4583380103651));
#64073=CARTESIAN_POINT('Ctrl Pts',(30.,-1.17523237272425,29.5000046770317));
#64074=CARTESIAN_POINT('Ctrl Pts',(30.6785207267527,-1.17523237272425,29.5416713436984));
#64075=CARTESIAN_POINT('Ctrl Pts',(31.017781090129,-0.587616186362132,29.5833380103651));
#64076=CARTESIAN_POINT('Ctrl Pts',(31.3570414535054,-1.35453513912972E-14,
29.6250046770317));
#64077=CARTESIAN_POINT('Ctrl Pts',(31.017781090129,0.587616186362104,29.6666713436984));
#64078=CARTESIAN_POINT('Ctrl Pts',(30.6785207267527,1.17523237272422,29.7083380103651));
#64079=CARTESIAN_POINT('Ctrl Pts',(30.,1.17523237272422,29.7500046770317));
#64080=CARTESIAN_POINT('Ctrl Pts',(29.3214792732473,1.17523237272422,29.7916713436984));
#64081=CARTESIAN_POINT('Ctrl Pts',(28.9822189098709,0.587616186362105,29.8333380103651));
#64082=CARTESIAN_POINT('Ctrl Pts',(28.6429585464946,-1.32141491426617E-14,
29.8750046770317));
#64083=CARTESIAN_POINT('Ctrl Pts',(28.9822189098709,-0.587616186362132,
29.9166713436984));
#64084=CARTESIAN_POINT('Ctrl Pts',(29.3214792732473,-1.17523237272425,29.9583380103651));
#64085=CARTESIAN_POINT('Ctrl Pts',(30.,-1.17523237272425,30.0000046770317));
#64086=CARTESIAN_POINT('Ctrl Pts',(30.6785207267527,-1.17523237272425,30.0416713436984));
#64087=CARTESIAN_POINT('Ctrl Pts',(31.017781090129,-0.587616186362132,30.0833380103651));
#64088=CARTESIAN_POINT('Ctrl Pts',(31.3570414535054,-1.35453513912972E-14,
30.1250046770317));
#64089=CARTESIAN_POINT('Ctrl Pts',(31.017781090129,0.587616186362104,30.1666713436984));
#64090=CARTESIAN_POINT('Ctrl Pts',(30.6785207267527,1.17523237272422,30.2083380103651));
#64091=CARTESIAN_POINT('Ctrl Pts',(30.,1.17523237272422,30.2500046770317));
#64092=CARTESIAN_POINT('Ctrl Pts',(29.3214792732473,1.17523237272422,30.2916713436984));
#64093=CARTESIAN_POINT('Ctrl Pts',(28.9822189098709,0.587616186362105,30.3333380103651));
#64094=CARTESIAN_POINT('Ctrl Pts',(28.6429585464946,-1.32141491426617E-14,
30.3750046770317));
#64095=CARTESIAN_POINT('Ctrl Pts',(28.9822189098709,-0.587616186362132,
30.4166713436984));
#64096=CARTESIAN_POINT('Ctrl Pts',(29.3214792732473,-1.17523237272425,30.4583380103651));
#64097=CARTESIAN_POINT('Ctrl Pts',(30.,-1.17523237272425,30.5000046770317));
#64098=CARTESIAN_POINT('Ctrl Pts',(30.6785207267527,-1.17523237272425,30.5416713436984));
#64099=CARTESIAN_POINT('Ctrl Pts',(31.017781090129,-0.587616186362132,30.5833380103651));
#64100=CARTESIAN_POINT('Ctrl Pts',(31.3570414535054,-1.35453513912972E-14,
30.6250046770317));
#64101=CARTESIAN_POINT('Ctrl Pts',(31.017781090129,0.587616186362104,30.6666713436984));
#64102=CARTESIAN_POINT('Ctrl Pts',(30.6785207267527,1.17523237272422,30.7083380103651));
#64103=CARTESIAN_POINT('Ctrl Pts',(30.,1.17523237272422,30.7500046770317));
#64104=CARTESIAN_POINT('Ctrl Pts',(29.3214792732473,1.17523237272422,30.7916713436984));
#64105=CARTESIAN_POINT('Ctrl Pts',(28.9822189098709,0.587616186362105,30.8333380103651));
#64106=CARTESIAN_POINT('Ctrl Pts',(28.6429585464946,-1.32141491426617E-14,
30.8750046770317));
#64107=CARTESIAN_POINT('Ctrl Pts',(28.9822189098709,-0.587616186362132,
30.9166713436984));
#64108=CARTESIAN_POINT('Ctrl Pts',(29.3214792732473,-1.17523237272425,30.9583380103651));
#64109=CARTESIAN_POINT('Ctrl Pts',(30.,-1.17523237272425,31.0000046770317));
#64110=CARTESIAN_POINT('Ctrl Pts',(30.6785207267527,-1.17523237272425,31.0416713436984));
#64111=CARTESIAN_POINT('Ctrl Pts',(31.017781090129,-0.587616186362132,31.0833380103651));
#64112=CARTESIAN_POINT('Ctrl Pts',(31.3570414535054,-1.35453513912972E-14,
31.1250046770317));
#64113=CARTESIAN_POINT('Ctrl Pts',(31.017781090129,0.587616186362104,31.1666713436984));
#64114=CARTESIAN_POINT('Ctrl Pts',(30.6785207267527,1.17523237272422,31.2083380103651));
#64115=CARTESIAN_POINT('Ctrl Pts',(30.,1.17523237272422,31.2500046770317));
#64116=CARTESIAN_POINT('Ctrl Pts',(30.,1.52706329386825,15.546875));
#64117=CARTESIAN_POINT('Ctrl Pts',(29.1183495962155,1.52706329386825,15.5885416666667));
#64118=CARTESIAN_POINT('Ctrl Pts',(28.6775243943233,0.76353164693412,15.6302083333334));
#64119=CARTESIAN_POINT('Ctrl Pts',(28.2366991924311,-1.31894491186926E-14,
15.671875));
#64120=CARTESIAN_POINT('Ctrl Pts',(28.6775243943233,-0.763531646934146,
15.7135416666667));
#64121=CARTESIAN_POINT('Ctrl Pts',(29.1183495962155,-1.52706329386828,15.7552083333334));
#64122=CARTESIAN_POINT('Ctrl Pts',(30.,-1.52706329386828,15.796875));
#64123=CARTESIAN_POINT('Ctrl Pts',(30.8816504037844,-1.52706329386828,15.8385416666667));
#64124=CARTESIAN_POINT('Ctrl Pts',(31.3224756056766,-0.763531646934147,
15.8802083333334));
#64125=CARTESIAN_POINT('Ctrl Pts',(31.7633008075689,-1.36198038370242E-14,
15.921875));
#64126=CARTESIAN_POINT('Ctrl Pts',(31.3224756056766,0.763531646934118,15.9635416666667));
#64127=CARTESIAN_POINT('Ctrl Pts',(30.8816504037844,1.52706329386825,16.0052083333334));
#64128=CARTESIAN_POINT('Ctrl Pts',(30.,1.52706329386825,16.046875));
#64129=CARTESIAN_POINT('Ctrl Pts',(29.1183495962155,1.52706329386825,16.0885416666667));
#64130=CARTESIAN_POINT('Ctrl Pts',(28.6775243943233,0.76353164693412,16.1302083333334));
#64131=CARTESIAN_POINT('Ctrl Pts',(28.2366991924311,-1.31894491186926E-14,
16.171875));
#64132=CARTESIAN_POINT('Ctrl Pts',(28.6775243943233,-0.763531646934146,
16.2135416666667));
#64133=CARTESIAN_POINT('Ctrl Pts',(29.1183495962155,-1.52706329386828,16.2552083333334));
#64134=CARTESIAN_POINT('Ctrl Pts',(30.,-1.52706329386828,16.296875));
#64135=CARTESIAN_POINT('Ctrl Pts',(30.8816504037844,-1.52706329386828,16.3385416666667));
#64136=CARTESIAN_POINT('Ctrl Pts',(31.3224756056766,-0.763531646934147,
16.3802083333334));
#64137=CARTESIAN_POINT('Ctrl Pts',(31.7633008075689,-1.36198038370242E-14,
16.421875));
#64138=CARTESIAN_POINT('Ctrl Pts',(31.3224756056766,0.763531646934118,16.4635416666667));
#64139=CARTESIAN_POINT('Ctrl Pts',(30.8816504037844,1.52706329386825,16.5052083333334));
#64140=CARTESIAN_POINT('Ctrl Pts',(30.,1.52706329386825,16.546875));
#64141=CARTESIAN_POINT('Ctrl Pts',(29.1183495962155,1.52706329386825,16.5885416666667));
#64142=CARTESIAN_POINT('Ctrl Pts',(28.6775243943233,0.76353164693412,16.6302083333334));
#64143=CARTESIAN_POINT('Ctrl Pts',(28.2366991924311,-1.31894491186926E-14,
16.671875));
#64144=CARTESIAN_POINT('Ctrl Pts',(28.6775243943233,-0.763531646934146,
16.7135416666667));
#64145=CARTESIAN_POINT('Ctrl Pts',(29.1183495962155,-1.52706329386828,16.7552083333334));
#64146=CARTESIAN_POINT('Ctrl Pts',(30.,-1.52706329386828,16.796875));
#64147=CARTESIAN_POINT('Ctrl Pts',(30.8816504037844,-1.52706329386828,16.8385416666667));
#64148=CARTESIAN_POINT('Ctrl Pts',(31.3224756056766,-0.763531646934147,
16.8802083333334));
#64149=CARTESIAN_POINT('Ctrl Pts',(31.7633008075689,-1.36198038370242E-14,
16.921875));
#64150=CARTESIAN_POINT('Ctrl Pts',(31.3224756056766,0.763531646934118,16.9635416666667));
#64151=CARTESIAN_POINT('Ctrl Pts',(30.8816504037844,1.52706329386825,17.0052083333334));
#64152=CARTESIAN_POINT('Ctrl Pts',(30.,1.52706329386825,17.046875));
#64153=CARTESIAN_POINT('Ctrl Pts',(29.1183495962155,1.52706329386825,17.0885416666667));
#64154=CARTESIAN_POINT('Ctrl Pts',(28.6775243943233,0.76353164693412,17.1302083333334));
#64155=CARTESIAN_POINT('Ctrl Pts',(28.2366991924311,-1.31894491186926E-14,
17.171875));
#64156=CARTESIAN_POINT('Ctrl Pts',(28.6775243943233,-0.763531646934146,
17.2135416666667));
#64157=CARTESIAN_POINT('Ctrl Pts',(29.1183495962155,-1.52706329386828,17.2552083333334));
#64158=CARTESIAN_POINT('Ctrl Pts',(30.,-1.52706329386828,17.296875));
#64159=CARTESIAN_POINT('Ctrl Pts',(30.8816504037844,-1.52706329386828,17.3385416666667));
#64160=CARTESIAN_POINT('Ctrl Pts',(31.3224756056766,-0.763531646934147,
17.3802083333334));
#64161=CARTESIAN_POINT('Ctrl Pts',(31.7633008075689,-1.36198038370242E-14,
17.421875));
#64162=CARTESIAN_POINT('Ctrl Pts',(31.3224756056766,0.763531646934118,17.4635416666667));
#64163=CARTESIAN_POINT('Ctrl Pts',(30.8816504037844,1.52706329386825,17.5052083333334));
#64164=CARTESIAN_POINT('Ctrl Pts',(30.,1.52706329386825,17.546875));
#64165=CARTESIAN_POINT('Ctrl Pts',(29.1183495962155,1.52706329386825,17.5885416666667));
#64166=CARTESIAN_POINT('Ctrl Pts',(28.6775243943233,0.76353164693412,17.6302083333334));
#64167=CARTESIAN_POINT('Ctrl Pts',(28.2366991924311,-1.31894491186926E-14,
17.671875));
#64168=CARTESIAN_POINT('Ctrl Pts',(28.6775243943233,-0.763531646934146,
17.7135416666667));
#64169=CARTESIAN_POINT('Ctrl Pts',(29.1183495962155,-1.52706329386828,17.7552083333334));
#64170=CARTESIAN_POINT('Ctrl Pts',(30.,-1.52706329386828,17.796875));
#64171=CARTESIAN_POINT('Ctrl Pts',(30.8816504037844,-1.52706329386828,17.8385416666667));
#64172=CARTESIAN_POINT('Ctrl Pts',(31.3224756056766,-0.763531646934147,
17.8802083333334));
#64173=CARTESIAN_POINT('Ctrl Pts',(31.7633008075689,-1.36198038370242E-14,
17.921875));
#64174=CARTESIAN_POINT('Ctrl Pts',(31.3224756056766,0.763531646934118,17.9635416666667));
#64175=CARTESIAN_POINT('Ctrl Pts',(30.8816504037844,1.52706329386825,18.0052083333334));
#64176=CARTESIAN_POINT('Ctrl Pts',(30.,1.52706329386825,18.046875));
#64177=CARTESIAN_POINT('Ctrl Pts',(29.1183495962155,1.52706329386825,18.0885416666667));
#64178=CARTESIAN_POINT('Ctrl Pts',(28.6775243943233,0.76353164693412,18.1302083333334));
#64179=CARTESIAN_POINT('Ctrl Pts',(28.2366991924311,-1.31894491186926E-14,
18.171875));
#64180=CARTESIAN_POINT('Ctrl Pts',(28.6775243943233,-0.763531646934146,
18.2135416666667));
#64181=CARTESIAN_POINT('Ctrl Pts',(29.1183495962155,-1.52706329386828,18.2552083333334));
#64182=CARTESIAN_POINT('Ctrl Pts',(30.,-1.52706329386828,18.296875));
#64183=CARTESIAN_POINT('Ctrl Pts',(30.8816504037844,-1.52706329386828,18.3385416666667));
#64184=CARTESIAN_POINT('Ctrl Pts',(31.3224756056766,-0.763531646934147,
18.3802083333334));
#64185=CARTESIAN_POINT('Ctrl Pts',(31.7633008075689,-1.36198038370242E-14,
18.421875));
#64186=CARTESIAN_POINT('Ctrl Pts',(31.3224756056766,0.763531646934118,18.4635416666667));
#64187=CARTESIAN_POINT('Ctrl Pts',(30.8816504037844,1.52706329386825,18.5052083333334));
#64188=CARTESIAN_POINT('Ctrl Pts',(30.,1.52706329386825,18.546875));
#64189=CARTESIAN_POINT('Ctrl Pts',(29.1183495962155,1.52706329386825,18.5885416666667));
#64190=CARTESIAN_POINT('Ctrl Pts',(28.6775243943233,0.76353164693412,18.6302083333334));
#64191=CARTESIAN_POINT('Ctrl Pts',(28.2366991924311,-1.31894491186926E-14,
18.671875));
#64192=CARTESIAN_POINT('Ctrl Pts',(28.6775243943233,-0.763531646934146,
18.7135416666667));
#64193=CARTESIAN_POINT('Ctrl Pts',(29.1183495962155,-1.52706329386828,18.7552083333334));
#64194=CARTESIAN_POINT('Ctrl Pts',(30.,-1.52706329386828,18.796875));
#64195=CARTESIAN_POINT('Ctrl Pts',(30.8816504037844,-1.52706329386828,18.8385416666667));
#64196=CARTESIAN_POINT('Ctrl Pts',(31.3224756056766,-0.763531646934147,
18.8802083333334));
#64197=CARTESIAN_POINT('Ctrl Pts',(31.7633008075689,-1.36198038370242E-14,
18.921875));
#64198=CARTESIAN_POINT('Ctrl Pts',(31.3224756056766,0.763531646934118,18.9635416666667));
#64199=CARTESIAN_POINT('Ctrl Pts',(30.8816504037844,1.52706329386825,19.0052083333334));
#64200=CARTESIAN_POINT('Ctrl Pts',(30.,1.52706329386825,19.046875));
#64201=CARTESIAN_POINT('Ctrl Pts',(29.1183495962155,1.52706329386825,19.0885416666667));
#64202=CARTESIAN_POINT('Ctrl Pts',(28.6775243943233,0.76353164693412,19.1302083333334));
#64203=CARTESIAN_POINT('Ctrl Pts',(28.2366991924311,-1.31894491186926E-14,
19.171875));
#64204=CARTESIAN_POINT('Ctrl Pts',(28.6775243943233,-0.763531646934146,
19.2135416666667));
#64205=CARTESIAN_POINT('Ctrl Pts',(29.1183495962155,-1.52706329386828,19.2552083333334));
#64206=CARTESIAN_POINT('Ctrl Pts',(30.,-1.52706329386828,19.296875));
#64207=CARTESIAN_POINT('Ctrl Pts',(30.8816504037844,-1.52706329386828,19.3385416666667));
#64208=CARTESIAN_POINT('Ctrl Pts',(31.3224756056766,-0.763531646934147,
19.3802083333334));
#64209=CARTESIAN_POINT('Ctrl Pts',(31.7633008075689,-1.36198038370242E-14,
19.421875));
#64210=CARTESIAN_POINT('Ctrl Pts',(31.3224756056766,0.763531646934118,19.4635416666667));
#64211=CARTESIAN_POINT('Ctrl Pts',(30.8816504037844,1.52706329386825,19.5052083333334));
#64212=CARTESIAN_POINT('Ctrl Pts',(30.,1.52706329386825,19.546875));
#64213=CARTESIAN_POINT('Ctrl Pts',(29.1183495962155,1.52706329386825,19.5885416666667));
#64214=CARTESIAN_POINT('Ctrl Pts',(28.6775243943233,0.76353164693412,19.6302083333334));
#64215=CARTESIAN_POINT('Ctrl Pts',(28.2366991924311,-1.31894491186926E-14,
19.671875));
#64216=CARTESIAN_POINT('Ctrl Pts',(28.6775243943233,-0.763531646934146,
19.7135416666667));
#64217=CARTESIAN_POINT('Ctrl Pts',(29.1183495962155,-1.52706329386828,19.7552083333334));
#64218=CARTESIAN_POINT('Ctrl Pts',(30.,-1.52706329386828,19.796875));
#64219=CARTESIAN_POINT('Ctrl Pts',(30.8816504037844,-1.52706329386828,19.8385416666667));
#64220=CARTESIAN_POINT('Ctrl Pts',(31.3224756056766,-0.763531646934147,
19.8802083333334));
#64221=CARTESIAN_POINT('Ctrl Pts',(31.7633008075689,-1.36198038370242E-14,
19.921875));
#64222=CARTESIAN_POINT('Ctrl Pts',(31.3224756056766,0.763531646934118,19.9635416666667));
#64223=CARTESIAN_POINT('Ctrl Pts',(30.8816504037844,1.52706329386825,20.0052083333334));
#64224=CARTESIAN_POINT('Ctrl Pts',(30.,1.52706329386825,20.046875));
#64225=CARTESIAN_POINT('Ctrl Pts',(29.1183495962155,1.52706329386825,20.0885416666667));
#64226=CARTESIAN_POINT('Ctrl Pts',(28.6775243943233,0.76353164693412,20.1302083333334));
#64227=CARTESIAN_POINT('Ctrl Pts',(28.2366991924311,-1.31894491186926E-14,
20.171875));
#64228=CARTESIAN_POINT('Ctrl Pts',(28.6775243943233,-0.763531646934146,
20.2135416666667));
#64229=CARTESIAN_POINT('Ctrl Pts',(29.1183495962155,-1.52706329386828,20.2552083333334));
#64230=CARTESIAN_POINT('Ctrl Pts',(30.,-1.52706329386828,20.296875));
#64231=CARTESIAN_POINT('Ctrl Pts',(30.8816504037844,-1.52706329386828,20.3385416666667));
#64232=CARTESIAN_POINT('Ctrl Pts',(31.3224756056766,-0.763531646934147,
20.3802083333334));
#64233=CARTESIAN_POINT('Ctrl Pts',(31.7633008075689,-1.36198038370242E-14,
20.421875));
#64234=CARTESIAN_POINT('Ctrl Pts',(31.3224756056766,0.763531646934118,20.4635416666667));
#64235=CARTESIAN_POINT('Ctrl Pts',(30.8816504037844,1.52706329386825,20.5052083333334));
#64236=CARTESIAN_POINT('Ctrl Pts',(30.,1.52706329386825,20.546875));
#64237=CARTESIAN_POINT('Ctrl Pts',(29.1183495962155,1.52706329386825,20.5885416666667));
#64238=CARTESIAN_POINT('Ctrl Pts',(28.6775243943233,0.76353164693412,20.6302083333334));
#64239=CARTESIAN_POINT('Ctrl Pts',(28.2366991924311,-1.31894491186926E-14,
20.671875));
#64240=CARTESIAN_POINT('Ctrl Pts',(28.6775243943233,-0.763531646934146,
20.7135416666667));
#64241=CARTESIAN_POINT('Ctrl Pts',(29.1183495962155,-1.52706329386828,20.7552083333334));
#64242=CARTESIAN_POINT('Ctrl Pts',(30.,-1.52706329386828,20.796875));
#64243=CARTESIAN_POINT('Ctrl Pts',(30.8816504037844,-1.52706329386828,20.8385416666667));
#64244=CARTESIAN_POINT('Ctrl Pts',(31.3224756056766,-0.763531646934147,
20.8802083333334));
#64245=CARTESIAN_POINT('Ctrl Pts',(31.7633008075689,-1.36198038370242E-14,
20.921875));
#64246=CARTESIAN_POINT('Ctrl Pts',(31.3224756056766,0.763531646934118,20.9635416666667));
#64247=CARTESIAN_POINT('Ctrl Pts',(30.8816504037844,1.52706329386825,21.0052083333334));
#64248=CARTESIAN_POINT('Ctrl Pts',(30.,1.52706329386825,21.046875));
#64249=CARTESIAN_POINT('Ctrl Pts',(29.1183495962155,1.52706329386825,21.0885416666667));
#64250=CARTESIAN_POINT('Ctrl Pts',(28.6775243943233,0.76353164693412,21.1302083333334));
#64251=CARTESIAN_POINT('Ctrl Pts',(28.2366991924311,-1.31894491186926E-14,
21.171875));
#64252=CARTESIAN_POINT('Ctrl Pts',(28.6775243943233,-0.763531646934146,
21.2135416666667));
#64253=CARTESIAN_POINT('Ctrl Pts',(29.1183495962155,-1.52706329386828,21.2552083333334));
#64254=CARTESIAN_POINT('Ctrl Pts',(30.,-1.52706329386828,21.296875));
#64255=CARTESIAN_POINT('Ctrl Pts',(30.8816504037844,-1.52706329386828,21.3385416666667));
#64256=CARTESIAN_POINT('Ctrl Pts',(31.3224756056766,-0.763531646934147,
21.3802083333334));
#64257=CARTESIAN_POINT('Ctrl Pts',(31.7633008075689,-1.36198038370242E-14,
21.421875));
#64258=CARTESIAN_POINT('Ctrl Pts',(31.3224756056766,0.763531646934118,21.4635416666667));
#64259=CARTESIAN_POINT('Ctrl Pts',(30.8816504037844,1.52706329386825,21.5052083333334));
#64260=CARTESIAN_POINT('Ctrl Pts',(30.,1.52706329386825,21.546875));
#64261=CARTESIAN_POINT('Ctrl Pts',(29.1183495962155,1.52706329386825,21.5885416666667));
#64262=CARTESIAN_POINT('Ctrl Pts',(28.6775243943233,0.76353164693412,21.6302083333334));
#64263=CARTESIAN_POINT('Ctrl Pts',(28.2366991924311,-1.31894491186926E-14,
21.671875));
#64264=CARTESIAN_POINT('Ctrl Pts',(28.6775243943233,-0.763531646934146,
21.7135416666667));
#64265=CARTESIAN_POINT('Ctrl Pts',(29.1183495962155,-1.52706329386828,21.7552083333334));
#64266=CARTESIAN_POINT('Ctrl Pts',(30.,-1.52706329386828,21.796875));
#64267=CARTESIAN_POINT('Ctrl Pts',(30.8816504037844,-1.52706329386828,21.8385416666667));
#64268=CARTESIAN_POINT('Ctrl Pts',(31.3224756056766,-0.763531646934147,
21.8802083333334));
#64269=CARTESIAN_POINT('Ctrl Pts',(31.7633008075689,-1.36198038370242E-14,
21.921875));
#64270=CARTESIAN_POINT('Ctrl Pts',(31.3224756056766,0.763531646934118,21.9635416666667));
#64271=CARTESIAN_POINT('Ctrl Pts',(30.8816504037844,1.52706329386825,22.0052083333334));
#64272=CARTESIAN_POINT('Ctrl Pts',(30.,1.52706329386825,22.046875));
#64273=CARTESIAN_POINT('Ctrl Pts',(29.1183495962155,1.52706329386825,22.0885416666667));
#64274=CARTESIAN_POINT('Ctrl Pts',(28.6775243943233,0.76353164693412,22.1302083333334));
#64275=CARTESIAN_POINT('Ctrl Pts',(28.2366991924311,-1.31894491186926E-14,
22.171875));
#64276=CARTESIAN_POINT('Ctrl Pts',(28.6775243943233,-0.763531646934146,
22.2135416666667));
#64277=CARTESIAN_POINT('Ctrl Pts',(29.1183495962155,-1.52706329386828,22.2552083333334));
#64278=CARTESIAN_POINT('Ctrl Pts',(30.,-1.52706329386828,22.296875));
#64279=CARTESIAN_POINT('Ctrl Pts',(30.8816504037844,-1.52706329386828,22.3385416666667));
#64280=CARTESIAN_POINT('Ctrl Pts',(31.3224756056766,-0.763531646934147,
22.3802083333334));
#64281=CARTESIAN_POINT('Ctrl Pts',(31.7633008075689,-1.36198038370242E-14,
22.421875));
#64282=CARTESIAN_POINT('Ctrl Pts',(31.3224756056766,0.763531646934118,22.4635416666667));
#64283=CARTESIAN_POINT('Ctrl Pts',(30.8816504037844,1.52706329386825,22.5052083333334));
#64284=CARTESIAN_POINT('Ctrl Pts',(30.,1.52706329386825,22.546875));
#64285=CARTESIAN_POINT('Ctrl Pts',(29.1183495962155,1.52706329386825,22.5885416666667));
#64286=CARTESIAN_POINT('Ctrl Pts',(28.6775243943233,0.76353164693412,22.6302083333334));
#64287=CARTESIAN_POINT('Ctrl Pts',(28.2366991924311,-1.31894491186926E-14,
22.671875));
#64288=CARTESIAN_POINT('Ctrl Pts',(28.6775243943233,-0.763531646934146,
22.7135416666667));
#64289=CARTESIAN_POINT('Ctrl Pts',(29.1183495962155,-1.52706329386828,22.7552083333334));
#64290=CARTESIAN_POINT('Ctrl Pts',(30.,-1.52706329386828,22.796875));
#64291=CARTESIAN_POINT('Ctrl Pts',(30.8816504037844,-1.52706329386828,22.8385416666667));
#64292=CARTESIAN_POINT('Ctrl Pts',(31.3224756056766,-0.763531646934147,
22.8802083333334));
#64293=CARTESIAN_POINT('Ctrl Pts',(31.7633008075689,-1.36198038370242E-14,
22.921875));
#64294=CARTESIAN_POINT('Ctrl Pts',(31.3224756056766,0.763531646934118,22.9635416666667));
#64295=CARTESIAN_POINT('Ctrl Pts',(30.8816504037844,1.52706329386825,23.0052083333334));
#64296=CARTESIAN_POINT('Ctrl Pts',(30.,1.52706329386825,23.046875));
#64297=CARTESIAN_POINT('Ctrl Pts',(29.1183495962155,1.52706329386825,23.0885416666667));
#64298=CARTESIAN_POINT('Ctrl Pts',(28.6775243943233,0.76353164693412,23.1302083333334));
#64299=CARTESIAN_POINT('Ctrl Pts',(28.2366991924311,-1.31894491186926E-14,
23.171875));
#64300=CARTESIAN_POINT('Ctrl Pts',(28.6775243943233,-0.763531646934146,
23.2135416666667));
#64301=CARTESIAN_POINT('Ctrl Pts',(29.1183495962155,-1.52706329386828,23.2552083333334));
#64302=CARTESIAN_POINT('Ctrl Pts',(30.,-1.52706329386828,23.296875));
#64303=CARTESIAN_POINT('Ctrl Pts',(30.8816504037844,-1.52706329386828,23.3385416666667));
#64304=CARTESIAN_POINT('Ctrl Pts',(31.3224756056766,-0.763531646934147,
23.3802083333334));
#64305=CARTESIAN_POINT('Ctrl Pts',(31.7633008075689,-1.36198038370242E-14,
23.421875));
#64306=CARTESIAN_POINT('Ctrl Pts',(31.3224756056766,0.763531646934118,23.4635416666667));
#64307=CARTESIAN_POINT('Ctrl Pts',(30.8816504037844,1.52706329386825,23.5052083333334));
#64308=CARTESIAN_POINT('Ctrl Pts',(30.,1.52706329386825,23.546875));
#64309=CARTESIAN_POINT('Ctrl Pts',(29.1183495962155,1.52706329386825,23.5885416666667));
#64310=CARTESIAN_POINT('Ctrl Pts',(28.6775243943233,0.76353164693412,23.6302083333334));
#64311=CARTESIAN_POINT('Ctrl Pts',(28.2366991924311,-1.31894491186926E-14,
23.671875));
#64312=CARTESIAN_POINT('Ctrl Pts',(28.6775243943233,-0.763531646934146,
23.7135416666667));
#64313=CARTESIAN_POINT('Ctrl Pts',(29.1183495962155,-1.52706329386828,23.7552083333334));
#64314=CARTESIAN_POINT('Ctrl Pts',(30.,-1.52706329386828,23.796875));
#64315=CARTESIAN_POINT('Ctrl Pts',(30.8816504037844,-1.52706329386828,23.8385416666667));
#64316=CARTESIAN_POINT('Ctrl Pts',(31.3224756056766,-0.763531646934147,
23.8802083333334));
#64317=CARTESIAN_POINT('Ctrl Pts',(31.7633008075689,-1.36198038370242E-14,
23.921875));
#64318=CARTESIAN_POINT('Ctrl Pts',(31.3224756056766,0.763531646934118,23.9635416666667));
#64319=CARTESIAN_POINT('Ctrl Pts',(30.8816504037844,1.52706329386825,24.0052083333334));
#64320=CARTESIAN_POINT('Ctrl Pts',(30.,1.52706329386825,24.046875));
#64321=CARTESIAN_POINT('Ctrl Pts',(29.1183495962155,1.52706329386825,24.0885416666667));
#64322=CARTESIAN_POINT('Ctrl Pts',(28.6775243943233,0.76353164693412,24.1302083333334));
#64323=CARTESIAN_POINT('Ctrl Pts',(28.2366991924311,-1.31894491186926E-14,
24.171875));
#64324=CARTESIAN_POINT('Ctrl Pts',(28.6775243943233,-0.763531646934146,
24.2135416666667));
#64325=CARTESIAN_POINT('Ctrl Pts',(29.1183495962155,-1.52706329386828,24.2552083333334));
#64326=CARTESIAN_POINT('Ctrl Pts',(30.,-1.52706329386828,24.296875));
#64327=CARTESIAN_POINT('Ctrl Pts',(30.8816504037844,-1.52706329386828,24.3385416666667));
#64328=CARTESIAN_POINT('Ctrl Pts',(31.3224756056766,-0.763531646934147,
24.3802083333334));
#64329=CARTESIAN_POINT('Ctrl Pts',(31.7633008075689,-1.36198038370242E-14,
24.421875));
#64330=CARTESIAN_POINT('Ctrl Pts',(31.3224756056766,0.763531646934118,24.4635416666667));
#64331=CARTESIAN_POINT('Ctrl Pts',(30.8816504037844,1.52706329386825,24.5052083333334));
#64332=CARTESIAN_POINT('Ctrl Pts',(30.,1.52706329386825,24.546875));
#64333=CARTESIAN_POINT('Ctrl Pts',(29.1183495962155,1.52706329386825,24.5885416666667));
#64334=CARTESIAN_POINT('Ctrl Pts',(28.6775243943233,0.76353164693412,24.6302083333334));
#64335=CARTESIAN_POINT('Ctrl Pts',(28.2366991924311,-1.31894491186926E-14,
24.671875));
#64336=CARTESIAN_POINT('Ctrl Pts',(28.6775243943233,-0.763531646934146,
24.7135416666667));
#64337=CARTESIAN_POINT('Ctrl Pts',(29.1183495962155,-1.52706329386828,24.7552083333334));
#64338=CARTESIAN_POINT('Ctrl Pts',(30.,-1.52706329386828,24.796875));
#64339=CARTESIAN_POINT('Ctrl Pts',(30.8816504037844,-1.52706329386828,24.8385416666667));
#64340=CARTESIAN_POINT('Ctrl Pts',(31.3224756056766,-0.763531646934147,
24.8802083333334));
#64341=CARTESIAN_POINT('Ctrl Pts',(31.7633008075689,-1.36198038370242E-14,
24.921875));
#64342=CARTESIAN_POINT('Ctrl Pts',(31.3224756056766,0.763531646934118,24.9635416666667));
#64343=CARTESIAN_POINT('Ctrl Pts',(30.8816504037844,1.52706329386825,25.0052083333334));
#64344=CARTESIAN_POINT('Ctrl Pts',(30.,1.52706329386825,25.046875));
#64345=CARTESIAN_POINT('Ctrl Pts',(29.1183495962155,1.52706329386825,25.0885416666667));
#64346=CARTESIAN_POINT('Ctrl Pts',(28.6775243943233,0.76353164693412,25.1302083333334));
#64347=CARTESIAN_POINT('Ctrl Pts',(28.2366991924311,-1.31894491186926E-14,
25.171875));
#64348=CARTESIAN_POINT('Ctrl Pts',(28.6775243943233,-0.763531646934146,
25.2135416666667));
#64349=CARTESIAN_POINT('Ctrl Pts',(29.1183495962155,-1.52706329386828,25.2552083333334));
#64350=CARTESIAN_POINT('Ctrl Pts',(30.,-1.52706329386828,25.296875));
#64351=CARTESIAN_POINT('Ctrl Pts',(30.8816504037844,-1.52706329386828,25.3385416666667));
#64352=CARTESIAN_POINT('Ctrl Pts',(31.3224756056766,-0.763531646934147,
25.3802083333334));
#64353=CARTESIAN_POINT('Ctrl Pts',(31.7633008075689,-1.36198038370242E-14,
25.421875));
#64354=CARTESIAN_POINT('Ctrl Pts',(31.3224756056766,0.763531646934118,25.4635416666667));
#64355=CARTESIAN_POINT('Ctrl Pts',(30.8816504037844,1.52706329386825,25.5052083333334));
#64356=CARTESIAN_POINT('Ctrl Pts',(30.,1.52706329386825,25.546875));
#64357=CARTESIAN_POINT('Ctrl Pts',(29.1183495962155,1.52706329386825,25.5885416666667));
#64358=CARTESIAN_POINT('Ctrl Pts',(28.6775243943233,0.76353164693412,25.6302083333334));
#64359=CARTESIAN_POINT('Ctrl Pts',(28.2366991924311,-1.31894491186926E-14,
25.671875));
#64360=CARTESIAN_POINT('Ctrl Pts',(28.6775243943233,-0.763531646934146,
25.7135416666667));
#64361=CARTESIAN_POINT('Ctrl Pts',(29.1183495962155,-1.52706329386828,25.7552083333334));
#64362=CARTESIAN_POINT('Ctrl Pts',(30.,-1.52706329386828,25.796875));
#64363=CARTESIAN_POINT('Ctrl Pts',(30.8816504037844,-1.52706329386828,25.8385416666667));
#64364=CARTESIAN_POINT('Ctrl Pts',(31.3224756056766,-0.763531646934147,
25.8802083333334));
#64365=CARTESIAN_POINT('Ctrl Pts',(31.7633008075689,-1.36198038370242E-14,
25.921875));
#64366=CARTESIAN_POINT('Ctrl Pts',(31.3224756056766,0.763531646934118,25.9635416666667));
#64367=CARTESIAN_POINT('Ctrl Pts',(30.8816504037844,1.52706329386825,26.0052083333334));
#64368=CARTESIAN_POINT('Ctrl Pts',(30.,1.52706329386825,26.046875));
#64369=CARTESIAN_POINT('Ctrl Pts',(29.1183495962155,1.52706329386825,26.0885416666667));
#64370=CARTESIAN_POINT('Ctrl Pts',(28.6775243943233,0.76353164693412,26.1302083333334));
#64371=CARTESIAN_POINT('Ctrl Pts',(28.2366991924311,-1.31894491186926E-14,
26.171875));
#64372=CARTESIAN_POINT('Ctrl Pts',(28.6775243943233,-0.763531646934146,
26.2135416666667));
#64373=CARTESIAN_POINT('Ctrl Pts',(29.1183495962155,-1.52706329386828,26.2552083333334));
#64374=CARTESIAN_POINT('Ctrl Pts',(30.,-1.52706329386828,26.296875));
#64375=CARTESIAN_POINT('Ctrl Pts',(30.8816504037844,-1.52706329386828,26.3385416666667));
#64376=CARTESIAN_POINT('Ctrl Pts',(31.3224756056766,-0.763531646934147,
26.3802083333334));
#64377=CARTESIAN_POINT('Ctrl Pts',(31.7633008075689,-1.36198038370242E-14,
26.421875));
#64378=CARTESIAN_POINT('Ctrl Pts',(31.3224756056766,0.763531646934118,26.4635416666667));
#64379=CARTESIAN_POINT('Ctrl Pts',(30.8816504037844,1.52706329386825,26.5052083333334));
#64380=CARTESIAN_POINT('Ctrl Pts',(30.,1.52706329386825,26.546875));
#64381=CARTESIAN_POINT('Ctrl Pts',(29.1183495962155,1.52706329386825,26.5885416666667));
#64382=CARTESIAN_POINT('Ctrl Pts',(28.6775243943233,0.76353164693412,26.6302083333334));
#64383=CARTESIAN_POINT('Ctrl Pts',(28.2366991924311,-1.31894491186926E-14,
26.671875));
#64384=CARTESIAN_POINT('Ctrl Pts',(28.6775243943233,-0.763531646934146,
26.7135416666667));
#64385=CARTESIAN_POINT('Ctrl Pts',(29.1183495962155,-1.52706329386828,26.7552083333334));
#64386=CARTESIAN_POINT('Ctrl Pts',(30.,-1.52706329386828,26.796875));
#64387=CARTESIAN_POINT('Ctrl Pts',(30.8816504037844,-1.52706329386828,26.8385416666667));
#64388=CARTESIAN_POINT('Ctrl Pts',(31.3224756056766,-0.763531646934147,
26.8802083333334));
#64389=CARTESIAN_POINT('Ctrl Pts',(31.7633008075689,-1.36198038370242E-14,
26.921875));
#64390=CARTESIAN_POINT('Ctrl Pts',(31.3224756056766,0.763531646934118,26.9635416666667));
#64391=CARTESIAN_POINT('Ctrl Pts',(30.8816504037844,1.52706329386825,27.0052083333334));
#64392=CARTESIAN_POINT('Ctrl Pts',(30.,1.52706329386825,27.046875));
#64393=CARTESIAN_POINT('Ctrl Pts',(29.1183495962155,1.52706329386825,27.0885416666667));
#64394=CARTESIAN_POINT('Ctrl Pts',(28.6775243943233,0.76353164693412,27.1302083333334));
#64395=CARTESIAN_POINT('Ctrl Pts',(28.2366991924311,-1.31894491186926E-14,
27.171875));
#64396=CARTESIAN_POINT('Ctrl Pts',(28.6775243943233,-0.763531646934146,
27.2135416666667));
#64397=CARTESIAN_POINT('Ctrl Pts',(29.1183495962155,-1.52706329386828,27.2552083333334));
#64398=CARTESIAN_POINT('Ctrl Pts',(30.,-1.52706329386828,27.296875));
#64399=CARTESIAN_POINT('Ctrl Pts',(30.8816504037844,-1.52706329386828,27.3385416666667));
#64400=CARTESIAN_POINT('Ctrl Pts',(31.3224756056766,-0.763531646934147,
27.3802083333334));
#64401=CARTESIAN_POINT('Ctrl Pts',(31.7633008075689,-1.36198038370242E-14,
27.421875));
#64402=CARTESIAN_POINT('Ctrl Pts',(31.3224756056766,0.763531646934118,27.4635416666667));
#64403=CARTESIAN_POINT('Ctrl Pts',(30.8816504037844,1.52706329386825,27.5052083333334));
#64404=CARTESIAN_POINT('Ctrl Pts',(30.,1.52706329386825,27.546875));
#64405=CARTESIAN_POINT('Ctrl Pts',(29.1183495962155,1.52706329386825,27.5885416666667));
#64406=CARTESIAN_POINT('Ctrl Pts',(28.6775243943233,0.76353164693412,27.6302083333334));
#64407=CARTESIAN_POINT('Ctrl Pts',(28.2366991924311,-1.31894491186926E-14,
27.671875));
#64408=CARTESIAN_POINT('Ctrl Pts',(28.6775243943233,-0.763531646934146,
27.7135416666667));
#64409=CARTESIAN_POINT('Ctrl Pts',(29.1183495962155,-1.52706329386828,27.7552083333334));
#64410=CARTESIAN_POINT('Ctrl Pts',(30.,-1.52706329386828,27.796875));
#64411=CARTESIAN_POINT('Ctrl Pts',(30.8816504037844,-1.52706329386828,27.8385416666667));
#64412=CARTESIAN_POINT('Ctrl Pts',(31.3224756056766,-0.763531646934147,
27.8802083333334));
#64413=CARTESIAN_POINT('Ctrl Pts',(31.7633008075689,-1.36198038370242E-14,
27.921875));
#64414=CARTESIAN_POINT('Ctrl Pts',(31.3224756056766,0.763531646934118,27.9635416666667));
#64415=CARTESIAN_POINT('Ctrl Pts',(30.8816504037844,1.52706329386825,28.0052083333334));
#64416=CARTESIAN_POINT('Ctrl Pts',(30.,1.52706329386825,28.046875));
#64417=CARTESIAN_POINT('Ctrl Pts',(29.1183495962155,1.52706329386825,28.0885416666667));
#64418=CARTESIAN_POINT('Ctrl Pts',(28.6775243943233,0.76353164693412,28.1302083333334));
#64419=CARTESIAN_POINT('Ctrl Pts',(28.2366991924311,-1.31894491186926E-14,
28.171875));
#64420=CARTESIAN_POINT('Ctrl Pts',(28.6775243943233,-0.763531646934146,
28.2135416666667));
#64421=CARTESIAN_POINT('Ctrl Pts',(29.1183495962155,-1.52706329386828,28.2552083333334));
#64422=CARTESIAN_POINT('Ctrl Pts',(30.,-1.52706329386828,28.296875));
#64423=CARTESIAN_POINT('Ctrl Pts',(30.8816504037844,-1.52706329386828,28.3385416666667));
#64424=CARTESIAN_POINT('Ctrl Pts',(31.3224756056766,-0.763531646934147,
28.3802083333334));
#64425=CARTESIAN_POINT('Ctrl Pts',(31.7633008075689,-1.36198038370242E-14,
28.421875));
#64426=CARTESIAN_POINT('Ctrl Pts',(31.3224756056766,0.763531646934118,28.4635416666667));
#64427=CARTESIAN_POINT('Ctrl Pts',(30.8816504037844,1.52706329386825,28.5052083333334));
#64428=CARTESIAN_POINT('Ctrl Pts',(30.,1.52706329386825,28.546875));
#64429=CARTESIAN_POINT('Ctrl Pts',(29.1183495962155,1.52706329386825,28.5885416666667));
#64430=CARTESIAN_POINT('Ctrl Pts',(28.6775243943233,0.76353164693412,28.6302083333334));
#64431=CARTESIAN_POINT('Ctrl Pts',(28.2366991924311,-1.31894491186926E-14,
28.671875));
#64432=CARTESIAN_POINT('Ctrl Pts',(28.6775243943233,-0.763531646934146,
28.7135416666667));
#64433=CARTESIAN_POINT('Ctrl Pts',(29.1183495962155,-1.52706329386828,28.7552083333334));
#64434=CARTESIAN_POINT('Ctrl Pts',(30.,-1.52706329386828,28.796875));
#64435=CARTESIAN_POINT('Ctrl Pts',(30.8816504037844,-1.52706329386828,28.8385416666667));
#64436=CARTESIAN_POINT('Ctrl Pts',(31.3224756056766,-0.763531646934147,
28.8802083333334));
#64437=CARTESIAN_POINT('Ctrl Pts',(31.7633008075689,-1.36198038370242E-14,
28.921875));
#64438=CARTESIAN_POINT('Ctrl Pts',(31.3224756056766,0.763531646934118,28.9635416666667));
#64439=CARTESIAN_POINT('Ctrl Pts',(30.8816504037844,1.52706329386825,29.0052083333334));
#64440=CARTESIAN_POINT('Ctrl Pts',(30.,1.52706329386825,29.046875));
#64441=CARTESIAN_POINT('Ctrl Pts',(29.1183495962155,1.52706329386825,29.0885416666667));
#64442=CARTESIAN_POINT('Ctrl Pts',(28.6775243943233,0.76353164693412,29.1302083333334));
#64443=CARTESIAN_POINT('Ctrl Pts',(28.2366991924311,-1.31894491186926E-14,
29.171875));
#64444=CARTESIAN_POINT('Ctrl Pts',(28.6775243943233,-0.763531646934146,
29.2135416666667));
#64445=CARTESIAN_POINT('Ctrl Pts',(29.1183495962155,-1.52706329386828,29.2552083333334));
#64446=CARTESIAN_POINT('Ctrl Pts',(30.,-1.52706329386828,29.296875));
#64447=CARTESIAN_POINT('Ctrl Pts',(30.8816504037844,-1.52706329386828,29.3385416666667));
#64448=CARTESIAN_POINT('Ctrl Pts',(31.3224756056766,-0.763531646934147,
29.3802083333334));
#64449=CARTESIAN_POINT('Ctrl Pts',(31.7633008075689,-1.36198038370242E-14,
29.421875));
#64450=CARTESIAN_POINT('Ctrl Pts',(31.3224756056766,0.763531646934118,29.4635416666667));
#64451=CARTESIAN_POINT('Ctrl Pts',(30.8816504037844,1.52706329386825,29.5052083333334));
#64452=CARTESIAN_POINT('Ctrl Pts',(30.,1.52706329386825,29.546875));
#64453=CARTESIAN_POINT('Ctrl Pts',(29.1183495962155,1.52706329386825,29.5885416666667));
#64454=CARTESIAN_POINT('Ctrl Pts',(28.6775243943233,0.76353164693412,29.6302083333334));
#64455=CARTESIAN_POINT('Ctrl Pts',(28.2366991924311,-1.31894491186926E-14,
29.671875));
#64456=CARTESIAN_POINT('Ctrl Pts',(28.6775243943233,-0.763531646934146,
29.7135416666667));
#64457=CARTESIAN_POINT('Ctrl Pts',(29.1183495962155,-1.52706329386828,29.7552083333334));
#64458=CARTESIAN_POINT('Ctrl Pts',(30.,-1.52706329386828,29.796875));
#64459=CARTESIAN_POINT('Ctrl Pts',(30.8816504037844,-1.52706329386828,29.8385416666667));
#64460=CARTESIAN_POINT('Ctrl Pts',(31.3224756056766,-0.763531646934147,
29.8802083333334));
#64461=CARTESIAN_POINT('Ctrl Pts',(31.7633008075689,-1.36198038370242E-14,
29.921875));
#64462=CARTESIAN_POINT('Ctrl Pts',(31.3224756056766,0.763531646934118,29.9635416666667));
#64463=CARTESIAN_POINT('Ctrl Pts',(30.8816504037844,1.52706329386825,30.0052083333334));
#64464=CARTESIAN_POINT('Ctrl Pts',(30.,1.52706329386825,30.046875));
#64465=CARTESIAN_POINT('Ctrl Pts',(29.1183495962155,1.52706329386825,30.0885416666667));
#64466=CARTESIAN_POINT('Ctrl Pts',(28.6775243943233,0.76353164693412,30.1302083333334));
#64467=CARTESIAN_POINT('Ctrl Pts',(28.2366991924311,-1.31894491186926E-14,
30.171875));
#64468=CARTESIAN_POINT('Ctrl Pts',(28.6775243943233,-0.763531646934146,
30.2135416666667));
#64469=CARTESIAN_POINT('Ctrl Pts',(29.1183495962155,-1.52706329386828,30.2552083333334));
#64470=CARTESIAN_POINT('Ctrl Pts',(30.,-1.52706329386828,30.296875));
#64471=CARTESIAN_POINT('Ctrl Pts',(30.8816504037844,-1.52706329386828,30.3385416666667));
#64472=CARTESIAN_POINT('Ctrl Pts',(31.3224756056766,-0.763531646934147,
30.3802083333334));
#64473=CARTESIAN_POINT('Ctrl Pts',(31.7633008075689,-1.36198038370242E-14,
30.421875));
#64474=CARTESIAN_POINT('Ctrl Pts',(31.3224756056766,0.763531646934118,30.4635416666667));
#64475=CARTESIAN_POINT('Ctrl Pts',(30.8816504037844,1.52706329386825,30.5052083333334));
#64476=CARTESIAN_POINT('Ctrl Pts',(30.,1.52706329386825,30.546875));
#64477=CARTESIAN_POINT('Ctrl Pts',(29.1183495962155,1.52706329386825,30.5885416666667));
#64478=CARTESIAN_POINT('Ctrl Pts',(28.6775243943233,0.76353164693412,30.6302083333334));
#64479=CARTESIAN_POINT('Ctrl Pts',(28.2366991924311,-1.31894491186926E-14,
30.671875));
#64480=CARTESIAN_POINT('Ctrl Pts',(28.6775243943233,-0.763531646934146,
30.7135416666667));
#64481=CARTESIAN_POINT('Ctrl Pts',(29.1183495962155,-1.52706329386828,30.7552083333334));
#64482=CARTESIAN_POINT('Ctrl Pts',(30.,-1.52706329386828,30.796875));
#64483=CARTESIAN_POINT('Ctrl Pts',(30.8816504037844,-1.52706329386828,30.8385416666667));
#64484=CARTESIAN_POINT('Ctrl Pts',(31.3224756056766,-0.763531646934147,
30.8802083333334));
#64485=CARTESIAN_POINT('Ctrl Pts',(31.7633008075689,-1.36198038370242E-14,
30.921875));
#64486=CARTESIAN_POINT('Ctrl Pts',(31.3224756056766,0.763531646934118,30.9635416666667));
#64487=CARTESIAN_POINT('Ctrl Pts',(30.8816504037844,1.52706329386825,31.0052083333334));
#64488=CARTESIAN_POINT('Ctrl Pts',(30.,1.52706329386825,31.046875));
#64489=CARTESIAN_POINT('Ctrl Pts',(30.8234003400376,-0.838570603170131,
30.5624996575278));
#64490=CARTESIAN_POINT('Ctrl Pts',(30.9252409219315,-0.749808119816165,
30.5671289662449));
#64491=CARTESIAN_POINT('Ctrl Pts',(31.0094069192668,-0.645130506686946,
30.571193014068));
#64492=CARTESIAN_POINT('Ctrl Pts',(31.1396529784097,-0.412074319923831,
30.5795221820465));
#64493=CARTESIAN_POINT('Ctrl Pts',(31.1849584507844,-0.287685440765051,
30.5838904393726));
#64494=CARTESIAN_POINT('Ctrl Pts',(31.2386945750578,-0.00655181811616603,
30.5935664195233));
#64495=CARTESIAN_POINT('Ctrl Pts',(31.2387490550162,0.149503133824081,30.5988162542928));
#64496=CARTESIAN_POINT('Ctrl Pts',(31.1719223736106,0.500568259068406,30.610386374166));
#64497=CARTESIAN_POINT('Ctrl Pts',(31.0923154827319,0.652496494934345,30.6150433766711));
#64498=CARTESIAN_POINT('Ctrl Pts',(30.9283336729762,0.900293879400657,30.6239504439807));
#64499=CARTESIAN_POINT('Ctrl Pts',(30.8055598520391,1.02369588322745,30.6294622341334));
#64500=CARTESIAN_POINT('Ctrl Pts',(30.5288337282237,1.20882504193349,30.6401101417162));
#64501=CARTESIAN_POINT('Ctrl Pts',(30.3799906896905,1.27260041719159,30.6451552807199));
#64502=CARTESIAN_POINT('Ctrl Pts',(30.0014927028803,1.35728019461807,30.6565651904367));
#64503=CARTESIAN_POINT('Ctrl Pts',(29.8132785668206,1.33887636851719,30.6613880776071));
#64504=CARTESIAN_POINT('Ctrl Pts',(29.5198061598154,1.28660005614596,30.6701589170659));
#64505=CARTESIAN_POINT('Ctrl Pts',(29.3521505621284,1.22147978200258,30.6756096035631));
#64506=CARTESIAN_POINT('Ctrl Pts',(29.0485837866741,1.02916361274227,30.6863949411503));
#64507=CARTESIAN_POINT('Ctrl Pts',(28.9162494293832,0.902843317652004,30.6916208752244));
#64508=CARTESIAN_POINT('Ctrl Pts',(28.7272437086822,0.633185410868888,30.7002552651022));
#64509=CARTESIAN_POINT('Ctrl Pts',(28.6461891944724,0.476094037694283,30.7048351996635));
#64510=CARTESIAN_POINT('Ctrl Pts',(28.551105022901,0.105569064666544,30.715730913862));
#64511=CARTESIAN_POINT('Ctrl Pts',(28.5402826505383,-0.0831493783931786,
30.7211721595761));
#64512=CARTESIAN_POINT('Ctrl Pts',(28.5859138822382,-0.415083694084825,
30.7305650693331));
#64513=CARTESIAN_POINT('Ctrl Pts',(28.6283908398168,-0.557537406078615,
30.7345346397522));
#64514=CARTESIAN_POINT('Ctrl Pts',(28.7447696187018,-0.802908073480822,
30.7412906353098));
#64515=CARTESIAN_POINT('Ctrl Pts',(28.8264704242263,-0.938163811130005,
30.7451577422722));
#64516=CARTESIAN_POINT('Ctrl Pts',(28.9490560961683,-1.07028823734174,30.7500000000014));
#64517=CARTESIAN_POINT('Ctrl Pts',(30.,1.52706329386825,16.015625));
#64518=CARTESIAN_POINT('Ctrl Pts',(29.1183495962155,1.52706329386825,16.0572916666666));
#64519=CARTESIAN_POINT('Ctrl Pts',(28.6775243943233,0.76353164693412,16.0989583333333));
#64520=CARTESIAN_POINT('Ctrl Pts',(28.2366991924311,-1.31894491186926E-14,
16.140625));
#64521=CARTESIAN_POINT('Ctrl Pts',(28.6775243943233,-0.763531646934146,
16.1822916666666));
#64522=CARTESIAN_POINT('Ctrl Pts',(29.1183495962155,-1.52706329386828,16.2239583333333));
#64523=CARTESIAN_POINT('Ctrl Pts',(30.,-1.52706329386828,16.265625));
#64524=CARTESIAN_POINT('Ctrl Pts',(30.8816504037844,-1.52706329386828,16.3072916666666));
#64525=CARTESIAN_POINT('Ctrl Pts',(31.3224756056766,-0.763531646934147,
16.3489583333333));
#64526=CARTESIAN_POINT('Ctrl Pts',(31.7633008075689,-1.36198038370242E-14,
16.390625));
#64527=CARTESIAN_POINT('Ctrl Pts',(31.3224756056766,0.763531646934118,16.4322916666666));
#64528=CARTESIAN_POINT('Ctrl Pts',(30.8816504037844,1.52706329386825,16.4739583333333));
#64529=CARTESIAN_POINT('Ctrl Pts',(30.,1.52706329386825,16.515625));
#64530=CARTESIAN_POINT('Ctrl Pts',(29.1183495962155,1.52706329386825,16.5572916666666));
#64531=CARTESIAN_POINT('Ctrl Pts',(28.6775243943233,0.76353164693412,16.5989583333333));
#64532=CARTESIAN_POINT('Ctrl Pts',(28.2366991924311,-1.31894491186926E-14,
16.640625));
#64533=CARTESIAN_POINT('Ctrl Pts',(28.6775243943233,-0.763531646934146,
16.6822916666666));
#64534=CARTESIAN_POINT('Ctrl Pts',(29.1183495962155,-1.52706329386828,16.7239583333333));
#64535=CARTESIAN_POINT('Ctrl Pts',(30.,-1.52706329386828,16.765625));
#64536=CARTESIAN_POINT('Ctrl Pts',(30.8816504037844,-1.52706329386828,16.8072916666666));
#64537=CARTESIAN_POINT('Ctrl Pts',(31.3224756056766,-0.763531646934147,
16.8489583333333));
#64538=CARTESIAN_POINT('Ctrl Pts',(31.7633008075689,-1.36198038370242E-14,
16.890625));
#64539=CARTESIAN_POINT('Ctrl Pts',(31.3224756056766,0.763531646934118,16.9322916666666));
#64540=CARTESIAN_POINT('Ctrl Pts',(30.8816504037844,1.52706329386825,16.9739583333333));
#64541=CARTESIAN_POINT('Ctrl Pts',(30.,1.52706329386825,17.015625));
#64542=CARTESIAN_POINT('Ctrl Pts',(29.1183495962155,1.52706329386825,17.0572916666666));
#64543=CARTESIAN_POINT('Ctrl Pts',(28.6775243943233,0.76353164693412,17.0989583333333));
#64544=CARTESIAN_POINT('Ctrl Pts',(28.2366991924311,-1.31894491186926E-14,
17.140625));
#64545=CARTESIAN_POINT('Ctrl Pts',(28.6775243943233,-0.763531646934146,
17.1822916666666));
#64546=CARTESIAN_POINT('Ctrl Pts',(29.1183495962155,-1.52706329386828,17.2239583333333));
#64547=CARTESIAN_POINT('Ctrl Pts',(30.,-1.52706329386828,17.265625));
#64548=CARTESIAN_POINT('Ctrl Pts',(30.8816504037844,-1.52706329386828,17.3072916666666));
#64549=CARTESIAN_POINT('Ctrl Pts',(31.3224756056766,-0.763531646934147,
17.3489583333333));
#64550=CARTESIAN_POINT('Ctrl Pts',(31.7633008075689,-1.36198038370242E-14,
17.390625));
#64551=CARTESIAN_POINT('Ctrl Pts',(31.3224756056766,0.763531646934118,17.4322916666666));
#64552=CARTESIAN_POINT('Ctrl Pts',(30.8816504037844,1.52706329386825,17.4739583333333));
#64553=CARTESIAN_POINT('Ctrl Pts',(30.,1.52706329386825,17.515625));
#64554=CARTESIAN_POINT('Ctrl Pts',(29.1183495962155,1.52706329386825,17.5572916666666));
#64555=CARTESIAN_POINT('Ctrl Pts',(28.6775243943233,0.76353164693412,17.5989583333333));
#64556=CARTESIAN_POINT('Ctrl Pts',(28.2366991924311,-1.31894491186926E-14,
17.640625));
#64557=CARTESIAN_POINT('Ctrl Pts',(28.6775243943233,-0.763531646934146,
17.6822916666666));
#64558=CARTESIAN_POINT('Ctrl Pts',(29.1183495962155,-1.52706329386828,17.7239583333333));
#64559=CARTESIAN_POINT('Ctrl Pts',(30.,-1.52706329386828,17.765625));
#64560=CARTESIAN_POINT('Ctrl Pts',(30.8816504037844,-1.52706329386828,17.8072916666666));
#64561=CARTESIAN_POINT('Ctrl Pts',(31.3224756056766,-0.763531646934147,
17.8489583333333));
#64562=CARTESIAN_POINT('Ctrl Pts',(31.7633008075689,-1.36198038370242E-14,
17.890625));
#64563=CARTESIAN_POINT('Ctrl Pts',(31.3224756056766,0.763531646934118,17.9322916666666));
#64564=CARTESIAN_POINT('Ctrl Pts',(30.8816504037844,1.52706329386825,17.9739583333333));
#64565=CARTESIAN_POINT('Ctrl Pts',(30.,1.52706329386825,18.015625));
#64566=CARTESIAN_POINT('Ctrl Pts',(29.1183495962155,1.52706329386825,18.0572916666666));
#64567=CARTESIAN_POINT('Ctrl Pts',(28.6775243943233,0.76353164693412,18.0989583333333));
#64568=CARTESIAN_POINT('Ctrl Pts',(28.2366991924311,-1.31894491186926E-14,
18.140625));
#64569=CARTESIAN_POINT('Ctrl Pts',(28.6775243943233,-0.763531646934146,
18.1822916666666));
#64570=CARTESIAN_POINT('Ctrl Pts',(29.1183495962155,-1.52706329386828,18.2239583333333));
#64571=CARTESIAN_POINT('Ctrl Pts',(30.,-1.52706329386828,18.265625));
#64572=CARTESIAN_POINT('Ctrl Pts',(30.8816504037844,-1.52706329386828,18.3072916666666));
#64573=CARTESIAN_POINT('Ctrl Pts',(31.3224756056766,-0.763531646934147,
18.3489583333333));
#64574=CARTESIAN_POINT('Ctrl Pts',(31.7633008075689,-1.36198038370242E-14,
18.390625));
#64575=CARTESIAN_POINT('Ctrl Pts',(31.3224756056766,0.763531646934118,18.4322916666666));
#64576=CARTESIAN_POINT('Ctrl Pts',(30.8816504037844,1.52706329386825,18.4739583333333));
#64577=CARTESIAN_POINT('Ctrl Pts',(30.,1.52706329386825,18.515625));
#64578=CARTESIAN_POINT('Ctrl Pts',(29.1183495962155,1.52706329386825,18.5572916666666));
#64579=CARTESIAN_POINT('Ctrl Pts',(28.6775243943233,0.76353164693412,18.5989583333333));
#64580=CARTESIAN_POINT('Ctrl Pts',(28.2366991924311,-1.31894491186926E-14,
18.640625));
#64581=CARTESIAN_POINT('Ctrl Pts',(28.6775243943233,-0.763531646934146,
18.6822916666666));
#64582=CARTESIAN_POINT('Ctrl Pts',(29.1183495962155,-1.52706329386828,18.7239583333333));
#64583=CARTESIAN_POINT('Ctrl Pts',(30.,-1.52706329386828,18.765625));
#64584=CARTESIAN_POINT('Ctrl Pts',(30.8816504037844,-1.52706329386828,18.8072916666666));
#64585=CARTESIAN_POINT('Ctrl Pts',(31.3224756056766,-0.763531646934147,
18.8489583333333));
#64586=CARTESIAN_POINT('Ctrl Pts',(31.7633008075689,-1.36198038370242E-14,
18.890625));
#64587=CARTESIAN_POINT('Ctrl Pts',(31.3224756056766,0.763531646934118,18.9322916666666));
#64588=CARTESIAN_POINT('Ctrl Pts',(30.8816504037844,1.52706329386825,18.9739583333333));
#64589=CARTESIAN_POINT('Ctrl Pts',(30.,1.52706329386825,19.015625));
#64590=CARTESIAN_POINT('Ctrl Pts',(29.1183495962155,1.52706329386825,19.0572916666666));
#64591=CARTESIAN_POINT('Ctrl Pts',(28.6775243943233,0.76353164693412,19.0989583333333));
#64592=CARTESIAN_POINT('Ctrl Pts',(28.2366991924311,-1.31894491186926E-14,
19.140625));
#64593=CARTESIAN_POINT('Ctrl Pts',(28.6775243943233,-0.763531646934146,
19.1822916666666));
#64594=CARTESIAN_POINT('Ctrl Pts',(29.1183495962155,-1.52706329386828,19.2239583333333));
#64595=CARTESIAN_POINT('Ctrl Pts',(30.,-1.52706329386828,19.265625));
#64596=CARTESIAN_POINT('Ctrl Pts',(30.8816504037844,-1.52706329386828,19.3072916666666));
#64597=CARTESIAN_POINT('Ctrl Pts',(31.3224756056766,-0.763531646934147,
19.3489583333333));
#64598=CARTESIAN_POINT('Ctrl Pts',(31.7633008075689,-1.36198038370242E-14,
19.390625));
#64599=CARTESIAN_POINT('Ctrl Pts',(31.3224756056766,0.763531646934118,19.4322916666666));
#64600=CARTESIAN_POINT('Ctrl Pts',(30.8816504037844,1.52706329386825,19.4739583333333));
#64601=CARTESIAN_POINT('Ctrl Pts',(30.,1.52706329386825,19.515625));
#64602=CARTESIAN_POINT('Ctrl Pts',(29.1183495962155,1.52706329386825,19.5572916666666));
#64603=CARTESIAN_POINT('Ctrl Pts',(28.6775243943233,0.76353164693412,19.5989583333333));
#64604=CARTESIAN_POINT('Ctrl Pts',(28.2366991924311,-1.31894491186926E-14,
19.640625));
#64605=CARTESIAN_POINT('Ctrl Pts',(28.6775243943233,-0.763531646934146,
19.6822916666666));
#64606=CARTESIAN_POINT('Ctrl Pts',(29.1183495962155,-1.52706329386828,19.7239583333333));
#64607=CARTESIAN_POINT('Ctrl Pts',(30.,-1.52706329386828,19.765625));
#64608=CARTESIAN_POINT('Ctrl Pts',(30.8816504037844,-1.52706329386828,19.8072916666666));
#64609=CARTESIAN_POINT('Ctrl Pts',(31.3224756056766,-0.763531646934147,
19.8489583333333));
#64610=CARTESIAN_POINT('Ctrl Pts',(31.7633008075689,-1.36198038370242E-14,
19.890625));
#64611=CARTESIAN_POINT('Ctrl Pts',(31.3224756056766,0.763531646934118,19.9322916666666));
#64612=CARTESIAN_POINT('Ctrl Pts',(30.8816504037844,1.52706329386825,19.9739583333333));
#64613=CARTESIAN_POINT('Ctrl Pts',(30.,1.52706329386825,20.015625));
#64614=CARTESIAN_POINT('Ctrl Pts',(29.1183495962155,1.52706329386825,20.0572916666666));
#64615=CARTESIAN_POINT('Ctrl Pts',(28.6775243943233,0.76353164693412,20.0989583333333));
#64616=CARTESIAN_POINT('Ctrl Pts',(28.2366991924311,-1.31894491186926E-14,
20.140625));
#64617=CARTESIAN_POINT('Ctrl Pts',(28.6775243943233,-0.763531646934146,
20.1822916666666));
#64618=CARTESIAN_POINT('Ctrl Pts',(29.1183495962155,-1.52706329386828,20.2239583333333));
#64619=CARTESIAN_POINT('Ctrl Pts',(30.,-1.52706329386828,20.265625));
#64620=CARTESIAN_POINT('Ctrl Pts',(30.8816504037844,-1.52706329386828,20.3072916666666));
#64621=CARTESIAN_POINT('Ctrl Pts',(31.3224756056766,-0.763531646934147,
20.3489583333333));
#64622=CARTESIAN_POINT('Ctrl Pts',(31.7633008075689,-1.36198038370242E-14,
20.390625));
#64623=CARTESIAN_POINT('Ctrl Pts',(31.3224756056766,0.763531646934118,20.4322916666666));
#64624=CARTESIAN_POINT('Ctrl Pts',(30.8816504037844,1.52706329386825,20.4739583333333));
#64625=CARTESIAN_POINT('Ctrl Pts',(30.,1.52706329386825,20.515625));
#64626=CARTESIAN_POINT('Ctrl Pts',(29.1183495962155,1.52706329386825,20.5572916666666));
#64627=CARTESIAN_POINT('Ctrl Pts',(28.6775243943233,0.76353164693412,20.5989583333333));
#64628=CARTESIAN_POINT('Ctrl Pts',(28.2366991924311,-1.31894491186926E-14,
20.640625));
#64629=CARTESIAN_POINT('Ctrl Pts',(28.6775243943233,-0.763531646934146,
20.6822916666666));
#64630=CARTESIAN_POINT('Ctrl Pts',(29.1183495962155,-1.52706329386828,20.7239583333333));
#64631=CARTESIAN_POINT('Ctrl Pts',(30.,-1.52706329386828,20.765625));
#64632=CARTESIAN_POINT('Ctrl Pts',(30.8816504037844,-1.52706329386828,20.8072916666666));
#64633=CARTESIAN_POINT('Ctrl Pts',(31.3224756056766,-0.763531646934147,
20.8489583333333));
#64634=CARTESIAN_POINT('Ctrl Pts',(31.7633008075689,-1.36198038370242E-14,
20.890625));
#64635=CARTESIAN_POINT('Ctrl Pts',(31.3224756056766,0.763531646934118,20.9322916666666));
#64636=CARTESIAN_POINT('Ctrl Pts',(30.8816504037844,1.52706329386825,20.9739583333333));
#64637=CARTESIAN_POINT('Ctrl Pts',(30.,1.52706329386825,21.015625));
#64638=CARTESIAN_POINT('Ctrl Pts',(29.1183495962155,1.52706329386825,21.0572916666666));
#64639=CARTESIAN_POINT('Ctrl Pts',(28.6775243943233,0.76353164693412,21.0989583333333));
#64640=CARTESIAN_POINT('Ctrl Pts',(28.2366991924311,-1.31894491186926E-14,
21.140625));
#64641=CARTESIAN_POINT('Ctrl Pts',(28.6775243943233,-0.763531646934146,
21.1822916666666));
#64642=CARTESIAN_POINT('Ctrl Pts',(29.1183495962155,-1.52706329386828,21.2239583333333));
#64643=CARTESIAN_POINT('Ctrl Pts',(30.,-1.52706329386828,21.265625));
#64644=CARTESIAN_POINT('Ctrl Pts',(30.8816504037844,-1.52706329386828,21.3072916666666));
#64645=CARTESIAN_POINT('Ctrl Pts',(31.3224756056766,-0.763531646934147,
21.3489583333333));
#64646=CARTESIAN_POINT('Ctrl Pts',(31.7633008075689,-1.36198038370242E-14,
21.390625));
#64647=CARTESIAN_POINT('Ctrl Pts',(31.3224756056766,0.763531646934118,21.4322916666666));
#64648=CARTESIAN_POINT('Ctrl Pts',(30.8816504037844,1.52706329386825,21.4739583333333));
#64649=CARTESIAN_POINT('Ctrl Pts',(30.,1.52706329386825,21.515625));
#64650=CARTESIAN_POINT('Ctrl Pts',(29.1183495962155,1.52706329386825,21.5572916666666));
#64651=CARTESIAN_POINT('Ctrl Pts',(28.6775243943233,0.76353164693412,21.5989583333333));
#64652=CARTESIAN_POINT('Ctrl Pts',(28.2366991924311,-1.31894491186926E-14,
21.640625));
#64653=CARTESIAN_POINT('Ctrl Pts',(28.6775243943233,-0.763531646934146,
21.6822916666666));
#64654=CARTESIAN_POINT('Ctrl Pts',(29.1183495962155,-1.52706329386828,21.7239583333333));
#64655=CARTESIAN_POINT('Ctrl Pts',(30.,-1.52706329386828,21.765625));
#64656=CARTESIAN_POINT('Ctrl Pts',(30.8816504037844,-1.52706329386828,21.8072916666666));
#64657=CARTESIAN_POINT('Ctrl Pts',(31.3224756056766,-0.763531646934147,
21.8489583333333));
#64658=CARTESIAN_POINT('Ctrl Pts',(31.7633008075689,-1.36198038370242E-14,
21.890625));
#64659=CARTESIAN_POINT('Ctrl Pts',(31.3224756056766,0.763531646934118,21.9322916666666));
#64660=CARTESIAN_POINT('Ctrl Pts',(30.8816504037844,1.52706329386825,21.9739583333333));
#64661=CARTESIAN_POINT('Ctrl Pts',(30.,1.52706329386825,22.015625));
#64662=CARTESIAN_POINT('Ctrl Pts',(29.1183495962155,1.52706329386825,22.0572916666666));
#64663=CARTESIAN_POINT('Ctrl Pts',(28.6775243943233,0.76353164693412,22.0989583333333));
#64664=CARTESIAN_POINT('Ctrl Pts',(28.2366991924311,-1.31894491186926E-14,
22.140625));
#64665=CARTESIAN_POINT('Ctrl Pts',(28.6775243943233,-0.763531646934146,
22.1822916666666));
#64666=CARTESIAN_POINT('Ctrl Pts',(29.1183495962155,-1.52706329386828,22.2239583333333));
#64667=CARTESIAN_POINT('Ctrl Pts',(30.,-1.52706329386828,22.265625));
#64668=CARTESIAN_POINT('Ctrl Pts',(30.8816504037844,-1.52706329386828,22.3072916666666));
#64669=CARTESIAN_POINT('Ctrl Pts',(31.3224756056766,-0.763531646934147,
22.3489583333333));
#64670=CARTESIAN_POINT('Ctrl Pts',(31.7633008075689,-1.36198038370242E-14,
22.390625));
#64671=CARTESIAN_POINT('Ctrl Pts',(31.3224756056766,0.763531646934118,22.4322916666666));
#64672=CARTESIAN_POINT('Ctrl Pts',(30.8816504037844,1.52706329386825,22.4739583333333));
#64673=CARTESIAN_POINT('Ctrl Pts',(30.,1.52706329386825,22.515625));
#64674=CARTESIAN_POINT('Ctrl Pts',(29.1183495962155,1.52706329386825,22.5572916666666));
#64675=CARTESIAN_POINT('Ctrl Pts',(28.6775243943233,0.76353164693412,22.5989583333333));
#64676=CARTESIAN_POINT('Ctrl Pts',(28.2366991924311,-1.31894491186926E-14,
22.640625));
#64677=CARTESIAN_POINT('Ctrl Pts',(28.6775243943233,-0.763531646934146,
22.6822916666666));
#64678=CARTESIAN_POINT('Ctrl Pts',(29.1183495962155,-1.52706329386828,22.7239583333333));
#64679=CARTESIAN_POINT('Ctrl Pts',(30.,-1.52706329386828,22.765625));
#64680=CARTESIAN_POINT('Ctrl Pts',(30.8816504037844,-1.52706329386828,22.8072916666666));
#64681=CARTESIAN_POINT('Ctrl Pts',(31.3224756056766,-0.763531646934147,
22.8489583333333));
#64682=CARTESIAN_POINT('Ctrl Pts',(31.7633008075689,-1.36198038370242E-14,
22.890625));
#64683=CARTESIAN_POINT('Ctrl Pts',(31.3224756056766,0.763531646934118,22.9322916666666));
#64684=CARTESIAN_POINT('Ctrl Pts',(30.8816504037844,1.52706329386825,22.9739583333333));
#64685=CARTESIAN_POINT('Ctrl Pts',(30.,1.52706329386825,23.015625));
#64686=CARTESIAN_POINT('Ctrl Pts',(29.1183495962155,1.52706329386825,23.0572916666666));
#64687=CARTESIAN_POINT('Ctrl Pts',(28.6775243943233,0.76353164693412,23.0989583333333));
#64688=CARTESIAN_POINT('Ctrl Pts',(28.2366991924311,-1.31894491186926E-14,
23.140625));
#64689=CARTESIAN_POINT('Ctrl Pts',(28.6775243943233,-0.763531646934146,
23.1822916666666));
#64690=CARTESIAN_POINT('Ctrl Pts',(29.1183495962155,-1.52706329386828,23.2239583333333));
#64691=CARTESIAN_POINT('Ctrl Pts',(30.,-1.52706329386828,23.265625));
#64692=CARTESIAN_POINT('Ctrl Pts',(30.8816504037844,-1.52706329386828,23.3072916666666));
#64693=CARTESIAN_POINT('Ctrl Pts',(31.3224756056766,-0.763531646934147,
23.3489583333333));
#64694=CARTESIAN_POINT('Ctrl Pts',(31.7633008075689,-1.36198038370242E-14,
23.390625));
#64695=CARTESIAN_POINT('Ctrl Pts',(31.3224756056766,0.763531646934118,23.4322916666666));
#64696=CARTESIAN_POINT('Ctrl Pts',(30.8816504037844,1.52706329386825,23.4739583333333));
#64697=CARTESIAN_POINT('Ctrl Pts',(30.,1.52706329386825,23.515625));
#64698=CARTESIAN_POINT('Ctrl Pts',(29.1183495962155,1.52706329386825,23.5572916666666));
#64699=CARTESIAN_POINT('Ctrl Pts',(28.6775243943233,0.76353164693412,23.5989583333333));
#64700=CARTESIAN_POINT('Ctrl Pts',(28.2366991924311,-1.31894491186926E-14,
23.640625));
#64701=CARTESIAN_POINT('Ctrl Pts',(28.6775243943233,-0.763531646934146,
23.6822916666666));
#64702=CARTESIAN_POINT('Ctrl Pts',(29.1183495962155,-1.52706329386828,23.7239583333333));
#64703=CARTESIAN_POINT('Ctrl Pts',(30.,-1.52706329386828,23.765625));
#64704=CARTESIAN_POINT('Ctrl Pts',(30.8816504037844,-1.52706329386828,23.8072916666666));
#64705=CARTESIAN_POINT('Ctrl Pts',(31.3224756056766,-0.763531646934147,
23.8489583333333));
#64706=CARTESIAN_POINT('Ctrl Pts',(31.7633008075689,-1.36198038370242E-14,
23.890625));
#64707=CARTESIAN_POINT('Ctrl Pts',(31.3224756056766,0.763531646934118,23.9322916666666));
#64708=CARTESIAN_POINT('Ctrl Pts',(30.8816504037844,1.52706329386825,23.9739583333333));
#64709=CARTESIAN_POINT('Ctrl Pts',(30.,1.52706329386825,24.015625));
#64710=CARTESIAN_POINT('Ctrl Pts',(29.1183495962155,1.52706329386825,24.0572916666666));
#64711=CARTESIAN_POINT('Ctrl Pts',(28.6775243943233,0.76353164693412,24.0989583333333));
#64712=CARTESIAN_POINT('Ctrl Pts',(28.2366991924311,-1.31894491186926E-14,
24.140625));
#64713=CARTESIAN_POINT('Ctrl Pts',(28.6775243943233,-0.763531646934146,
24.1822916666666));
#64714=CARTESIAN_POINT('Ctrl Pts',(29.1183495962155,-1.52706329386828,24.2239583333333));
#64715=CARTESIAN_POINT('Ctrl Pts',(30.,-1.52706329386828,24.265625));
#64716=CARTESIAN_POINT('Ctrl Pts',(30.8816504037844,-1.52706329386828,24.3072916666666));
#64717=CARTESIAN_POINT('Ctrl Pts',(31.3224756056766,-0.763531646934147,
24.3489583333333));
#64718=CARTESIAN_POINT('Ctrl Pts',(31.7633008075689,-1.36198038370242E-14,
24.390625));
#64719=CARTESIAN_POINT('Ctrl Pts',(31.3224756056766,0.763531646934118,24.4322916666666));
#64720=CARTESIAN_POINT('Ctrl Pts',(30.8816504037844,1.52706329386825,24.4739583333333));
#64721=CARTESIAN_POINT('Ctrl Pts',(30.,1.52706329386825,24.515625));
#64722=CARTESIAN_POINT('Ctrl Pts',(29.1183495962155,1.52706329386825,24.5572916666666));
#64723=CARTESIAN_POINT('Ctrl Pts',(28.6775243943233,0.76353164693412,24.5989583333333));
#64724=CARTESIAN_POINT('Ctrl Pts',(28.2366991924311,-1.31894491186926E-14,
24.640625));
#64725=CARTESIAN_POINT('Ctrl Pts',(28.6775243943233,-0.763531646934146,
24.6822916666666));
#64726=CARTESIAN_POINT('Ctrl Pts',(29.1183495962155,-1.52706329386828,24.7239583333333));
#64727=CARTESIAN_POINT('Ctrl Pts',(30.,-1.52706329386828,24.765625));
#64728=CARTESIAN_POINT('Ctrl Pts',(30.8816504037844,-1.52706329386828,24.8072916666666));
#64729=CARTESIAN_POINT('Ctrl Pts',(31.3224756056766,-0.763531646934147,
24.8489583333333));
#64730=CARTESIAN_POINT('Ctrl Pts',(31.7633008075689,-1.36198038370242E-14,
24.890625));
#64731=CARTESIAN_POINT('Ctrl Pts',(31.3224756056766,0.763531646934118,24.9322916666666));
#64732=CARTESIAN_POINT('Ctrl Pts',(30.8816504037844,1.52706329386825,24.9739583333333));
#64733=CARTESIAN_POINT('Ctrl Pts',(30.,1.52706329386825,25.015625));
#64734=CARTESIAN_POINT('Ctrl Pts',(29.1183495962155,1.52706329386825,25.0572916666666));
#64735=CARTESIAN_POINT('Ctrl Pts',(28.6775243943233,0.76353164693412,25.0989583333333));
#64736=CARTESIAN_POINT('Ctrl Pts',(28.2366991924311,-1.31894491186926E-14,
25.140625));
#64737=CARTESIAN_POINT('Ctrl Pts',(28.6775243943233,-0.763531646934146,
25.1822916666666));
#64738=CARTESIAN_POINT('Ctrl Pts',(29.1183495962155,-1.52706329386828,25.2239583333333));
#64739=CARTESIAN_POINT('Ctrl Pts',(30.,-1.52706329386828,25.265625));
#64740=CARTESIAN_POINT('Ctrl Pts',(30.8816504037844,-1.52706329386828,25.3072916666666));
#64741=CARTESIAN_POINT('Ctrl Pts',(31.3224756056766,-0.763531646934147,
25.3489583333333));
#64742=CARTESIAN_POINT('Ctrl Pts',(31.7633008075689,-1.36198038370242E-14,
25.390625));
#64743=CARTESIAN_POINT('Ctrl Pts',(31.3224756056766,0.763531646934118,25.4322916666666));
#64744=CARTESIAN_POINT('Ctrl Pts',(30.8816504037844,1.52706329386825,25.4739583333333));
#64745=CARTESIAN_POINT('Ctrl Pts',(30.,1.52706329386825,25.515625));
#64746=CARTESIAN_POINT('Ctrl Pts',(29.1183495962155,1.52706329386825,25.5572916666666));
#64747=CARTESIAN_POINT('Ctrl Pts',(28.6775243943233,0.76353164693412,25.5989583333333));
#64748=CARTESIAN_POINT('Ctrl Pts',(28.2366991924311,-1.31894491186926E-14,
25.640625));
#64749=CARTESIAN_POINT('Ctrl Pts',(28.6775243943233,-0.763531646934146,
25.6822916666666));
#64750=CARTESIAN_POINT('Ctrl Pts',(29.1183495962155,-1.52706329386828,25.7239583333333));
#64751=CARTESIAN_POINT('Ctrl Pts',(30.,-1.52706329386828,25.765625));
#64752=CARTESIAN_POINT('Ctrl Pts',(30.8816504037844,-1.52706329386828,25.8072916666666));
#64753=CARTESIAN_POINT('Ctrl Pts',(31.3224756056766,-0.763531646934147,
25.8489583333333));
#64754=CARTESIAN_POINT('Ctrl Pts',(31.7633008075689,-1.36198038370242E-14,
25.890625));
#64755=CARTESIAN_POINT('Ctrl Pts',(31.3224756056766,0.763531646934118,25.9322916666666));
#64756=CARTESIAN_POINT('Ctrl Pts',(30.8816504037844,1.52706329386825,25.9739583333333));
#64757=CARTESIAN_POINT('Ctrl Pts',(30.,1.52706329386825,26.015625));
#64758=CARTESIAN_POINT('Ctrl Pts',(29.1183495962155,1.52706329386825,26.0572916666666));
#64759=CARTESIAN_POINT('Ctrl Pts',(28.6775243943233,0.76353164693412,26.0989583333333));
#64760=CARTESIAN_POINT('Ctrl Pts',(28.2366991924311,-1.31894491186926E-14,
26.140625));
#64761=CARTESIAN_POINT('Ctrl Pts',(28.6775243943233,-0.763531646934146,
26.1822916666666));
#64762=CARTESIAN_POINT('Ctrl Pts',(29.1183495962155,-1.52706329386828,26.2239583333333));
#64763=CARTESIAN_POINT('Ctrl Pts',(30.,-1.52706329386828,26.265625));
#64764=CARTESIAN_POINT('Ctrl Pts',(30.8816504037844,-1.52706329386828,26.3072916666666));
#64765=CARTESIAN_POINT('Ctrl Pts',(31.3224756056766,-0.763531646934147,
26.3489583333333));
#64766=CARTESIAN_POINT('Ctrl Pts',(31.7633008075689,-1.36198038370242E-14,
26.390625));
#64767=CARTESIAN_POINT('Ctrl Pts',(31.3224756056766,0.763531646934118,26.4322916666666));
#64768=CARTESIAN_POINT('Ctrl Pts',(30.8816504037844,1.52706329386825,26.4739583333333));
#64769=CARTESIAN_POINT('Ctrl Pts',(30.,1.52706329386825,26.515625));
#64770=CARTESIAN_POINT('Ctrl Pts',(29.1183495962155,1.52706329386825,26.5572916666666));
#64771=CARTESIAN_POINT('Ctrl Pts',(28.6775243943233,0.76353164693412,26.5989583333333));
#64772=CARTESIAN_POINT('Ctrl Pts',(28.2366991924311,-1.31894491186926E-14,
26.640625));
#64773=CARTESIAN_POINT('Ctrl Pts',(28.6775243943233,-0.763531646934146,
26.6822916666666));
#64774=CARTESIAN_POINT('Ctrl Pts',(29.1183495962155,-1.52706329386828,26.7239583333333));
#64775=CARTESIAN_POINT('Ctrl Pts',(30.,-1.52706329386828,26.765625));
#64776=CARTESIAN_POINT('Ctrl Pts',(30.8816504037844,-1.52706329386828,26.8072916666666));
#64777=CARTESIAN_POINT('Ctrl Pts',(31.3224756056766,-0.763531646934147,
26.8489583333333));
#64778=CARTESIAN_POINT('Ctrl Pts',(31.7633008075689,-1.36198038370242E-14,
26.890625));
#64779=CARTESIAN_POINT('Ctrl Pts',(31.3224756056766,0.763531646934118,26.9322916666666));
#64780=CARTESIAN_POINT('Ctrl Pts',(30.8816504037844,1.52706329386825,26.9739583333333));
#64781=CARTESIAN_POINT('Ctrl Pts',(30.,1.52706329386825,27.015625));
#64782=CARTESIAN_POINT('Ctrl Pts',(29.1183495962155,1.52706329386825,27.0572916666666));
#64783=CARTESIAN_POINT('Ctrl Pts',(28.6775243943233,0.76353164693412,27.0989583333333));
#64784=CARTESIAN_POINT('Ctrl Pts',(28.2366991924311,-1.31894491186926E-14,
27.140625));
#64785=CARTESIAN_POINT('Ctrl Pts',(28.6775243943233,-0.763531646934146,
27.1822916666666));
#64786=CARTESIAN_POINT('Ctrl Pts',(29.1183495962155,-1.52706329386828,27.2239583333333));
#64787=CARTESIAN_POINT('Ctrl Pts',(30.,-1.52706329386828,27.265625));
#64788=CARTESIAN_POINT('Ctrl Pts',(30.8816504037844,-1.52706329386828,27.3072916666666));
#64789=CARTESIAN_POINT('Ctrl Pts',(31.3224756056766,-0.763531646934147,
27.3489583333333));
#64790=CARTESIAN_POINT('Ctrl Pts',(31.7633008075689,-1.36198038370242E-14,
27.390625));
#64791=CARTESIAN_POINT('Ctrl Pts',(31.3224756056766,0.763531646934118,27.4322916666666));
#64792=CARTESIAN_POINT('Ctrl Pts',(30.8816504037844,1.52706329386825,27.4739583333333));
#64793=CARTESIAN_POINT('Ctrl Pts',(30.,1.52706329386825,27.515625));
#64794=CARTESIAN_POINT('Ctrl Pts',(29.1183495962155,1.52706329386825,27.5572916666666));
#64795=CARTESIAN_POINT('Ctrl Pts',(28.6775243943233,0.76353164693412,27.5989583333333));
#64796=CARTESIAN_POINT('Ctrl Pts',(28.2366991924311,-1.31894491186926E-14,
27.640625));
#64797=CARTESIAN_POINT('Ctrl Pts',(28.6775243943233,-0.763531646934146,
27.6822916666666));
#64798=CARTESIAN_POINT('Ctrl Pts',(29.1183495962155,-1.52706329386828,27.7239583333333));
#64799=CARTESIAN_POINT('Ctrl Pts',(30.,-1.52706329386828,27.765625));
#64800=CARTESIAN_POINT('Ctrl Pts',(30.8816504037844,-1.52706329386828,27.8072916666666));
#64801=CARTESIAN_POINT('Ctrl Pts',(31.3224756056766,-0.763531646934147,
27.8489583333333));
#64802=CARTESIAN_POINT('Ctrl Pts',(31.7633008075689,-1.36198038370242E-14,
27.890625));
#64803=CARTESIAN_POINT('Ctrl Pts',(31.3224756056766,0.763531646934118,27.9322916666666));
#64804=CARTESIAN_POINT('Ctrl Pts',(30.8816504037844,1.52706329386825,27.9739583333333));
#64805=CARTESIAN_POINT('Ctrl Pts',(30.,1.52706329386825,28.015625));
#64806=CARTESIAN_POINT('Ctrl Pts',(29.1183495962155,1.52706329386825,28.0572916666666));
#64807=CARTESIAN_POINT('Ctrl Pts',(28.6775243943233,0.76353164693412,28.0989583333333));
#64808=CARTESIAN_POINT('Ctrl Pts',(28.2366991924311,-1.31894491186926E-14,
28.140625));
#64809=CARTESIAN_POINT('Ctrl Pts',(28.6775243943233,-0.763531646934146,
28.1822916666666));
#64810=CARTESIAN_POINT('Ctrl Pts',(29.1183495962155,-1.52706329386828,28.2239583333333));
#64811=CARTESIAN_POINT('Ctrl Pts',(30.,-1.52706329386828,28.265625));
#64812=CARTESIAN_POINT('Ctrl Pts',(30.8816504037844,-1.52706329386828,28.3072916666666));
#64813=CARTESIAN_POINT('Ctrl Pts',(31.3224756056766,-0.763531646934147,
28.3489583333333));
#64814=CARTESIAN_POINT('Ctrl Pts',(31.7633008075689,-1.36198038370242E-14,
28.390625));
#64815=CARTESIAN_POINT('Ctrl Pts',(31.3224756056766,0.763531646934118,28.4322916666666));
#64816=CARTESIAN_POINT('Ctrl Pts',(30.8816504037844,1.52706329386825,28.4739583333333));
#64817=CARTESIAN_POINT('Ctrl Pts',(30.,1.52706329386825,28.515625));
#64818=CARTESIAN_POINT('Ctrl Pts',(29.1183495962155,1.52706329386825,28.5572916666666));
#64819=CARTESIAN_POINT('Ctrl Pts',(28.6775243943233,0.76353164693412,28.5989583333333));
#64820=CARTESIAN_POINT('Ctrl Pts',(28.2366991924311,-1.31894491186926E-14,
28.640625));
#64821=CARTESIAN_POINT('Ctrl Pts',(28.6775243943233,-0.763531646934146,
28.6822916666666));
#64822=CARTESIAN_POINT('Ctrl Pts',(29.1183495962155,-1.52706329386828,28.7239583333333));
#64823=CARTESIAN_POINT('Ctrl Pts',(30.,-1.52706329386828,28.765625));
#64824=CARTESIAN_POINT('Ctrl Pts',(30.8816504037844,-1.52706329386828,28.8072916666666));
#64825=CARTESIAN_POINT('Ctrl Pts',(31.3224756056766,-0.763531646934147,
28.8489583333333));
#64826=CARTESIAN_POINT('Ctrl Pts',(31.7633008075689,-1.36198038370242E-14,
28.890625));
#64827=CARTESIAN_POINT('Ctrl Pts',(31.3224756056766,0.763531646934118,28.9322916666666));
#64828=CARTESIAN_POINT('Ctrl Pts',(30.8816504037844,1.52706329386825,28.9739583333333));
#64829=CARTESIAN_POINT('Ctrl Pts',(30.,1.52706329386825,29.015625));
#64830=CARTESIAN_POINT('Ctrl Pts',(29.1183495962155,1.52706329386825,29.0572916666666));
#64831=CARTESIAN_POINT('Ctrl Pts',(28.6775243943233,0.76353164693412,29.0989583333333));
#64832=CARTESIAN_POINT('Ctrl Pts',(28.2366991924311,-1.31894491186926E-14,
29.140625));
#64833=CARTESIAN_POINT('Ctrl Pts',(28.6775243943233,-0.763531646934146,
29.1822916666666));
#64834=CARTESIAN_POINT('Ctrl Pts',(29.1183495962155,-1.52706329386828,29.2239583333333));
#64835=CARTESIAN_POINT('Ctrl Pts',(30.,-1.52706329386828,29.265625));
#64836=CARTESIAN_POINT('Ctrl Pts',(30.8816504037844,-1.52706329386828,29.3072916666666));
#64837=CARTESIAN_POINT('Ctrl Pts',(31.3224756056766,-0.763531646934147,
29.3489583333333));
#64838=CARTESIAN_POINT('Ctrl Pts',(31.7633008075689,-1.36198038370242E-14,
29.390625));
#64839=CARTESIAN_POINT('Ctrl Pts',(31.3224756056766,0.763531646934118,29.4322916666666));
#64840=CARTESIAN_POINT('Ctrl Pts',(30.8816504037844,1.52706329386825,29.4739583333333));
#64841=CARTESIAN_POINT('Ctrl Pts',(30.,1.52706329386825,29.515625));
#64842=CARTESIAN_POINT('Ctrl Pts',(29.1183495962155,1.52706329386825,29.5572916666666));
#64843=CARTESIAN_POINT('Ctrl Pts',(28.6775243943233,0.76353164693412,29.5989583333333));
#64844=CARTESIAN_POINT('Ctrl Pts',(28.2366991924311,-1.31894491186926E-14,
29.640625));
#64845=CARTESIAN_POINT('Ctrl Pts',(28.6775243943233,-0.763531646934146,
29.6822916666666));
#64846=CARTESIAN_POINT('Ctrl Pts',(29.1183495962155,-1.52706329386828,29.7239583333333));
#64847=CARTESIAN_POINT('Ctrl Pts',(30.,-1.52706329386828,29.765625));
#64848=CARTESIAN_POINT('Ctrl Pts',(30.8816504037844,-1.52706329386828,29.8072916666666));
#64849=CARTESIAN_POINT('Ctrl Pts',(31.3224756056766,-0.763531646934147,
29.8489583333333));
#64850=CARTESIAN_POINT('Ctrl Pts',(31.7633008075689,-1.36198038370242E-14,
29.890625));
#64851=CARTESIAN_POINT('Ctrl Pts',(31.3224756056766,0.763531646934118,29.9322916666666));
#64852=CARTESIAN_POINT('Ctrl Pts',(30.8816504037844,1.52706329386825,29.9739583333333));
#64853=CARTESIAN_POINT('Ctrl Pts',(30.,1.52706329386825,30.015625));
#64854=CARTESIAN_POINT('Ctrl Pts',(29.1183495962155,1.52706329386825,30.0572916666666));
#64855=CARTESIAN_POINT('Ctrl Pts',(28.6775243943233,0.76353164693412,30.0989583333333));
#64856=CARTESIAN_POINT('Ctrl Pts',(28.2366991924311,-1.31894491186926E-14,
30.140625));
#64857=CARTESIAN_POINT('Ctrl Pts',(28.6775243943233,-0.763531646934146,
30.1822916666666));
#64858=CARTESIAN_POINT('Ctrl Pts',(29.1183495962155,-1.52706329386828,30.2239583333333));
#64859=CARTESIAN_POINT('Ctrl Pts',(30.,-1.52706329386828,30.265625));
#64860=CARTESIAN_POINT('Ctrl Pts',(30.8816504037844,-1.52706329386828,30.3072916666666));
#64861=CARTESIAN_POINT('Ctrl Pts',(31.3224756056766,-0.763531646934147,
30.3489583333333));
#64862=CARTESIAN_POINT('Ctrl Pts',(31.7633008075689,-1.36198038370242E-14,
30.390625));
#64863=CARTESIAN_POINT('Ctrl Pts',(31.3224756056766,0.763531646934118,30.4322916666666));
#64864=CARTESIAN_POINT('Ctrl Pts',(30.8816504037844,1.52706329386825,30.4739583333333));
#64865=CARTESIAN_POINT('Ctrl Pts',(30.,1.52706329386825,30.515625));
#64866=CARTESIAN_POINT('Ctrl Pts',(29.1183495962155,1.52706329386825,30.5572916666666));
#64867=CARTESIAN_POINT('Ctrl Pts',(28.6775243943233,0.76353164693412,30.5989583333333));
#64868=CARTESIAN_POINT('Ctrl Pts',(28.2366991924311,-1.31894491186926E-14,
30.640625));
#64869=CARTESIAN_POINT('Ctrl Pts',(28.6775243943233,-0.763531646934146,
30.6822916666666));
#64870=CARTESIAN_POINT('Ctrl Pts',(29.1183495962155,-1.52706329386828,30.7239583333333));
#64871=CARTESIAN_POINT('Ctrl Pts',(30.,-1.52706329386828,30.765625));
#64872=CARTESIAN_POINT('Ctrl Pts',(30.8816504037844,-1.52706329386828,30.8072916666666));
#64873=CARTESIAN_POINT('Ctrl Pts',(31.3224756056766,-0.763531646934147,
30.8489583333333));
#64874=CARTESIAN_POINT('Ctrl Pts',(31.7633008075689,-1.36198038370242E-14,
30.890625));
#64875=CARTESIAN_POINT('Ctrl Pts',(31.3224756056766,0.763531646934118,30.9322916666666));
#64876=CARTESIAN_POINT('Ctrl Pts',(30.8816504037844,1.52706329386825,30.9739583333333));
#64877=CARTESIAN_POINT('Ctrl Pts',(30.,1.52706329386825,31.015625));
#64878=CARTESIAN_POINT('Ctrl Pts',(29.1183495962155,1.52706329386825,31.0572916666666));
#64879=CARTESIAN_POINT('Ctrl Pts',(28.6775243943233,0.76353164693412,31.0989583333333));
#64880=CARTESIAN_POINT('Ctrl Pts',(28.2366991924311,-1.31894491186926E-14,
31.140625));
#64881=CARTESIAN_POINT('Ctrl Pts',(28.6775243943233,-0.763531646934146,
31.1822916666666));
#64882=CARTESIAN_POINT('Ctrl Pts',(29.1183495962155,-1.52706329386828,31.2239583333333));
#64883=CARTESIAN_POINT('Ctrl Pts',(30.,-1.52706329386828,31.265625));
#64884=CARTESIAN_POINT('Ctrl Pts',(30.8816504037844,-1.52706329386828,31.3072916666666));
#64885=CARTESIAN_POINT('Ctrl Pts',(31.3224756056766,-0.763531646934147,
31.3489583333333));
#64886=CARTESIAN_POINT('Ctrl Pts',(31.7633008075689,-1.36198038370242E-14,
31.390625));
#64887=CARTESIAN_POINT('Ctrl Pts',(31.3224756056766,0.763531646934118,31.4322916666666));
#64888=CARTESIAN_POINT('Ctrl Pts',(30.8816504037844,1.52706329386825,31.4739583333333));
#64889=CARTESIAN_POINT('Ctrl Pts',(30.,1.52706329386825,31.515625));
#64890=CARTESIAN_POINT('Ctrl Pts',(30.,1.17523507120987,15.8124968809397));
#64891=CARTESIAN_POINT('Ctrl Pts',(29.3214777152758,1.17523507120987,15.8541635476064));
#64892=CARTESIAN_POINT('Ctrl Pts',(28.9822165729138,0.587617535604928,15.895830214273));
#64893=CARTESIAN_POINT('Ctrl Pts',(28.6429554305518,-1.32141489532166E-14,
15.9374968809397));
#64894=CARTESIAN_POINT('Ctrl Pts',(28.9822165729138,-0.587617535604954,
15.9791635476064));
#64895=CARTESIAN_POINT('Ctrl Pts',(29.3214777152758,-1.17523507120989,16.020830214273));
#64896=CARTESIAN_POINT('Ctrl Pts',(30.,-1.17523507120989,16.0624968809397));
#64897=CARTESIAN_POINT('Ctrl Pts',(30.6785222847241,-1.17523507120989,16.1041635476064));
#64898=CARTESIAN_POINT('Ctrl Pts',(31.0177834270861,-0.587617535604955,
16.145830214273));
#64899=CARTESIAN_POINT('Ctrl Pts',(31.3570445694482,-1.35453519623354E-14,
16.1874968809397));
#64900=CARTESIAN_POINT('Ctrl Pts',(31.0177834270861,0.587617535604927,16.2291635476064));
#64901=CARTESIAN_POINT('Ctrl Pts',(30.6785222847241,1.17523507120987,16.270830214273));
#64902=CARTESIAN_POINT('Ctrl Pts',(30.,1.17523507120987,16.3124968809397));
#64903=CARTESIAN_POINT('Ctrl Pts',(29.3214777152758,1.17523507120987,16.3541635476064));
#64904=CARTESIAN_POINT('Ctrl Pts',(28.9822165729138,0.587617535604928,16.395830214273));
#64905=CARTESIAN_POINT('Ctrl Pts',(28.6429554305518,-1.32141489532166E-14,
16.4374968809397));
#64906=CARTESIAN_POINT('Ctrl Pts',(28.9822165729138,-0.587617535604954,
16.4791635476064));
#64907=CARTESIAN_POINT('Ctrl Pts',(29.3214777152758,-1.17523507120989,16.520830214273));
#64908=CARTESIAN_POINT('Ctrl Pts',(30.,-1.17523507120989,16.5624968809397));
#64909=CARTESIAN_POINT('Ctrl Pts',(30.6785222847241,-1.17523507120989,16.6041635476064));
#64910=CARTESIAN_POINT('Ctrl Pts',(31.0177834270861,-0.587617535604955,
16.645830214273));
#64911=CARTESIAN_POINT('Ctrl Pts',(31.3570445694482,-1.35453519623354E-14,
16.6874968809397));
#64912=CARTESIAN_POINT('Ctrl Pts',(31.0177834270861,0.587617535604927,16.7291635476064));
#64913=CARTESIAN_POINT('Ctrl Pts',(30.6785222847241,1.17523507120987,16.770830214273));
#64914=CARTESIAN_POINT('Ctrl Pts',(30.,1.17523507120987,16.8124968809397));
#64915=CARTESIAN_POINT('Ctrl Pts',(29.3214777152758,1.17523507120987,16.8541635476064));
#64916=CARTESIAN_POINT('Ctrl Pts',(28.9822165729138,0.587617535604928,16.895830214273));
#64917=CARTESIAN_POINT('Ctrl Pts',(28.6429554305518,-1.32141489532166E-14,
16.9374968809397));
#64918=CARTESIAN_POINT('Ctrl Pts',(28.9822165729138,-0.587617535604954,
16.9791635476064));
#64919=CARTESIAN_POINT('Ctrl Pts',(29.3214777152758,-1.17523507120989,17.020830214273));
#64920=CARTESIAN_POINT('Ctrl Pts',(30.,-1.17523507120989,17.0624968809397));
#64921=CARTESIAN_POINT('Ctrl Pts',(30.6785222847241,-1.17523507120989,17.1041635476064));
#64922=CARTESIAN_POINT('Ctrl Pts',(31.0177834270861,-0.587617535604955,
17.145830214273));
#64923=CARTESIAN_POINT('Ctrl Pts',(31.3570445694482,-1.35453519623354E-14,
17.1874968809397));
#64924=CARTESIAN_POINT('Ctrl Pts',(31.0177834270861,0.587617535604927,17.2291635476064));
#64925=CARTESIAN_POINT('Ctrl Pts',(30.6785222847241,1.17523507120987,17.270830214273));
#64926=CARTESIAN_POINT('Ctrl Pts',(30.,1.17523507120987,17.3124968809397));
#64927=CARTESIAN_POINT('Ctrl Pts',(29.3214777152758,1.17523507120987,17.3541635476064));
#64928=CARTESIAN_POINT('Ctrl Pts',(28.9822165729138,0.587617535604928,17.395830214273));
#64929=CARTESIAN_POINT('Ctrl Pts',(28.6429554305518,-1.32141489532166E-14,
17.4374968809397));
#64930=CARTESIAN_POINT('Ctrl Pts',(28.9822165729138,-0.587617535604954,
17.4791635476064));
#64931=CARTESIAN_POINT('Ctrl Pts',(29.3214777152758,-1.17523507120989,17.520830214273));
#64932=CARTESIAN_POINT('Ctrl Pts',(30.,-1.17523507120989,17.5624968809397));
#64933=CARTESIAN_POINT('Ctrl Pts',(30.6785222847241,-1.17523507120989,17.6041635476064));
#64934=CARTESIAN_POINT('Ctrl Pts',(31.0177834270861,-0.587617535604955,
17.645830214273));
#64935=CARTESIAN_POINT('Ctrl Pts',(31.3570445694482,-1.35453519623354E-14,
17.6874968809397));
#64936=CARTESIAN_POINT('Ctrl Pts',(31.0177834270861,0.587617535604927,17.7291635476064));
#64937=CARTESIAN_POINT('Ctrl Pts',(30.6785222847241,1.17523507120987,17.770830214273));
#64938=CARTESIAN_POINT('Ctrl Pts',(30.,1.17523507120987,17.8124968809397));
#64939=CARTESIAN_POINT('Ctrl Pts',(29.3214777152758,1.17523507120987,17.8541635476064));
#64940=CARTESIAN_POINT('Ctrl Pts',(28.9822165729138,0.587617535604928,17.895830214273));
#64941=CARTESIAN_POINT('Ctrl Pts',(28.6429554305518,-1.32141489532166E-14,
17.9374968809397));
#64942=CARTESIAN_POINT('Ctrl Pts',(28.9822165729138,-0.587617535604954,
17.9791635476064));
#64943=CARTESIAN_POINT('Ctrl Pts',(29.3214777152758,-1.17523507120989,18.020830214273));
#64944=CARTESIAN_POINT('Ctrl Pts',(30.,-1.17523507120989,18.0624968809397));
#64945=CARTESIAN_POINT('Ctrl Pts',(30.6785222847241,-1.17523507120989,18.1041635476064));
#64946=CARTESIAN_POINT('Ctrl Pts',(31.0177834270861,-0.587617535604955,
18.145830214273));
#64947=CARTESIAN_POINT('Ctrl Pts',(31.3570445694482,-1.35453519623354E-14,
18.1874968809397));
#64948=CARTESIAN_POINT('Ctrl Pts',(31.0177834270861,0.587617535604927,18.2291635476064));
#64949=CARTESIAN_POINT('Ctrl Pts',(30.6785222847241,1.17523507120987,18.270830214273));
#64950=CARTESIAN_POINT('Ctrl Pts',(30.,1.17523507120987,18.3124968809397));
#64951=CARTESIAN_POINT('Ctrl Pts',(29.3214777152758,1.17523507120987,18.3541635476064));
#64952=CARTESIAN_POINT('Ctrl Pts',(28.9822165729138,0.587617535604928,18.395830214273));
#64953=CARTESIAN_POINT('Ctrl Pts',(28.6429554305518,-1.32141489532166E-14,
18.4374968809397));
#64954=CARTESIAN_POINT('Ctrl Pts',(28.9822165729138,-0.587617535604954,
18.4791635476064));
#64955=CARTESIAN_POINT('Ctrl Pts',(29.3214777152758,-1.17523507120989,18.520830214273));
#64956=CARTESIAN_POINT('Ctrl Pts',(30.,-1.17523507120989,18.5624968809397));
#64957=CARTESIAN_POINT('Ctrl Pts',(30.6785222847241,-1.17523507120989,18.6041635476064));
#64958=CARTESIAN_POINT('Ctrl Pts',(31.0177834270861,-0.587617535604955,
18.645830214273));
#64959=CARTESIAN_POINT('Ctrl Pts',(31.3570445694482,-1.35453519623354E-14,
18.6874968809397));
#64960=CARTESIAN_POINT('Ctrl Pts',(31.0177834270861,0.587617535604927,18.7291635476064));
#64961=CARTESIAN_POINT('Ctrl Pts',(30.6785222847241,1.17523507120987,18.770830214273));
#64962=CARTESIAN_POINT('Ctrl Pts',(30.,1.17523507120987,18.8124968809397));
#64963=CARTESIAN_POINT('Ctrl Pts',(29.3214777152758,1.17523507120987,18.8541635476064));
#64964=CARTESIAN_POINT('Ctrl Pts',(28.9822165729138,0.587617535604928,18.895830214273));
#64965=CARTESIAN_POINT('Ctrl Pts',(28.6429554305518,-1.32141489532166E-14,
18.9374968809397));
#64966=CARTESIAN_POINT('Ctrl Pts',(28.9822165729138,-0.587617535604954,
18.9791635476064));
#64967=CARTESIAN_POINT('Ctrl Pts',(29.3214777152758,-1.17523507120989,19.020830214273));
#64968=CARTESIAN_POINT('Ctrl Pts',(30.,-1.17523507120989,19.0624968809397));
#64969=CARTESIAN_POINT('Ctrl Pts',(30.6785222847241,-1.17523507120989,19.1041635476064));
#64970=CARTESIAN_POINT('Ctrl Pts',(31.0177834270861,-0.587617535604955,
19.145830214273));
#64971=CARTESIAN_POINT('Ctrl Pts',(31.3570445694482,-1.35453519623354E-14,
19.1874968809397));
#64972=CARTESIAN_POINT('Ctrl Pts',(31.0177834270861,0.587617535604927,19.2291635476064));
#64973=CARTESIAN_POINT('Ctrl Pts',(30.6785222847241,1.17523507120987,19.270830214273));
#64974=CARTESIAN_POINT('Ctrl Pts',(30.,1.17523507120987,19.3124968809397));
#64975=CARTESIAN_POINT('Ctrl Pts',(29.3214777152758,1.17523507120987,19.3541635476064));
#64976=CARTESIAN_POINT('Ctrl Pts',(28.9822165729138,0.587617535604928,19.395830214273));
#64977=CARTESIAN_POINT('Ctrl Pts',(28.6429554305518,-1.32141489532166E-14,
19.4374968809397));
#64978=CARTESIAN_POINT('Ctrl Pts',(28.9822165729138,-0.587617535604954,
19.4791635476064));
#64979=CARTESIAN_POINT('Ctrl Pts',(29.3214777152758,-1.17523507120989,19.520830214273));
#64980=CARTESIAN_POINT('Ctrl Pts',(30.,-1.17523507120989,19.5624968809397));
#64981=CARTESIAN_POINT('Ctrl Pts',(30.6785222847241,-1.17523507120989,19.6041635476064));
#64982=CARTESIAN_POINT('Ctrl Pts',(31.0177834270861,-0.587617535604955,
19.645830214273));
#64983=CARTESIAN_POINT('Ctrl Pts',(31.3570445694482,-1.35453519623354E-14,
19.6874968809397));
#64984=CARTESIAN_POINT('Ctrl Pts',(31.0177834270861,0.587617535604927,19.7291635476064));
#64985=CARTESIAN_POINT('Ctrl Pts',(30.6785222847241,1.17523507120987,19.770830214273));
#64986=CARTESIAN_POINT('Ctrl Pts',(30.,1.17523507120987,19.8124968809397));
#64987=CARTESIAN_POINT('Ctrl Pts',(29.3214777152758,1.17523507120987,19.8541635476064));
#64988=CARTESIAN_POINT('Ctrl Pts',(28.9822165729138,0.587617535604928,19.895830214273));
#64989=CARTESIAN_POINT('Ctrl Pts',(28.6429554305518,-1.32141489532166E-14,
19.9374968809397));
#64990=CARTESIAN_POINT('Ctrl Pts',(28.9822165729138,-0.587617535604954,
19.9791635476064));
#64991=CARTESIAN_POINT('Ctrl Pts',(29.3214777152758,-1.17523507120989,20.020830214273));
#64992=CARTESIAN_POINT('Ctrl Pts',(30.,-1.17523507120989,20.0624968809397));
#64993=CARTESIAN_POINT('Ctrl Pts',(30.6785222847241,-1.17523507120989,20.1041635476064));
#64994=CARTESIAN_POINT('Ctrl Pts',(31.0177834270861,-0.587617535604955,
20.145830214273));
#64995=CARTESIAN_POINT('Ctrl Pts',(31.3570445694482,-1.35453519623354E-14,
20.1874968809397));
#64996=CARTESIAN_POINT('Ctrl Pts',(31.0177834270861,0.587617535604927,20.2291635476064));
#64997=CARTESIAN_POINT('Ctrl Pts',(30.6785222847241,1.17523507120987,20.270830214273));
#64998=CARTESIAN_POINT('Ctrl Pts',(30.,1.17523507120987,20.3124968809397));
#64999=CARTESIAN_POINT('Ctrl Pts',(29.3214777152758,1.17523507120987,20.3541635476064));
#65000=CARTESIAN_POINT('Ctrl Pts',(28.9822165729138,0.587617535604928,20.395830214273));
#65001=CARTESIAN_POINT('Ctrl Pts',(28.6429554305518,-1.32141489532166E-14,
20.4374968809397));
#65002=CARTESIAN_POINT('Ctrl Pts',(28.9822165729138,-0.587617535604954,
20.4791635476064));
#65003=CARTESIAN_POINT('Ctrl Pts',(29.3214777152758,-1.17523507120989,20.520830214273));
#65004=CARTESIAN_POINT('Ctrl Pts',(30.,-1.17523507120989,20.5624968809397));
#65005=CARTESIAN_POINT('Ctrl Pts',(30.6785222847241,-1.17523507120989,20.6041635476064));
#65006=CARTESIAN_POINT('Ctrl Pts',(31.0177834270861,-0.587617535604955,
20.645830214273));
#65007=CARTESIAN_POINT('Ctrl Pts',(31.3570445694482,-1.35453519623354E-14,
20.6874968809397));
#65008=CARTESIAN_POINT('Ctrl Pts',(31.0177834270861,0.587617535604927,20.7291635476064));
#65009=CARTESIAN_POINT('Ctrl Pts',(30.6785222847241,1.17523507120987,20.770830214273));
#65010=CARTESIAN_POINT('Ctrl Pts',(30.,1.17523507120987,20.8124968809397));
#65011=CARTESIAN_POINT('Ctrl Pts',(29.3214777152758,1.17523507120987,20.8541635476064));
#65012=CARTESIAN_POINT('Ctrl Pts',(28.9822165729138,0.587617535604928,20.895830214273));
#65013=CARTESIAN_POINT('Ctrl Pts',(28.6429554305518,-1.32141489532166E-14,
20.9374968809397));
#65014=CARTESIAN_POINT('Ctrl Pts',(28.9822165729138,-0.587617535604954,
20.9791635476064));
#65015=CARTESIAN_POINT('Ctrl Pts',(29.3214777152758,-1.17523507120989,21.020830214273));
#65016=CARTESIAN_POINT('Ctrl Pts',(30.,-1.17523507120989,21.0624968809397));
#65017=CARTESIAN_POINT('Ctrl Pts',(30.6785222847241,-1.17523507120989,21.1041635476064));
#65018=CARTESIAN_POINT('Ctrl Pts',(31.0177834270861,-0.587617535604955,
21.145830214273));
#65019=CARTESIAN_POINT('Ctrl Pts',(31.3570445694482,-1.35453519623354E-14,
21.1874968809397));
#65020=CARTESIAN_POINT('Ctrl Pts',(31.0177834270861,0.587617535604927,21.2291635476064));
#65021=CARTESIAN_POINT('Ctrl Pts',(30.6785222847241,1.17523507120987,21.270830214273));
#65022=CARTESIAN_POINT('Ctrl Pts',(30.,1.17523507120987,21.3124968809397));
#65023=CARTESIAN_POINT('Ctrl Pts',(29.3214777152758,1.17523507120987,21.3541635476064));
#65024=CARTESIAN_POINT('Ctrl Pts',(28.9822165729138,0.587617535604928,21.395830214273));
#65025=CARTESIAN_POINT('Ctrl Pts',(28.6429554305518,-1.32141489532166E-14,
21.4374968809397));
#65026=CARTESIAN_POINT('Ctrl Pts',(28.9822165729138,-0.587617535604954,
21.4791635476064));
#65027=CARTESIAN_POINT('Ctrl Pts',(29.3214777152758,-1.17523507120989,21.520830214273));
#65028=CARTESIAN_POINT('Ctrl Pts',(30.,-1.17523507120989,21.5624968809397));
#65029=CARTESIAN_POINT('Ctrl Pts',(30.6785222847241,-1.17523507120989,21.6041635476064));
#65030=CARTESIAN_POINT('Ctrl Pts',(31.0177834270861,-0.587617535604955,
21.645830214273));
#65031=CARTESIAN_POINT('Ctrl Pts',(31.3570445694482,-1.35453519623354E-14,
21.6874968809397));
#65032=CARTESIAN_POINT('Ctrl Pts',(31.0177834270861,0.587617535604927,21.7291635476064));
#65033=CARTESIAN_POINT('Ctrl Pts',(30.6785222847241,1.17523507120987,21.770830214273));
#65034=CARTESIAN_POINT('Ctrl Pts',(30.,1.17523507120987,21.8124968809397));
#65035=CARTESIAN_POINT('Ctrl Pts',(29.3214777152758,1.17523507120987,21.8541635476064));
#65036=CARTESIAN_POINT('Ctrl Pts',(28.9822165729138,0.587617535604928,21.895830214273));
#65037=CARTESIAN_POINT('Ctrl Pts',(28.6429554305518,-1.32141489532166E-14,
21.9374968809397));
#65038=CARTESIAN_POINT('Ctrl Pts',(28.9822165729138,-0.587617535604954,
21.9791635476064));
#65039=CARTESIAN_POINT('Ctrl Pts',(29.3214777152758,-1.17523507120989,22.020830214273));
#65040=CARTESIAN_POINT('Ctrl Pts',(30.,-1.17523507120989,22.0624968809397));
#65041=CARTESIAN_POINT('Ctrl Pts',(30.6785222847241,-1.17523507120989,22.1041635476064));
#65042=CARTESIAN_POINT('Ctrl Pts',(31.0177834270861,-0.587617535604955,
22.145830214273));
#65043=CARTESIAN_POINT('Ctrl Pts',(31.3570445694482,-1.35453519623354E-14,
22.1874968809397));
#65044=CARTESIAN_POINT('Ctrl Pts',(31.0177834270861,0.587617535604927,22.2291635476064));
#65045=CARTESIAN_POINT('Ctrl Pts',(30.6785222847241,1.17523507120987,22.270830214273));
#65046=CARTESIAN_POINT('Ctrl Pts',(30.,1.17523507120987,22.3124968809397));
#65047=CARTESIAN_POINT('Ctrl Pts',(29.3214777152758,1.17523507120987,22.3541635476064));
#65048=CARTESIAN_POINT('Ctrl Pts',(28.9822165729138,0.587617535604928,22.395830214273));
#65049=CARTESIAN_POINT('Ctrl Pts',(28.6429554305518,-1.32141489532166E-14,
22.4374968809397));
#65050=CARTESIAN_POINT('Ctrl Pts',(28.9822165729138,-0.587617535604954,
22.4791635476064));
#65051=CARTESIAN_POINT('Ctrl Pts',(29.3214777152758,-1.17523507120989,22.520830214273));
#65052=CARTESIAN_POINT('Ctrl Pts',(30.,-1.17523507120989,22.5624968809397));
#65053=CARTESIAN_POINT('Ctrl Pts',(30.6785222847241,-1.17523507120989,22.6041635476064));
#65054=CARTESIAN_POINT('Ctrl Pts',(31.0177834270861,-0.587617535604955,
22.645830214273));
#65055=CARTESIAN_POINT('Ctrl Pts',(31.3570445694482,-1.35453519623354E-14,
22.6874968809397));
#65056=CARTESIAN_POINT('Ctrl Pts',(31.0177834270861,0.587617535604927,22.7291635476064));
#65057=CARTESIAN_POINT('Ctrl Pts',(30.6785222847241,1.17523507120987,22.770830214273));
#65058=CARTESIAN_POINT('Ctrl Pts',(30.,1.17523507120987,22.8124968809397));
#65059=CARTESIAN_POINT('Ctrl Pts',(29.3214777152758,1.17523507120987,22.8541635476064));
#65060=CARTESIAN_POINT('Ctrl Pts',(28.9822165729138,0.587617535604928,22.895830214273));
#65061=CARTESIAN_POINT('Ctrl Pts',(28.6429554305518,-1.32141489532166E-14,
22.9374968809397));
#65062=CARTESIAN_POINT('Ctrl Pts',(28.9822165729138,-0.587617535604954,
22.9791635476064));
#65063=CARTESIAN_POINT('Ctrl Pts',(29.3214777152758,-1.17523507120989,23.020830214273));
#65064=CARTESIAN_POINT('Ctrl Pts',(30.,-1.17523507120989,23.0624968809397));
#65065=CARTESIAN_POINT('Ctrl Pts',(30.6785222847241,-1.17523507120989,23.1041635476064));
#65066=CARTESIAN_POINT('Ctrl Pts',(31.0177834270861,-0.587617535604955,
23.145830214273));
#65067=CARTESIAN_POINT('Ctrl Pts',(31.3570445694482,-1.35453519623354E-14,
23.1874968809397));
#65068=CARTESIAN_POINT('Ctrl Pts',(31.0177834270861,0.587617535604927,23.2291635476064));
#65069=CARTESIAN_POINT('Ctrl Pts',(30.6785222847241,1.17523507120987,23.270830214273));
#65070=CARTESIAN_POINT('Ctrl Pts',(30.,1.17523507120987,23.3124968809397));
#65071=CARTESIAN_POINT('Ctrl Pts',(29.3214777152758,1.17523507120987,23.3541635476064));
#65072=CARTESIAN_POINT('Ctrl Pts',(28.9822165729138,0.587617535604928,23.395830214273));
#65073=CARTESIAN_POINT('Ctrl Pts',(28.6429554305518,-1.32141489532166E-14,
23.4374968809397));
#65074=CARTESIAN_POINT('Ctrl Pts',(28.9822165729138,-0.587617535604954,
23.4791635476064));
#65075=CARTESIAN_POINT('Ctrl Pts',(29.3214777152758,-1.17523507120989,23.520830214273));
#65076=CARTESIAN_POINT('Ctrl Pts',(30.,-1.17523507120989,23.5624968809397));
#65077=CARTESIAN_POINT('Ctrl Pts',(30.6785222847241,-1.17523507120989,23.6041635476064));
#65078=CARTESIAN_POINT('Ctrl Pts',(31.0177834270861,-0.587617535604955,
23.645830214273));
#65079=CARTESIAN_POINT('Ctrl Pts',(31.3570445694482,-1.35453519623354E-14,
23.6874968809397));
#65080=CARTESIAN_POINT('Ctrl Pts',(31.0177834270861,0.587617535604927,23.7291635476064));
#65081=CARTESIAN_POINT('Ctrl Pts',(30.6785222847241,1.17523507120987,23.770830214273));
#65082=CARTESIAN_POINT('Ctrl Pts',(30.,1.17523507120987,23.8124968809397));
#65083=CARTESIAN_POINT('Ctrl Pts',(29.3214777152758,1.17523507120987,23.8541635476064));
#65084=CARTESIAN_POINT('Ctrl Pts',(28.9822165729138,0.587617535604928,23.895830214273));
#65085=CARTESIAN_POINT('Ctrl Pts',(28.6429554305518,-1.32141489532166E-14,
23.9374968809397));
#65086=CARTESIAN_POINT('Ctrl Pts',(28.9822165729138,-0.587617535604954,
23.9791635476064));
#65087=CARTESIAN_POINT('Ctrl Pts',(29.3214777152758,-1.17523507120989,24.020830214273));
#65088=CARTESIAN_POINT('Ctrl Pts',(30.,-1.17523507120989,24.0624968809397));
#65089=CARTESIAN_POINT('Ctrl Pts',(30.6785222847241,-1.17523507120989,24.1041635476064));
#65090=CARTESIAN_POINT('Ctrl Pts',(31.0177834270861,-0.587617535604955,
24.145830214273));
#65091=CARTESIAN_POINT('Ctrl Pts',(31.3570445694482,-1.35453519623354E-14,
24.1874968809397));
#65092=CARTESIAN_POINT('Ctrl Pts',(31.0177834270861,0.587617535604927,24.2291635476064));
#65093=CARTESIAN_POINT('Ctrl Pts',(30.6785222847241,1.17523507120987,24.270830214273));
#65094=CARTESIAN_POINT('Ctrl Pts',(30.,1.17523507120987,24.3124968809397));
#65095=CARTESIAN_POINT('Ctrl Pts',(29.3214777152758,1.17523507120987,24.3541635476064));
#65096=CARTESIAN_POINT('Ctrl Pts',(28.9822165729138,0.587617535604928,24.395830214273));
#65097=CARTESIAN_POINT('Ctrl Pts',(28.6429554305518,-1.32141489532166E-14,
24.4374968809397));
#65098=CARTESIAN_POINT('Ctrl Pts',(28.9822165729138,-0.587617535604954,
24.4791635476064));
#65099=CARTESIAN_POINT('Ctrl Pts',(29.3214777152758,-1.17523507120989,24.520830214273));
#65100=CARTESIAN_POINT('Ctrl Pts',(30.,-1.17523507120989,24.5624968809397));
#65101=CARTESIAN_POINT('Ctrl Pts',(30.6785222847241,-1.17523507120989,24.6041635476064));
#65102=CARTESIAN_POINT('Ctrl Pts',(31.0177834270861,-0.587617535604955,
24.645830214273));
#65103=CARTESIAN_POINT('Ctrl Pts',(31.3570445694482,-1.35453519623354E-14,
24.6874968809397));
#65104=CARTESIAN_POINT('Ctrl Pts',(31.0177834270861,0.587617535604927,24.7291635476064));
#65105=CARTESIAN_POINT('Ctrl Pts',(30.6785222847241,1.17523507120987,24.770830214273));
#65106=CARTESIAN_POINT('Ctrl Pts',(30.,1.17523507120987,24.8124968809397));
#65107=CARTESIAN_POINT('Ctrl Pts',(29.3214777152758,1.17523507120987,24.8541635476064));
#65108=CARTESIAN_POINT('Ctrl Pts',(28.9822165729138,0.587617535604928,24.895830214273));
#65109=CARTESIAN_POINT('Ctrl Pts',(28.6429554305518,-1.32141489532166E-14,
24.9374968809397));
#65110=CARTESIAN_POINT('Ctrl Pts',(28.9822165729138,-0.587617535604954,
24.9791635476064));
#65111=CARTESIAN_POINT('Ctrl Pts',(29.3214777152758,-1.17523507120989,25.020830214273));
#65112=CARTESIAN_POINT('Ctrl Pts',(30.,-1.17523507120989,25.0624968809397));
#65113=CARTESIAN_POINT('Ctrl Pts',(30.6785222847241,-1.17523507120989,25.1041635476064));
#65114=CARTESIAN_POINT('Ctrl Pts',(31.0177834270861,-0.587617535604955,
25.145830214273));
#65115=CARTESIAN_POINT('Ctrl Pts',(31.3570445694482,-1.35453519623354E-14,
25.1874968809397));
#65116=CARTESIAN_POINT('Ctrl Pts',(31.0177834270861,0.587617535604927,25.2291635476064));
#65117=CARTESIAN_POINT('Ctrl Pts',(30.6785222847241,1.17523507120987,25.270830214273));
#65118=CARTESIAN_POINT('Ctrl Pts',(30.,1.17523507120987,25.3124968809397));
#65119=CARTESIAN_POINT('Ctrl Pts',(29.3214777152758,1.17523507120987,25.3541635476064));
#65120=CARTESIAN_POINT('Ctrl Pts',(28.9822165729138,0.587617535604928,25.395830214273));
#65121=CARTESIAN_POINT('Ctrl Pts',(28.6429554305518,-1.32141489532166E-14,
25.4374968809397));
#65122=CARTESIAN_POINT('Ctrl Pts',(28.9822165729138,-0.587617535604954,
25.4791635476064));
#65123=CARTESIAN_POINT('Ctrl Pts',(29.3214777152758,-1.17523507120989,25.520830214273));
#65124=CARTESIAN_POINT('Ctrl Pts',(30.,-1.17523507120989,25.5624968809397));
#65125=CARTESIAN_POINT('Ctrl Pts',(30.6785222847241,-1.17523507120989,25.6041635476064));
#65126=CARTESIAN_POINT('Ctrl Pts',(31.0177834270861,-0.587617535604955,
25.645830214273));
#65127=CARTESIAN_POINT('Ctrl Pts',(31.3570445694482,-1.35453519623354E-14,
25.6874968809397));
#65128=CARTESIAN_POINT('Ctrl Pts',(31.0177834270861,0.587617535604927,25.7291635476064));
#65129=CARTESIAN_POINT('Ctrl Pts',(30.6785222847241,1.17523507120987,25.770830214273));
#65130=CARTESIAN_POINT('Ctrl Pts',(30.,1.17523507120987,25.8124968809397));
#65131=CARTESIAN_POINT('Ctrl Pts',(29.3214777152758,1.17523507120987,25.8541635476064));
#65132=CARTESIAN_POINT('Ctrl Pts',(28.9822165729138,0.587617535604928,25.895830214273));
#65133=CARTESIAN_POINT('Ctrl Pts',(28.6429554305518,-1.32141489532166E-14,
25.9374968809397));
#65134=CARTESIAN_POINT('Ctrl Pts',(28.9822165729138,-0.587617535604954,
25.9791635476064));
#65135=CARTESIAN_POINT('Ctrl Pts',(29.3214777152758,-1.17523507120989,26.020830214273));
#65136=CARTESIAN_POINT('Ctrl Pts',(30.,-1.17523507120989,26.0624968809397));
#65137=CARTESIAN_POINT('Ctrl Pts',(30.6785222847241,-1.17523507120989,26.1041635476064));
#65138=CARTESIAN_POINT('Ctrl Pts',(31.0177834270861,-0.587617535604955,
26.145830214273));
#65139=CARTESIAN_POINT('Ctrl Pts',(31.3570445694482,-1.35453519623354E-14,
26.1874968809397));
#65140=CARTESIAN_POINT('Ctrl Pts',(31.0177834270861,0.587617535604927,26.2291635476064));
#65141=CARTESIAN_POINT('Ctrl Pts',(30.6785222847241,1.17523507120987,26.270830214273));
#65142=CARTESIAN_POINT('Ctrl Pts',(30.,1.17523507120987,26.3124968809397));
#65143=CARTESIAN_POINT('Ctrl Pts',(29.3214777152758,1.17523507120987,26.3541635476064));
#65144=CARTESIAN_POINT('Ctrl Pts',(28.9822165729138,0.587617535604928,26.395830214273));
#65145=CARTESIAN_POINT('Ctrl Pts',(28.6429554305518,-1.32141489532166E-14,
26.4374968809397));
#65146=CARTESIAN_POINT('Ctrl Pts',(28.9822165729138,-0.587617535604954,
26.4791635476064));
#65147=CARTESIAN_POINT('Ctrl Pts',(29.3214777152758,-1.17523507120989,26.520830214273));
#65148=CARTESIAN_POINT('Ctrl Pts',(30.,-1.17523507120989,26.5624968809397));
#65149=CARTESIAN_POINT('Ctrl Pts',(30.6785222847241,-1.17523507120989,26.6041635476064));
#65150=CARTESIAN_POINT('Ctrl Pts',(31.0177834270861,-0.587617535604955,
26.645830214273));
#65151=CARTESIAN_POINT('Ctrl Pts',(31.3570445694482,-1.35453519623354E-14,
26.6874968809397));
#65152=CARTESIAN_POINT('Ctrl Pts',(31.0177834270861,0.587617535604927,26.7291635476064));
#65153=CARTESIAN_POINT('Ctrl Pts',(30.6785222847241,1.17523507120987,26.770830214273));
#65154=CARTESIAN_POINT('Ctrl Pts',(30.,1.17523507120987,26.8124968809397));
#65155=CARTESIAN_POINT('Ctrl Pts',(29.3214777152758,1.17523507120987,26.8541635476064));
#65156=CARTESIAN_POINT('Ctrl Pts',(28.9822165729138,0.587617535604928,26.895830214273));
#65157=CARTESIAN_POINT('Ctrl Pts',(28.6429554305518,-1.32141489532166E-14,
26.9374968809397));
#65158=CARTESIAN_POINT('Ctrl Pts',(28.9822165729138,-0.587617535604954,
26.9791635476064));
#65159=CARTESIAN_POINT('Ctrl Pts',(29.3214777152758,-1.17523507120989,27.020830214273));
#65160=CARTESIAN_POINT('Ctrl Pts',(30.,-1.17523507120989,27.0624968809397));
#65161=CARTESIAN_POINT('Ctrl Pts',(30.6785222847241,-1.17523507120989,27.1041635476064));
#65162=CARTESIAN_POINT('Ctrl Pts',(31.0177834270861,-0.587617535604955,
27.145830214273));
#65163=CARTESIAN_POINT('Ctrl Pts',(31.3570445694482,-1.35453519623354E-14,
27.1874968809397));
#65164=CARTESIAN_POINT('Ctrl Pts',(31.0177834270861,0.587617535604927,27.2291635476064));
#65165=CARTESIAN_POINT('Ctrl Pts',(30.6785222847241,1.17523507120987,27.270830214273));
#65166=CARTESIAN_POINT('Ctrl Pts',(30.,1.17523507120987,27.3124968809397));
#65167=CARTESIAN_POINT('Ctrl Pts',(29.3214777152758,1.17523507120987,27.3541635476064));
#65168=CARTESIAN_POINT('Ctrl Pts',(28.9822165729138,0.587617535604928,27.395830214273));
#65169=CARTESIAN_POINT('Ctrl Pts',(28.6429554305518,-1.32141489532166E-14,
27.4374968809397));
#65170=CARTESIAN_POINT('Ctrl Pts',(28.9822165729138,-0.587617535604954,
27.4791635476064));
#65171=CARTESIAN_POINT('Ctrl Pts',(29.3214777152758,-1.17523507120989,27.520830214273));
#65172=CARTESIAN_POINT('Ctrl Pts',(30.,-1.17523507120989,27.5624968809397));
#65173=CARTESIAN_POINT('Ctrl Pts',(30.6785222847241,-1.17523507120989,27.6041635476064));
#65174=CARTESIAN_POINT('Ctrl Pts',(31.0177834270861,-0.587617535604955,
27.645830214273));
#65175=CARTESIAN_POINT('Ctrl Pts',(31.3570445694482,-1.35453519623354E-14,
27.6874968809397));
#65176=CARTESIAN_POINT('Ctrl Pts',(31.0177834270861,0.587617535604927,27.7291635476064));
#65177=CARTESIAN_POINT('Ctrl Pts',(30.6785222847241,1.17523507120987,27.770830214273));
#65178=CARTESIAN_POINT('Ctrl Pts',(30.,1.17523507120987,27.8124968809397));
#65179=CARTESIAN_POINT('Ctrl Pts',(29.3214777152758,1.17523507120987,27.8541635476064));
#65180=CARTESIAN_POINT('Ctrl Pts',(28.9822165729138,0.587617535604928,27.895830214273));
#65181=CARTESIAN_POINT('Ctrl Pts',(28.6429554305518,-1.32141489532166E-14,
27.9374968809397));
#65182=CARTESIAN_POINT('Ctrl Pts',(28.9822165729138,-0.587617535604954,
27.9791635476064));
#65183=CARTESIAN_POINT('Ctrl Pts',(29.3214777152758,-1.17523507120989,28.020830214273));
#65184=CARTESIAN_POINT('Ctrl Pts',(30.,-1.17523507120989,28.0624968809397));
#65185=CARTESIAN_POINT('Ctrl Pts',(30.6785222847241,-1.17523507120989,28.1041635476064));
#65186=CARTESIAN_POINT('Ctrl Pts',(31.0177834270861,-0.587617535604955,
28.145830214273));
#65187=CARTESIAN_POINT('Ctrl Pts',(31.3570445694482,-1.35453519623354E-14,
28.1874968809397));
#65188=CARTESIAN_POINT('Ctrl Pts',(31.0177834270861,0.587617535604927,28.2291635476064));
#65189=CARTESIAN_POINT('Ctrl Pts',(30.6785222847241,1.17523507120987,28.270830214273));
#65190=CARTESIAN_POINT('Ctrl Pts',(30.,1.17523507120987,28.3124968809397));
#65191=CARTESIAN_POINT('Ctrl Pts',(29.3214777152758,1.17523507120987,28.3541635476064));
#65192=CARTESIAN_POINT('Ctrl Pts',(28.9822165729138,0.587617535604928,28.395830214273));
#65193=CARTESIAN_POINT('Ctrl Pts',(28.6429554305518,-1.32141489532166E-14,
28.4374968809397));
#65194=CARTESIAN_POINT('Ctrl Pts',(28.9822165729138,-0.587617535604954,
28.4791635476064));
#65195=CARTESIAN_POINT('Ctrl Pts',(29.3214777152758,-1.17523507120989,28.520830214273));
#65196=CARTESIAN_POINT('Ctrl Pts',(30.,-1.17523507120989,28.5624968809397));
#65197=CARTESIAN_POINT('Ctrl Pts',(30.6785222847241,-1.17523507120989,28.6041635476064));
#65198=CARTESIAN_POINT('Ctrl Pts',(31.0177834270861,-0.587617535604955,
28.645830214273));
#65199=CARTESIAN_POINT('Ctrl Pts',(31.3570445694482,-1.35453519623354E-14,
28.6874968809397));
#65200=CARTESIAN_POINT('Ctrl Pts',(31.0177834270861,0.587617535604927,28.7291635476064));
#65201=CARTESIAN_POINT('Ctrl Pts',(30.6785222847241,1.17523507120987,28.770830214273));
#65202=CARTESIAN_POINT('Ctrl Pts',(30.,1.17523507120987,28.8124968809397));
#65203=CARTESIAN_POINT('Ctrl Pts',(29.3214777152758,1.17523507120987,28.8541635476064));
#65204=CARTESIAN_POINT('Ctrl Pts',(28.9822165729138,0.587617535604928,28.895830214273));
#65205=CARTESIAN_POINT('Ctrl Pts',(28.6429554305518,-1.32141489532166E-14,
28.9374968809397));
#65206=CARTESIAN_POINT('Ctrl Pts',(28.9822165729138,-0.587617535604954,
28.9791635476064));
#65207=CARTESIAN_POINT('Ctrl Pts',(29.3214777152758,-1.17523507120989,29.020830214273));
#65208=CARTESIAN_POINT('Ctrl Pts',(30.,-1.17523507120989,29.0624968809397));
#65209=CARTESIAN_POINT('Ctrl Pts',(30.6785222847241,-1.17523507120989,29.1041635476064));
#65210=CARTESIAN_POINT('Ctrl Pts',(31.0177834270861,-0.587617535604955,
29.145830214273));
#65211=CARTESIAN_POINT('Ctrl Pts',(31.3570445694482,-1.35453519623354E-14,
29.1874968809397));
#65212=CARTESIAN_POINT('Ctrl Pts',(31.0177834270861,0.587617535604927,29.2291635476064));
#65213=CARTESIAN_POINT('Ctrl Pts',(30.6785222847241,1.17523507120987,29.270830214273));
#65214=CARTESIAN_POINT('Ctrl Pts',(30.,1.17523507120987,29.3124968809397));
#65215=CARTESIAN_POINT('Ctrl Pts',(29.3214777152758,1.17523507120987,29.3541635476064));
#65216=CARTESIAN_POINT('Ctrl Pts',(28.9822165729138,0.587617535604928,29.395830214273));
#65217=CARTESIAN_POINT('Ctrl Pts',(28.6429554305518,-1.32141489532166E-14,
29.4374968809397));
#65218=CARTESIAN_POINT('Ctrl Pts',(28.9822165729138,-0.587617535604954,
29.4791635476064));
#65219=CARTESIAN_POINT('Ctrl Pts',(29.3214777152758,-1.17523507120989,29.520830214273));
#65220=CARTESIAN_POINT('Ctrl Pts',(30.,-1.17523507120989,29.5624968809397));
#65221=CARTESIAN_POINT('Ctrl Pts',(30.6785222847241,-1.17523507120989,29.6041635476064));
#65222=CARTESIAN_POINT('Ctrl Pts',(31.0177834270861,-0.587617535604955,
29.645830214273));
#65223=CARTESIAN_POINT('Ctrl Pts',(31.3570445694482,-1.35453519623354E-14,
29.6874968809397));
#65224=CARTESIAN_POINT('Ctrl Pts',(31.0177834270861,0.587617535604927,29.7291635476064));
#65225=CARTESIAN_POINT('Ctrl Pts',(30.6785222847241,1.17523507120987,29.770830214273));
#65226=CARTESIAN_POINT('Ctrl Pts',(30.,1.17523507120987,29.8124968809397));
#65227=CARTESIAN_POINT('Ctrl Pts',(29.3214777152758,1.17523507120987,29.8541635476064));
#65228=CARTESIAN_POINT('Ctrl Pts',(28.9822165729138,0.587617535604928,29.895830214273));
#65229=CARTESIAN_POINT('Ctrl Pts',(28.6429554305518,-1.32141489532166E-14,
29.9374968809397));
#65230=CARTESIAN_POINT('Ctrl Pts',(28.9822165729138,-0.587617535604954,
29.9791635476064));
#65231=CARTESIAN_POINT('Ctrl Pts',(29.3214777152758,-1.17523507120989,30.020830214273));
#65232=CARTESIAN_POINT('Ctrl Pts',(30.,-1.17523507120989,30.0624968809397));
#65233=CARTESIAN_POINT('Ctrl Pts',(30.6785222847241,-1.17523507120989,30.1041635476064));
#65234=CARTESIAN_POINT('Ctrl Pts',(31.0177834270861,-0.587617535604955,
30.145830214273));
#65235=CARTESIAN_POINT('Ctrl Pts',(31.3570445694482,-1.35453519623354E-14,
30.1874968809397));
#65236=CARTESIAN_POINT('Ctrl Pts',(31.0177834270861,0.587617535604927,30.2291635476064));
#65237=CARTESIAN_POINT('Ctrl Pts',(30.6785222847241,1.17523507120987,30.270830214273));
#65238=CARTESIAN_POINT('Ctrl Pts',(30.,1.17523507120987,30.3124968809397));
#65239=CARTESIAN_POINT('Ctrl Pts',(29.3214777152758,1.17523507120987,30.3541635476064));
#65240=CARTESIAN_POINT('Ctrl Pts',(28.9822165729138,0.587617535604928,30.395830214273));
#65241=CARTESIAN_POINT('Ctrl Pts',(28.6429554305518,-1.32141489532166E-14,
30.4374968809397));
#65242=CARTESIAN_POINT('Ctrl Pts',(28.9822165729138,-0.587617535604954,
30.4791635476064));
#65243=CARTESIAN_POINT('Ctrl Pts',(29.3214777152758,-1.17523507120989,30.520830214273));
#65244=CARTESIAN_POINT('Ctrl Pts',(30.,-1.17523507120989,30.5624968809397));
#65245=CARTESIAN_POINT('Ctrl Pts',(30.6785222847241,-1.17523507120989,30.6041635476064));
#65246=CARTESIAN_POINT('Ctrl Pts',(31.0177834270861,-0.587617535604955,
30.645830214273));
#65247=CARTESIAN_POINT('Ctrl Pts',(31.3570445694482,-1.35453519623354E-14,
30.6874968809397));
#65248=CARTESIAN_POINT('Ctrl Pts',(31.0177834270861,0.587617535604927,30.7291635476064));
#65249=CARTESIAN_POINT('Ctrl Pts',(30.6785222847241,1.17523507120987,30.770830214273));
#65250=CARTESIAN_POINT('Ctrl Pts',(30.,1.17523507120987,30.8124968809397));
#65251=CARTESIAN_POINT('Ctrl Pts',(29.3214777152758,1.17523507120987,30.8541635476064));
#65252=CARTESIAN_POINT('Ctrl Pts',(28.9822165729138,0.587617535604928,30.895830214273));
#65253=CARTESIAN_POINT('Ctrl Pts',(28.6429554305518,-1.32141489532166E-14,
30.9374968809397));
#65254=CARTESIAN_POINT('Ctrl Pts',(28.9822165729138,-0.587617535604954,
30.9791635476064));
#65255=CARTESIAN_POINT('Ctrl Pts',(29.3214777152758,-1.17523507120989,31.020830214273));
#65256=CARTESIAN_POINT('Ctrl Pts',(30.,-1.17523507120989,31.0624968809397));
#65257=CARTESIAN_POINT('Ctrl Pts',(30.6785222847241,-1.17523507120989,31.1041635476064));
#65258=CARTESIAN_POINT('Ctrl Pts',(31.0177834270861,-0.587617535604955,
31.145830214273));
#65259=CARTESIAN_POINT('Ctrl Pts',(31.3570445694482,-1.35453519623354E-14,
31.1874968809397));
#65260=CARTESIAN_POINT('Ctrl Pts',(31.0177834270861,0.587617535604927,31.2291635476064));
#65261=CARTESIAN_POINT('Ctrl Pts',(30.6785222847241,1.17523507120987,31.270830214273));
#65262=CARTESIAN_POINT('Ctrl Pts',(30.,1.17523507120987,31.3124968809397));
#65263=CARTESIAN_POINT('',(30.,-1.50000000000002,30.75));
#65264=CARTESIAN_POINT('Origin',(30.,-1.24258096838242E-13,1029.88397459622));
#65265=CARTESIAN_POINT('Origin',(30.06875,2.82851012598683,15.7235432561772));
#65266=CARTESIAN_POINT('',(30.012548982272,2.70302030326666,15.7235432561772));
#65267=CARTESIAN_POINT('Origin',(30.,2.70864040503946,15.7235432561772));
#65268=CARTESIAN_POINT('',(29.987451017728,2.70302030326666,15.7235432561772));
#65269=CARTESIAN_POINT('Origin',(29.987451017728,2.70302030326666,15.7235432561772));
#65270=CARTESIAN_POINT('Origin',(30.2904604134361,2.81439671040465,15.7235432561772));
#65271=CARTESIAN_POINT('',(30.224586826676,2.69370321195774,15.7235432561772));
#65272=CARTESIAN_POINT('Origin',(30.2125174768313,2.70029057063376,15.7235432561772));
#65273=CARTESIAN_POINT('',(30.1995662307806,2.69567237556048,15.7235432561772));
#65274=CARTESIAN_POINT('Origin',(30.1995662307806,2.69567237556048,15.7235432561772));
#65275=CARTESIAN_POINT('Origin',(29.8466157199522,2.82518483606723,15.7235432561772));
#65276=CARTESIAN_POINT('',(29.8004337692194,2.69567237556048,15.7235432561772));
#65277=CARTESIAN_POINT('Origin',(29.7874825231687,2.70029057063376,15.7235432561772));
#65278=CARTESIAN_POINT('',(29.775413173324,2.69370321195775,15.7235432561772));
#65279=CARTESIAN_POINT('Origin',(29.775413173324,2.69370321195775,15.7235432561772));
#65280=CARTESIAN_POINT('Origin',(29.6254271049963,2.804441342164,15.7235432561772));
#65281=CARTESIAN_POINT('',(29.589548948342,2.67170473125694,15.7235432561772));
#65282=CARTESIAN_POINT('Origin',(29.5762752872513,2.67529254692237,15.7235432561772));
#65283=CARTESIAN_POINT('',(29.5647599813892,2.6677785445999,15.7235432561772));
#65284=CARTESIAN_POINT('Origin',(29.5647599813892,2.6677785445999,15.7235432561772));
#65285=CARTESIAN_POINT('Origin',(29.4065478564962,2.76640753481494,15.7235432561772));
#65286=CARTESIAN_POINT('',(29.3811946946869,2.63126513885323,15.7235432561772));
#65287=CARTESIAN_POINT('Origin',(29.3676804550908,2.63380045503416,15.7235432561772));
#65288=CARTESIAN_POINT('',(29.3567901889011,2.6254061353882,15.7235432561772));
#65289=CARTESIAN_POINT('Origin',(29.3567901889011,2.6254061353882,15.7235432561772));
#65290=CARTESIAN_POINT('Origin',(29.1913274378037,2.71131790508989,15.7235432561772));
#65291=CARTESIAN_POINT('',(29.1766555815128,2.57460292188403,15.7235432561772));
#65292=CARTESIAN_POINT('Origin',(29.1629840831922,2.57607010751313,15.7235432561772));
#65293=CARTESIAN_POINT('',(29.1527859987874,2.56684722431571,15.7235432561772));
#65294=CARTESIAN_POINT('Origin',(29.1527859987874,2.56684722431571,15.7235432561772));
#65295=CARTESIAN_POINT('Origin',(28.9810927543681,2.63951209887526,15.7235432561772));
#65296=CARTESIAN_POINT('',(28.9771926604684,2.50206742175908,15.7235432561772));
#65297=CARTESIAN_POINT('Origin',(28.9634481927567,2.50245743114905,15.7235432561772));
#65298=CARTESIAN_POINT('',(28.9540051647184,2.49246284654199,15.7235432561772));
#65299=CARTESIAN_POINT('Origin',(28.9540051647184,2.49246284654199,15.7235432561772));
#65300=CARTESIAN_POINT('Origin',(28.7771399729228,2.55143282284423,15.7235432561772));
#65301=CARTESIAN_POINT('Origin',(28.7616732366375,2.40271160649133,15.7235432561772));
#65302=CARTESIAN_POINT('Origin',(28.5807265301867,2.44762311502286,15.7235432561772));
#65303=CARTESIAN_POINT('Origin',(28.5769760048382,2.29814685040398,15.7235432561772));
#65304=CARTESIAN_POINT('Origin',(28.3930633803483,2.32872299678009,15.7235432561772));
#65305=CARTESIAN_POINT('Origin',(28.4010521891726,2.1794132547725,15.7235432561772));
#65306=CARTESIAN_POINT('Origin',(28.2153075291307,2.1954655268832,15.7235432561772));
#65307=CARTESIAN_POINT('Origin',(28.2349864184648,2.0472428516969,15.7235432561772));
#65308=CARTESIAN_POINT('Origin',(28.0485549004665,2.0486722819467,15.7235432561772));
#65309=CARTESIAN_POINT('Origin',(28.0798025434137,1.90245051566326,15.7235432561772));
#65310=CARTESIAN_POINT('Origin',(27.8938335797622,1.88924829113933,15.7235432561772));
#65311=CARTESIAN_POINT('Origin',(27.9364573242129,1.74592893957157,15.7235432561772));
#65312=CARTESIAN_POINT('Origin',(27.7520974754101,1.71817645637828,15.7235432561772));
#65313=CARTESIAN_POINT('Origin',(27.805834531806,1.57864313098712,15.7235432561772));
#65314=CARTESIAN_POINT('Origin',(27.6242204376256,1.53651149241201,15.7235432561772));
#65315=CARTESIAN_POINT('Origin',(27.6887394991445,1.40162446254803,15.7235432561772));
#65316=CARTESIAN_POINT('Origin',(27.5109908708699,1.3453734241531,15.7235432561772));
#65317=CARTESIAN_POINT('Origin',(27.5858941560429,1.2159643132099,15.7235432561772));
#65318=CARTESIAN_POINT('Origin',(30.5103800418355,2.78293160322096,15.7235432561772));
#65319=CARTESIAN_POINT('',(30.4352400186108,2.66777854459989,15.7235432561772));
#65320=CARTESIAN_POINT('Origin',(30.4237247127487,2.67529254692237,15.7235432561772));
#65321=CARTESIAN_POINT('',(30.410451051658,2.67170473125694,15.7235432561772));
#65322=CARTESIAN_POINT('Origin',(30.410451051658,2.67170473125694,15.7235432561772));
#65323=CARTESIAN_POINT('Origin',(30.7271530075584,2.73430879728474,15.7235432561772));
#65324=CARTESIAN_POINT('',(30.6432098110989,2.62540613538819,15.7235432561772));
#65325=CARTESIAN_POINT('Origin',(30.6323195449092,2.63380045503415,15.7235432561772));
#65326=CARTESIAN_POINT('',(30.6188053053131,2.63126513885322,15.7235432561772));
#65327=CARTESIAN_POINT('Origin',(30.6188053053131,2.63126513885322,15.7235432561772));
#65328=CARTESIAN_POINT('Origin',(30.9394428331868,2.66882806836332,15.7235432561772));
#65329=CARTESIAN_POINT('',(30.8472140012126,2.5668472243157,15.7235432561772));
#65330=CARTESIAN_POINT('Origin',(30.8370159168078,2.57607010751312,15.7235432561772));
#65331=CARTESIAN_POINT('',(30.8233444184872,2.57460292188402,15.7235432561772));
#65332=CARTESIAN_POINT('Origin',(30.8233444184872,2.57460292188402,15.7235432561772));
#65333=CARTESIAN_POINT('Origin',(31.1459406813522,2.58689312692505,15.7235432561772));
#65334=CARTESIAN_POINT('',(31.0459948352816,2.49246284654197,15.7235432561772));
#65335=CARTESIAN_POINT('Origin',(31.0365518072432,2.50245743114904,15.7235432561772));
#65336=CARTESIAN_POINT('',(31.0228073395316,2.50206742175906,15.7235432561772));
#65337=CARTESIAN_POINT('Origin',(31.0228073395316,2.50206742175906,15.7235432561772));
#65338=CARTESIAN_POINT('Origin',(31.3453734241531,2.48900912913003,15.7235432561772));
#65339=CARTESIAN_POINT('',(31.2383267633625,2.40271160649132,15.7235432561772));
#65340=CARTESIAN_POINT('Origin',(31.2296970110986,2.41341627257038,15.7235432561772));
#65341=CARTESIAN_POINT('',(31.2159643132099,2.41410584395711,15.7235432561772));
#65342=CARTESIAN_POINT('Origin',(31.2159643132099,2.41410584395711,15.7235432561772));
#65343=CARTESIAN_POINT('Origin',(31.536511492412,2.3757795623744,15.7235432561772));
#65344=CARTESIAN_POINT('',(31.4230239951618,2.29814685040396,15.7235432561772));
#65345=CARTESIAN_POINT('Origin',(31.4152607239647,2.30949560012898,15.7235432561772));
#65346=CARTESIAN_POINT('',(31.401624462548,2.3112605008555,15.7235432561772));
#65347=CARTESIAN_POINT('Origin',(31.401624462548,2.3112605008555,15.7235432561772));
#65348=CARTESIAN_POINT('Origin',(31.7181764563782,2.24790252458986,15.7235432561772));
#65349=CARTESIAN_POINT('',(31.5989478108274,2.17941325477248,15.7235432561772));
#65350=CARTESIAN_POINT('Origin',(31.5920988838457,2.19133611932756,15.7235432561772));
#65351=CARTESIAN_POINT('',(31.5786431309871,2.19416546819402,15.7235432561772));
#65352=CARTESIAN_POINT('Origin',(31.5786431309871,2.19416546819402,15.7235432561772));
#65353=CARTESIAN_POINT('Origin',(31.8892482911393,2.10616642023777,15.7235432561772));
#65354=CARTESIAN_POINT('',(31.7650135815352,2.04724285169688,15.7235432561772));
#65355=CARTESIAN_POINT('Origin',(31.7591212246811,2.05966632265728,15.7235432561772));
#65356=CARTESIAN_POINT('',(31.7459289395715,2.06354267578706,15.7235432561772));
#65357=CARTESIAN_POINT('Origin',(31.7459289395715,2.06354267578706,15.7235432561772));
#65358=CARTESIAN_POINT('Origin',(32.0486722819467,1.95144509953352,15.7235432561772));
#65359=CARTESIAN_POINT('',(31.9201974565863,1.90245051566323,15.7235432561772));
#65360=CARTESIAN_POINT('Origin',(31.9152979981993,1.91529799819927,15.7235432561772));
#65361=CARTESIAN_POINT('',(31.9024505156632,1.9201974565863,15.7235432561772));
#65362=CARTESIAN_POINT('Origin',(31.9024505156632,1.9201974565863,15.7235432561772));
#65363=CARTESIAN_POINT('Origin',(32.1954655268832,1.7846924708693,15.7235432561772));
#65364=CARTESIAN_POINT('',(32.0635426757871,1.74592893957153,15.7235432561772));
#65365=CARTESIAN_POINT('Origin',(32.0596663226573,1.75912122468115,15.7235432561772));
#65366=CARTESIAN_POINT('',(32.0472428516969,1.76501358153524,15.7235432561772));
#65367=CARTESIAN_POINT('Origin',(32.0472428516969,1.76501358153524,15.7235432561772));
#65368=CARTESIAN_POINT('Origin',(32.3287229967801,1.6069366196517,15.7235432561772));
#65369=CARTESIAN_POINT('',(32.194165468194,1.57864313098709,15.7235432561772));
#65370=CARTESIAN_POINT('Origin',(32.1913361193276,1.59209888384569,15.7235432561772));
#65371=CARTESIAN_POINT('',(32.1794132547725,1.59894781082743,15.7235432561772));
#65372=CARTESIAN_POINT('Origin',(32.1794132547725,1.59894781082743,15.7235432561772));
#65373=CARTESIAN_POINT('Origin',(32.4476231150228,1.41927346981329,15.7235432561772));
#65374=CARTESIAN_POINT('',(32.3112605008555,1.401624462548,15.7235432561772));
#65375=CARTESIAN_POINT('Origin',(32.309495600129,1.41526072396473,15.7235432561772));
#65376=CARTESIAN_POINT('',(32.298146850404,1.42302399516178,15.7235432561772));
#65377=CARTESIAN_POINT('Origin',(32.298146850404,1.42302399516178,15.7235432561772));
#65378=CARTESIAN_POINT('Origin',(32.5514328228442,1.22286002707717,15.7235432561772));
#65379=CARTESIAN_POINT('',(32.4141058439571,1.21596431320987,15.7235432561772));
#65380=CARTESIAN_POINT('Origin',(32.4134162725704,1.22969701109858,15.7235432561772));
#65381=CARTESIAN_POINT('',(32.4027116064913,1.23832676336245,15.7235432561772));
#65382=CARTESIAN_POINT('Origin',(32.4027116064913,1.23832676336245,15.7235432561772));
#65383=CARTESIAN_POINT('Origin',(32.6395120988752,1.01890724563189,15.7235432561772));
#65384=CARTESIAN_POINT('',(32.5020674217591,1.02280733953163,15.7235432561772));
#65385=CARTESIAN_POINT('Origin',(32.502457431149,1.03655180724325,15.7235432561772));
#65386=CARTESIAN_POINT('',(32.492462846542,1.04599483528156,15.7235432561772));
#65387=CARTESIAN_POINT('Origin',(32.492462846542,1.04599483528156,15.7235432561772));
#65388=CARTESIAN_POINT('Origin',(32.7113179050899,0.808672562196245,15.7235432561772));
#65389=CARTESIAN_POINT('',(32.574602921884,0.823344418487232,15.7235432561772));
#65390=CARTESIAN_POINT('Origin',(32.5760701075131,0.837015916807817,15.7235432561772));
#65391=CARTESIAN_POINT('',(32.5668472243157,0.84721400121258,15.7235432561772));
#65392=CARTESIAN_POINT('Origin',(32.5668472243157,0.84721400121258,15.7235432561772));
#65393=CARTESIAN_POINT('Origin',(32.7664075348149,0.593452143503749,15.7235432561772));
#65394=CARTESIAN_POINT('',(32.6312651388532,0.618805305313054,15.7235432561772));
#65395=CARTESIAN_POINT('Origin',(32.6338004550341,0.632319544909225,15.7235432561772));
#65396=CARTESIAN_POINT('',(32.6254061353882,0.64320981109888,15.7235432561772));
#65397=CARTESIAN_POINT('Origin',(32.6254061353882,0.64320981109888,15.7235432561772));
#65398=CARTESIAN_POINT('Origin',(32.804441342164,0.37457289500369,15.7235432561772));
#65399=CARTESIAN_POINT('',(32.6717047312569,0.410451051657977,15.7235432561772));
#65400=CARTESIAN_POINT('Origin',(32.6752925469224,0.423724712748682,15.7235432561772));
#65401=CARTESIAN_POINT('',(32.6677785445999,0.435240018610789,15.7235432561772));
#65402=CARTESIAN_POINT('Origin',(32.6677785445999,0.435240018610789,15.7235432561772));
#65403=CARTESIAN_POINT('Origin',(32.8251848360672,0.153384280047806,15.7235432561772));
#65404=CARTESIAN_POINT('',(32.6956723755605,0.199566230780603,15.7235432561772));
#65405=CARTESIAN_POINT('Origin',(32.7002905706337,0.212517476831278,15.7235432561772));
#65406=CARTESIAN_POINT('',(32.6937032119577,0.224586826675969,15.7235432561772));
#65407=CARTESIAN_POINT('Origin',(32.6937032119577,0.224586826675969,15.7235432561772));
#65408=CARTESIAN_POINT('Origin',(32.8285101259868,-0.0687500000000229,15.7235432561772));
#65409=CARTESIAN_POINT('',(32.7030203032667,-0.0125489822720396,15.7235432561772));
#65410=CARTESIAN_POINT('Origin',(32.7086404050395,-2.31188656783185E-14,
15.7235432561772));
#65411=CARTESIAN_POINT('',(32.7030203032667,0.0125489822719939,15.7235432561772));
#65412=CARTESIAN_POINT('Origin',(32.7030203032667,0.0125489822719939,15.7235432561772));
#65413=CARTESIAN_POINT('Origin',(32.8143967104046,-0.290460413436156,15.7235432561772));
#65414=CARTESIAN_POINT('',(32.6937032119577,-0.224586826676015,15.7235432561772));
#65415=CARTESIAN_POINT('Origin',(32.7002905706337,-0.212517476831324,15.7235432561772));
#65416=CARTESIAN_POINT('',(32.6956723755605,-0.199566230780649,15.7235432561772));
#65417=CARTESIAN_POINT('Origin',(32.6956723755605,-0.199566230780649,15.7235432561772));
#65418=CARTESIAN_POINT('Origin',(32.7829316032209,-0.510380041835567,15.7235432561772));
#65419=CARTESIAN_POINT('',(32.6677785445999,-0.435240018610835,15.7235432561772));
#65420=CARTESIAN_POINT('Origin',(32.6752925469224,-0.423724712748728,15.7235432561772));
#65421=CARTESIAN_POINT('',(32.6717047312569,-0.410451051658023,15.7235432561772));
#65422=CARTESIAN_POINT('Origin',(32.6717047312569,-0.410451051658023,15.7235432561772));
#65423=CARTESIAN_POINT('Origin',(32.7343087972847,-0.727153007558476,15.7235432561772));
#65424=CARTESIAN_POINT('',(32.6254061353882,-0.643209811098926,15.7235432561772));
#65425=CARTESIAN_POINT('Origin',(32.6338004550341,-0.632319544909271,15.7235432561772));
#65426=CARTESIAN_POINT('',(32.6312651388532,-0.6188053053131,15.7235432561772));
#65427=CARTESIAN_POINT('Origin',(32.6312651388532,-0.6188053053131,15.7235432561772));
#65428=CARTESIAN_POINT('Origin',(32.6688280683633,-0.939442833186874,15.7235432561772));
#65429=CARTESIAN_POINT('',(32.5668472243157,-0.847214001212625,15.7235432561772));
#65430=CARTESIAN_POINT('Origin',(32.5760701075131,-0.837015916807863,15.7235432561772));
#65431=CARTESIAN_POINT('',(32.574602921884,-0.823344418487278,15.7235432561772));
#65432=CARTESIAN_POINT('Origin',(32.574602921884,-0.823344418487278,15.7235432561772));
#65433=CARTESIAN_POINT('Origin',(32.586893126925,-1.14594068135223,15.7235432561772));
#65434=CARTESIAN_POINT('',(32.492462846542,-1.0459948352816,15.7235432561772));
#65435=CARTESIAN_POINT('Origin',(32.502457431149,-1.0365518072433,15.7235432561772));
#65436=CARTESIAN_POINT('',(32.5020674217591,-1.02280733953168,15.7235432561772));
#65437=CARTESIAN_POINT('Origin',(32.5020674217591,-1.02280733953168,15.7235432561772));
#65438=CARTESIAN_POINT('Origin',(32.48900912913,-1.34537342415311,15.7235432561772));
#65439=CARTESIAN_POINT('',(32.4027116064913,-1.2383267633625,15.7235432561772));
#65440=CARTESIAN_POINT('Origin',(32.4134162725704,-1.22969701109862,15.7235432561772));
#65441=CARTESIAN_POINT('',(32.4141058439571,-1.21596431320991,15.7235432561772));
#65442=CARTESIAN_POINT('Origin',(32.4141058439571,-1.21596431320991,15.7235432561772));
#65443=CARTESIAN_POINT('Origin',(32.3757795623744,-1.53651149241202,15.7235432561772));
#65444=CARTESIAN_POINT('',(32.2981468504039,-1.42302399516182,15.7235432561772));
#65445=CARTESIAN_POINT('Origin',(32.309495600129,-1.41526072396478,15.7235432561772));
#65446=CARTESIAN_POINT('',(32.3112605008555,-1.40162446254804,15.7235432561772));
#65447=CARTESIAN_POINT('Origin',(32.3112605008555,-1.40162446254804,15.7235432561772));
#65448=CARTESIAN_POINT('Origin',(32.2479025245898,-1.71817645637829,15.7235432561772));
#65449=CARTESIAN_POINT('',(32.1794132547725,-1.59894781082747,15.7235432561772));
#65450=CARTESIAN_POINT('Origin',(32.1913361193275,-1.59209888384574,15.7235432561772));
#65451=CARTESIAN_POINT('',(32.194165468194,-1.57864313098713,15.7235432561772));
#65452=CARTESIAN_POINT('Origin',(32.194165468194,-1.57864313098713,15.7235432561772));
#65453=CARTESIAN_POINT('Origin',(32.1061664202378,-1.88924829113934,15.7235432561772));
#65454=CARTESIAN_POINT('',(32.0472428516969,-1.76501358153528,15.7235432561772));
#65455=CARTESIAN_POINT('Origin',(32.0596663226573,-1.75912122468119,15.7235432561772));
#65456=CARTESIAN_POINT('',(32.063542675787,-1.74592893957158,15.7235432561772));
#65457=CARTESIAN_POINT('Origin',(32.063542675787,-1.74592893957158,15.7235432561772));
#65458=CARTESIAN_POINT('Origin',(31.9514450995335,-2.04867228194671,15.7235432561772));
#65459=CARTESIAN_POINT('',(31.9024505156632,-1.92019745658634,15.7235432561772));
#65460=CARTESIAN_POINT('Origin',(31.9152979981993,-1.91529799819931,15.7235432561772));
#65461=CARTESIAN_POINT('',(31.9201974565863,-1.90245051566327,15.7235432561772));
#65462=CARTESIAN_POINT('Origin',(31.9201974565863,-1.90245051566327,15.7235432561772));
#65463=CARTESIAN_POINT('Origin',(31.7846924708693,-2.19546552688321,15.7235432561772));
#65464=CARTESIAN_POINT('',(31.7459289395715,-2.0635426757871,15.7235432561772));
#65465=CARTESIAN_POINT('Origin',(31.7591212246811,-2.05966632265732,15.7235432561772));
#65466=CARTESIAN_POINT('',(31.7650135815352,-2.04724285169692,15.7235432561772));
#65467=CARTESIAN_POINT('Origin',(31.7650135815352,-2.04724285169692,15.7235432561772));
#65468=CARTESIAN_POINT('Origin',(31.6069366196517,-2.32872299678011,15.7235432561772));
#65469=CARTESIAN_POINT('',(31.5786431309871,-2.19416546819406,15.7235432561772));
#65470=CARTESIAN_POINT('Origin',(31.5920988838457,-2.1913361193276,15.7235432561772));
#65471=CARTESIAN_POINT('',(31.5989478108274,-2.17941325477251,15.7235432561772));
#65472=CARTESIAN_POINT('Origin',(31.5989478108274,-2.17941325477251,15.7235432561772));
#65473=CARTESIAN_POINT('Origin',(31.4192734698133,-2.44762311502288,15.7235432561772));
#65474=CARTESIAN_POINT('',(31.401624462548,-2.31126050085554,15.7235432561772));
#65475=CARTESIAN_POINT('Origin',(31.4152607239647,-2.30949560012901,15.7235432561772));
#65476=CARTESIAN_POINT('',(31.4230239951618,-2.29814685040399,15.7235432561772));
#65477=CARTESIAN_POINT('Origin',(31.4230239951618,-2.29814685040399,15.7235432561772));
#65478=CARTESIAN_POINT('Origin',(31.2228600270771,-2.55143282284425,15.7235432561772));
#65479=CARTESIAN_POINT('',(31.2159643132098,-2.41410584395714,15.7235432561772));
#65480=CARTESIAN_POINT('Origin',(31.2296970110986,-2.41341627257041,15.7235432561772));
#65481=CARTESIAN_POINT('',(31.2383267633624,-2.40271160649135,15.7235432561772));
#65482=CARTESIAN_POINT('Origin',(31.2383267633624,-2.40271160649135,15.7235432561772));
#65483=CARTESIAN_POINT('Origin',(31.0189072456319,-2.63951209887528,15.7235432561772));
#65484=CARTESIAN_POINT('',(31.0228073395316,-2.5020674217591,15.7235432561772));
#65485=CARTESIAN_POINT('Origin',(31.0365518072432,-2.50245743114907,15.7235432561772));
#65486=CARTESIAN_POINT('',(31.0459948352815,-2.49246284654201,15.7235432561772));
#65487=CARTESIAN_POINT('Origin',(31.0459948352815,-2.49246284654201,15.7235432561772));
#65488=CARTESIAN_POINT('Origin',(30.8086725621962,-2.71131790508991,15.7235432561772));
#65489=CARTESIAN_POINT('',(30.8233444184872,-2.57460292188405,15.7235432561772));
#65490=CARTESIAN_POINT('Origin',(30.8370159168078,-2.57607010751315,15.7235432561772));
#65491=CARTESIAN_POINT('',(30.8472140012126,-2.56684722431573,15.7235432561772));
#65492=CARTESIAN_POINT('Origin',(30.8472140012126,-2.56684722431573,15.7235432561772));
#65493=CARTESIAN_POINT('Origin',(30.5934521435037,-2.76640753481496,15.7235432561772));
#65494=CARTESIAN_POINT('',(30.618805305313,-2.63126513885325,15.7235432561772));
#65495=CARTESIAN_POINT('Origin',(30.6323195449092,-2.63380045503418,15.7235432561772));
#65496=CARTESIAN_POINT('',(30.6432098110989,-2.62540613538822,15.7235432561772));
#65497=CARTESIAN_POINT('Origin',(30.6432098110989,-2.62540613538822,15.7235432561772));
#65498=CARTESIAN_POINT('Origin',(30.3745728950037,-2.80444134216402,15.7235432561772));
#65499=CARTESIAN_POINT('',(30.410451051658,-2.67170473125697,15.7235432561772));
#65500=CARTESIAN_POINT('Origin',(30.4237247127487,-2.67529254692239,15.7235432561772));
#65501=CARTESIAN_POINT('',(30.4352400186108,-2.66777854459992,15.7235432561772));
#65502=CARTESIAN_POINT('Origin',(30.4352400186108,-2.66777854459992,15.7235432561772));
#65503=CARTESIAN_POINT('Origin',(30.1533842800478,-2.82518483606726,15.7235432561772));
#65504=CARTESIAN_POINT('',(30.1995662307806,-2.69567237556051,15.7235432561772));
#65505=CARTESIAN_POINT('Origin',(30.2125174768313,-2.70029057063379,15.7235432561772));
#65506=CARTESIAN_POINT('',(30.224586826676,-2.69370321195777,15.7235432561772));
#65507=CARTESIAN_POINT('Origin',(30.224586826676,-2.69370321195777,15.7235432561772));
#65508=CARTESIAN_POINT('Origin',(29.93125,-2.82851012598686,15.7235432561772));
#65509=CARTESIAN_POINT('',(29.987451017728,-2.70302030326669,15.7235432561772));
#65510=CARTESIAN_POINT('Origin',(30.,-2.70864040503949,15.7235432561772));
#65511=CARTESIAN_POINT('',(30.012548982272,-2.70302030326669,15.7235432561772));
#65512=CARTESIAN_POINT('Origin',(30.012548982272,-2.70302030326669,15.7235432561772));
#65513=CARTESIAN_POINT('Origin',(29.7095395865638,-2.81439671040468,15.7235432561772));
#65514=CARTESIAN_POINT('',(29.775413173324,-2.69370321195777,15.7235432561772));
#65515=CARTESIAN_POINT('Origin',(29.7874825231687,-2.70029057063378,15.7235432561772));
#65516=CARTESIAN_POINT('',(29.8004337692193,-2.6956723755605,15.7235432561772));
#65517=CARTESIAN_POINT('Origin',(29.8004337692193,-2.6956723755605,15.7235432561772));
#65518=CARTESIAN_POINT('Origin',(29.4896199581644,-2.78293160322098,15.7235432561772));
#65519=CARTESIAN_POINT('',(29.5647599813891,-2.66777854459992,15.7235432561772));
#65520=CARTESIAN_POINT('Origin',(29.5762752872513,-2.67529254692239,15.7235432561772));
#65521=CARTESIAN_POINT('',(29.589548948342,-2.67170473125696,15.7235432561772));
#65522=CARTESIAN_POINT('Origin',(29.589548948342,-2.67170473125696,15.7235432561772));
#65523=CARTESIAN_POINT('Origin',(29.2728469924415,-2.73430879728476,15.7235432561772));
#65524=CARTESIAN_POINT('',(29.3567901889011,-2.62540613538822,15.7235432561772));
#65525=CARTESIAN_POINT('Origin',(29.3676804550907,-2.63380045503417,15.7235432561772));
#65526=CARTESIAN_POINT('',(29.3811946946869,-2.63126513885324,15.7235432561772));
#65527=CARTESIAN_POINT('Origin',(29.3811946946869,-2.63126513885324,15.7235432561772));
#65528=CARTESIAN_POINT('Origin',(29.0605571668131,-2.66882806836334,15.7235432561772));
#65529=CARTESIAN_POINT('',(29.1527859987874,-2.56684722431572,15.7235432561772));
#65530=CARTESIAN_POINT('Origin',(29.1629840831921,-2.57607010751314,15.7235432561772));
#65531=CARTESIAN_POINT('',(29.1766555815127,-2.57460292188404,15.7235432561772));
#65532=CARTESIAN_POINT('Origin',(29.1766555815127,-2.57460292188404,15.7235432561772));
#65533=CARTESIAN_POINT('Origin',(28.8540593186477,-2.58689312692507,15.7235432561772));
#65534=CARTESIAN_POINT('',(28.9540051647184,-2.49246284654199,15.7235432561772));
#65535=CARTESIAN_POINT('Origin',(28.9634481927567,-2.50245743114906,15.7235432561772));
#65536=CARTESIAN_POINT('',(28.9771926604683,-2.50206742175908,15.7235432561772));
#65537=CARTESIAN_POINT('Origin',(28.9771926604683,-2.50206742175908,15.7235432561772));
#65538=CARTESIAN_POINT('Origin',(28.6546265758469,-2.48900912913005,15.7235432561772));
#65539=CARTESIAN_POINT('',(28.7616732366375,-2.40271160649133,15.7235432561772));
#65540=CARTESIAN_POINT('Origin',(28.7703029889014,-2.4134162725704,15.7235432561772));
#65541=CARTESIAN_POINT('',(28.7840356867901,-2.41410584395713,15.7235432561772));
#65542=CARTESIAN_POINT('Origin',(28.7840356867901,-2.41410584395713,15.7235432561772));
#65543=CARTESIAN_POINT('Origin',(28.463488507588,-2.37577956237441,15.7235432561772));
#65544=CARTESIAN_POINT('',(28.5769760048382,-2.29814685040397,15.7235432561772));
#65545=CARTESIAN_POINT('Origin',(28.5847392760352,-2.30949560012899,15.7235432561772));
#65546=CARTESIAN_POINT('',(28.5983755374519,-2.31126050085552,15.7235432561772));
#65547=CARTESIAN_POINT('Origin',(28.5983755374519,-2.31126050085552,15.7235432561772));
#65548=CARTESIAN_POINT('Origin',(28.2818235436217,-2.24790252458987,15.7235432561772));
#65549=CARTESIAN_POINT('',(28.4010521891725,-2.17941325477249,15.7235432561772));
#65550=CARTESIAN_POINT('Origin',(28.4079011161542,-2.19133611932757,15.7235432561772));
#65551=CARTESIAN_POINT('',(28.4213568690129,-2.19416546819403,15.7235432561772));
#65552=CARTESIAN_POINT('Origin',(28.4213568690129,-2.19416546819403,15.7235432561772));
#65553=CARTESIAN_POINT('Origin',(28.1107517088606,-2.10616642023779,15.7235432561772));
#65554=CARTESIAN_POINT('',(28.2349864184647,-2.04724285169689,15.7235432561772));
#65555=CARTESIAN_POINT('Origin',(28.2408787753188,-2.0596663226573,15.7235432561772));
#65556=CARTESIAN_POINT('',(28.2540710604284,-2.06354267578707,15.7235432561772));
#65557=CARTESIAN_POINT('Origin',(28.2540710604284,-2.06354267578707,15.7235432561772));
#65558=CARTESIAN_POINT('Origin',(27.9513277180533,-1.95144509953353,15.7235432561772));
#65559=CARTESIAN_POINT('',(28.0798025434136,-1.90245051566325,15.7235432561772));
#65560=CARTESIAN_POINT('Origin',(28.0847020018007,-1.91529799819928,15.7235432561772));
#65561=CARTESIAN_POINT('',(28.0975494843367,-1.92019745658631,15.7235432561772));
#65562=CARTESIAN_POINT('Origin',(28.0975494843367,-1.92019745658631,15.7235432561772));
#65563=CARTESIAN_POINT('Origin',(27.8045344731168,-1.78469247086931,15.7235432561772));
#65564=CARTESIAN_POINT('',(27.9364573242129,-1.74592893957155,15.7235432561772));
#65565=CARTESIAN_POINT('Origin',(27.9403336773427,-1.75912122468116,15.7235432561772));
#65566=CARTESIAN_POINT('',(27.9527571483031,-1.76501358153525,15.7235432561772));
#65567=CARTESIAN_POINT('Origin',(27.9527571483031,-1.76501358153525,15.7235432561772));
#65568=CARTESIAN_POINT('Origin',(27.6712770032199,-1.6069366196517,15.7235432561772));
#65569=CARTESIAN_POINT('',(27.8058345318059,-1.5786431309871,15.7235432561772));
#65570=CARTESIAN_POINT('Origin',(27.8086638806724,-1.59209888384571,15.7235432561772));
#65571=CARTESIAN_POINT('',(27.8205867452275,-1.59894781082744,15.7235432561772));
#65572=CARTESIAN_POINT('Origin',(27.8205867452275,-1.59894781082744,15.7235432561772));
#65573=CARTESIAN_POINT('Origin',(27.5523768849771,-1.4192734698133,15.7235432561772));
#65574=CARTESIAN_POINT('',(27.6887394991444,-1.40162446254801,15.7235432561772));
#65575=CARTESIAN_POINT('Origin',(27.690504399871,-1.41526072396474,15.7235432561772));
#65576=CARTESIAN_POINT('',(27.701853149596,-1.42302399516179,15.7235432561772));
#65577=CARTESIAN_POINT('Origin',(27.701853149596,-1.42302399516179,15.7235432561772));
#65578=CARTESIAN_POINT('Origin',(27.4485671771557,-1.22286002707717,15.7235432561772));
#65579=CARTESIAN_POINT('',(27.5858941560428,-1.21596431320988,15.7235432561772));
#65580=CARTESIAN_POINT('Origin',(27.5865837274296,-1.22969701109859,15.7235432561772));
#65581=CARTESIAN_POINT('',(27.5972883935086,-1.23832676336246,15.7235432561772));
#65582=CARTESIAN_POINT('Origin',(27.5972883935086,-1.23832676336246,15.7235432561772));
#65583=CARTESIAN_POINT('Origin',(27.3604879011247,-1.01890724563189,15.7235432561772));
#65584=CARTESIAN_POINT('',(27.4979325782409,-1.02280733953164,15.7235432561772));
#65585=CARTESIAN_POINT('Origin',(27.4975425688509,-1.03655180724326,15.7235432561772));
#65586=CARTESIAN_POINT('',(27.507537153458,-1.04599483528157,15.7235432561772));
#65587=CARTESIAN_POINT('Origin',(27.507537153458,-1.04599483528157,15.7235432561772));
#65588=CARTESIAN_POINT('Origin',(27.2886820949101,-0.808672562196254,15.7235432561772));
#65589=CARTESIAN_POINT('',(27.4253970781159,-0.823344418487241,15.7235432561772));
#65590=CARTESIAN_POINT('Origin',(27.4239298924868,-0.837015916807826,15.7235432561772));
#65591=CARTESIAN_POINT('',(27.4331527756843,-0.847214001212589,15.7235432561772));
#65592=CARTESIAN_POINT('Origin',(27.4331527756843,-0.847214001212589,15.7235432561772));
#65593=CARTESIAN_POINT('Origin',(27.233592465185,-0.593452143503757,15.7235432561772));
#65594=CARTESIAN_POINT('',(27.3687348611467,-0.618805305313063,15.7235432561772));
#65595=CARTESIAN_POINT('Origin',(27.3661995449658,-0.632319544909233,15.7235432561772));
#65596=CARTESIAN_POINT('',(27.3745938646118,-0.643209811098888,15.7235432561772));
#65597=CARTESIAN_POINT('Origin',(27.3745938646118,-0.643209811098888,15.7235432561772));
#65598=CARTESIAN_POINT('Origin',(27.195558657836,-0.374572895003696,15.7235432561772));
#65599=CARTESIAN_POINT('',(27.328295268743,-0.410451051657984,15.7235432561772));
#65600=CARTESIAN_POINT('Origin',(27.3247074530776,-0.423724712748689,15.7235432561772));
#65601=CARTESIAN_POINT('',(27.3322214554001,-0.435240018610796,15.7235432561772));
#65602=CARTESIAN_POINT('Origin',(27.3322214554001,-0.435240018610796,15.7235432561772));
#65603=CARTESIAN_POINT('Origin',(27.1748151639327,-0.153384280047813,15.7235432561772));
#65604=CARTESIAN_POINT('',(27.3043276244395,-0.199566230780611,15.7235432561772));
#65605=CARTESIAN_POINT('Origin',(27.2997094293662,-0.212517476831286,15.7235432561772));
#65606=CARTESIAN_POINT('',(27.3062967880422,-0.224586826675978,15.7235432561772));
#65607=CARTESIAN_POINT('Origin',(27.3062967880422,-0.224586826675978,15.7235432561772));
#65608=CARTESIAN_POINT('Origin',(27.1714898740131,0.068750000000016,15.7235432561772));
#65609=CARTESIAN_POINT('Origin',(27.2969796967333,-0.0125489822720016,15.7235432561772));
#65610=CARTESIAN_POINT('Origin',(27.1856032895953,0.29046041343615,15.7235432561772));
#65611=CARTESIAN_POINT('Origin',(27.3043276244395,0.199566230780642,15.7235432561772));
#65612=CARTESIAN_POINT('Origin',(27.217068396779,0.510380041835561,15.7235432561772));
#65613=CARTESIAN_POINT('Origin',(27.328295268743,0.410451051658016,15.7235432561772));
#65614=CARTESIAN_POINT('Origin',(27.2656912027152,0.727153007558468,15.7235432561772));
#65615=CARTESIAN_POINT('Origin',(27.3687348611468,0.618805305313091,15.7235432561772));
#65616=CARTESIAN_POINT('Origin',(27.3311719316367,0.939442833186866,15.7235432561772));
#65617=CARTESIAN_POINT('Origin',(27.4253970781159,0.823344418487269,15.7235432561772));
#65618=CARTESIAN_POINT('Origin',(27.4131068730749,1.14594068135223,15.7235432561772));
#65619=CARTESIAN_POINT('Origin',(27.4979325782409,1.02280733953167,15.7235432561772));
#65620=CARTESIAN_POINT('',(0.,0.,0.));
#65621=CARTESIAN_POINT('Origin',(30.,-1.32966554433622E-14,16.));
#65622=CARTESIAN_POINT('',(29.9999999999999,-1.50000000000001,30.25));
#65623=CARTESIAN_POINT('',(30.,-1.50000000000001,30.3125));
#65624=CARTESIAN_POINT('',(30.,-1.50000000000001,16.));
#65625=CARTESIAN_POINT('',(30.,-1.50000000000002,30.75));
#65626=CARTESIAN_POINT('Ctrl Pts',(29.9999999999999,-1.50000000000001,30.25));
#65627=CARTESIAN_POINT('Ctrl Pts',(30.1658036138247,-1.50000000000003,30.2579772300895));
#65628=CARTESIAN_POINT('Ctrl Pts',(30.3306771390814,-1.47251502213024,30.2666731828795));
#65629=CARTESIAN_POINT('Ctrl Pts',(30.6740051197163,-1.35441705513551,30.2864720571327));
#65630=CARTESIAN_POINT('Ctrl Pts',(30.8456956760641,-1.25440329321601,30.2975106829297));
#65631=CARTESIAN_POINT('Ctrl Pts',(31.1355371924707,-0.998320157723232,
30.31856910982));
#65632=CARTESIAN_POINT('Ctrl Pts',(31.2526807741055,-0.846671576374736,
30.3279626902015));
#65633=CARTESIAN_POINT('Ctrl Pts',(31.4282014939959,-0.499786966349004,
30.3472340574251));
#65634=CARTESIAN_POINT('Ctrl Pts',(31.4817951924464,-0.306278304449559,
30.3579845386417));
#65635=CARTESIAN_POINT('Ctrl Pts',(31.5101111597472,0.0860175204635018,
30.3797787511369));
#65636=CARTESIAN_POINT('Ctrl Pts',(31.4862462216493,0.280921846793951,30.3906067692664));
#65637=CARTESIAN_POINT('Ctrl Pts',(31.3664146176937,0.647698903970874,30.4109832724428));
#65638=CARTESIAN_POINT('Ctrl Pts',(31.2727727808063,0.816486916731949,30.4197772164968));
#65639=CARTESIAN_POINT('Ctrl Pts',(31.0215777110749,1.11639419547156,30.440193602667));
#65640=CARTESIAN_POINT('Ctrl Pts',(30.8638920671928,1.2424306705166,30.4512812699412));
#65641=CARTESIAN_POINT('Ctrl Pts',(30.51519869364,1.4218077371841,30.4730404839947));
#65642=CARTESIAN_POINT('Ctrl Pts',(30.3288784064271,1.47608428096084,30.4835125047644));
#65643=CARTESIAN_POINT('Ctrl Pts',(29.9417076474062,1.51169090841865,30.5031293395779));
#65644=CARTESIAN_POINT('Ctrl Pts',(29.7444133180912,1.49107258678014,30.5125449036674));
#65645=CARTESIAN_POINT('Ctrl Pts',(29.3680874803138,1.37464650826943,30.5338849467157));
#65646=CARTESIAN_POINT('Ctrl Pts',(29.192868275455,1.27964935682832,30.5449539944024));
#65647=CARTESIAN_POINT('Ctrl Pts',(28.8948089362382,1.03185947909864,30.5661774332058));
#65648=CARTESIAN_POINT('Ctrl Pts',(28.7730426891403,0.883581363472215,30.5759121464738));
#65649=CARTESIAN_POINT('Ctrl Pts',(28.5872420086988,0.541893735862482,30.5948947924521));
#65650=CARTESIAN_POINT('Ctrl Pts',(28.5279457886126,0.350092848014275,30.6055503973326));
#65651=CARTESIAN_POINT('Ctrl Pts',(28.4879441501424,-0.0417086531130522,
30.6273171473952));
#65652=CARTESIAN_POINT('Ctrl Pts',(28.5061747163527,-0.237794814766365,
30.6382108230426));
#65653=CARTESIAN_POINT('Ctrl Pts',(28.6154381406337,-0.60772707143957,30.65876261508));
#65654=CARTESIAN_POINT('Ctrl Pts',(28.7037802077497,-0.77855877037785,30.6675955620118));
#65655=CARTESIAN_POINT('Ctrl Pts',(28.9458348287961,-1.08578773838532,30.687775558397));
#65656=CARTESIAN_POINT('Ctrl Pts',(29.1002278810903,-1.21679626071423,30.6988429232091));
#65657=CARTESIAN_POINT('Ctrl Pts',(29.3881527190005,-1.37554036843891,30.7171052719799));
#65658=CARTESIAN_POINT('Ctrl Pts',(29.5080276522,-1.42282651307167,30.7241862614101));
#65659=CARTESIAN_POINT('Ctrl Pts',(29.7526687702711,-1.48465507368766,30.7376740227083));
#65660=CARTESIAN_POINT('Ctrl Pts',(29.8761199631302,-1.50000000000009,30.7440398189472));
#65661=CARTESIAN_POINT('Ctrl Pts',(30.0000000000009,-1.50000000000001,30.75));
#65662=CARTESIAN_POINT('',(30.,-1.50000000000001,30.85));
#65663=CARTESIAN_POINT('',(30.,-1.50000000000001,16.));
#65664=CARTESIAN_POINT('Origin',(30.,-1.32966554433622E-14,30.85));
#65665=CARTESIAN_POINT('',(28.9490560961666,-1.07028823734334,30.75));
#65666=CARTESIAN_POINT('Origin',(30.,-1.5916987375435E-14,30.75));
#65667=CARTESIAN_POINT('Ctrl Pts',(28.9490560961666,-1.07028823734332,30.75));
#65668=CARTESIAN_POINT('Ctrl Pts',(28.8761609488349,-0.998710593084209,
30.7445045626927));
#65669=CARTESIAN_POINT('Ctrl Pts',(28.8107674297946,-0.919873442584925,
30.7391683946938));
#65670=CARTESIAN_POINT('Ctrl Pts',(28.6983154051604,-0.752052754529888,
30.7290963583567));
#65671=CARTESIAN_POINT('Ctrl Pts',(28.6511686993163,-0.663795554008335,
30.7243775307781));
#65672=CARTESIAN_POINT('Ctrl Pts',(28.5395598759442,-0.392939439769756,
30.709329968876));
#65673=CARTESIAN_POINT('Ctrl Pts',(28.5011631241701,-0.201888114570883,
30.6987160063649));
#65674=CARTESIAN_POINT('Ctrl Pts',(28.4988436150777,0.191908857459164,30.6768383968077));
#65675=CARTESIAN_POINT('Ctrl Pts',(28.5379718270057,0.390884408078152,30.6657841995511));
#65676=CARTESIAN_POINT('Ctrl Pts',(28.6882496652404,0.752033457565058,30.6457203634686));
#65677=CARTESIAN_POINT('Ctrl Pts',(28.7941652988744,0.912256576314666,30.6368419553212));
#65678=CARTESIAN_POINT('Ctrl Pts',(29.0637866570552,1.18813740110581,30.6162064354332));
#65679=CARTESIAN_POINT('Ctrl Pts',(29.2263162356668,1.29983562680085,30.6052839989448));
#65680=CARTESIAN_POINT('Ctrl Pts',(29.5881540142218,1.45598200117754,30.5835376714189));
#65681=CARTESIAN_POINT('Ctrl Pts',(29.7845106480132,1.49769538170803,30.5729317534561));
#65682=CARTESIAN_POINT('Ctrl Pts',(30.1735918421599,1.5020241460186,30.5540918323215));
#65683=CARTESIAN_POINT('Ctrl Pts',(30.3626153088868,1.46791385953203,30.544162381137));
#65684=CARTESIAN_POINT('Ctrl Pts',(30.7246797057952,1.32812661690519,30.5228595707569));
#65685=CARTESIAN_POINT('Ctrl Pts',(30.8932233177541,1.2211620663456,30.5117792749302));
#65686=CARTESIAN_POINT('Ctrl Pts',(31.1776737025205,0.949411483501645,30.4905450221109));
#65687=CARTESIAN_POINT('Ctrl Pts',(31.2913339229655,0.787872571372875,30.4812706984095));
#65688=CARTESIAN_POINT('Ctrl Pts',(31.4489779041399,0.433069950768308,30.4615594417092));
#65689=CARTESIAN_POINT('Ctrl Pts',(31.4925441992832,0.243681023738972,30.451037834652));
#65690=CARTESIAN_POINT('Ctrl Pts',(31.5059639907605,-0.148777135728896,
30.4292346035705));
#65691=CARTESIAN_POINT('Ctrl Pts',(31.4726973264507,-0.348194823891665,
30.418155843117));
#65692=CARTESIAN_POINT('Ctrl Pts',(31.3331360295961,-0.713588890875335,
30.3978561727291));
#65693=CARTESIAN_POINT('Ctrl Pts',(31.2315888806866,-0.877298264710928,
30.3890521180742));
#65694=CARTESIAN_POINT('Ctrl Pts',(30.969887909143,-1.16071911064266,30.3685882229343));
#65695=CARTESIAN_POINT('Ctrl Pts',(30.8111118646049,-1.27673016594729,30.3577265776157));
#65696=CARTESIAN_POINT('Ctrl Pts',(30.4544959445291,-1.44324278722566,30.3359435355702));
#65697=CARTESIAN_POINT('Ctrl Pts',(30.2594138454525,-1.49071962728781,30.3252388425894));
#65698=CARTESIAN_POINT('Ctrl Pts',(30.0404799678322,-1.49959063127059,30.3144589647139));
#65699=CARTESIAN_POINT('Ctrl Pts',(30.0202329450965,-1.50000000000001,30.3134734580248));
#65700=CARTESIAN_POINT('Ctrl Pts',(30.,-1.50000000000001,30.3125));
#65701=CARTESIAN_POINT('Origin',(30.,-1.32966554433622E-14,16.));
#65702=CARTESIAN_POINT('',(30.0000000422953,-1.50000000000001,29.7500000040699));
#65703=CARTESIAN_POINT('',(30.0000000000001,-1.50000000000001,29.8125));
#65704=CARTESIAN_POINT('',(30.,-1.50000000000001,16.));
#65705=CARTESIAN_POINT('Ctrl Pts',(30.0000000423936,-1.50000000000001,29.7500000020397));
#65706=CARTESIAN_POINT('Ctrl Pts',(30.195284159332,-1.49999999448081,29.7593956136499));
#65707=CARTESIAN_POINT('Ctrl Pts',(30.3888046451199,-1.46186371850976,29.7697657133627));
#65708=CARTESIAN_POINT('Ctrl Pts',(30.7506676874449,-1.3133124636612,29.7913022808498));
#65709=CARTESIAN_POINT('Ctrl Pts',(30.9154176613495,-1.20428706546983,29.8022573009481));
#65710=CARTESIAN_POINT('Ctrl Pts',(31.18981388205,-0.933008136594988,29.8229947210741));
#65711=CARTESIAN_POINT('Ctrl Pts',(31.2983679232815,-0.774850228387389,
29.8319527650896));
#65712=CARTESIAN_POINT('Ctrl Pts',(31.4541476549185,-0.418353419581691,
29.8517581433566));
#65713=CARTESIAN_POINT('Ctrl Pts',(31.4967395542031,-0.22207441884915,29.8626625322862));
#65714=CARTESIAN_POINT('Ctrl Pts',(31.5028167108854,0.170195075492689,29.8844552819718));
#65715=CARTESIAN_POINT('Ctrl Pts',(31.4683656451658,0.362410265994727,29.8951339036664));
#65716=CARTESIAN_POINT('Ctrl Pts',(31.3284167977355,0.722950513431523,29.9151639174129));
#65717=CARTESIAN_POINT('Ctrl Pts',(31.2243440361084,0.887881539566768,29.9240904295301));
#65718=CARTESIAN_POINT('Ctrl Pts',(30.9555499935672,1.17320843290826,29.9449485359688));
#65719=CARTESIAN_POINT('Ctrl Pts',(30.7918896841479,1.28933944326239,29.9560485076758));
#65720=CARTESIAN_POINT('Ctrl Pts',(30.4356884609645,1.44801470954154,29.9775938933022));
#65721=CARTESIAN_POINT('Ctrl Pts',(30.24769400318,1.49172420709908,29.9878529335795));
#65722=CARTESIAN_POINT('Ctrl Pts',(29.8564383086953,1.50648133745832,30.007087152245));
#65723=CARTESIAN_POINT('Ctrl Pts',(29.6568006042803,1.4738887523207,30.0172375010609));
#65724=CARTESIAN_POINT('Ctrl Pts',(29.2858871639067,1.33362042993594,30.0389794245699));
#65725=CARTESIAN_POINT('Ctrl Pts',(29.1177424716204,1.22887149382963,30.049978982519));
#65726=CARTESIAN_POINT('Ctrl Pts',(28.8358984689122,0.964859074366596,30.0708728867402));
#65727=CARTESIAN_POINT('Ctrl Pts',(28.7232154667205,0.809870978335536,30.0800071678703));
#65728=CARTESIAN_POINT('Ctrl Pts',(28.5578456280088,0.457982195266601,30.0995565447074));
#65729=CARTESIAN_POINT('Ctrl Pts',(28.5099042682065,0.262965364708001,30.1103908130718));
#65730=CARTESIAN_POINT('Ctrl Pts',(28.4930631778567,-0.129475272168894,
30.1321930706761));
#65731=CARTESIAN_POINT('Ctrl Pts',(28.5224126203679,-0.323064053208287,
30.142948002956));
#65732=CARTESIAN_POINT('Ctrl Pts',(28.6526173206986,-0.686662322858743,
30.1631479068255));
#65733=CARTESIAN_POINT('Ctrl Pts',(28.7515795011674,-0.85345907766542,30.1719758706799));
#65734=CARTESIAN_POINT('Ctrl Pts',(29.0118186458561,-1.14595641051804,30.1926215582791));
#65735=CARTESIAN_POINT('Ctrl Pts',(29.172636650331,-1.26695599442051,30.2037200176798));
#65736=CARTESIAN_POINT('Ctrl Pts',(29.5253217759949,-1.43577307549295,30.2253779520631));
#65737=CARTESIAN_POINT('Ctrl Pts',(29.7125728326969,-1.48464476779679,30.2357446197376));
#65738=CARTESIAN_POINT('Ctrl Pts',(29.9359811243456,-1.49897644179293,30.2468914582366));
#65739=CARTESIAN_POINT('Ctrl Pts',(29.9680065223165,-1.50000000000001,30.2484607130873));
#65740=CARTESIAN_POINT('Ctrl Pts',(29.9999999999999,-1.50000000000001,30.25));
#65741=CARTESIAN_POINT('Ctrl Pts',(30.,-1.50000000000001,30.3125));
#65742=CARTESIAN_POINT('Ctrl Pts',(29.8305649734084,-1.50000000000001,30.3043480534823));
#65743=CARTESIAN_POINT('Ctrl Pts',(29.6621927434306,-1.471296371185,30.2954499177677));
#65744=CARTESIAN_POINT('Ctrl Pts',(29.3161242189391,-1.34950305066004,30.2754165403276));
#65745=CARTESIAN_POINT('Ctrl Pts',(29.1449154106261,-1.2480688680691,30.264361636514));
#65746=CARTESIAN_POINT('Ctrl Pts',(28.8512754656375,-0.984586302069753,
30.242914917907));
#65747=CARTESIAN_POINT('Ctrl Pts',(28.7318299827785,-0.825047829175388,
30.2333359905097));
#65748=CARTESIAN_POINT('Ctrl Pts',(28.5638630976012,-0.47370253085421,30.2138168072696));
#65749=CARTESIAN_POINT('Ctrl Pts',(28.5150825240157,-0.286153024679847,
30.2033973902599));
#65750=CARTESIAN_POINT('Ctrl Pts',(28.4904050702493,0.104624550291977,30.1816875249837));
#65751=CARTESIAN_POINT('Ctrl Pts',(28.5176966903753,0.304322584656878,30.1705931897412));
#65752=CARTESIAN_POINT('Ctrl Pts',(28.6462704703314,0.673930577459572,30.1500594123633));
#65753=CARTESIAN_POINT('Ctrl Pts',(28.7433931121189,0.841252262459088,30.141257075347));
#65754=CARTESIAN_POINT('Ctrl Pts',(28.9970706151381,1.13219704351489,30.1209702113185));
#65755=CARTESIAN_POINT('Ctrl Pts',(29.1519620886259,1.25242080149054,30.1101784429931));
#65756=CARTESIAN_POINT('Ctrl Pts',(29.5030294160994,1.42917820121841,30.0883777805545));
#65757=CARTESIAN_POINT('Ctrl Pts',(29.696654967539,1.48240812812318,30.0775833577866));
#65758=CARTESIAN_POINT('Ctrl Pts',(30.0844620336651,1.50960977413546,30.0581693803401));
#65759=CARTESIAN_POINT('Ctrl Pts',(30.2746950762916,1.48681483093204,30.0489174722834));
#65760=CARTESIAN_POINT('Ctrl Pts',(30.642872277816,1.3694262764412,30.0279427452356));
#65761=CARTESIAN_POINT('Ctrl Pts',(30.8165454300566,1.27352463490858,30.0169229573155));
#65762=CARTESIAN_POINT('Ctrl Pts',(31.1192034235311,1.01839257572982,29.9952743161713));
#65763=CARTESIAN_POINT('Ctrl Pts',(31.2444516003803,0.860842115189833,29.9853245619549));
#65764=CARTESIAN_POINT('Ctrl Pts',(31.4225185229473,0.51295924874081,29.9659977360411));
#65765=CARTESIAN_POINT('Ctrl Pts',(31.476317491186,0.327339595503408,29.9556855330835));
#65766=CARTESIAN_POINT('Ctrl Pts',(31.5118899575654,-0.0614966036299657,
29.9340835220205));
#65767=CARTESIAN_POINT('Ctrl Pts',(31.49041063713,-0.261302093346022,29.9229832170363));
#65768=CARTESIAN_POINT('Ctrl Pts',(31.3726040951777,-0.63490434793495,29.9022275362258));
#65769=CARTESIAN_POINT('Ctrl Pts',(31.2797800327084,-0.805795593106099,
29.8933569012793));
#65770=CARTESIAN_POINT('Ctrl Pts',(31.0338687856651,-1.10392432463312,29.873244137236));
#65771=CARTESIAN_POINT('Ctrl Pts',(30.8828092373533,-1.22807490132932,29.8625276541988));
#65772=CARTESIAN_POINT('Ctrl Pts',(30.5373473005298,-1.41449618106684,29.8407282401322));
#65773=CARTESIAN_POINT('Ctrl Pts',(30.3452845785499,-1.47320733373471,29.8298567527606));
#65774=CARTESIAN_POINT('Ctrl Pts',(30.0982962322989,-1.49758712755237,29.8172963039161));
#65775=CARTESIAN_POINT('Ctrl Pts',(30.0491225084885,-1.50000000000001,29.8148634077916));
#65776=CARTESIAN_POINT('Ctrl Pts',(30.0000000000002,-1.50000000000001,29.8125));
#65777=CARTESIAN_POINT('Origin',(30.,-1.32966554433622E-14,16.));
#65778=CARTESIAN_POINT('',(30.,-1.50000000000001,29.25));
#65779=CARTESIAN_POINT('',(30.,-1.50000000000001,29.3125));
#65780=CARTESIAN_POINT('',(30.,-1.50000000000001,16.));
#65781=CARTESIAN_POINT('Ctrl Pts',(30.0000000000001,-1.50000000000001,29.25));
#65782=CARTESIAN_POINT('Ctrl Pts',(30.0257058009192,-1.50000000000001,29.2512367709234));
#65783=CARTESIAN_POINT('Ctrl Pts',(30.0514327409082,-1.49933922123128,29.2524929138666));
#65784=CARTESIAN_POINT('Ctrl Pts',(30.2757518694164,-1.4877855903611,29.2636064071598));
#65785=CARTESIAN_POINT('Ctrl Pts',(30.4703136581261,-1.43816783024051,29.2743455366981));
#65786=CARTESIAN_POINT('Ctrl Pts',(30.8249043497727,-1.26783071251083,29.2961373759079));
#65787=CARTESIAN_POINT('Ctrl Pts',(30.9822510518058,-1.15024113589767,29.3069740997672));
#65788=CARTESIAN_POINT('Ctrl Pts',(31.2409808029183,-0.864020908483806,
29.3273728025942));
#65789=CARTESIAN_POINT('Ctrl Pts',(31.3408899715229,-0.698983488656709,
29.3361675839636));
#65790=CARTESIAN_POINT('Ctrl Pts',(31.4763980403227,-0.332018378933428,
29.3565545345038));
#65791=CARTESIAN_POINT('Ctrl Pts',(31.5074559153656,-0.132477013527386,
29.3676401659153));
#65792=CARTESIAN_POINT('Ctrl Pts',(31.4898677318573,0.259397054955175,29.3894109474976));
#65793=CARTESIAN_POINT('Ctrl Pts',(31.444367356687,0.448123046557066,29.3998957248088));
#65794=CARTESIAN_POINT('Ctrl Pts',(31.2829132867175,0.801659109129801,29.419536617174));
#65795=CARTESIAN_POINT('Ctrl Pts',(31.1671346623852,0.962462537199801,29.4289146111855));
#65796=CARTESIAN_POINT('Ctrl Pts',(30.8792964511142,1.23119218867364,29.4502279461232));
#65797=CARTESIAN_POINT('Ctrl Pts',(30.7097525390342,1.33613064071083,29.4613000883974));
#65798=CARTESIAN_POINT('Ctrl Pts',(30.346523773562,1.47177468007876,29.4825438305068));
#65799=CARTESIAN_POINT('Ctrl Pts',(30.1572989096959,1.50379960302192,29.4923264081504));
#65800=CARTESIAN_POINT('Ctrl Pts',(29.7684168962525,1.49529312487305,29.5112727938055));
#65801=CARTESIAN_POINT('Ctrl Pts',(29.5725063077327,1.45146676708809,29.5219159452176));
#65802=CARTESIAN_POINT('Ctrl Pts',(29.2125442219205,1.29150806105852,29.5436779265358));
#65803=CARTESIAN_POINT('Ctrl Pts',(29.051374885103,1.17821798386326,29.5545791364576));
#65804=CARTESIAN_POINT('Ctrl Pts',(28.784644635234,0.899571593555892,29.5751523790963));
#65805=CARTESIAN_POINT('Ctrl Pts',(28.6803243600253,0.738084850822973,29.5839952860653));
#65806=CARTESIAN_POINT('Ctrl Pts',(28.5339435846744,0.375376943196454,29.6041457253779));
#65807=CARTESIAN_POINT('Ctrl Pts',(28.4969501646145,0.176221200716502,29.6152099332935));
#65808=CARTESIAN_POINT('Ctrl Pts',(28.5033188891713,-0.217123692718195,
29.6370624273732));
#65809=CARTESIAN_POINT('Ctrl Pts',(28.5436046203998,-0.407585858885439,
29.6476436588269));
#65810=CARTESIAN_POINT('Ctrl Pts',(28.6948329707667,-0.764496194056087,
29.6674720107808));
#65811=CARTESIAN_POINT('Ctrl Pts',(28.8049699824855,-0.927268122072015,
29.6765948726435));
#65812=CARTESIAN_POINT('Ctrl Pts',(29.0837280295094,-1.20402609540407,29.6976943469156));
#65813=CARTESIAN_POINT('Ctrl Pts',(29.2505451199729,-1.31436112105669,29.7087851997463));
#65814=CARTESIAN_POINT('Ctrl Pts',(29.6105129505334,-1.46104267840857,29.7301786477734));
#65815=CARTESIAN_POINT('Ctrl Pts',(29.799201008928,-1.49868271487424,29.7403024627842));
#65816=CARTESIAN_POINT('Ctrl Pts',(29.9932712661576,-1.49998868274459,29.7496759492739));
#65817=CARTESIAN_POINT('Ctrl Pts',(29.9966359009771,-1.50000000009509,29.7498381447076));
#65818=CARTESIAN_POINT('Ctrl Pts',(30.0000000423936,-1.50000000000001,29.7500000020397));
#65819=CARTESIAN_POINT('Ctrl Pts',(30.0000000000002,-1.50000000000001,29.8125));
#65820=CARTESIAN_POINT('Ctrl Pts',(29.8597537134085,-1.50000000000001,29.8057523973903));
#65821=CARTESIAN_POINT('Ctrl Pts',(29.7199776172616,-1.48033650865739,29.798481208736));
#65822=CARTESIAN_POINT('Ctrl Pts',(29.396444095828,-1.38712528602054,29.7803259942996));
#65823=CARTESIAN_POINT('Ctrl Pts',(29.2206000446906,-1.29650603057681,29.7693484919046));
#65824=CARTESIAN_POINT('Ctrl Pts',(28.911420128637,-1.05097346611518,29.747652717245));
#65825=CARTESIAN_POINT('Ctrl Pts',(28.7818724475201,-0.897590413872414,
29.737366134104));
#65826=CARTESIAN_POINT('Ctrl Pts',(28.5939020851709,-0.556198210295242,
29.7183999005719));
#65827=CARTESIAN_POINT('Ctrl Pts',(28.5345980064858,-0.372882477899534,
29.7082156932166));
#65828=CARTESIAN_POINT('Ctrl Pts',(28.4870031451474,0.0134445146485481,
29.6867530825195));
#65829=CARTESIAN_POINT('Ctrl Pts',(28.502033993864,0.213177772539474,29.6756567904145));
#65830=CARTESIAN_POINT('Ctrl Pts',(28.6077791980133,0.591085049341038,29.6546619417033));
#65831=CARTESIAN_POINT('Ctrl Pts',(28.6958240597398,0.766015662165753,29.6456356480104));
#65832=CARTESIAN_POINT('Ctrl Pts',(28.9331445661562,1.07197536298372,29.6257186792435));
#65833=CARTESIAN_POINT('Ctrl Pts',(29.079894739921,1.20029258347643,29.6150937909803));
#65834=CARTESIAN_POINT('Ctrl Pts',(29.4205899711736,1.39807482372058,29.5932081329061));
#65835=CARTESIAN_POINT('Ctrl Pts',(29.6127784235583,1.46301280498413,29.5821576288666));
#65836=CARTESIAN_POINT('Ctrl Pts',(30.000882127086,1.51202551870596,29.5621235164545));
#65837=CARTESIAN_POINT('Ctrl Pts',(30.1924980276144,1.49972435337029,29.5532307774773));
#65838=CARTESIAN_POINT('Ctrl Pts',(30.565900986819,1.40283604422102,29.5325740773055));
#65839=CARTESIAN_POINT('Ctrl Pts',(30.7436552900603,1.31725598082702,29.5216446454201));
#65840=CARTESIAN_POINT('Ctrl Pts',(31.0589827795059,1.08076551025951,29.4999042647726));
#65841=CARTESIAN_POINT('Ctrl Pts',(31.1927323157941,0.931082658468895,29.4893113802134));
#65842=CARTESIAN_POINT('Ctrl Pts',(31.3898152208091,0.595521362119493,29.470508077404));
#65843=CARTESIAN_POINT('Ctrl Pts',(31.454132752542,0.414466978649508,29.4605259432583));
#65844=CARTESIAN_POINT('Ctrl Pts',(31.5126702779257,0.0306540870738048,
29.4392030048374));
#65845=CARTESIAN_POINT('Ctrl Pts',(31.5035323460368,-0.168835937693657,
29.4281202256837));
#65846=CARTESIAN_POINT('Ctrl Pts',(31.4089367798935,-0.550558804938134,
29.4069133997257));
#65847=CARTESIAN_POINT('Ctrl Pts',(31.3252882833553,-0.729258932876967,
29.3976724363492));
#65848=CARTESIAN_POINT('Ctrl Pts',(31.095809753143,-1.04226364925314,29.3779370699617));
#65849=CARTESIAN_POINT('Ctrl Pts',(30.9530486497371,-1.17422022183269,29.3674030128222));
#65850=CARTESIAN_POINT('Ctrl Pts',(30.6189939852,-1.38091973480463,29.3455891471428));
#65851=CARTESIAN_POINT('Ctrl Pts',(30.429320489981,-1.45113472826307,29.3345130603643));
#65852=CARTESIAN_POINT('Ctrl Pts',(30.1547092959792,-1.49402062264703,29.3201095482887));
#65853=CARTESIAN_POINT('Ctrl Pts',(30.0773321028638,-1.50000000000001,29.3162206425338));
#65854=CARTESIAN_POINT('Ctrl Pts',(30.,-1.50000000000001,29.3125));
#65855=CARTESIAN_POINT('Origin',(30.,-1.32966554433622E-14,16.));
#65856=CARTESIAN_POINT('',(30.0000000000001,-1.50000000000001,28.75));
#65857=CARTESIAN_POINT('',(30.,-1.50000000000001,28.8125));
#65858=CARTESIAN_POINT('',(30.,-1.50000000000001,16.));
#65859=CARTESIAN_POINT('Ctrl Pts',(30.0000000000002,-1.50000000000001,28.75));
#65860=CARTESIAN_POINT('Ctrl Pts',(30.0540853804301,-1.50000000000001,28.7526021840792));
#65861=CARTESIAN_POINT('Ctrl Pts',(30.1082259230801,-1.49707499170992,28.7552882723823));
#65862=CARTESIAN_POINT('Ctrl Pts',(30.3599293953789,-1.46969892581938,28.7681588076143));
#65863=CARTESIAN_POINT('Ctrl Pts',(30.551406195325,-1.40907643365525,28.7790551975627));
#65864=CARTESIAN_POINT('Ctrl Pts',(30.8948389562126,-1.21930777033508,28.8008499657338));
#65865=CARTESIAN_POINT('Ctrl Pts',(31.0445316684251,-1.09380802186036,28.8115381638324));
#65866=CARTESIAN_POINT('Ctrl Pts',(31.2877030940359,-0.793168713090864,
28.8315888464123));
#65867=CARTESIAN_POINT('Ctrl Pts',(31.379006293082,-0.620999590881335,28.8405000227289));
#65868=CARTESIAN_POINT('Ctrl Pts',(31.4929834420294,-0.246010850263539,
28.861332730541));
#65869=CARTESIAN_POINT('Ctrl Pts',(31.5124077516471,-0.0462064671363202,
28.872432974048));
#65870=CARTESIAN_POINT('Ctrl Pts',(31.472996504913,0.34187077296362,28.8939928207202));
#65871=CARTESIAN_POINT('Ctrl Pts',(31.4174359900152,0.526774847879437,28.9042652693267));
#65872=CARTESIAN_POINT('Ctrl Pts',(31.2357811865968,0.873408443354475,28.9235226912975));
#65873=CARTESIAN_POINT('Ctrl Pts',(31.1084372252019,1.03024288184359,28.9336214802999));
#65874=CARTESIAN_POINT('Ctrl Pts',(30.8025714917792,1.28234443647017,28.9553402732223));
#65875=CARTESIAN_POINT('Ctrl Pts',(30.6280587815183,1.37625325113107,28.9663450980946));
#65876=CARTESIAN_POINT('Ctrl Pts',(30.2588396849677,1.48965870484553,28.9872593116519));
#65877=CARTESIAN_POINT('Ctrl Pts',(30.068359262301,1.51042753130005,28.996421409812));
#65878=CARTESIAN_POINT('Ctrl Pts',(29.6808324457,1.4790834395187,29.015936971685));
#65879=CARTESIAN_POINT('Ctrl Pts',(29.4877765738488,1.42378431516532,29.0267614634377));
#65880=CARTESIAN_POINT('Ctrl Pts',(29.1387883585853,1.24336756773843,29.0485637430906));
#65881=CARTESIAN_POINT('Ctrl Pts',(28.9853282851658,1.12165139698337,29.0593280990587));
#65882=CARTESIAN_POINT('Ctrl Pts',(28.7345675292747,0.827996981331758,29.0795498986531));
#65883=CARTESIAN_POINT('Ctrl Pts',(28.6390572969471,0.659343561113025,29.0883698021604));
#65884=CARTESIAN_POINT('Ctrl Pts',(28.5145121329283,0.288224890453508,29.108987506086));
#65885=CARTESIAN_POINT('Ctrl Pts',(28.4894007489509,0.0884674237606763,
29.1200851431244));
#65886=CARTESIAN_POINT('Ctrl Pts',(28.5181714945435,-0.301617414497863,
29.1417565230277));
#65887=CARTESIAN_POINT('Ctrl Pts',(28.5688407456957,-0.488459284239858,
29.1521366269022));
#65888=CARTESIAN_POINT('Ctrl Pts',(28.7405885892344,-0.838517734954907,
29.1715843186086));
#65889=CARTESIAN_POINT('Ctrl Pts',(28.8621896492638,-0.99731625641509,29.1812936366545));
#65890=CARTESIAN_POINT('Ctrl Pts',(29.1592029920166,-1.25770358504828,29.2028166791214));
#65891=CARTESIAN_POINT('Ctrl Pts',(29.3313514615525,-1.35708034159287,29.2138596416832));
#65892=CARTESIAN_POINT('Ctrl Pts',(29.6732716198879,-1.47316539526991,29.2335348677957));
#65893=CARTESIAN_POINT('Ctrl Pts',(29.836171069295,-1.50000000000001,29.2421177768964));
#65894=CARTESIAN_POINT('Ctrl Pts',(30.0000000000001,-1.50000000000001,29.25));
#65895=CARTESIAN_POINT('Ctrl Pts',(30.,-1.50000000000001,29.3125));
#65896=CARTESIAN_POINT('Ctrl Pts',(29.8873008443269,-1.50000000000001,29.3070777593446));
#65897=CARTESIAN_POINT('Ctrl Pts',(29.7747317592542,-1.48730209620256,29.3013090571639));
#65898=CARTESIAN_POINT('Ctrl Pts',(29.4744632015876,-1.41837586794508,29.2849477619958));
#65899=CARTESIAN_POINT('Ctrl Pts',(29.294837753903,-1.33817655775596,29.2740777699983));
#65900=CARTESIAN_POINT('Ctrl Pts',(28.9731315511867,-1.11133054751215,29.2522983950411));
#65901=CARTESIAN_POINT('Ctrl Pts',(28.8350302040853,-0.965600487241644,
29.241605933651));
#65902=CARTESIAN_POINT('Ctrl Pts',(28.6283822605559,-0.636211572057215,
29.2225138877439));
#65903=CARTESIAN_POINT('Ctrl Pts',(28.5588803689078,-0.457503373167084,
29.2129168540649));
#65904=CARTESIAN_POINT('Ctrl Pts',(28.4890373687744,-0.0765943370343735,
29.1917552409464));
#65905=CARTESIAN_POINT('Ctrl Pts',(28.4920613555339,0.122462822378066,29.1806965098678));
#65906=CARTESIAN_POINT('Ctrl Pts',(28.5749385187676,0.508021327520356,29.1592765929154));
#65907=CARTESIAN_POINT('Ctrl Pts',(28.6539760022703,0.690715131611738,29.1497407450183));
#65908=CARTESIAN_POINT('Ctrl Pts',(28.8753117279029,1.01093295253508,29.1301967854836));
#65909=CARTESIAN_POINT('Ctrl Pts',(29.0138845897616,1.14650161502305,29.1197638993787));
#65910=CARTESIAN_POINT('Ctrl Pts',(29.3408853293963,1.36213850199283,29.0980411554306));
#65911=CARTESIAN_POINT('Ctrl Pts',(29.5278326261113,1.43768005817386,29.0869482728631));
#65912=CARTESIAN_POINT('Ctrl Pts',(29.9124519842907,1.50965487695232,29.0664439648431));
#65913=CARTESIAN_POINT('Ctrl Pts',(30.1057978761999,1.50848592114141,29.0576455173396));
#65914=CARTESIAN_POINT('Ctrl Pts',(30.4842893221004,1.43290905070853,29.0373359816462));
#65915=CARTESIAN_POINT('Ctrl Pts',(30.6656448486515,1.3581864320247,29.02653488151));
#65916=CARTESIAN_POINT('Ctrl Pts',(30.9934995933557,1.14126552935963,29.0047353821212));
#65917=CARTESIAN_POINT('Ctrl Pts',(31.1358790692293,0.999664672511309,28.9939517892597));
#65918=CARTESIAN_POINT('Ctrl Pts',(31.3521306759684,0.67660748989115,28.974573568351));
#65919=CARTESIAN_POINT('Ctrl Pts',(31.426848104494,0.500181082019829,28.9652878378899));
#65920=CARTESIAN_POINT('Ctrl Pts',(31.5078778462889,0.122255781263764,28.9442919878479));
#65921=CARTESIAN_POINT('Ctrl Pts',(31.5109056485428,-0.0761896933508503,
28.9332672392582));
#65922=CARTESIAN_POINT('Ctrl Pts',(31.4398008862795,-0.46541654048851,28.9116435255283));
#65923=CARTESIAN_POINT('Ctrl Pts',(31.3653977766762,-0.65214948337147,28.9017441343992));
#65924=CARTESIAN_POINT('Ctrl Pts',(31.1521444486118,-0.979425287841449,
28.8823929843003));
#65925=CARTESIAN_POINT('Ctrl Pts',(31.0177656624447,-1.1184106596764,28.8720669771632));
#65926=CARTESIAN_POINT('Ctrl Pts',(30.6979072153004,-1.34258973369453,28.8504505839492));
#65927=CARTESIAN_POINT('Ctrl Pts',(30.5137720633169,-1.42326028628083,28.8393505286358));
#65928=CARTESIAN_POINT('Ctrl Pts',(30.2141280739392,-1.48853135114915,28.8231208153399));
#65929=CARTESIAN_POINT('Ctrl Pts',(30.107104215103,-1.50000000000001,28.8176530539518));
#65930=CARTESIAN_POINT('Ctrl Pts',(30.,-1.50000000000001,28.8125));
#65931=CARTESIAN_POINT('Origin',(30.,-1.32966554433622E-14,16.));
#65932=CARTESIAN_POINT('',(30.,-1.50000000000001,28.25));
#65933=CARTESIAN_POINT('',(29.9999999999999,-1.50000000000001,28.3125));
#65934=CARTESIAN_POINT('',(30.,-1.50000000000001,16.));
#65935=CARTESIAN_POINT('Ctrl Pts',(30.,-1.50000000000001,28.25));
#65936=CARTESIAN_POINT('Ctrl Pts',(30.0829658981124,-1.50000000000001,28.2539916986341));
#65937=CARTESIAN_POINT('Ctrl Pts',(30.1659646402018,-1.49311778203419,28.258176150196));
#65938=CARTESIAN_POINT('Ctrl Pts',(30.4454386189069,-1.44623695759697,28.272924593389));
#65939=CARTESIAN_POINT('Ctrl Pts',(30.6341065114148,-1.37401296366571,28.2840081036532));
#65940=CARTESIAN_POINT('Ctrl Pts',(30.9655430066945,-1.16393488515826,28.305789851648));
#65941=CARTESIAN_POINT('Ctrl Pts',(31.1067439460802,-1.03060853555517,28.3162868947229));
#65942=CARTESIAN_POINT('Ctrl Pts',(31.3331794991128,-0.714896180931114,
28.3359510679762));
#65943=CARTESIAN_POINT('Ctrl Pts',(31.4151109522262,-0.5347128589249,28.3452937300598));
#65944=CARTESIAN_POINT('Ctrl Pts',(31.5053441166005,-0.151540941191815,
28.3665810588227));
#65945=CARTESIAN_POINT('Ctrl Pts',(31.5121960357138,0.047808853319833,28.3776560474067));
#65946=CARTESIAN_POINT('Ctrl Pts',(31.4494295470438,0.430548940590616,28.3989193855884));
#65947=CARTESIAN_POINT('Ctrl Pts',(31.3831821322801,0.610720967506089,28.4087494232854));
#65948=CARTESIAN_POINT('Ctrl Pts',(31.1825379493516,0.943999251999173,28.4276606511623));
#65949=CARTESIAN_POINT('Ctrl Pts',(31.047158086339,1.09222920702457,28.4382916166091));
#65950=CARTESIAN_POINT('Ctrl Pts',(30.7294268326579,1.32515752881874,28.4600486998403));
#65951=CARTESIAN_POINT('Ctrl Pts',(30.550958922042,1.4087432384851,28.4709570664618));
#65952=CARTESIAN_POINT('Ctrl Pts',(30.1765920486677,1.5017020595339,28.4915509905286));
#65953=CARTESIAN_POINT('Ctrl Pts',(29.9846796160604,1.51197023290498,28.5004045958464));
#65954=CARTESIAN_POINT('Ctrl Pts',(29.5971747277955,1.45876321333926,28.5205264062414));
#65955=CARTESIAN_POINT('Ctrl Pts',(29.4058997547266,1.39186434368365,28.5315874296089));
#65956=CARTESIAN_POINT('Ctrl Pts',(29.0676327101079,1.19076140439435,28.5534485031393));
#65957=CARTESIAN_POINT('Ctrl Pts',(28.9223466869136,1.06108495094317,28.5640407038963));
#65958=CARTESIAN_POINT('Ctrl Pts',(28.6879155980949,0.752518131365587,28.5838910754598));
#65959=CARTESIAN_POINT('Ctrl Pts',(28.6014862328755,0.576207606788701,28.5929884662895));
#65960=CARTESIAN_POINT('Ctrl Pts',(28.499833643426,0.196881228217823,28.6140621539879));
#65961=CARTESIAN_POINT('Ctrl Pts',(28.4869739372834,-0.00278217893022192,
28.6251545654961));
#65962=CARTESIAN_POINT('Ctrl Pts',(28.5386011115484,-0.388179803466622,
28.646565544637));
#65963=CARTESIAN_POINT('Ctrl Pts',(28.5997438056181,-0.57068109411198,28.6567045052284));
#65964=CARTESIAN_POINT('Ctrl Pts',(28.7910752661536,-0.909939730661663,
28.6755522072589));
#65965=CARTESIAN_POINT('Ctrl Pts',(28.9221594106395,-1.06198129449833,28.6859751842018));
#65966=CARTESIAN_POINT('Ctrl Pts',(29.2336502066539,-1.30423330232361,28.7076910145522));
#65967=CARTESIAN_POINT('Ctrl Pts',(29.4102115046891,-1.39300789458955,28.7186517848609));
#65968=CARTESIAN_POINT('Ctrl Pts',(29.7297304238973,-1.48169043732429,28.7364880499937));
#65969=CARTESIAN_POINT('Ctrl Pts',(29.8646679236608,-1.50000000000001,28.7434888324413));
#65970=CARTESIAN_POINT('Ctrl Pts',(30.0000000000002,-1.50000000000001,28.75));
#65971=CARTESIAN_POINT('Ctrl Pts',(30.,-1.50000000000001,28.8125));
#65972=CARTESIAN_POINT('Ctrl Pts',(29.915383015882,-1.50000000000001,28.8084288634535));
#65973=CARTESIAN_POINT('Ctrl Pts',(29.8307352254749,-1.4928411598692,28.8041573880682));
#65974=CARTESIAN_POINT('Ctrl Pts',(29.5559284168413,-1.44580747389306,28.7896292480462));
#65975=CARTESIAN_POINT('Ctrl Pts',(29.3730572440495,-1.37640415455312,28.7789029846613));
#65976=CARTESIAN_POINT('Ctrl Pts',(29.0395563050654,-1.16922544646275,28.7571024491396));
#65977=CARTESIAN_POINT('Ctrl Pts',(28.8931654598463,-1.03173520870096,28.7462400430439));
#65978=CARTESIAN_POINT('Ctrl Pts',(28.6676984257239,-0.714888535897263,
28.7265909588401));
#65979=CARTESIAN_POINT('Ctrl Pts',(28.5879546245725,-0.540586509645268,
28.7175325838691));
#65980=CARTESIAN_POINT('Ctrl Pts',(28.4963360655409,-0.165582907317607,
28.6966990504065));
#65981=CARTESIAN_POINT('Ctrl Pts',(28.4875887561367,0.032114568158461,28.6857158573245));
#65982=CARTESIAN_POINT('Ctrl Pts',(28.5470557852483,0.422500942588754,28.6640277254117));
#65983=CARTESIAN_POINT('Ctrl Pts',(28.6157998677826,0.611145026803925,28.6537877758344));
#65984=CARTESIAN_POINT('Ctrl Pts',(28.8187186237447,0.943964110383672,28.6347798680923));
#65985=CARTESIAN_POINT('Ctrl Pts',(28.9483973542157,1.08655537048085,28.6245798289275));
#65986=CARTESIAN_POINT('Ctrl Pts',(29.2601643471919,1.31985362966521,28.6030994252846));
#65987=CARTESIAN_POINT('Ctrl Pts',(29.4410566887989,1.40604402433623,28.5920020608114));
#65988=CARTESIAN_POINT('Ctrl Pts',(29.8214920682634,1.50190823479761,28.5710354603478));
#65989=CARTESIAN_POINT('Ctrl Pts',(30.0168727428654,1.5123834847247,28.5620321954671));
#65990=CARTESIAN_POINT('Ctrl Pts',(30.4002098002625,1.45848214178997,28.5420916231679));
#65991=CARTESIAN_POINT('Ctrl Pts',(30.5845472296663,1.39485738401663,28.531455330078));
#65992=CARTESIAN_POINT('Ctrl Pts',(30.9255768985555,1.19735876148644,28.5095614596354));
#65993=CARTESIAN_POINT('Ctrl Pts',(31.0774615143075,1.06275841541511,28.4985150091509));
#65994=CARTESIAN_POINT('Ctrl Pts',(31.3127681711381,0.750226996476014,28.4785123840417));
#65995=CARTESIAN_POINT('Ctrl Pts',(31.3972426471779,0.57785906771898,28.4696032815399));
#65996=CARTESIAN_POINT('Ctrl Pts',(31.4986444188222,0.205636520695856,28.4489242511497));
#65997=CARTESIAN_POINT('Ctrl Pts',(31.5126593744967,0.00877624847217685,
28.4379875693595));
#65998=CARTESIAN_POINT('Ctrl Pts',(31.4639817400215,-0.38243148199871,28.4162538065556));
#65999=CARTESIAN_POINT('Ctrl Pts',(31.4004868863224,-0.572852347631721,
28.405674869576));
#66000=CARTESIAN_POINT('Ctrl Pts',(31.2070793636249,-0.910612756316215,
28.3869104024268));
#66001=CARTESIAN_POINT('Ctrl Pts',(31.0818178721223,-1.05640050494828,28.3768711948362));
#66002=CARTESIAN_POINT('Ctrl Pts',(30.7776023551779,-1.29787423387296,28.3555270153716));
#66003=CARTESIAN_POINT('Ctrl Pts',(30.5998203088742,-1.38901510440857,28.3444417818325));
#66004=CARTESIAN_POINT('Ctrl Pts',(30.2759956104928,-1.48090471471267,28.3263092695923));
#66005=CARTESIAN_POINT('Ctrl Pts',(30.1382050521625,-1.50000000000003,28.3191493936725));
#66006=CARTESIAN_POINT('Ctrl Pts',(29.9999999999998,-1.50000000000001,28.3125));
#66007=CARTESIAN_POINT('Origin',(30.,-1.32966554433622E-14,16.));
#66008=CARTESIAN_POINT('',(30.,-1.50000000000001,27.75));
#66009=CARTESIAN_POINT('',(29.9999999999999,-1.50000000000001,27.8125));
#66010=CARTESIAN_POINT('',(30.,-1.50000000000001,16.));
#66011=CARTESIAN_POINT('Ctrl Pts',(30.,-1.50000000000001,27.75));
#66012=CARTESIAN_POINT('Ctrl Pts',(30.1124415068704,-1.50000000000002,27.7554098445216));
#66013=CARTESIAN_POINT('Ctrl Pts',(30.2247618661566,-1.48736003703784,27.7611649704098));
#66014=CARTESIAN_POINT('Ctrl Pts',(30.5287085515254,-1.41774990238772,27.7777222269793));
#66015=CARTESIAN_POINT('Ctrl Pts',(30.7117935692984,-1.3352484713228,27.7888226154224));
#66016=CARTESIAN_POINT('Ctrl Pts',(31.0290158327245,-1.10803593258209,27.810396438097));
#66017=CARTESIAN_POINT('Ctrl Pts',(31.1618575965723,-0.967846133863366,
27.8206819515156));
#66018=CARTESIAN_POINT('Ctrl Pts',(31.3721629460689,-0.6380210664967,27.8399620797878));
#66019=CARTESIAN_POINT('Ctrl Pts',(31.4448593309443,-0.449797513993593,
27.8500112492227));
#66020=CARTESIAN_POINT('Ctrl Pts',(31.5116357099559,-0.0592694964018678,
27.8717072502));
#66021=CARTESIAN_POINT('Ctrl Pts',(31.5064070816201,0.138907825669745,27.8827171014262));
#66022=CARTESIAN_POINT('Ctrl Pts',(31.4213057895144,0.515720730899333,27.9036511517167));
#66023=CARTESIAN_POINT('Ctrl Pts',(31.3446665574137,0.691326301909506,27.9128415418121));
#66024=CARTESIAN_POINT('Ctrl Pts',(31.1248857141117,1.01202109760975,27.9323239413351));
#66025=CARTESIAN_POINT('Ctrl Pts',(30.9809587395189,1.15206471718701,27.9431387316727));
#66026=CARTESIAN_POINT('Ctrl Pts',(30.6509116511972,1.36527940308072,27.964940759777));
#66027=CARTESIAN_POINT('Ctrl Pts',(30.4689587309927,1.43797198007731,27.9757142119819));
#66028=CARTESIAN_POINT('Ctrl Pts',(30.0895559298121,1.50958056680736,27.9959573651739));
#66029=CARTESIAN_POINT('Ctrl Pts',(29.8958570870542,1.50864454830606,28.0047704518936));
#66030=CARTESIAN_POINT('Ctrl Pts',(29.5119529197823,1.43233602869983,28.0253607308535));
#66031=CARTESIAN_POINT('Ctrl Pts',(29.326059536573,1.35483178794297,28.0364574259998));
#66032=CARTESIAN_POINT('Ctrl Pts',(29.0017503691465,1.13591853977073,28.058141681653));
#66033=CARTESIAN_POINT('Ctrl Pts',(28.8647633102306,0.999035130825837,28.0685347915132));
#66034=CARTESIAN_POINT('Ctrl Pts',(28.6464909172802,0.676130375169667,28.0880060034614));
#66035=CARTESIAN_POINT('Ctrl Pts',(28.5692025798653,0.491914163630282,28.097671435354));
#66036=CARTESIAN_POINT('Ctrl Pts',(28.4907708909632,0.10494838810591,28.1191695339942));
#66037=CARTESIAN_POINT('Ctrl Pts',(28.4900432259905,-0.0938982867387415,
28.1302165714856));
#66038=CARTESIAN_POINT('Ctrl Pts',(28.5641302538219,-0.473688030944453,
28.1513160017192));
#66039=CARTESIAN_POINT('Ctrl Pts',(28.6356001259049,-0.65152593371875,28.1607865563875));
#66040=CARTESIAN_POINT('Ctrl Pts',(28.845875335272,-0.978539657712538,28.1799871416705));
#66041=CARTESIAN_POINT('Ctrl Pts',(28.9856037255401,-1.12272886979256,28.1907150828729));
#66042=CARTESIAN_POINT('Ctrl Pts',(29.3096631032409,-1.34585412683097,28.2125043207586));
#66043=CARTESIAN_POINT('Ctrl Pts',(29.4899597666947,-1.42399330666579,28.2233493807965));
#66044=CARTESIAN_POINT('Ctrl Pts',(29.7854687062271,-1.48848755634025,28.2393585682142));
#66045=CARTESIAN_POINT('Ctrl Pts',(29.8926913234913,-1.50000000000001,28.2448371088943));
#66046=CARTESIAN_POINT('Ctrl Pts',(30.,-1.50000000000001,28.25));
#66047=CARTESIAN_POINT('Ctrl Pts',(29.9999999999998,-1.50000000000001,28.3125));
#66048=CARTESIAN_POINT('Ctrl Pts',(29.9436942937174,-1.50000000000001,28.3097909904434));
#66049=CARTESIAN_POINT('Ctrl Pts',(29.8873283119117,-1.49682992210333,28.3069910231599));
#66050=CARTESIAN_POINT('Ctrl Pts',(29.6396724584349,-1.46877643215582,28.2942964117443));
#66051=CARTESIAN_POINT('Ctrl Pts',(29.4541661443778,-1.41038581308707,28.2837492734071));
#66052=CARTESIAN_POINT('Ctrl Pts',(29.1087260311914,-1.22301113475657,28.2619244260365));
#66053=CARTESIAN_POINT('Ctrl Pts',(28.9535330490943,-1.09318251992373,28.250851349792));
#66054=CARTESIAN_POINT('Ctrl Pts',(28.7092889328235,-0.787692454984111,
28.2306143141317));
#66055=CARTESIAN_POINT('Ctrl Pts',(28.6196840987504,-0.61735395437333,28.2217974419096));
#66056=CARTESIAN_POINT('Ctrl Pts',(28.5078809954767,-0.248171981043882,
28.2012873322802));
#66057=CARTESIAN_POINT('Ctrl Pts',(28.4882926923279,-0.0523550997824531,
28.1904086166545));
#66058=CARTESIAN_POINT('Ctrl Pts',(28.5254878247544,0.339597077669009,28.168633495685));
#66059=CARTESIAN_POINT('Ctrl Pts',(28.5834194437059,0.531823926835376,28.1579542262869));
#66060=CARTESIAN_POINT('Ctrl Pts',(28.7667554264755,0.874769226053054,28.1389017096637));
#66061=CARTESIAN_POINT('Ctrl Pts',(28.8874031082008,1.02385470321529,28.129256101159));
#66062=CARTESIAN_POINT('Ctrl Pts',(29.1834814070674,1.27365788399194,28.1080720501192));
#66063=CARTESIAN_POINT('Ctrl Pts',(29.3578610118793,1.36987818467188,28.0970094213409));
#66064=CARTESIAN_POINT('Ctrl Pts',(29.7335617480327,1.48922788034193,28.0756182419206));
#66065=CARTESIAN_POINT('Ctrl Pts',(29.9311376367095,1.51130087803589,28.0661270552772));
#66066=CARTESIAN_POINT('Ctrl Pts',(30.3188296259211,1.47827076732948,28.0465567126743));
#66067=CARTESIAN_POINT('Ctrl Pts',(30.5053902810264,1.4253063260919,28.0361095744917));
#66068=CARTESIAN_POINT('Ctrl Pts',(30.8550820522802,1.24848731142734,28.0143733820065));
#66069=CARTESIAN_POINT('Ctrl Pts',(31.0135429189334,1.12366789185429,28.0032822239058));
#66070=CARTESIAN_POINT('Ctrl Pts',(31.2669421658592,0.825551327222966,27.9828095312695));
#66071=CARTESIAN_POINT('Ctrl Pts',(31.3618736710286,0.657250577679458,27.9740139209821));
#66072=CARTESIAN_POINT('Ctrl Pts',(31.4842407851538,0.291243414392501,27.9536801896884));
#66073=CARTESIAN_POINT('Ctrl Pts',(31.509450941646,0.0966465287303217,27.9428692515961));
#66074=CARTESIAN_POINT('Ctrl Pts',(31.4839402912682,-0.295715862316101,
27.9210713409824));
#66075=CARTESIAN_POINT('Ctrl Pts',(31.4317236332783,-0.489608696036187,
27.9102995168868));
#66076=CARTESIAN_POINT('Ctrl Pts',(31.2586786377253,-0.837725609348495,
27.8909596883695));
#66077=CARTESIAN_POINT('Ctrl Pts',(31.1426320784322,-0.99018742000189,27.8816363720611));
#66078=CARTESIAN_POINT('Ctrl Pts',(30.8547518896528,-1.24822771259633,27.8606179441152));
#66079=CARTESIAN_POINT('Ctrl Pts',(30.683921012954,-1.3494162779034,27.8495880462471));
#66080=CARTESIAN_POINT('Ctrl Pts',(30.3380948295812,-1.47125624803439,27.8295650326271));
#66081=CARTESIAN_POINT('Ctrl Pts',(30.1695563642114,-1.50000000000003,27.8206577843767));
#66082=CARTESIAN_POINT('Ctrl Pts',(29.9999999999999,-1.50000000000001,27.8125));
#66083=CARTESIAN_POINT('Origin',(30.,-1.32966554433622E-14,16.));
#66084=CARTESIAN_POINT('',(29.9999999999999,-1.50000000000001,27.25));
#66085=CARTESIAN_POINT('',(30.0000000001561,-1.50000000000001,27.312500000015));
#66086=CARTESIAN_POINT('',(30.,-1.50000000000001,16.));
#66087=CARTESIAN_POINT('Ctrl Pts',(29.9999999999998,-1.50000000000001,27.25));
#66088=CARTESIAN_POINT('Ctrl Pts',(30.1442714687728,-1.50000000000004,27.2569412642777));
#66089=CARTESIAN_POINT('Ctrl Pts',(30.2880340149987,-1.4791914741294,27.2644360576155));
#66090=CARTESIAN_POINT('Ctrl Pts',(30.6163114314673,-1.38174334274362,27.2829372047179));
#66091=CARTESIAN_POINT('Ctrl Pts',(30.7927900386128,-1.28861749288707,27.2940148648257));
#66092=CARTESIAN_POINT('Ctrl Pts',(31.0938533402203,-1.04389816914467,27.3152975386708));
#66093=CARTESIAN_POINT('Ctrl Pts',(31.2173213404585,-0.896838599044721,
27.3251756333865));
#66094=CARTESIAN_POINT('Ctrl Pts',(31.4068435879888,-0.557063752560209,
27.3440520137467));
#66095=CARTESIAN_POINT('Ctrl Pts',(31.4681965573585,-0.365925712559008,
27.3546707937468));
#66096=CARTESIAN_POINT('Ctrl Pts',(31.5124404667227,0.0256096349450533,
27.376422757497));
#66097=CARTESIAN_POINT('Ctrl Pts',(31.4962677243898,0.222085336897189,27.3873380742721));
#66098=CARTESIAN_POINT('Ctrl Pts',(31.3908461160845,0.593142920619804,27.4079523844789));
#66099=CARTESIAN_POINT('Ctrl Pts',(31.304401721973,0.764723471695272,27.4168175948822));
#66100=CARTESIAN_POINT('Ctrl Pts',(31.0656503667188,1.07455866625052,27.4369110579998));
#66101=CARTESIAN_POINT('Ctrl Pts',(30.9124772117446,1.20733392111332,27.4479688063785));
#66102=CARTESIAN_POINT('Ctrl Pts',(30.5697179509117,1.40095220523075,27.4698381046742));
#66103=CARTESIAN_POINT('Ctrl Pts',(30.3849139570494,1.46256729268532,27.4804410211816));
#66104=CARTESIAN_POINT('Ctrl Pts',(30.0007344874447,1.51254230178002,27.5003130592281));
#66105=CARTESIAN_POINT('Ctrl Pts',(29.8049569216954,1.49991645600797,27.5093863351468));
#66106=CARTESIAN_POINT('Ctrl Pts',(29.4253565109394,1.3996692288739,27.5304345136228));
#66107=CARTESIAN_POINT('Ctrl Pts',(29.245638701995,1.31157237616612,27.5415283255346));
#66108=CARTESIAN_POINT('Ctrl Pts',(28.9367683949736,1.07514318986943,27.562956332507));
#66109=CARTESIAN_POINT('Ctrl Pts',(28.8087599369318,0.93132448347984,27.5731101063824));
#66110=CARTESIAN_POINT('Ctrl Pts',(28.6094708234815,0.596592375009914,27.591996522448));
#66111=CARTESIAN_POINT('Ctrl Pts',(28.5427132787644,0.407261741609369,27.6023743476884));
#66112=CARTESIAN_POINT('Ctrl Pts',(28.4873635075659,0.0164898797776363,
27.624083895568));
#66113=CARTESIAN_POINT('Ctrl Pts',(28.4981279946982,-0.180903932406258,
27.6350502184671));
#66114=CARTESIAN_POINT('Ctrl Pts',(28.5934885065557,-0.554852956622451,
27.6558251642568));
#66115=CARTESIAN_POINT('Ctrl Pts',(28.6750314181996,-0.72841210507679,27.6648194223046));
#66116=CARTESIAN_POINT('Ctrl Pts',(28.9037835277885,-1.04301134033857,27.6845641309549));
#66117=CARTESIAN_POINT('Ctrl Pts',(29.0515807305306,-1.17900166318454,27.6954525361552));
#66118=CARTESIAN_POINT('Ctrl Pts',(29.3870321030576,-1.38265756586298,27.7172490562487));
#66119=CARTESIAN_POINT('Ctrl Pts',(29.570408592882,-1.45015060314336,27.7279465683201));
#66120=CARTESIAN_POINT('Ctrl Pts',(29.8405845073873,-1.49365112485936,27.7421537608929));
#66121=CARTESIAN_POINT('Ctrl Pts',(29.920314098353,-1.50000000000001,27.7461661102695));
#66122=CARTESIAN_POINT('Ctrl Pts',(30.,-1.50000000000001,27.75));
#66123=CARTESIAN_POINT('Ctrl Pts',(29.9999999999999,-1.50000000000001,27.8125));
#66124=CARTESIAN_POINT('Ctrl Pts',(29.9712572824709,-1.50000000000001,27.8111171153581));
#66125=CARTESIAN_POINT('Ctrl Pts',(29.9424874969812,-1.49917387170699,27.8097099804002));
#66126=CARTESIAN_POINT('Ctrl Pts',(29.7223735770152,-1.48649276547853,27.7987674915373));
#66127=CARTESIAN_POINT('Ctrl Pts',(29.5349257292356,-1.43889608772887,27.7884267728186));
#66128=CARTESIAN_POINT('Ctrl Pts',(29.1813453265204,-1.27257887490163,27.7667952051828));
#66129=CARTESIAN_POINT('Ctrl Pts',(29.0198117779222,-1.15277654761383,27.7556955762776));
#66130=CARTESIAN_POINT('Ctrl Pts',(28.7574522908629,-0.862041024530384,
27.7349968128188));
#66131=CARTESIAN_POINT('Ctrl Pts',(28.6572312223829,-0.695708343276581,
27.7261504635153));
#66132=CARTESIAN_POINT('Ctrl Pts',(28.524605736016,-0.332863036208749,27.7059923909005));
#66133=CARTESIAN_POINT('Ctrl Pts',(28.4939840388333,-0.139603136099824,
27.6952557297833));
#66134=CARTESIAN_POINT('Ctrl Pts',(28.508148989394,0.25282273238934,27.673454292645));
#66135=CARTESIAN_POINT('Ctrl Pts',(28.5547646373704,0.44816718663467,27.6626018229647));
#66136=CARTESIAN_POINT('Ctrl Pts',(28.7177569938957,0.801209312950165,27.6429883715028));
#66137=CARTESIAN_POINT('Ctrl Pts',(28.8294090431484,0.956981758536969,27.6339039237114));
#66138=CARTESIAN_POINT('Ctrl Pts',(29.1093968787388,1.22281551664853,27.6130487316321));
#66139=CARTESIAN_POINT('Ctrl Pts',(29.2767036270498,1.32864238149993,27.6020595468161));
#66140=CARTESIAN_POINT('Ctrl Pts',(29.6469534397504,1.47162694755714,27.5802741008953));
#66141=CARTESIAN_POINT('Ctrl Pts',(29.8468632228895,1.50560128622732,27.570023387908));
#66142=CARTESIAN_POINT('Ctrl Pts',(30.2385607914922,1.49319741260661,27.5508332778069));
#66143=CARTESIAN_POINT('Ctrl Pts',(30.4267058309758,1.45067195878526,27.540599882768));
#66144=CARTESIAN_POINT('Ctrl Pts',(30.7836729511717,1.29433057010809,27.5190824778378));
#66145=CARTESIAN_POINT('Ctrl Pts',(30.9479647504538,1.17932417828325,27.5079833629642));
#66146=CARTESIAN_POINT('Ctrl Pts',(31.2187102492265,0.89565657574078,27.4870774584548));
#66147=CARTESIAN_POINT('Ctrl Pts',(31.3239608540741,0.731149127851972,27.4781193959917));
#66148=CARTESIAN_POINT('Ctrl Pts',(31.4661242989034,0.37131396030254,27.4581285533501));
#66149=CARTESIAN_POINT('Ctrl Pts',(31.5017272578984,0.179429293592902,27.4474682940885));
#66150=CARTESIAN_POINT('Ctrl Pts',(31.4980926781097,-0.21275991516766,27.4256800047129));
#66151=CARTESIAN_POINT('Ctrl Pts',(31.4567210643059,-0.409304691427262,
27.4147608504762));
#66152=CARTESIAN_POINT('Ctrl Pts',(31.3031284414201,-0.766835781066652,
27.394898012163));
#66153=CARTESIAN_POINT('Ctrl Pts',(31.1955054411838,-0.925718941221814,
27.3859710339898));
#66154=CARTESIAN_POINT('Ctrl Pts',(30.9227930606553,-1.19862566676885,27.3652694110877));
#66155=CARTESIAN_POINT('Ctrl Pts',(30.75882230211,-1.30859982122977,27.354325526665));
#66156=CARTESIAN_POINT('Ctrl Pts',(30.3950972752779,-1.46060207029247,27.3326035134561));
#66157=CARTESIAN_POINT('Ctrl Pts',(30.198484714314,-1.4999999999587,27.3220496002711));
#66158=CARTESIAN_POINT('Ctrl Pts',(30.0000000003122,-1.50000000000001,27.312500000015));
#66159=CARTESIAN_POINT('Origin',(30.,-1.32966554433622E-14,16.));
#66160=CARTESIAN_POINT('',(30.,-1.50000000000001,26.75));
#66161=CARTESIAN_POINT('',(30.0000000000001,-1.50000000000001,26.8125));
#66162=CARTESIAN_POINT('',(30.,-1.50000000000001,16.));
#66163=CARTESIAN_POINT('Ctrl Pts',(29.9999999999999,-1.50000000000002,26.75));
#66164=CARTESIAN_POINT('Ctrl Pts',(30.1755630845093,-1.50000000000003,26.7584467828418));
#66165=CARTESIAN_POINT('Ctrl Pts',(30.3499584064833,-1.46918259215549,26.7676934207892));
#66166=CARTESIAN_POINT('Ctrl Pts',(30.6997034276012,-1.3412672085792,26.7880737410627));
#66167=CARTESIAN_POINT('Ctrl Pts',(30.8691431470038,-1.23821435243508,26.7990884927007));
#66168=CARTESIAN_POINT('Ctrl Pts',(31.1538803669515,-0.977054933639417,
26.8200423468827));
#66169=CARTESIAN_POINT('Ctrl Pts',(31.2681733329846,-0.823282264050392,
26.8292620964417));
#66170=CARTESIAN_POINT('Ctrl Pts',(31.4372326110993,-0.473197410553428,
26.8487112549693));
#66171=CARTESIAN_POINT('Ctrl Pts',(31.4872301101415,-0.278708237309613,
26.8595162090384));
#66172=CARTESIAN_POINT('Ctrl Pts',(31.5082331683214,0.113718878171538,26.881317715454));
#66173=CARTESIAN_POINT('Ctrl Pts',(31.4808674747884,0.307802550913579,26.8921001417175));
#66174=CARTESIAN_POINT('Ctrl Pts',(31.3544261384598,0.67256246632588,26.9123645814626));
#66175=CARTESIAN_POINT('Ctrl Pts',(31.2574072539999,0.840081862517357,26.9211719059107));
#66176=CARTESIAN_POINT('Ctrl Pts',(31.0004574791989,1.1352928844589,26.9417347138799));
#66177=CARTESIAN_POINT('Ctrl Pts',(30.8407636896231,1.25813738072432,26.9528303320317));
#66178=CARTESIAN_POINT('Ctrl Pts',(30.4894980147219,1.43081423936239,26.9745271891017));
#66179=CARTESIAN_POINT('Ctrl Pts',(30.302568408204,1.48165789304525,26.984933167702));
#66180=CARTESIAN_POINT('Ctrl Pts',(29.9140424353861,1.51051713966446,27.0044277780243));
#66181=CARTESIAN_POINT('Ctrl Pts',(29.7160053760103,1.48607476032932,27.0140505099305));
#66182=CARTESIAN_POINT('Ctrl Pts',(29.3413420123945,1.36197834203437,27.0355236321475));
#66183=CARTESIAN_POINT('Ctrl Pts',(29.1683424827117,1.26378814603618,27.0465745813446));
#66184=CARTESIAN_POINT('Ctrl Pts',(28.87548492057,1.01073104588063,27.0676940612658));
#66185=CARTESIAN_POINT('Ctrl Pts',(28.7566499301147,0.860326156686485,27.0772041024063));
#66186=CARTESIAN_POINT('Ctrl Pts',(28.5773390955292,0.515342682333064,27.0963698509815));
#66187=CARTESIAN_POINT('Ctrl Pts',(28.5216397715234,0.322442560698391,27.1070865244057));
#66188=CARTESIAN_POINT('Ctrl Pts',(28.4890218615652,-0.0697120082430973,
27.1288728893469));
#66189=CARTESIAN_POINT('Ctrl Pts',(28.510818362855,-0.265069960572926,27.1397261089208));
#66190=CARTESIAN_POINT('Ctrl Pts',(28.6267610927498,-0.633018179794785,
27.1601676766553));
#66191=CARTESIAN_POINT('Ctrl Pts',(28.7184387624141,-0.802555681667626,
27.1689674029211));
#66192=CARTESIAN_POINT('Ctrl Pts',(28.9662614123549,-1.10518359683465,27.1892971067025));
#66193=CARTESIAN_POINT('Ctrl Pts',(29.1227466839353,-1.23306866661795,27.2003783708913));
#66194=CARTESIAN_POINT('Ctrl Pts',(29.4698813680168,-1.416339226716,27.2221707450579));
#66195=CARTESIAN_POINT('Ctrl Pts',(29.6558172836666,-1.47261637710131,27.232679845148));
#66196=CARTESIAN_POINT('Ctrl Pts',(29.8981460836565,-1.49740948534734,27.2450275924248));
#66197=CARTESIAN_POINT('Ctrl Pts',(29.9491012405249,-1.5,27.247551132293));
#66198=CARTESIAN_POINT('Ctrl Pts',(29.9999999999998,-1.50000000000001,27.25));
#66199=CARTESIAN_POINT('Ctrl Pts',(30.0000000003122,-1.50000000000001,27.312500000015));
#66200=CARTESIAN_POINT('Ctrl Pts',(29.9998020603292,-1.50000000000005,27.3124904766232));
#66201=CARTESIAN_POINT('Ctrl Pts',(29.9996041185888,-1.49999996081992,27.3124809520584));
#66202=CARTESIAN_POINT('Ctrl Pts',(29.8088160951652,-1.49992443102837,27.3032995609518));
#66203=CARTESIAN_POINT('Ctrl Pts',(29.6200100906951,-1.46352575850992,27.2932045535897));
#66204=CARTESIAN_POINT('Ctrl Pts',(29.2593205849108,-1.31930644298838,27.2718447795537));
#66205=CARTESIAN_POINT('Ctrl Pts',(29.0918823606668,-1.21016636340677,27.2607572353565));
#66206=CARTESIAN_POINT('Ctrl Pts',(28.8110979291704,-0.935181294724627,
27.2396095139674));
#66207=CARTESIAN_POINT('Ctrl Pts',(28.6997118002275,-0.772848068745042,
27.2304360038192));
#66208=CARTESIAN_POINT('Ctrl Pts',(28.5461974612702,-0.416685157506792,
27.210649175417));
#66209=CARTESIAN_POINT('Ctrl Pts',(28.5047394765833,-0.226599155889903,
27.2000888419939));
#66210=CARTESIAN_POINT('Ctrl Pts',(28.4958539389935,0.166443777601294,27.1782531234666));
#66211=CARTESIAN_POINT('Ctrl Pts',(28.5315184967694,0.365700597221805,27.1671833001544));
#66212=CARTESIAN_POINT('Ctrl Pts',(28.6754701753172,0.729371435414476,27.1469793646992));
#66213=CARTESIAN_POINT('Ctrl Pts',(28.7788000491734,0.891648198610453,27.1381536711784));
#66214=CARTESIAN_POINT('Ctrl Pts',(29.0437345128306,1.17200464814443,27.1176193266989));
#66215=CARTESIAN_POINT('Ctrl Pts',(29.2040531543845,1.2862733419873,27.1067318620762));
#66216=CARTESIAN_POINT('Ctrl Pts',(29.5628324377282,1.44858368838945,27.0849614650246));
#66217=CARTESIAN_POINT('Ctrl Pts',(29.7584548095726,1.49371725552991,27.0742958690726));
#66218=CARTESIAN_POINT('Ctrl Pts',(30.1472060622831,1.50481186242553,27.055283882181));
#66219=CARTESIAN_POINT('Ctrl Pts',(30.3365600149074,1.47407427722924,27.045587089767));
#66220=CARTESIAN_POINT('Ctrl Pts',(30.7004989886168,1.34098519143669,27.0243801486806));
#66221=CARTESIAN_POINT('Ctrl Pts',(30.8706482413977,1.23730103012925,27.0133137233474));
#66222=CARTESIAN_POINT('Ctrl Pts',(31.1605713571455,0.970446090199086,26.991952153717));
#66223=CARTESIAN_POINT('Ctrl Pts',(31.2776619344983,0.810096307036669,26.9825053503909));
#66224=CARTESIAN_POINT('Ctrl Pts',(31.4414580755822,0.457344311316898,26.9629080172954));
#66225=CARTESIAN_POINT('Ctrl Pts',(31.4881418689773,0.269035150966863,26.9524463972759));
#66226=CARTESIAN_POINT('Ctrl Pts',(31.508284818313,-0.122458793694974,26.9306967336836));
#66227=CARTESIAN_POINT('Ctrl Pts',(31.478582774639,-0.322064434897177,26.9196075313946));
#66228=CARTESIAN_POINT('Ctrl Pts',(31.3455674834561,-0.689986184900448,
26.8991674341722));
#66229=CARTESIAN_POINT('Ctrl Pts',(31.246662212612,-0.855842984261559,26.8903733141072));
#66230=CARTESIAN_POINT('Ctrl Pts',(30.9897531567272,-1.14377092738595,26.8700147729728));
#66231=CARTESIAN_POINT('Ctrl Pts',(30.8332877383797,-1.26231706455743,26.8591938787678));
#66232=CARTESIAN_POINT('Ctrl Pts',(30.4799553603842,-1.43498001100993,26.8373979738484));
#66233=CARTESIAN_POINT('Ctrl Pts',(30.2857235516143,-1.48590367409306,26.8266384453951));
#66234=CARTESIAN_POINT('Ctrl Pts',(30.0581276265954,-1.49915605873645,26.8153201095514));
#66235=CARTESIAN_POINT('Ctrl Pts',(30.0290509426437,-1.50000000000001,26.8138977141296));
#66236=CARTESIAN_POINT('Ctrl Pts',(30.0000000000001,-1.50000000000001,26.8125));
#66237=CARTESIAN_POINT('Origin',(30.,-1.32966554433622E-14,16.));
#66238=CARTESIAN_POINT('',(30.,-1.50000000000001,26.25));
#66239=CARTESIAN_POINT('',(30.0000000000001,-1.50000000000001,26.3125));
#66240=CARTESIAN_POINT('',(30.,-1.50000000000001,16.));
#66241=CARTESIAN_POINT('Ctrl Pts',(30.,-1.50000000000001,26.25));
#66242=CARTESIAN_POINT('Ctrl Pts',(30.0056194401817,-1.50000000000001,26.2502703654418));
#66243=CARTESIAN_POINT('Ctrl Pts',(30.0112401600052,-1.49996842190559,26.2505416696197));
#66244=CARTESIAN_POINT('Ctrl Pts',(30.2156637559459,-1.49767029707552,26.2604408412659));
#66245=CARTESIAN_POINT('Ctrl Pts',(30.4120156853044,-1.45593401100177,26.2710471691517));
#66246=CARTESIAN_POINT('Ctrl Pts',(30.7738333695248,-1.29974623576057,26.2927936799124));
#66247=CARTESIAN_POINT('Ctrl Pts',(30.9363483004055,-1.18803068750778,26.3037158928437));
#66248=CARTESIAN_POINT('Ctrl Pts',(31.2059383925193,-0.91211987124096,26.3243507415389));
#66249=CARTESIAN_POINT('Ctrl Pts',(31.3118367658411,-0.751883140819906,
26.3332287143989));
#66250=CARTESIAN_POINT('Ctrl Pts',(31.4620725484111,-0.390717177178761,
26.3532934901568));
#66251=CARTESIAN_POINT('Ctrl Pts',(31.5011777050095,-0.191739563198423,
26.3643478020445));
#66252=CARTESIAN_POINT('Ctrl Pts',(31.4988144256802,0.202052743889533,26.3862251524383));
#66253=CARTESIAN_POINT('Ctrl Pts',(31.4603972352794,0.393097806012914,26.3968387670007));
#66254=CARTESIAN_POINT('Ctrl Pts',(31.3127984325509,0.751186708707084,26.4167325949282));
#66255=CARTESIAN_POINT('Ctrl Pts',(31.2046306350456,0.914654115967526,26.4257825736587));
#66256=CARTESIAN_POINT('Ctrl Pts',(30.929085340333,1.1942016269637,26.4468049614706));
#66257=CARTESIAN_POINT('Ctrl Pts',(30.763267624326,1.30642002708729,26.4579000478329));
#66258=CARTESIAN_POINT('Ctrl Pts',(30.4044749371868,1.4569895622401,26.479344956129));
#66259=CARTESIAN_POINT('Ctrl Pts',(30.2159899848526,1.49659297949806,26.4895135375502));
#66260=CARTESIAN_POINT('Ctrl Pts',(29.8264040657205,1.50311771775866,26.5084387415533));
#66261=CARTESIAN_POINT('Ctrl Pts',(29.6289313228251,1.46692091172634,26.5187719136178));
#66262=CARTESIAN_POINT('Ctrl Pts',(29.2622864534942,1.32066065000658,26.5404749081659));
#66263=CARTESIAN_POINT('Ctrl Pts',(29.0963152488665,1.21314636529189,26.5514467093804));
#66264=CARTESIAN_POINT('Ctrl Pts',(28.8192613253014,0.944447852152411,26.5722403200802));
#66265=CARTESIAN_POINT('Ctrl Pts',(28.7092361098565,0.787428080615722,26.5812539955214));
#66266=CARTESIAN_POINT('Ctrl Pts',(28.5500186537103,0.4325695152731,26.6009683602626));
#66267=CARTESIAN_POINT('Ctrl Pts',(28.5055087117716,0.236724815037938,26.6118486213868));
#66268=CARTESIAN_POINT('Ctrl Pts',(28.4955827399852,-0.155640049113208,
26.6336466693952));
#66269=CARTESIAN_POINT('Ctrl Pts',(28.5282144121142,-0.348361913823613,
26.6443534396569));
#66270=CARTESIAN_POINT('Ctrl Pts',(28.6646766132005,-0.710004687419899,
26.6644447048566));
#66271=CARTESIAN_POINT('Ctrl Pts',(28.7669073789545,-0.875602741749661,
26.6733284353239));
#66272=CARTESIAN_POINT('Ctrl Pts',(29.0326342692594,-1.16351957915387,26.6941109162225));
#66273=CARTESIAN_POINT('Ctrl Pts',(29.1952892767769,-1.28140768888904,26.7052113286353));
#66274=CARTESIAN_POINT('Ctrl Pts',(29.5502593863542,-1.44373597574174,26.7267989550745));
#66275=CARTESIAN_POINT('Ctrl Pts',(29.7380028348229,-1.48930167419739,26.7370974797965));
#66276=CARTESIAN_POINT('Ctrl Pts',(29.9528487018704,-1.49944465692866,26.7477160059146));
#66277=CARTESIAN_POINT('Ctrl Pts',(29.9764341399413,-1.50000000000001,26.7488661870293));
#66278=CARTESIAN_POINT('Ctrl Pts',(29.9999999999999,-1.50000000000001,26.75));
#66279=CARTESIAN_POINT('Ctrl Pts',(30.0000000000001,-1.50000000000001,26.8125));
#66280=CARTESIAN_POINT('Ctrl Pts',(29.8395800016776,-1.50000000000002,26.8047817892321));
#66281=CARTESIAN_POINT('Ctrl Pts',(29.6800130120943,-1.4742710204936,26.7963899249912));
#66282=CARTESIAN_POINT('Ctrl Pts',(29.3406580591605,-1.36160698346738,26.7769331456215));
#66283=CARTESIAN_POINT('Ctrl Pts',(29.1679496395237,-1.26348603655748,26.7658981260489));
#66284=CARTESIAN_POINT('Ctrl Pts',(28.8688888773426,-1.00499369846698,26.744329215695));
#66285=CARTESIAN_POINT('Ctrl Pts',(28.7459708502921,-0.846646295408431,
26.7345359053005));
#66286=CARTESIAN_POINT('Ctrl Pts',(28.5719299961441,-0.497373685523865,
26.7151318714181));
#66287=CARTESIAN_POINT('Ctrl Pts',(28.5201211210885,-0.310969647956289,
26.7047760915532));
#66288=CARTESIAN_POINT('Ctrl Pts',(28.4888763927518,0.078675171393689,26.6831291571448));
#66289=CARTESIAN_POINT('Ctrl Pts',(28.5126680280148,0.27845746343119,26.6720301409206));
#66290=CARTESIAN_POINT('Ctrl Pts',(28.6347687943924,0.650483449918004,26.6513620305602));
#66291=CARTESIAN_POINT('Ctrl Pts',(28.7293030467267,0.819946999855557,26.6425267967844));
#66292=CARTESIAN_POINT('Ctrl Pts',(28.9783004894773,1.11523286685495,26.62234451654));
#66293=CARTESIAN_POINT('Ctrl Pts',(29.1308905878018,1.23784103842587,26.6115972394678));
#66294=CARTESIAN_POINT('Ctrl Pts',(29.4786064716065,1.42045274911996,26.5897952036888));
#66295=CARTESIAN_POINT('Ctrl Pts',(29.671307799161,1.47699671076135,26.5789531911429));
#66296=CARTESIAN_POINT('Ctrl Pts',(30.058657983757,1.51083891985875,26.5593767353335));
#66297=CARTESIAN_POINT('Ctrl Pts',(30.2492918070221,1.49128918840572,26.5502639753537));
#66298=CARTESIAN_POINT('Ctrl Pts',(30.6191301716824,1.38027512961514,26.5293863948823));
#66299=CARTESIAN_POINT('Ctrl Pts',(30.7941362196709,1.2875659668366,26.518391157951));
#66300=CARTESIAN_POINT('Ctrl Pts',(31.1019229551517,1.03729505553015,26.4966307919773));
#66301=CARTESIAN_POINT('Ctrl Pts',(31.2305302882388,0.880892156398053,26.4864384531331));
#66302=CARTESIAN_POINT('Ctrl Pts',(31.4143329938993,0.535011347738905,26.467222852652));
#66303=CARTESIAN_POINT('Ctrl Pts',(31.4709425533457,0.350543024469619,26.4569746124704));
#66304=CARTESIAN_POINT('Ctrl Pts',(31.5126435249117,-0.0370627264893054,
26.4354409596394));
#66305=CARTESIAN_POINT('Ctrl Pts',(31.4944467514533,-0.236856679751601,
26.4243412955692));
#66306=CARTESIAN_POINT('Ctrl Pts',(31.382763240843,-0.612667143007661,26.4034629364995));
#66307=CARTESIAN_POINT('Ctrl Pts',(31.2923692914564,-0.785603738087747,
26.3945234871348));
#66308=CARTESIAN_POINT('Ctrl Pts',(31.0508333839059,-1.08773585408316,26.3745100265869));
#66309=CARTESIAN_POINT('Ctrl Pts',(30.9019600520426,-1.21403192877114,26.3638391307711));
#66310=CARTESIAN_POINT('Ctrl Pts',(30.559750929656,-1.4057831061822,26.3420481650989));
#66311=CARTESIAN_POINT('Ctrl Pts',(30.3686322762759,-1.46754077280931,26.3311374738613));
#66312=CARTESIAN_POINT('Ctrl Pts',(30.1141378164167,-1.49674664949133,26.3180818291001));
#66313=CARTESIAN_POINT('Ctrl Pts',(30.0570405412872,-1.50000000000001,26.3152443643222));
#66314=CARTESIAN_POINT('Ctrl Pts',(30.0000000000002,-1.50000000000001,26.3125));
#66315=CARTESIAN_POINT('Origin',(30.,-1.32966554433622E-14,16.));
#66316=CARTESIAN_POINT('',(30.0000000000001,-1.50000000000001,25.75));
#66317=CARTESIAN_POINT('',(30.,-1.50000000000001,25.8125));
#66318=CARTESIAN_POINT('',(30.,-1.50000000000001,16.));
#66319=CARTESIAN_POINT('Ctrl Pts',(30.0000000000002,-1.50000000000001,25.75));
#66320=CARTESIAN_POINT('Ctrl Pts',(30.0350308469701,-1.50000000000001,25.7516854224107));
#66321=CARTESIAN_POINT('Ctrl Pts',(30.0700958017757,-1.49877287551864,25.7534065726266));
#66322=CARTESIAN_POINT('Ctrl Pts',(30.3035194655511,-1.48237243734734,25.7650927416133));
#66323=CARTESIAN_POINT('Ctrl Pts',(30.4971388675202,-1.42911969045028,25.7758875024032));
#66324=CARTESIAN_POINT('Ctrl Pts',(30.848183508266,-1.2523218603483,25.7976881963921));
#66325=CARTESIAN_POINT('Ctrl Pts',(31.0030592952475,-1.13208157746957,25.8084796690252));
#66326=CARTESIAN_POINT('Ctrl Pts',(31.2567047166631,-0.841106936698577,
25.8287658189633));
#66327=CARTESIAN_POINT('Ctrl Pts',(31.3538096540821,-0.673770640691784,
25.8375682977395));
#66328=CARTESIAN_POINT('Ctrl Pts',(31.4823392304013,-0.304145984064151,
25.8581030008855));
#66329=CARTESIAN_POINT('Ctrl Pts',(31.5096068971125,-0.104447172132542,
25.8691973793261));
#66330=CARTESIAN_POINT('Ctrl Pts',(31.4848844296652,0.286323023183646,25.8909068346215));
#66331=CARTESIAN_POINT('Ctrl Pts',(31.4360830652788,0.473864860798067,25.9013258256));
#66332=CARTESIAN_POINT('Ctrl Pts',(31.2680746858178,0.825196096656156,25.9208442275921));
#66333=CARTESIAN_POINT('Ctrl Pts',(31.1486056539627,0.984726473310249,25.9304245311885));
#66334=CARTESIAN_POINT('Ctrl Pts',(30.8549287066094,1.24817526789042,25.9518720919776));
#66335=CARTESIAN_POINT('Ctrl Pts',(30.6837094772403,1.34958696185865,25.9629268724906));
#66336=CARTESIAN_POINT('Ctrl Pts',(30.3185036845909,1.47806545582453,25.9840666914365));
#66337=CARTESIAN_POINT('Ctrl Pts',(30.1289070957048,1.50647679352315,25.993618043535));
#66338=CARTESIAN_POINT('Ctrl Pts',(29.7404075656125,1.49068855536224,26.0127482980627));
#66339=CARTESIAN_POINT('Ctrl Pts',(29.545331017818,1.44318830470102,26.0234533742517));
#66340=CARTESIAN_POINT('Ctrl Pts',(29.188736991222,1.27663378618483,26.0452365267588));
#66341=CARTESIAN_POINT('Ctrl Pts',(29.0299764729631,1.16060540084053,26.056097906459));
#66342=CARTESIAN_POINT('Ctrl Pts',(28.7683079019703,0.877153943717209,26.0765610930375));
#66343=CARTESIAN_POINT('Ctrl Pts',(28.6667786145465,0.713430148276809,26.0853649917623));
#66344=CARTESIAN_POINT('Ctrl Pts',(28.5272614190292,0.348018884480366,26.1056656175288));
#66345=CARTESIAN_POINT('Ctrl Pts',(28.4940188142116,0.14859972255689,26.1167444598579));
#66346=CARTESIAN_POINT('Ctrl Pts',(28.5074840531687,-0.243852309362615,
26.1385473505201));
#66347=CARTESIAN_POINT('Ctrl Pts',(28.5510714566589,-0.433234122923729,
26.1490685623846));
#66348=CARTESIAN_POINT('Ctrl Pts',(28.7087569062828,-0.788023018123922,
26.1687790565624));
#66349=CARTESIAN_POINT('Ctrl Pts',(28.8224400778707,-0.949553940205162,
26.1780544535033));
#66350=CARTESIAN_POINT('Ctrl Pts',(29.1069273076436,-1.22127183449108,26.1992895710132));
#66351=CARTESIAN_POINT('Ctrl Pts',(29.2754819087647,-1.32821443027861,26.2103697857015));
#66352=CARTESIAN_POINT('Ctrl Pts',(29.6323103908041,-1.46593097223903,26.2313631635471));
#66353=CARTESIAN_POINT('Ctrl Pts',(29.8154198943914,-1.50000000000001,26.2411193855283));
#66354=CARTESIAN_POINT('Ctrl Pts',(30.,-1.50000000000001,26.25));
#66355=CARTESIAN_POINT('Ctrl Pts',(30.0000000000002,-1.50000000000001,26.3125));
#66356=CARTESIAN_POINT('Ctrl Pts',(29.867580258195,-1.50000000000001,26.3061289522019));
#66357=CARTESIAN_POINT('Ctrl Pts',(29.7355134428156,-1.48246999719879,26.299287940062));
#66358=CARTESIAN_POINT('Ctrl Pts',(29.4184023489971,-1.39643165750255,26.2816409715667));
#66359=CARTESIAN_POINT('Ctrl Pts',(29.2414246745114,-1.30875331188796,26.2706906196325));
#66360=CARTESIAN_POINT('Ctrl Pts',(28.9285790709285,-1.068455989113,26.2489639028796));
#66361=CARTESIAN_POINT('Ctrl Pts',(28.7965902868422,-0.917216536990246,
26.2384564742772));
#66362=CARTESIAN_POINT('Ctrl Pts',(28.6032774267936,-0.57923818308581,26.2196798990602));
#66363=CARTESIAN_POINT('Ctrl Pts',(28.5410496718181,-0.397228347537677,
26.2095682415298));
#66364=CARTESIAN_POINT('Ctrl Pts',(28.4870387262231,-0.0124011503103316,
26.1881889527949));
#66365=CARTESIAN_POINT('Ctrl Pts',(28.4986129287161,0.187210043596071,26.1770994420224));
#66366=CARTESIAN_POINT('Ctrl Pts',(28.5978341126594,0.567369358609899,26.1559794800772));
#66367=CARTESIAN_POINT('Ctrl Pts',(28.6833047820777,0.744501773375072,26.1468355900596));
#66368=CARTESIAN_POINT('Ctrl Pts',(28.9160253075989,1.05460577600707,26.1270248184819));
#66369=CARTESIAN_POINT('Ctrl Pts',(29.060441358732,1.18507685788338,26.1164524012633));
#66370=CARTESIAN_POINT('Ctrl Pts',(29.3972605323865,1.3881264388998,26.0946069150758));
#66371=CARTESIAN_POINT('Ctrl Pts',(29.5879874006837,1.45617711323181,26.0835402678372));
#66372=CARTESIAN_POINT('Ctrl Pts',(29.9751313819113,1.51185807000195,26.0633671011121));
#66373=CARTESIAN_POINT('Ctrl Pts',(30.1672228871666,1.50278877622694,26.0545319510962));
#66374=CARTESIAN_POINT('Ctrl Pts',(30.5421508905102,1.41213985662164,26.0339751935801));
#66375=CARTESIAN_POINT('Ctrl Pts',(30.7210278648892,1.32972839399854,26.0230797638426));
#66376=CARTESIAN_POINT('Ctrl Pts',(31.0401525812529,1.09890434445495,26.0013140896138));
#66377=CARTESIAN_POINT('Ctrl Pts',(31.1764827770535,0.951536572108244,25.9906613507783));
#66378=CARTESIAN_POINT('Ctrl Pts',(31.3792148041551,0.619604996410003,25.9716870800294));
#66379=CARTESIAN_POINT('Ctrl Pts',(31.4465937278795,0.439945368358781,25.9619414093531));
#66380=CARTESIAN_POINT('Ctrl Pts',(31.5118285637272,0.0578389075257285,
25.9407132726402));
#66381=CARTESIAN_POINT('Ctrl Pts',(31.5063115855957,-0.141417075009879,
25.9296434958327));
#66382=CARTESIAN_POINT('Ctrl Pts',(31.4186362556573,-0.525426994647723,
25.9083096114084));
#66383=CARTESIAN_POINT('Ctrl Pts',(31.3377111820022,-0.706481965554299,
25.8989028268757));
#66384=CARTESIAN_POINT('Ctrl Pts',(31.1130533652913,-1.0237694591265,25.8792804311414));
#66385=CARTESIAN_POINT('Ctrl Pts',(30.972766729538,-1.15788504149396,25.8688054543882));
#66386=CARTESIAN_POINT('Ctrl Pts',(30.6428698469895,-1.36991560346518,25.8470435453937));
#66387=CARTESIAN_POINT('Ctrl Pts',(30.4547968017865,-1.44330311864552,25.835956334699));
#66388=CARTESIAN_POINT('Ctrl Pts',(30.1725168697432,-1.4925627888959,25.8210068109627));
#66389=CARTESIAN_POINT('Ctrl Pts',(30.0862466800351,-1.50000000000001,25.8166495453279));
#66390=CARTESIAN_POINT('Ctrl Pts',(30.,-1.50000000000001,25.8125));
#66391=CARTESIAN_POINT('Origin',(30.,-1.32966554433622E-14,16.));
#66392=CARTESIAN_POINT('',(30.0000000000001,-1.50000000000001,25.25));
#66393=CARTESIAN_POINT('',(30.,-1.50000000000001,25.3125));
#66394=CARTESIAN_POINT('',(30.,-1.50000000000001,16.));
#66395=CARTESIAN_POINT('Ctrl Pts',(30.0000000000001,-1.50000000000001,25.25));
#66396=CARTESIAN_POINT('Ctrl Pts',(30.0627700539087,-1.50000000000001,25.2530200256268));
#66397=CARTESIAN_POINT('Ctrl Pts',(30.1255978857231,-1.49606031931736,25.2561522666689));
#66398=CARTESIAN_POINT('Ctrl Pts',(30.387395972516,-1.46296629655124,25.2696673114027));
#66399=CARTESIAN_POINT('Ctrl Pts',(30.5795743359629,-1.39800636679879,25.2807179397182));
#66400=CARTESIAN_POINT('Ctrl Pts',(30.9202426421314,-1.20018691165606,25.3026033361058));
#66401=CARTESIAN_POINT('Ctrl Pts',(31.0669765445057,-1.07185443274338,25.3132278653563));
#66402=CARTESIAN_POINT('Ctrl Pts',(31.3042648643842,-0.765865616588927,
25.3331440943071));
#66403=CARTESIAN_POINT('Ctrl Pts',(31.3922917557281,-0.59091969078094,25.3421711282901));
#66404=CARTESIAN_POINT('Ctrl Pts',(31.4979914701149,-0.212996523390812,
25.3631668598117));
#66405=CARTESIAN_POINT('Ctrl Pts',(31.5129981369395,-0.0132639168507718,
25.3742631157306));
#66406=CARTESIAN_POINT('Ctrl Pts',(31.4653583210385,0.373052959697002,25.3957251644277));
#66407=CARTESIAN_POINT('Ctrl Pts',(31.4060337226141,0.556359728684241,25.4059088738159));
#66408=CARTESIAN_POINT('Ctrl Pts',(31.2180258231604,0.89772836856045,25.4248737982534));
#66409=CARTESIAN_POINT('Ctrl Pts',(31.088460968798,1.05109657163312,25.4351618575451));
#66410=CARTESIAN_POINT('Ctrl Pts',(30.7792551558925,1.29659274113508,25.4568578671965));
#66411=CARTESIAN_POINT('Ctrl Pts',(30.6034030192283,1.3871914976091,25.4678351891908));
#66412=CARTESIAN_POINT('Ctrl Pts',(30.2324892526205,1.49400946706811,25.4886479519256));
#66413=CARTESIAN_POINT('Ctrl Pts',(30.0415773273281,1.51141487828139,25.4976825299541));
#66414=CARTESIAN_POINT('Ctrl Pts',(29.6545526771042,1.47316919187237,25.5173656422979));
#66415=CARTESIAN_POINT('Ctrl Pts',(29.4624963512885,1.41443679130397,25.5282374121534));
#66416=CARTESIAN_POINT('Ctrl Pts',(29.1170567587378,1.22797823527613,25.5500367866331));
#66417=CARTESIAN_POINT('Ctrl Pts',(28.9660123174462,1.10381260264269,25.560752961054));
#66418=CARTESIAN_POINT('Ctrl Pts',(28.7201314342041,0.805655980053721,25.5808650389699));
#66419=CARTESIAN_POINT('Ctrl Pts',(28.627324212077,0.634750626561539,25.5897360763022));
#66420=CARTESIAN_POINT('Ctrl Pts',(28.5095600205757,0.261132939276874,25.6104926144847));
#66421=CARTESIAN_POINT('Ctrl Pts',(28.4881034640454,0.0613273497745445,
25.6215929250126));
#66422=CARTESIAN_POINT('Ctrl Pts',(28.5237184917358,-0.327500650137204,
25.6431944805633));
#66423=CARTESIAN_POINT('Ctrl Pts',(28.57753700972,-0.513112472024964,25.6535062484459));
#66424=CARTESIAN_POINT('Ctrl Pts',(28.7556436240904,-0.860981573894074,
25.6728323096608));
#66425=CARTESIAN_POINT('Ctrl Pts',(28.8809148866478,-1.0185241445112,25.6827836630609));
#66426=CARTESIAN_POINT('Ctrl Pts',(29.1836083572217,-1.27362286430434,25.7044330850039));
#66427=CARTESIAN_POINT('Ctrl Pts',(29.357290902101,-1.3695025366285,25.7154527145718));
#66428=CARTESIAN_POINT('Ctrl Pts',(29.6920067607584,-1.47617903100382,25.7345199747848));
#66429=CARTESIAN_POINT('Ctrl Pts',(29.8456406050883,-1.50000000000001,25.7425733801496));
#66430=CARTESIAN_POINT('Ctrl Pts',(30.0000000000002,-1.50000000000001,25.75));
#66431=CARTESIAN_POINT('Ctrl Pts',(30.,-1.50000000000001,25.8125));
#66432=CARTESIAN_POINT('Ctrl Pts',(29.8958136711151,-1.50000000000001,25.8074873329144));
#66433=CARTESIAN_POINT('Ctrl Pts',(29.7916909834384,-1.4891476478018,25.80217627354));
#66434=CARTESIAN_POINT('Ctrl Pts',(29.4989680289332,-1.42717135574301,25.7863710701566));
#66435=CARTESIAN_POINT('Ctrl Pts',(29.3182929815531,-1.3502283271827,25.7755410315376));
#66436=CARTESIAN_POINT('Ctrl Pts',(28.9928896773701,-1.12927046795383,25.7537473394536));
#66437=CARTESIAN_POINT('Ctrl Pts',(28.8522264483536,-0.985982788210688,
25.7429994633659));
#66438=CARTESIAN_POINT('Ctrl Pts',(28.639853465626,-0.660351661724937,25.7237363544014));
#66439=CARTESIAN_POINT('Ctrl Pts',(28.5672444995779,-0.483012345456745,
25.714334019192));
#66440=CARTESIAN_POINT('Ctrl Pts',(28.4907135279836,-0.103874220197911,
25.6932707900109));
#66441=CARTESIAN_POINT('Ctrl Pts',(28.4901189594842,0.0948392876888842,
25.6822311506839));
#66442=CARTESIAN_POINT('Ctrl Pts',(28.5659791907661,0.482606924381713,25.660688504201));
#66443=CARTESIAN_POINT('Ctrl Pts',(28.6422553573453,0.667705397375409,25.6509438140946));
#66444=CARTESIAN_POINT('Ctrl Pts',(28.8587620723286,0.992152292410515,25.6315147161622));
#66445=CARTESIAN_POINT('Ctrl Pts',(28.9948328944551,1.12978254443193,25.6211449431241));
#66446=CARTESIAN_POINT('Ctrl Pts',(29.3175819275344,1.35056278988812,25.599483888434));
#66447=CARTESIAN_POINT('Ctrl Pts',(29.5028611462505,1.42918794783786,25.5883856057019));
#66448=CARTESIAN_POINT('Ctrl Pts',(29.8863465577115,1.507984767606,25.5677463546914));
#66449=CARTESIAN_POINT('Ctrl Pts',(30.0802506039983,1.51013051078303,25.5589203440921));
#66450=CARTESIAN_POINT('Ctrl Pts',(30.4601704571654,1.44079280620514,25.5387153942847));
#66451=CARTESIAN_POINT('Ctrl Pts',(30.6424548754516,1.36926262641685,25.5279582816823));
#66452=CARTESIAN_POINT('Ctrl Pts',(30.9737363815272,1.15817666999724,25.5061559940003));
#66453=CARTESIAN_POINT('Ctrl Pts',(31.118540202541,1.01903114337744,25.4953239633962));
#66454=CARTESIAN_POINT('Ctrl Pts',(31.3403349350297,0.699693252907024,25.4757823623965));
#66455=CARTESIAN_POINT('Ctrl Pts',(31.418072458882,0.524551989157358,25.4666417771753));
#66456=CARTESIAN_POINT('Ctrl Pts',(31.5054879258866,0.148377517280613,25.4457431954044));
#66457=CARTESIAN_POINT('Ctrl Pts',(31.5119666548414,-0.0496365545101339,
25.4347424136382));
#66458=CARTESIAN_POINT('Ctrl Pts',(31.4476607795272,-0.440895614279282,
25.4130057992066));
#66459=CARTESIAN_POINT('Ctrl Pts',(31.3759395541655,-0.629971074835861,
25.4028673928089));
#66460=CARTESIAN_POINT('Ctrl Pts',(31.1673112734267,-0.961240411187918,
25.383627833962));
#66461=CARTESIAN_POINT('Ctrl Pts',(31.0353453440586,-1.10210544227651,25.3733657026948));
#66462=CARTESIAN_POINT('Ctrl Pts',(30.7196295943324,-1.33102399282861,25.3518169729773));
#66463=CARTESIAN_POINT('Ctrl Pts',(30.5371475111052,-1.41455738295539,25.3407169277066));
#66464=CARTESIAN_POINT('Ctrl Pts',(30.2307882933611,-1.48667060842925,25.3239740678184));
#66465=CARTESIAN_POINT('Ctrl Pts',(30.1154677152456,-1.50000000000002,25.31805544304));
#66466=CARTESIAN_POINT('Ctrl Pts',(29.9999999999999,-1.50000000000001,25.3125));
#66467=CARTESIAN_POINT('Origin',(30.,-1.32966554433622E-14,16.));
#66468=CARTESIAN_POINT('',(30.,-1.50000000000001,24.75));
#66469=CARTESIAN_POINT('',(29.9999999999999,-1.50000000000001,24.8125));
#66470=CARTESIAN_POINT('',(30.,-1.50000000000001,16.));
#66471=CARTESIAN_POINT('Ctrl Pts',(30.,-1.50000000000001,24.75));
#66472=CARTESIAN_POINT('Ctrl Pts',(30.0924202028298,-1.50000000000002,24.7544465690819));
#66473=CARTESIAN_POINT('Ctrl Pts',(30.1848415762481,-1.49146009950343,24.759130413942));
#66474=CARTESIAN_POINT('Ctrl Pts',(30.4723479931102,-1.43762037173554,24.7744586208663));
#66475=CARTESIAN_POINT('Ctrl Pts',(30.6592834359903,-1.36205645668747,24.7855515541955));
#66476=CARTESIAN_POINT('Ctrl Pts',(30.9862537983022,-1.14638219357722,24.80727387484));
#66477=CARTESIAN_POINT('Ctrl Pts',(31.1248087259681,-1.01079850350159,24.8177063155187));
#66478=CARTESIAN_POINT('Ctrl Pts',(31.346109752526,-0.69055016576277,24.8372494532827));
#66479=CARTESIAN_POINT('Ctrl Pts',(31.4251274703691,-0.50783917665878,24.8467867124079));
#66480=CARTESIAN_POINT('Ctrl Pts',(31.5079543915197,-0.122264618516638,
24.8682075211936));
#66481=CARTESIAN_POINT('Ctrl Pts',(31.5109523526148,0.0767903025210503,
24.8792661279179));
#66482=CARTESIAN_POINT('Ctrl Pts',(31.441061251381,0.457686740875712,24.9004270411598));
#66483=CARTESIAN_POINT('Ctrl Pts',(31.3715371249325,0.636385044039808,24.9100225849775));
#66484=CARTESIAN_POINT('Ctrl Pts',(31.1648481820269,0.965747220324715,24.9291158607209));
#66485=CARTESIAN_POINT('Ctrl Pts',(31.0267283705006,1.11145999209774,24.939808730245));
#66486=CARTESIAN_POINT('Ctrl Pts',(30.7049953637051,1.33826413832451,24.9615882319247));
#66487=CARTESIAN_POINT('Ctrl Pts',(30.525362209954,1.41844022126688,24.9724579494792));
#66488=CARTESIAN_POINT('Ctrl Pts',(30.1493787440764,1.50469862427576,24.9929435291658));
#66489=CARTESIAN_POINT('Ctrl Pts',(29.9569371691124,1.5114809139774,25.00175294714));
#66490=CARTESIAN_POINT('Ctrl Pts',(29.5704977811955,1.45108059660786,25.0220233074535));
#66491=CARTESIAN_POINT('Ctrl Pts',(29.3808354910635,1.38084291684638,25.0330994853021));
#66492=CARTESIAN_POINT('Ctrl Pts',(29.0468101101847,1.17410520091496,25.0549130032641));
#66493=CARTESIAN_POINT('Ctrl Pts',(28.9040664949486,1.04213311105638,25.0654466500392));
#66494=CARTESIAN_POINT('Ctrl Pts',(28.6746221434491,0.72909790198446,25.0851812190219));
#66495=CARTESIAN_POINT('Ctrl Pts',(28.5909928953227,0.55038117737188,25.0944232679238));
#66496=CARTESIAN_POINT('Ctrl Pts',(28.496446216206,0.168641933616187,25.115631003688));
#66497=CARTESIAN_POINT('Ctrl Pts',(28.4873339658181,-0.0308466586561953,
25.1267137032587));
#66498=CARTESIAN_POINT('Ctrl Pts',(28.5459190178277,-0.414647584032544,
25.1480359768907));
#66499=CARTESIAN_POINT('Ctrl Pts',(28.6102581790788,-0.595692019972521,
25.1580163493537));
#66500=CARTESIAN_POINT('Ctrl Pts',(28.8073809961852,-0.931227827424643,
25.1768208644096));
#66501=CARTESIAN_POINT('Ctrl Pts',(28.9411488677475,-1.08089452062442,25.1874141822753));
#66502=CARTESIAN_POINT('Ctrl Pts',(29.2565034825196,-1.31734526046784,25.2091547643595));
#66503=CARTESIAN_POINT('Ctrl Pts',(29.4342658933141,-1.40290303357365,25.220083967145));
#66504=CARTESIAN_POINT('Ctrl Pts',(29.7466738861071,-1.48392560477994,25.2373653306843));
#66505=CARTESIAN_POINT('Ctrl Pts',(29.8731973879732,-1.50000000000001,25.2438992064844));
#66506=CARTESIAN_POINT('Ctrl Pts',(30.0000000000001,-1.50000000000001,25.25));
#66507=CARTESIAN_POINT('Ctrl Pts',(29.9999999999999,-1.50000000000001,25.3125));
#66508=CARTESIAN_POINT('Ctrl Pts',(29.9230963675565,-1.50000000000001,25.3087999722589));
#66509=CARTESIAN_POINT('Ctrl Pts',(29.8461434428577,-1.49408668250554,25.3049333141238));
#66510=CARTESIAN_POINT('Ctrl Pts',(29.5785997947569,-1.4525378268213,25.2909069794727));
#66511=CARTESIAN_POINT('Ctrl Pts',(29.394946779968,-1.38612426885289,25.2802261486243));
#66512=CARTESIAN_POINT('Ctrl Pts',(29.0584111434883,-1.1844646483524,25.2584329141398));
#66513=CARTESIAN_POINT('Ctrl Pts',(28.9098271705268,-1.04932739740415,25.2475303518813));
#66514=CARTESIAN_POINT('Ctrl Pts',(28.679224033866,-0.736002543967933,25.2277319851447));
#66515=CARTESIAN_POINT('Ctrl Pts',(28.5966653608253,-0.562858820299269,
25.218769934461));
#66516=CARTESIAN_POINT('Ctrl Pts',(28.4992036771274,-0.189506940379824,
25.1980281633544));
#66517=CARTESIAN_POINT('Ctrl Pts',(28.4873077258157,0.00770736323463039,
25.1870718131536));
#66518=CARTESIAN_POINT('Ctrl Pts',(28.5403428741226,0.398677937032776,25.1653512257204));
#66519=CARTESIAN_POINT('Ctrl Pts',(28.6059812891417,0.588385613614782,25.1548923783415));
#66520=CARTESIAN_POINT('Ctrl Pts',(28.8032229731553,0.924175534219124,25.1360750856002));
#66521=CARTESIAN_POINT('Ctrl Pts',(28.9302878616598,1.06867554049118,25.1259477842385));
#66522=CARTESIAN_POINT('Ctrl Pts',(29.2375170160562,1.30684882772379,25.1045502900104));
#66523=CARTESIAN_POINT('Ctrl Pts',(29.416566346389,1.39601031268743,25.0934590671725));
#66524=CARTESIAN_POINT('Ctrl Pts',(29.7956879290814,1.49872079338579,25.0723655026123));
#66525=CARTESIAN_POINT('Ctrl Pts',(29.9916913791595,1.51255777708596,25.0632485758478));
#66526=CARTESIAN_POINT('Ctrl Pts',(30.376338186137,1.46478286918679,25.0434151669436));
#66527=CARTESIAN_POINT('Ctrl Pts',(30.5613937867408,1.40429329778983,25.0328314093361));
#66528=CARTESIAN_POINT('Ctrl Pts',(30.9051019650582,1.2128519030953,25.0109769253773));
#66529=CARTESIAN_POINT('Ctrl Pts',(31.0589867932662,1.08110262857348,24.9999134360581));
#66530=CARTESIAN_POINT('Ctrl Pts',(31.2996601001576,0.7727813254929,24.9797695555402));
#66531=CARTESIAN_POINT('Ctrl Pts',(31.3872075591177,0.601637196257516,24.9709242886809));
#66532=CARTESIAN_POINT('Ctrl Pts',(31.4948659823167,0.231233394936456,24.9503462997187));
#66533=CARTESIAN_POINT('Ctrl Pts',(31.5122374051454,0.0349818838105959,
24.9394434379894));
#66534=CARTESIAN_POINT('Ctrl Pts',(31.4704629549247,-0.356714017311379,
24.9176825545938));
#66535=CARTESIAN_POINT('Ctrl Pts',(31.410306361987,-0.548240683911054,24.9070421842271));
#66536=CARTESIAN_POINT('Ctrl Pts',(31.2229499202263,-0.889130700933294,
24.8881038499482));
#66537=CARTESIAN_POINT('Ctrl Pts',(31.1004741653132,-1.03689935475768,24.8783104947773));
#66538=CARTESIAN_POINT('Ctrl Pts',(30.8011609016804,-1.28341012707365,24.8570622572132));
#66539=CARTESIAN_POINT('Ctrl Pts',(30.6254139659021,-1.37762857486559,24.8459894497178));
#66540=CARTESIAN_POINT('Ctrl Pts',(30.2947063232275,-1.4782094919839,24.8272843564766));
#66541=CARTESIAN_POINT('Ctrl Pts',(30.1476360382517,-1.50000000000004,24.8196031422022));
#66542=CARTESIAN_POINT('Ctrl Pts',(29.9999999999998,-1.50000000000001,24.8125));
#66543=CARTESIAN_POINT('Origin',(30.,-1.32966554433622E-14,16.));
#66544=CARTESIAN_POINT('',(30.,-1.50000000000001,24.25));
#66545=CARTESIAN_POINT('',(30.,-1.50000000000001,24.3125));
#66546=CARTESIAN_POINT('',(30.,-1.50000000000001,16.));
#66547=CARTESIAN_POINT('Ctrl Pts',(29.9999999999999,-1.50000000000001,24.25));
#66548=CARTESIAN_POINT('Ctrl Pts',(30.1233865336442,-1.50000000000002,24.2559364373678));
#66549=CARTESIAN_POINT('Ctrl Pts',(30.2465476489323,-1.48477988594364,24.2622848102359));
#66550=CARTESIAN_POINT('Ctrl Pts',(30.5591244259704,-1.40597165010196,24.2795127850953));
#66551=CARTESIAN_POINT('Ctrl Pts',(30.7400033595231,-1.31975922707827,24.2906101163719));
#66552=CARTESIAN_POINT('Ctrl Pts',(31.0517371878966,-1.08642473531537,24.3120899308425));
#66553=CARTESIAN_POINT('Ctrl Pts',(31.181396759577,-0.943819238764671,24.3222894436867));
#66554=CARTESIAN_POINT('Ctrl Pts',(31.3842738432636,-0.610977913754327,
24.341295964288));
#66555=CARTESIAN_POINT('Ctrl Pts',(31.4529950991553,-0.422325812949031,
24.3515374548362));
#66556=CARTESIAN_POINT('Ctrl Pts',(31.5124147536636,-0.0319347678693356,
24.3732258462295));
#66557=CARTESIAN_POINT('Ctrl Pts',(31.5036442008573,0.165759327603677,24.3842088515336));
#66558=CARTESIAN_POINT('Ctrl Pts',(31.4119825510711,0.540750850840327,24.4050417139356));
#66559=CARTESIAN_POINT('Ctrl Pts',(31.3322181025457,0.715044299742208,24.4140993016492));
#66560=CARTESIAN_POINT('Ctrl Pts',(31.106713322535,1.03186525150623,24.4337494874295));
#66561=CARTESIAN_POINT('Ctrl Pts',(30.9603062459911,1.1693383575936,24.4446121985753));
#66562=CARTESIAN_POINT('Ctrl Pts',(30.6267827077052,1.37647673516795,24.4664127011144));
#66563=CARTESIAN_POINT('Ctrl Pts',(30.4439056234701,1.4458581458551,24.47713864034));
#66564=CARTESIAN_POINT('Ctrl Pts',(30.0630400763872,1.51099956140736,24.4972725262831));
#66565=CARTESIAN_POINT('Ctrl Pts',(29.8687484810349,1.50660828894347,24.5061312780688));
#66566=CARTESIAN_POINT('Ctrl Pts',(29.4860566158504,1.4231980920111,24.526860498932));
#66567=CARTESIAN_POINT('Ctrl Pts',(29.3019333862064,1.34250650777999,24.5379605648438));
#66568=CARTESIAN_POINT('Ctrl Pts',(28.9821049580114,1.11829253966791,24.5595764830508));
#66569=CARTESIAN_POINT('Ctrl Pts',(28.8477437066725,0.979293286040407,24.5699020321484));
#66570=CARTESIAN_POINT('Ctrl Pts',(28.6345240475922,0.651988290747904,24.5892523732038));
#66571=CARTESIAN_POINT('Ctrl Pts',(28.5601403785395,0.465238374198666,24.5991534236556));
#66572=CARTESIAN_POINT('Ctrl Pts',(28.489084947481,0.0759965520384366,24.6207779693312));
#66573=CARTESIAN_POINT('Ctrl Pts',(28.4921379080883,-0.122445995567395,
24.6318025553093));
#66574=CARTESIAN_POINT('Ctrl Pts',(28.5732141775453,-0.500358663169468,
24.6527977035094));
#66575=CARTESIAN_POINT('Ctrl Pts',(28.6479534934179,-0.676775662247645,
24.662082289407));
#66576=CARTESIAN_POINT('Ctrl Pts',(28.8642453292122,-0.999806026462223,
24.6814617008812));
#66577=CARTESIAN_POINT('Ctrl Pts',(29.0066425215227,-1.1413892524153,24.6922456563782));
#66578=CARTESIAN_POINT('Ctrl Pts',(29.3345224631394,-1.35826808429126,24.7140451994209));
#66579=CARTESIAN_POINT('Ctrl Pts',(29.515884916708,-1.43296761407463,24.7248459914751));
#66580=CARTESIAN_POINT('Ctrl Pts',(29.8033393621129,-1.4903304156034,24.7402695610815));
#66581=CARTESIAN_POINT('Ctrl Pts',(29.901655948172,-1.50000000000001,24.7452684196003));
#66582=CARTESIAN_POINT('Ctrl Pts',(30.,-1.50000000000001,24.75));
#66583=CARTESIAN_POINT('Ctrl Pts',(29.9999999999998,-1.50000000000001,24.8125));
#66584=CARTESIAN_POINT('Ctrl Pts',(29.9520844763832,-1.50000000000001,24.8101946632951));
#66585=CARTESIAN_POINT('Ctrl Pts',(29.9041155058213,-1.49770423456202,24.8078229838607));
#66586=CARTESIAN_POINT('Ctrl Pts',(29.6647429412583,-1.47465918202179,24.7956660256301));
#66587=CARTESIAN_POINT('Ctrl Pts',(29.4785801635781,-1.4195491435244,24.7851784304102));
#66588=CARTESIAN_POINT('Ctrl Pts',(29.1305308217309,-1.23854895841351,24.7634051157232));
#66589=CARTESIAN_POINT('Ctrl Pts',(28.9733425780824,-1.11174127780071,24.752319957252));
#66590=CARTESIAN_POINT('Ctrl Pts',(28.7235507953419,-0.81069913235786,24.7319395626836));
#66591=CARTESIAN_POINT('Ctrl Pts',(28.6307275649839,-0.641599855569549,
24.7231444364205));
#66592=CARTESIAN_POINT('Ctrl Pts',(28.5125127288929,-0.274334472746556,
24.7027408040415));
#66593=CARTESIAN_POINT('Ctrl Pts',(28.4895069858667,-0.0792389156648355,
24.6919021619814));
#66594=CARTESIAN_POINT('Ctrl Pts',(28.5196116095794,0.313003938746328,24.6701108922919));
#66595=CARTESIAN_POINT('Ctrl Pts',(28.5740816740222,0.506262436197778,24.6593743091001));
#66596=CARTESIAN_POINT('Ctrl Pts',(28.7511791399573,0.852358280491469,24.640146762195));
#66597=CARTESIAN_POINT('Ctrl Pts',(28.8690245914396,1.00348928998653,24.630706043882));
#66598=CARTESIAN_POINT('Ctrl Pts',(29.1601188576535,1.25831795738381,24.6096221903744));
#66599=CARTESIAN_POINT('Ctrl Pts',(29.3323550489326,1.35757677634782,24.5985782833421));
#66600=CARTESIAN_POINT('Ctrl Pts',(29.7064392762191,1.4842685830248,24.577060930713));
#66601=CARTESIAN_POINT('Ctrl Pts',(29.9047304118308,1.51001063736079,24.5673617334579));
#66602=CARTESIAN_POINT('Ctrl Pts',(30.2937060245362,1.48342562743484,24.547908663068));
#66603=CARTESIAN_POINT('Ctrl Pts',(30.4808263548115,1.43373651283452,24.5375255787967));
#66604=CARTESIAN_POINT('Ctrl Pts',(30.8329282215013,1.26331849859809,24.5158512361083));
#66605=CARTESIAN_POINT('Ctrl Pts',(30.9932828024692,1.14155315563778,24.5047538020966));
#66606=CARTESIAN_POINT('Ctrl Pts',(31.2521599269974,0.847929325410954,24.4841423531291));
#66607=CARTESIAN_POINT('Ctrl Pts',(31.3503160471837,0.680833771104865,24.4753240983947));
#66608=CARTESIAN_POINT('Ctrl Pts',(31.4789636487266,0.316753550496772,24.455097419472));
#66609=CARTESIAN_POINT('Ctrl Pts',(31.5074931621648,0.122957581810777,24.4443309767673));
#66610=CARTESIAN_POINT('Ctrl Pts',(31.4889302469637,-0.269482846800126,
24.4225287307333));
#66611=CARTESIAN_POINT('Ctrl Pts',(31.4401374224707,-0.464284058469581,
24.4117064411961));
#66612=CARTESIAN_POINT('Ctrl Pts',(31.2732400969951,-0.815428064678723,
24.3921984408512));
#66613=CARTESIAN_POINT('Ctrl Pts',(31.1598920572171,-0.96991270557316,24.3830299796895));
#66614=CARTESIAN_POINT('Ctrl Pts',(30.8768520990815,-1.23274788918355,24.3621112360319));
#66615=CARTESIAN_POINT('Ctrl Pts',(30.7081704356177,-1.33679806788068,24.351105252973));
#66616=CARTESIAN_POINT('Ctrl Pts',(30.3563528915165,-1.46803396077468,24.330532982021));
#66617=CARTESIAN_POINT('Ctrl Pts',(30.1788031709794,-1.50000000000002,24.3211026715747));
#66618=CARTESIAN_POINT('Ctrl Pts',(29.9999999999999,-1.50000000000001,24.3125));
#66619=CARTESIAN_POINT('Origin',(30.,-1.32966554433622E-14,16.));
#66620=CARTESIAN_POINT('',(29.9999999999999,-1.50000000000001,23.75));
#66621=CARTESIAN_POINT('',(30.,-1.50000000000001,23.8125));
#66622=CARTESIAN_POINT('',(30.,-1.50000000000001,16.));
#66623=CARTESIAN_POINT('Ctrl Pts',(29.9999999999998,-1.50000000000001,23.75));
#66624=CARTESIAN_POINT('Ctrl Pts',(30.1539214445734,-1.50000000000004,23.7574055489549));
#66625=CARTESIAN_POINT('Ctrl Pts',(30.3071622224275,-1.47631426128188,23.7654362865035));
#66626=CARTESIAN_POINT('Ctrl Pts',(30.6423330661034,-1.36978679250727,23.7845212975935));
#66627=CARTESIAN_POINT('Ctrl Pts',(30.8166966283757,-1.27354330571266,23.7955837985834));
#66628=CARTESIAN_POINT('Ctrl Pts',(31.1127372375018,-1.02370190976136,23.8167670978074));
#66629=CARTESIAN_POINT('Ctrl Pts',(31.2333636655921,-0.874601042154043,
23.8264110532137));
#66630=CARTESIAN_POINT('Ctrl Pts',(31.4166526755054,-0.531631844802988,
23.8454648975109));
#66631=CARTESIAN_POINT('Ctrl Pts',(31.4745582697856,-0.339396978512901,
23.8561446123048));
#66632=CARTESIAN_POINT('Ctrl Pts',(31.511699941184,0.0525578729813968,23.8779198818323));
#66633=CARTESIAN_POINT('Ctrl Pts',(31.4920858025539,0.248369535334408,23.8887983075186));
#66634=CARTESIAN_POINT('Ctrl Pts',(31.3802343334373,0.617537171179423,23.909307620621));
#66635=CARTESIAN_POINT('Ctrl Pts',(31.2906053859832,0.78786629286171,23.9181242275504));
#66636=CARTESIAN_POINT('Ctrl Pts',(31.0463195284336,1.0933231170364,23.9383623481344));
#66637=CARTESIAN_POINT('Ctrl Pts',(30.8911113639651,1.22312916938911,23.9494355281055));
#66638=CARTESIAN_POINT('Ctrl Pts',(30.5456512461468,1.41045613992281,23.9712600127329));
#66639=CARTESIAN_POINT('Ctrl Pts',(30.3601397930707,1.4688221637187,23.9818067151192));
#66640=CARTESIAN_POINT('Ctrl Pts',(29.9746198000426,1.51244309002935,24.0015667468295));
#66641=CARTESIAN_POINT('Ctrl Pts',(29.7781833324316,1.4963071428617,24.0107747387592));
#66642=CARTESIAN_POINT('Ctrl Pts',(29.3999877237922,1.38893180194388,24.0319533318226));
#66643=CARTESIAN_POINT('Ctrl Pts',(29.222220687541,1.29776778429998,24.0430384861654));
#66644=CARTESIAN_POINT('Ctrl Pts',(28.9180417312452,1.05625627096343,24.0643819561719));
#66645=CARTESIAN_POINT('Ctrl Pts',(28.7928010889864,0.910453809129913,24.0744192328261));
#66646=CARTESIAN_POINT('Ctrl Pts',(28.5994385143727,0.572669994103534,24.0931850003275));
#66647=CARTESIAN_POINT('Ctrl Pts',(28.5359684061524,0.382240685005912,24.1037644063885));
#66648=CARTESIAN_POINT('Ctrl Pts',(28.4873420883061,-0.00897112678811804,
24.1254983959326));
#66649=CARTESIAN_POINT('Ctrl Pts',(28.5013820601517,-0.205827079960202,
24.1364348377755));
#66650=CARTESIAN_POINT('Ctrl Pts',(28.6028303892674,-0.578036208077185,
24.1571131226709));
#66651=CARTESIAN_POINT('Ctrl Pts',(28.6873275910153,-0.750394994115161,
24.1660216580016));
#66652=CARTESIAN_POINT('Ctrl Pts',(28.922674074919,-1.0628953635868,24.1860253368065));
#66653=CARTESIAN_POINT('Ctrl Pts',(29.0745736829203,-1.19747470970914,24.197071925274));
#66654=CARTESIAN_POINT('Ctrl Pts',(29.4156235588556,-1.39492862582615,24.2189655260838));
#66655=CARTESIAN_POINT('Ctrl Pts',(29.5999664963488,-1.45853020454807,24.2296014403193));
#66656=CARTESIAN_POINT('Ctrl Pts',(29.8606029709014,-1.49514680076604,24.2431584462207));
#66657=CARTESIAN_POINT('Ctrl Pts',(29.9303308703141,-1.50000000000001,24.2466480424351));
#66658=CARTESIAN_POINT('Ctrl Pts',(29.9999999999999,-1.50000000000001,24.25));
#66659=CARTESIAN_POINT('Ctrl Pts',(29.9999999999999,-1.50000000000001,24.3125));
#66660=CARTESIAN_POINT('Ctrl Pts',(29.9792133017942,-1.50000000000001,24.3114998995163));
#66661=CARTESIAN_POINT('Ctrl Pts',(29.9584107993835,-1.49956791710601,24.3104870363498));
#66662=CARTESIAN_POINT('Ctrl Pts',(29.7464034347025,-1.4907415866322,24.3000416514142));
#66663=CARTESIAN_POINT('Ctrl Pts',(29.5585103106211,-1.44626636462019,24.2897662164333));
#66664=CARTESIAN_POINT('Ctrl Pts',(29.2028124426411,-1.28608329400307,24.2682031650416));
#66665=CARTESIAN_POINT('Ctrl Pts',(29.0395645726164,-1.16922656097766,24.2571028778712));
#66666=CARTESIAN_POINT('Ctrl Pts',(28.7720346147835,-0.882829614311603,
24.2362758660328));
#66667=CARTESIAN_POINT('Ctrl Pts',(28.6687223598358,-0.717623891574991,
24.2273679939764));
#66668=CARTESIAN_POINT('Ctrl Pts',(28.5302095932634,-0.356628416668571,
24.2073126898149));
#66669=CARTESIAN_POINT('Ctrl Pts',(28.4965070465723,-0.164202501526158,
24.1966223611959));
#66670=CARTESIAN_POINT('Ctrl Pts',(28.504169008249,0.22811087427228,24.1748271736516));
#66671=CARTESIAN_POINT('Ctrl Pts',(28.547551398078,0.424213342298486,24.1639325920946));
#66672=CARTESIAN_POINT('Ctrl Pts',(28.7047478969298,0.780036844220854,24.1441646197656));
#66673=CARTESIAN_POINT('Ctrl Pts',(28.8139070776359,0.937725434330763,24.1351846602695));
#66674=CARTESIAN_POINT('Ctrl Pts',(29.089396967151,1.20794416549895,24.1144240709145));
#66675=CARTESIAN_POINT('Ctrl Pts',(29.2546507832928,1.31634974323744,24.10346202693));
#66676=CARTESIAN_POINT('Ctrl Pts',(29.6203184116569,1.46471395475137,24.0817476068599));
#66677=CARTESIAN_POINT('Ctrl Pts',(29.817562104219,1.50206749812624,24.0713349778568));
#66678=CARTESIAN_POINT('Ctrl Pts',(30.2070481745296,1.49784204922514,24.0524784469813));
#66679=CARTESIAN_POINT('Ctrl Pts',(30.3956551706626,1.45939464529562,24.0423361052064));
#66680=CARTESIAN_POINT('Ctrl Pts',(30.7551447714595,1.31111335433136,24.0209212289748));
#66681=CARTESIAN_POINT('Ctrl Pts',(30.9215534250012,1.20000288285394,24.0098284869129));
#66682=CARTESIAN_POINT('Ctrl Pts',(31.1989915137811,0.922095691461922,23.9887605964375));
#66683=CARTESIAN_POINT('Ctrl Pts',(31.3083178283937,0.759038041694919,23.9796687800942));
#66684=CARTESIAN_POINT('Ctrl Pts',(31.4580557742773,0.401642541393168,23.9598134745218));
#66685=CARTESIAN_POINT('Ctrl Pts',(31.4975752946798,0.210938880716583,23.9492188267065));
#66686=CARTESIAN_POINT('Ctrl Pts',(31.5023006219625,-0.182594498957542,
23.927355861169));
#66687=CARTESIAN_POINT('Ctrl Pts',(31.4644403140633,-0.381679718202,23.916295571211));
#66688=CARTESIAN_POINT('Ctrl Pts',(31.3164762945118,-0.74375638752885,23.8961802006929));
#66689=CARTESIAN_POINT('Ctrl Pts',(31.2115088567194,-0.904729197971778,
23.8873240471024));
#66690=CARTESIAN_POINT('Ctrl Pts',(30.9436055459159,-1.18225533242814,23.8667254837612));
#66691=CARTESIAN_POINT('Ctrl Pts',(30.7818828902994,-1.29490194314203,23.8558155263452));
#66692=CARTESIAN_POINT('Ctrl Pts',(30.4211554702292,-1.45331769745592,23.8340595826352));
#66693=CARTESIAN_POINT('Ctrl Pts',(30.225061216149,-1.49628795964726,23.8234313750427));
#66694=CARTESIAN_POINT('Ctrl Pts',(30.01751075903,-1.49992336974507,23.8133446154048));
#66695=CARTESIAN_POINT('Ctrl Pts',(30.0087538759465,-1.50000000000001,23.8129211710528));
#66696=CARTESIAN_POINT('Ctrl Pts',(30.,-1.50000000000001,23.8125));
#66697=CARTESIAN_POINT('Origin',(30.,-1.32966554433622E-14,16.));
#66698=CARTESIAN_POINT('',(30.,-1.50000000000001,23.25));
#66699=CARTESIAN_POINT('',(30.0000000000001,-1.50000000000001,23.3125));
#66700=CARTESIAN_POINT('',(30.,-1.50000000000001,16.));
#66701=CARTESIAN_POINT('Ctrl Pts',(30.,-1.50000000000001,23.25));
#66702=CARTESIAN_POINT('Ctrl Pts',(30.1848807806478,-1.50000000000001,23.2588950807062));
#66703=CARTESIAN_POINT('Ctrl Pts',(30.3682821495602,-1.46581977714696,23.268668433817));
#66704=CARTESIAN_POINT('Ctrl Pts',(30.7253175152828,-1.32777981441322,23.2896807492688));
#66705=CARTESIAN_POINT('Ctrl Pts',(30.8938177244611,-1.22072861570022,23.3007613637715));
#66706=CARTESIAN_POINT('Ctrl Pts',(31.17812266521,-0.948849031570725,23.3219922022812));
#66707=CARTESIAN_POINT('Ctrl Pts',(31.2916923057403,-0.787278580688064,
23.3312623010729));
#66708=CARTESIAN_POINT('Ctrl Pts',(31.4491725851422,-0.432421790169133,
23.3509765672128));
#66709=CARTESIAN_POINT('Ctrl Pts',(31.4926555401856,-0.243004803835009,
23.3614997331203));
#66710=CARTESIAN_POINT('Ctrl Pts',(31.5058959055076,0.149477495401521,23.3833043053001));
#66711=CARTESIAN_POINT('Ctrl Pts',(31.4725342594551,0.348889338242185,23.3943827410135));
#66712=CARTESIAN_POINT('Ctrl Pts',(31.3327988700423,0.714215497781599,23.4146786387656));
#66713=CARTESIAN_POINT('Ctrl Pts',(31.2311812032015,0.877867947558743,23.4234833208414));
#66714=CARTESIAN_POINT('Ctrl Pts',(30.9693523131294,1.16116792111582,23.4439500128983));
#66715=CARTESIAN_POINT('Ctrl Pts',(30.8105149834806,1.27711053175663,23.4548127055575));
#66716=CARTESIAN_POINT('Ctrl Pts',(30.4538126686857,1.44345770015622,23.4765953083576));
#66717=CARTESIAN_POINT('Ctrl Pts',(30.2587086794859,1.49084210066152,23.487298486762));
#66718=CARTESIAN_POINT('Ctrl Pts',(29.8701963712835,1.50640033026212,23.5064229669502));
#66719=CARTESIAN_POINT('Ctrl Pts',(29.6806119299331,1.47787523708767,23.5159811423084));
#66720=CARTESIAN_POINT('Ctrl Pts',(29.3158918902727,1.34932104216597,23.5370996932649));
#66721=CARTESIAN_POINT('Ctrl Pts',(29.1450773397405,1.24811033609704,23.5481294207781));
#66722=CARTESIAN_POINT('Ctrl Pts',(28.8572342555358,0.990033097118328,23.5691470898178));
#66723=CARTESIAN_POINT('Ctrl Pts',(28.741208429162,0.837555866674711,23.578469118518));
#66724=CARTESIAN_POINT('Ctrl Pts',(28.5682103547001,0.489415671302002,23.5978102404832));
#66725=CARTESIAN_POINT('Ctrl Pts',(28.5160198061383,0.295515658346084,23.6085824634252));
#66726=CARTESIAN_POINT('Ctrl Pts',(28.4905622848027,-0.0968477988030621,
23.6303804332668));
#66727=CARTESIAN_POINT('Ctrl Pts',(28.5157978904665,-0.291438773395986,
23.6411910429664));
#66728=CARTESIAN_POINT('Ctrl Pts',(28.6382130227664,-0.657431308298791,
23.6615239615721));
#66729=CARTESIAN_POINT('Ctrl Pts',(28.733169022031,-0.825722839750627,23.6703196450362));
#66730=CARTESIAN_POINT('Ctrl Pts',(28.9866100524997,-1.12380536152502,23.6907934023492));
#66731=CARTESIAN_POINT('Ctrl Pts',(29.1450855427347,-1.24860164286396,23.7018846212987));
#66732=CARTESIAN_POINT('Ctrl Pts',(29.4947960835532,-1.42537206508902,23.723620367045));
#66733=CARTESIAN_POINT('Ctrl Pts',(29.6813612118254,-1.47831159941945,23.7340670285844));
#66734=CARTESIAN_POINT('Ctrl Pts',(29.9152096611065,-1.49820471212254,23.7458706538102));
#66735=CARTESIAN_POINT('Ctrl Pts',(29.957628226374,-1.50000000000001,23.7479613870909));
#66736=CARTESIAN_POINT('Ctrl Pts',(29.9999999999998,-1.50000000000001,23.75));
#66737=CARTESIAN_POINT('Ctrl Pts',(30.,-1.50000000000001,23.8125));
#66738=CARTESIAN_POINT('Ctrl Pts',(29.8186899108673,-1.50000000000001,23.8037767142694));
#66739=CARTESIAN_POINT('Ctrl Pts',(29.6387564217711,-1.46712852254306,23.7942065636429));
#66740=CARTESIAN_POINT('Ctrl Pts',(29.284195027604,-1.33291119731626,23.7734194615783));
#66741=CARTESIAN_POINT('Ctrl Pts',(29.1150531352934,-1.22715164870581,23.762343853251));
#66742=CARTESIAN_POINT('Ctrl Pts',(28.8285848658366,-0.957196675383623,
23.7410623929517));
#66743=CARTESIAN_POINT('Ctrl Pts',(28.713664846415,-0.796095622176884,23.7317275345654));
#66744=CARTESIAN_POINT('Ctrl Pts',(28.5537507892143,-0.442046290271719,
23.7120581272374));
#66745=CARTESIAN_POINT('Ctrl Pts',(28.50903084701,-0.253050072432249,23.7015583373574));
#66746=CARTESIAN_POINT('Ctrl Pts',(28.493125704307,0.139065210502765,23.6797741549721));
#66747=CARTESIAN_POINT('Ctrl Pts',(28.5250759127101,0.338559440554235,23.6686911421915));
#66748=CARTESIAN_POINT('Ctrl Pts',(28.6622225705316,0.704891738980156,23.6483393478345));
#66749=CARTESIAN_POINT('Ctrl Pts',(28.7627930544851,0.869391639366899,23.6395420458263));
#66750=CARTESIAN_POINT('Ctrl Pts',(29.0227223626785,1.15448356589741,23.6191169709735));
#66751=CARTESIAN_POINT('Ctrl Pts',(29.1806474642266,1.27143845898823,23.6082700489523));
#66752=CARTESIAN_POINT('Ctrl Pts',(29.5360600403599,1.4402358268239,23.5864814376371));
#66753=CARTESIAN_POINT('Ctrl Pts',(29.7308346201,1.48899068833401,23.5757560395914));
#66754=CARTESIAN_POINT('Ctrl Pts',(30.1191927262396,1.50727161649964,23.5565633479378));
#66755=CARTESIAN_POINT('Ctrl Pts',(30.3089226794933,1.48009155403507,23.5470839383266));
#66756=CARTESIAN_POINT('Ctrl Pts',(30.6746275130695,1.35410584970156,23.5259893534154));
#66757=CARTESIAN_POINT('Ctrl Pts',(30.8462644331352,1.25401826984556,23.5149512576394));
#66758=CARTESIAN_POINT('Ctrl Pts',(31.1359831388577,0.997812339501797,23.4938953285128));
#66759=CARTESIAN_POINT('Ctrl Pts',(31.2530579642409,0.846112941875841,23.4845062745487));
#66760=CARTESIAN_POINT('Ctrl Pts',(31.4284239202414,0.499151075957345,23.465230615331));
#66761=CARTESIAN_POINT('Ctrl Pts',(31.4819315716114,0.305618089705,23.4544787827614));
#66762=CARTESIAN_POINT('Ctrl Pts',(31.5100720569101,-0.086682490418841,
23.4326843060879));
#66763=CARTESIAN_POINT('Ctrl Pts',(31.4861228872238,-0.281567854400411,
23.4218573414222));
#66764=CARTESIAN_POINT('Ctrl Pts',(31.3661326726942,-0.648296896097567,
23.4014835057724));
#66765=CARTESIAN_POINT('Ctrl Pts',(31.2724103712455,-0.817054396960877,
23.3926895837254));
#66766=CARTESIAN_POINT('Ctrl Pts',(31.0210775409326,-1.11685004948265,23.3722696702745));
#66767=CARTESIAN_POINT('Ctrl Pts',(30.8633432283804,-1.24281066274781,23.3611817686994));
#66768=CARTESIAN_POINT('Ctrl Pts',(30.5145869816219,-1.42202815813894,23.3394239621929));
#66769=CARTESIAN_POINT('Ctrl Pts',(30.3282514191413,-1.47622279958149,23.3289534815563));
#66770=CARTESIAN_POINT('Ctrl Pts',(30.0912045055574,-1.4979228580024,23.3169457772084));
#66771=CARTESIAN_POINT('Ctrl Pts',(30.0455768509778,-1.50000000000001,23.3146928172651));
#66772=CARTESIAN_POINT('Ctrl Pts',(30.0000000000002,-1.50000000000001,23.3125));
#66773=CARTESIAN_POINT('Origin',(30.,-1.32966554433622E-14,16.));
#66774=CARTESIAN_POINT('',(30.0000000000001,-1.50000000000001,22.75));
#66775=CARTESIAN_POINT('',(30.,-1.50000000000001,22.8125));
#66776=CARTESIAN_POINT('',(30.,-1.50000000000001,16.));
#66777=CARTESIAN_POINT('Ctrl Pts',(30.0000000000001,-1.50000000000001,22.75));
#66778=CARTESIAN_POINT('Ctrl Pts',(30.0238190927805,-1.50000000000001,22.7511459966357));
#66779=CARTESIAN_POINT('Ctrl Pts',(30.0476581179369,-1.49943265781826,22.7523087117734));
#66780=CARTESIAN_POINT('Ctrl Pts',(30.2627622738244,-1.48916810759789,22.7629430416939));
#66781=CARTESIAN_POINT('Ctrl Pts',(30.4504917710081,-1.44350305068679,22.7732436551414));
#66782=CARTESIAN_POINT('Ctrl Pts',(30.8053949324493,-1.28097942369943,22.7948334866517));
#66783=CARTESIAN_POINT('Ctrl Pts',(30.9679955997388,-1.16299746502374,22.8059338915341));
#66784=CARTESIAN_POINT('Ctrl Pts',(31.2335580340327,-0.874942371993705,
22.8267123004732));
#66785=CARTESIAN_POINT('Ctrl Pts',(31.3356903480274,-0.709308500806453,
22.8355939721774));
#66786=CARTESIAN_POINT('Ctrl Pts',(31.4719653898389,-0.347606806174152,
22.8556885107681));
#66787=CARTESIAN_POINT('Ctrl Pts',(31.5044992018676,-0.154858219876142,
22.8663967655625));
#66788=CARTESIAN_POINT('Ctrl Pts',(31.4943665307067,0.237510688978279,22.8881950382766));
#66789=CARTESIAN_POINT('Ctrl Pts',(31.4497537465181,0.433331528903234,22.899073973828));
#66790=CARTESIAN_POINT('Ctrl Pts',(31.2903519524536,0.78810181728577,22.9187834342937));
#66791=CARTESIAN_POINT('Ctrl Pts',(31.1802475750943,0.945060620681391,22.9278003293086));
#66792=CARTESIAN_POINT('Ctrl Pts',(30.9030507590494,1.21362000516214,22.948596950241));
#66793=CARTESIAN_POINT('Ctrl Pts',(30.7370141991215,1.32105257322674,22.9595696259569));
#66794=CARTESIAN_POINT('Ctrl Pts',(30.3702805499944,1.46712017353723,22.9812715402192));
#66795=CARTESIAN_POINT('Ctrl Pts',(30.1727871861063,1.50321114583692,22.991597574137));
#66796=CARTESIAN_POINT('Ctrl Pts',(29.7831928098337,1.49647610979574,23.0105290266394));
#66797=CARTESIAN_POINT('Ctrl Pts',(29.5947193673977,1.45676699750561,23.0206999902635));
#66798=CARTESIAN_POINT('Ctrl Pts',(29.2359911149794,1.30598838211349,23.0421476062271));
#66799=CARTESIAN_POINT('Ctrl Pts',(29.0702277888966,1.19366882317697,23.05324288572));
#66800=CARTESIAN_POINT('Ctrl Pts',(28.7948557226535,0.913971635465609,23.0742610967597));
#66801=CARTESIAN_POINT('Ctrl Pts',(28.686793719435,0.750466721324838,23.0833074043708));
#66802=CARTESIAN_POINT('Ctrl Pts',(28.5393908078851,0.39231449396832,23.1032047503351));
#66803=CARTESIAN_POINT('Ctrl Pts',(28.50107471408,0.201238476218244,23.1138200846545));
#66804=CARTESIAN_POINT('Ctrl Pts',(28.4989279287216,-0.192576857122968,
23.1356987142846));
#66805=CARTESIAN_POINT('Ctrl Pts',(28.5381471159066,-0.391544240809387,
23.1467524578227));
#66806=CARTESIAN_POINT('Ctrl Pts',(28.6885908974138,-0.752626531003943,
23.1668125850557));
#66807=CARTESIAN_POINT('Ctrl Pts',(28.7945746463293,-0.912795946069086,
23.1756927219105));
#66808=CARTESIAN_POINT('Ctrl Pts',(29.0643193882896,-1.1885583990927,23.1963308899987));
#66809=CARTESIAN_POINT('Ctrl Pts',(29.2269067570048,-1.30018824275338,23.2072542074138));
#66810=CARTESIAN_POINT('Ctrl Pts',(29.5888237919401,-1.45617120236401,23.228999808865));
#66811=CARTESIAN_POINT('Ctrl Pts',(29.7851989650319,-1.49779418034797,23.2396041076185));
#66812=CARTESIAN_POINT('Ctrl Pts',(29.9893352495882,-1.49997157194577,23.2494861022884));
#66813=CARTESIAN_POINT('Ctrl Pts',(29.9946682024469,-1.50000000000001,23.2497434737706));
#66814=CARTESIAN_POINT('Ctrl Pts',(30.,-1.50000000000001,23.25));
#66815=CARTESIAN_POINT('Ctrl Pts',(30.0000000000003,-1.50000000000001,23.3125));
#66816=CARTESIAN_POINT('Ctrl Pts',(29.8497176527518,-1.50000000000002,23.3052695371968));
#66817=CARTESIAN_POINT('Ctrl Pts',(29.7000480379928,-1.47742120454004,23.2974413657365));
#66818=CARTESIAN_POINT('Ctrl Pts',(29.3674490033452,-1.37435151569836,23.2785761403087));
#66819=CARTESIAN_POINT('Ctrl Pts',(29.1922818901849,-1.27927791742795,23.2675074753621));
#66820=CARTESIAN_POINT('Ctrl Pts',(28.8943459539799,-1.03136235914611,23.2462864826624));
#66821=CARTESIAN_POINT('Ctrl Pts',(28.7726494682524,-0.883034040962408,
23.2365574467202));
#66822=CARTESIAN_POINT('Ctrl Pts',(28.5870020748245,-0.541267982453404,
23.2175704434697));
#66823=CARTESIAN_POINT('Ctrl Pts',(28.5277906685824,-0.349440299767995,
23.2069133499871));
#66824=CARTESIAN_POINT('Ctrl Pts',(28.487963650694,0.0423711662580389,23.185146046319));
#66825=CARTESIAN_POINT('Ctrl Pts',(28.5062787794266,0.238440842104816,23.1742532865498));
#66826=CARTESIAN_POINT('Ctrl Pts',(28.6157002622386,0.608326552071247,23.1537040804405));
#66827=CARTESIAN_POINT('Ctrl Pts',(28.704120723826,0.779127514930934,23.1448722564411));
#66828=CARTESIAN_POINT('Ctrl Pts',(28.9463114752997,1.08624863564316,23.1246887062359));
#66829=CARTESIAN_POINT('Ctrl Pts',(29.100754465216,1.21718400346422,23.1136209708684));
#66830=CARTESIAN_POINT('Ctrl Pts',(29.4452036060534,1.40690072974557,23.0917787447896));
#66831=CARTESIAN_POINT('Ctrl Pts',(29.630453412942,1.46649956876065,23.0812103859941));
#66832=CARTESIAN_POINT('Ctrl Pts',(30.0154678344856,1.51253258675255,23.0614076760565));
#66833=CARTESIAN_POINT('Ctrl Pts',(30.2116518417758,1.49773354664468,23.052253938977));
#66834=CARTESIAN_POINT('Ctrl Pts',(30.5903886500576,1.39306917025536,23.031124612004));
#66835=CARTESIAN_POINT('Ctrl Pts',(30.7689034771477,1.3030667277533,23.0200357455338));
#66836=CARTESIAN_POINT('Ctrl Pts',(31.0748241700176,1.06351798971685,22.9986629977234));
#66837=CARTESIAN_POINT('Ctrl Pts',(31.2011381587389,0.918481956232081,22.9885569343996));
#66838=CARTESIAN_POINT('Ctrl Pts',(31.3967520547264,0.581861797904625,22.9697948964873));
#66839=CARTESIAN_POINT('Ctrl Pts',(31.4615014415134,0.391859484339943,22.9592699713522));
#66840=CARTESIAN_POINT('Ctrl Pts',(31.5127002734739,0.000740375396987882,
22.9375411319665));
#66841=CARTESIAN_POINT('Ctrl Pts',(31.4999079686113,-0.196327016676456,
22.9265929435179));
#66842=CARTESIAN_POINT('Ctrl Pts',(31.4007804390091,-0.569202940848263,
22.9058776143973));
#66843=CARTESIAN_POINT('Ctrl Pts',(31.3174135571943,-0.742018160934012,
22.8969391404085));
#66844=CARTESIAN_POINT('Ctrl Pts',(31.0853396535684,-1.05432624095891,22.8770982550692));
#66845=CARTESIAN_POINT('Ctrl Pts',(30.9361334950341,-1.18878161757634,22.8661846988469));
#66846=CARTESIAN_POINT('Ctrl Pts',(30.5987439832112,-1.38884930936682,22.8443946025078));
#66847=CARTESIAN_POINT('Ctrl Pts',(30.4148754905707,-1.45440359104526,22.8337272732621));
#66848=CARTESIAN_POINT('Ctrl Pts',(30.1494349053273,-1.49442202191131,22.8198446340705));
#66849=CARTESIAN_POINT('Ctrl Pts',(30.0746909808563,-1.50000000000001,22.816093571492));
#66850=CARTESIAN_POINT('Ctrl Pts',(30.0000000000001,-1.50000000000001,22.8125));
#66851=CARTESIAN_POINT('Origin',(30.,-1.32966554433622E-14,16.));
#66852=CARTESIAN_POINT('',(30.0000000000001,-1.50000000000001,22.25));
#66853=CARTESIAN_POINT('',(30.,-1.50000000000001,22.3125));
#66854=CARTESIAN_POINT('',(30.,-1.50000000000001,16.));
#66855=CARTESIAN_POINT('Ctrl Pts',(30.0000000000002,-1.50000000000001,22.25));
#66856=CARTESIAN_POINT('Ctrl Pts',(30.0511677444063,-1.50000000000001,22.2524618092506));
#66857=CARTESIAN_POINT('Ctrl Pts',(30.1023921263505,-1.49738203467576,22.254999064735));
#66858=CARTESIAN_POINT('Ctrl Pts',(30.3449868915282,-1.47242953219059,22.2673640358856));
#66859=CARTESIAN_POINT('Ctrl Pts',(30.5309019965201,-1.41604718249647,22.2778750569255));
#66860=CARTESIAN_POINT('Ctrl Pts',(30.8779534991821,-1.23257211766357,22.2996691097112));
#66861=CARTESIAN_POINT('Ctrl Pts',(31.0343750352224,-1.10459007945506,22.3107500009898));
#66862=CARTESIAN_POINT('Ctrl Pts',(31.2820199524192,-0.801819415517196,
22.3310751188442));
#66863=CARTESIAN_POINT('Ctrl Pts',(31.3735944009353,-0.632242273686504,
22.3398754292397));
#66864=CARTESIAN_POINT('Ctrl Pts',(31.4893318529591,-0.264232559817084,
22.3603204133435));
#66865=CARTESIAN_POINT('Ctrl Pts',(31.511019003439,-0.0688512669519718,
22.3711749296138));
#66866=CARTESIAN_POINT('Ctrl Pts',(31.4781740542578,0.32329452926424,22.3929608071814));
#66867=CARTESIAN_POINT('Ctrl Pts',(31.422363807823,0.516161881943181,22.403675660108));
#66868=CARTESIAN_POINT('Ctrl Pts',(31.2428531453717,0.861044634974944,22.4228358130542));
#66869=CARTESIAN_POINT('Ctrl Pts',(31.1239285676202,1.01138399102137,22.4323522946618));
#66870=CARTESIAN_POINT('Ctrl Pts',(30.8309115401787,1.26428053578999,22.4534749869891));
#66871=CARTESIAN_POINT('Ctrl Pts',(30.6578432463629,1.3623737449238,22.4645265505225));
#66872=CARTESIAN_POINT('Ctrl Pts',(30.2831279004866,1.48623532989505,22.4859956505893));
#66873=CARTESIAN_POINT('Ctrl Pts',(30.0851137662052,1.5105602610331,22.49561162143));
#66874=CARTESIAN_POINT('Ctrl Pts',(29.6966286981958,1.48149502237994,22.5151099857196));
#66875=CARTESIAN_POINT('Ctrl Pts',(29.5097167303907,1.43054672747056,22.5255180223776));
#66876=CARTESIAN_POINT('Ctrl Pts',(29.1585275612845,1.25766527467259,22.547216881732));
#66877=CARTESIAN_POINT('Ctrl Pts',(28.9988940242273,1.13472310971196,22.5583123140024));
#66878=CARTESIAN_POINT('Ctrl Pts',(28.7421191463059,0.839368453848379,22.5788706970727));
#66879=CARTESIAN_POINT('Ctrl Pts',(28.6452032661271,0.671810533827306,22.5876771925652));
#66880=CARTESIAN_POINT('Ctrl Pts',(28.5189623058816,0.306989072921277,22.6079450515044));
#66881=CARTESIAN_POINT('Ctrl Pts',(28.4917024287485,0.112879611784448,22.6187289104564));
#66882=CARTESIAN_POINT('Ctrl Pts',(28.5129271256702,-0.27954553838217,22.6405303076879));
#66883=CARTESIAN_POINT('Ctrl Pts',(28.5630339289139,-0.474005993650327,
22.6513336663139));
#66884=CARTESIAN_POINT('Ctrl Pts',(28.7322894218787,-0.823994430176359,
22.6707774683431));
#66885=CARTESIAN_POINT('Ctrl Pts',(28.8466683628132,-0.977702516203741,
22.680002042295));
#66886=CARTESIAN_POINT('Ctrl Pts',(29.1315598866997,-1.23870928805523,22.7009590802358));
#66887=CARTESIAN_POINT('Ctrl Pts',(29.301068288962,-1.34167114530826,22.7119746086325));
#66888=CARTESIAN_POINT('Ctrl Pts',(29.6506233621551,-1.46928601783117,22.732337442503));
#66889=CARTESIAN_POINT('Ctrl Pts',(29.8247316115896,-1.50000000000001,22.7415673957309));
#66890=CARTESIAN_POINT('Ctrl Pts',(30.0000000000001,-1.50000000000001,22.75));
#66891=CARTESIAN_POINT('Ctrl Pts',(30.0000000000001,-1.50000000000001,22.8125));
#66892=CARTESIAN_POINT('Ctrl Pts',(29.8821180181442,-1.50000000000001,22.8068284005036));
#66893=CARTESIAN_POINT('Ctrl Pts',(29.7644054408515,-1.48610745961779,22.8007790475884));
#66894=CARTESIAN_POINT('Ctrl Pts',(29.4561358619788,-1.41197523055228,22.7838881919746));
#66895=CARTESIAN_POINT('Ctrl Pts',(29.2741386603191,-1.32762177587115,22.7727886960081));
#66896=CARTESIAN_POINT('Ctrl Pts',(28.9596308471203,-1.09734948081223,22.7512604791499));
#66897=CARTESIAN_POINT('Ctrl Pts',(28.8283658665089,-0.955949757636784,
22.7410172197375));
#66898=CARTESIAN_POINT('Ctrl Pts',(28.6210784753189,-0.623528783846783,
22.7218101845402));
#66899=CARTESIAN_POINT('Ctrl Pts',(28.550139211662,-0.43377020073728,22.7115983444854));
#66900=CARTESIAN_POINT('Ctrl Pts',(28.4878128315539,-0.0419315259951405,
22.6898295292219));
#66901=CARTESIAN_POINT('Ctrl Pts',(28.4952899772074,0.155946448584049,22.678836308412));
#66902=CARTESIAN_POINT('Ctrl Pts',(28.5845546436209,0.531607574681399,22.657966245851));
#66903=CARTESIAN_POINT('Ctrl Pts',(28.6631729955745,0.706378968214403,22.6488631478995));
#66904=CARTESIAN_POINT('Ctrl Pts',(28.886581089556,1.02462509962909,22.6292742506491));
#66905=CARTESIAN_POINT('Ctrl Pts',(29.0320840520478,1.16304620087307,22.6184287055121));
#66906=CARTESIAN_POINT('Ctrl Pts',(29.3643456686259,1.37241961531272,22.5966268328521));
#66907=CARTESIAN_POINT('Ctrl Pts',(29.5468906971467,1.44301653433814,22.585883105544));
#66908=CARTESIAN_POINT('Ctrl Pts',(29.9272228832809,1.51053148619831,22.5657089493774));
#66909=CARTESIAN_POINT('Ctrl Pts',(30.1212939503538,1.50741198602448,22.5568701305933));
#66910=CARTESIAN_POINT('Ctrl Pts',(30.5044378408363,1.42661367919911,22.5361917141558));
#66911=CARTESIAN_POINT('Ctrl Pts',(30.6892182911204,1.34709011542225,22.5250924727137));
#66912=CARTESIAN_POINT('Ctrl Pts',(31.0107046879826,1.12481571216727,22.5034506622537));
#66913=CARTESIAN_POINT('Ctrl Pts',(31.1460355364563,0.986589014961116,22.4930999232927));
#66914=CARTESIAN_POINT('Ctrl Pts',(31.3611183370781,0.66090197936205,22.473704885123));
#66915=CARTESIAN_POINT('Ctrl Pts',(31.4365760335144,0.475089538086611,22.463893863227));
#66916=CARTESIAN_POINT('Ctrl Pts',(31.5103576978905,0.0866802952431828,
22.4423155719579));
#66917=CARTESIAN_POINT('Ctrl Pts',(31.5086976507443,-0.111919508747406,
22.431282249514));
#66918=CARTESIAN_POINT('Ctrl Pts',(31.4301969979147,-0.490528747223499,
22.410248402932));
#66919=CARTESIAN_POINT('Ctrl Pts',(31.3566667795852,-0.667467593155736,
22.4008985610562));
#66920=CARTESIAN_POINT('Ctrl Pts',(31.1425983489439,-0.991976419659515,
22.3815850548154));
#66921=CARTESIAN_POINT('Ctrl Pts',(31.0011829334274,-1.13452992378446,22.370821382905));
#66922=CARTESIAN_POINT('Ctrl Pts',(30.6747026750166,-1.35372782384191,22.3490247635913));
#66923=CARTESIAN_POINT('Ctrl Pts',(30.4937271061129,-1.42970164427305,22.3382071885718));
#66924=CARTESIAN_POINT('Ctrl Pts',(30.2032733713701,-1.48966742655325,22.322567010569));
#66925=CARTESIAN_POINT('Ctrl Pts',(30.1016602333963,-1.50000000000001,22.3173911302598));
#66926=CARTESIAN_POINT('Ctrl Pts',(30.,-1.50000000000001,22.3125));
#66927=CARTESIAN_POINT('Origin',(30.,-1.32966554433622E-14,16.));
#66928=CARTESIAN_POINT('',(30.,-1.50000000000001,21.75));
#66929=CARTESIAN_POINT('',(29.9999999999999,-1.50000000000001,21.8125));
#66930=CARTESIAN_POINT('',(30.,-1.50000000000001,16.));
#66931=CARTESIAN_POINT('Ctrl Pts',(30.,-1.50000000000001,21.75));
#66932=CARTESIAN_POINT('Ctrl Pts',(30.0799345840677,-1.50000000000001,21.7538458544691));
#66933=CARTESIAN_POINT('Ctrl Pts',(30.1599122998412,-1.4936114408734,21.7578712440892));
#66934=CARTESIAN_POINT('Ctrl Pts',(30.4303228176761,-1.44993500309235,21.7720946105773));
#66935=CARTESIAN_POINT('Ctrl Pts',(30.6136742893428,-1.38234553687229,21.7827935975436));
#66936=CARTESIAN_POINT('Ctrl Pts',(30.9490281775211,-1.17851150378185,21.8045903754862));
#66937=CARTESIAN_POINT('Ctrl Pts',(31.096754819913,-1.04244516916321,21.8154774972882));
#66938=CARTESIAN_POINT('Ctrl Pts',(31.3253413942278,-0.727732251316939,
21.8352173994684));
#66939=CARTESIAN_POINT('Ctrl Pts',(31.4067935410376,-0.554135842314364,
21.8442146754271));
#66940=CARTESIAN_POINT('Ctrl Pts',(31.5019658936778,-0.180133518226551,
21.8649925823208));
#66941=CARTESIAN_POINT('Ctrl Pts',(31.5126290136531,0.0172760533687308,
21.8759597807428));
#66942=CARTESIAN_POINT('Ctrl Pts',(31.457072059222,0.408029499969523,21.8976683055539));
#66943=CARTESIAN_POINT('Ctrl Pts',(31.3902144216195,0.597326073407902,21.9080390017153));
#66944=CARTESIAN_POINT('Ctrl Pts',(31.1907422817111,0.931962878929858,21.9269315763413));
#66945=CARTESIAN_POINT('Ctrl Pts',(31.0626495240423,1.07572029471252,21.9370877035676));
#66946=CARTESIAN_POINT('Ctrl Pts',(30.7536327605205,1.31199280194067,21.9585184047354));
#66947=CARTESIAN_POINT('Ctrl Pts',(30.5738554020277,1.39999410781883,21.9696124276475));
#66948=CARTESIAN_POINT('Ctrl Pts',(30.1942124641512,1.50002082255712,21.9906565268663));
#66949=CARTESIAN_POINT('Ctrl Pts',(29.9984550225415,1.51253833676667,21.9997260456303));
#66950=CARTESIAN_POINT('Ctrl Pts',(29.6143176021754,1.46236614670513,22.0196015378309));
#66951=CARTESIAN_POINT('Ctrl Pts',(29.4295365026789,1.40065016331119,22.0302061554976));
#66952=CARTESIAN_POINT('Ctrl Pts',(29.0868629977602,1.20683686352092,22.052076744962));
#66953=CARTESIAN_POINT('Ctrl Pts',(28.9337539891966,1.07396976987892,22.0631339581722));
#66954=CARTESIAN_POINT('Ctrl Pts',(28.6951751765203,0.763999003449345,22.0832228857165));
#66955=CARTESIAN_POINT('Ctrl Pts',(28.60882966791,0.592379173375639,22.0920900459236));
#66956=CARTESIAN_POINT('Ctrl Pts',(28.5036090779159,0.221263029136351,22.1127076094925));
#66957=CARTESIAN_POINT('Ctrl Pts',(28.4875441317865,0.0247675363524192,
22.1236240257582));
#66958=CARTESIAN_POINT('Ctrl Pts',(28.5320098906898,-0.36675262012417,22.1453751455625));
#66959=CARTESIAN_POINT('Ctrl Pts',(28.593470220051,-0.557855368091198,22.155991964894));
#66960=CARTESIAN_POINT('Ctrl Pts',(28.7831869687067,-0.897529793649072,
22.1748627663138));
#66961=CARTESIAN_POINT('Ctrl Pts',(28.9067443386156,-1.04452569047662,22.1847486483138));
#66962=CARTESIAN_POINT('Ctrl Pts',(29.2079650540828,-1.28908351396432,22.2060344096185));
#66963=CARTESIAN_POINT('Ctrl Pts',(29.3845091949262,-1.38211075548827,22.2171124835975));
#66964=CARTESIAN_POINT('Ctrl Pts',(29.7125665428598,-1.47927872450056,22.2355952603595));
#66965=CARTESIAN_POINT('Ctrl Pts',(29.8560312883098,-1.50000000000001,22.2430733021292));
#66966=CARTESIAN_POINT('Ctrl Pts',(30.0000000000002,-1.50000000000001,22.25));
#66967=CARTESIAN_POINT('Ctrl Pts',(30.,-1.50000000000001,22.3125));
#66968=CARTESIAN_POINT('Ctrl Pts',(29.9110895843884,-1.50000000000001,22.3082222956344));
#66969=CARTESIAN_POINT('Ctrl Pts',(29.8221645100457,-1.49209634975764,22.3037243401601));
#66970=CARTESIAN_POINT('Ctrl Pts',(29.5376207680931,-1.44087704391974,22.288611464497));
#66971=CARTESIAN_POINT('Ctrl Pts',(29.3500356587678,-1.36654835932947,22.2775215860335));
#66972=CARTESIAN_POINT('Ctrl Pts',(29.0213968226607,-1.15294073825471,22.2557763976293));
#66973=CARTESIAN_POINT('Ctrl Pts',(28.8818555948118,-1.01818896609304,22.2453196123919));
#66974=CARTESIAN_POINT('Ctrl Pts',(28.6586442869874,-0.699623440719697,
22.2257313109655));
#66975=CARTESIAN_POINT('Ctrl Pts',(28.5785399664869,-0.517856468116547,
22.2162698037842));
#66976=CARTESIAN_POINT('Ctrl Pts',(28.4929509348882,-0.133169441708886,
22.1948983023171));
#66977=CARTESIAN_POINT('Ctrl Pts',(28.4885197532221,0.0660037349236151,
22.1838331258375));
#66978=CARTESIAN_POINT('Ctrl Pts',(28.555761801385,0.44759093437612,22.1626338369791));
#66979=CARTESIAN_POINT('Ctrl Pts',(28.6240637192867,0.626835313372202,22.1529543398));
#66980=CARTESIAN_POINT('Ctrl Pts',(28.8284985352011,0.957663958533704,22.1339287805455));
#66981=CARTESIAN_POINT('Ctrl Pts',(28.9656007252824,1.10432288929781,22.1232585891618));
#66982=CARTESIAN_POINT('Ctrl Pts',(29.2858531479679,1.33342212875051,22.1014865695287));
#66983=CARTESIAN_POINT('Ctrl Pts',(29.4650586076933,1.41487321083335,22.0906020127698));
#66984=CARTESIAN_POINT('Ctrl Pts',(29.8404420905807,1.50363480947233,22.0700757665663));
#66985=CARTESIAN_POINT('Ctrl Pts',(30.0326825220108,1.51172235919918,22.0612531825154));
#66986=CARTESIAN_POINT('Ctrl Pts',(30.4195266402016,1.45401546056375,22.0410381667945));
#66987=CARTESIAN_POINT('Ctrl Pts',(30.6097995465824,1.38502427774371,22.029967235573));
#66988=CARTESIAN_POINT('Ctrl Pts',(30.9454244752463,1.18038733089544,22.0081351140291));
#66989=CARTESIAN_POINT('Ctrl Pts',(31.0891246269642,1.04926948856203,21.997579174969));
#66990=CARTESIAN_POINT('Ctrl Pts',(31.3204408508467,0.737906981306312,21.9778010094235));
#66991=CARTESIAN_POINT('Ctrl Pts',(31.4051230902783,0.560097094369773,21.9686165052427));
#66992=CARTESIAN_POINT('Ctrl Pts',(31.5023434434385,0.179258057369552,21.9474587809649));
#66993=CARTESIAN_POINT('Ctrl Pts',(31.5128623034415,-0.0203042234475934,
21.9363719875862));
#66994=CARTESIAN_POINT('Ctrl Pts',(31.4568810475112,-0.404757677376984,
21.9150134623679));
#66995=CARTESIAN_POINT('Ctrl Pts',(31.3937249627295,-0.586348141727015,
21.9049348418193));
#66996=CARTESIAN_POINT('Ctrl Pts',(31.1987850558466,-0.923274808506461,
21.8861967170992));
#66997=CARTESIAN_POINT('Ctrl Pts',(31.0660220732146,-1.07382111006007,21.8756273134093));
#66998=CARTESIAN_POINT('Ctrl Pts',(30.7521571303647,-1.31243843036869,21.8538982204082));
#66999=CARTESIAN_POINT('Ctrl Pts',(30.5748417786265,-1.39921326582906,21.8429567194739));
#67000=CARTESIAN_POINT('Ctrl Pts',(30.2597272838717,-1.48309858829145,21.8254656184301));
#67001=CARTESIAN_POINT('Ctrl Pts',(30.1300238421579,-1.50000000000003,21.8187557750226));
#67002=CARTESIAN_POINT('Ctrl Pts',(29.9999999999998,-1.50000000000001,21.8125));
#67003=CARTESIAN_POINT('Origin',(30.,-1.32966554433622E-14,16.));
#67004=CARTESIAN_POINT('',(30.,-1.50000000000001,21.25));
#67005=CARTESIAN_POINT('',(29.9999999999999,-1.50000000000001,21.3125));
#67006=CARTESIAN_POINT('',(30.,-1.50000000000001,16.));
#67007=CARTESIAN_POINT('Ctrl Pts',(30.,-1.50000000000001,21.25));
#67008=CARTESIAN_POINT('Ctrl Pts',(30.1075848726609,-1.50000000000001,21.2551761795993));
#67009=CARTESIAN_POINT('Ctrl Pts',(30.2150815962025,-1.48842822791985,21.2606695562356));
#67010=CARTESIAN_POINT('Ctrl Pts',(30.5108359622909,-1.42370950162225,21.2766967872056));
#67011=CARTESIAN_POINT('Ctrl Pts',(30.6910987866292,-1.34546461195666,21.2875431555427));
#67012=CARTESIAN_POINT('Ctrl Pts',(31.0150386063333,-1.12214805976604,21.3093319549459));
#67013=CARTESIAN_POINT('Ctrl Pts',(31.1546840327806,-0.977879417444189,
21.3200581109451));
#67014=CARTESIAN_POINT('Ctrl Pts',(31.3647735631693,-0.650743634461253,
21.3392531532717));
#67015=CARTESIAN_POINT('Ctrl Pts',(31.4361426481554,-0.472861434650035,
21.3487299202974));
#67016=CARTESIAN_POINT('Ctrl Pts',(31.5100129878737,-0.0930141634261118,
21.3698325464765));
#67017=CARTESIAN_POINT('Ctrl Pts',(31.5091680819865,0.105843895299734,21.3808802164057));
#67018=CARTESIAN_POINT('Ctrl Pts',(31.4305088048906,0.492738271362424,21.4023743484091));
#67019=CARTESIAN_POINT('Ctrl Pts',(31.3531309016418,0.676876453829759,21.4120329161916));
#67020=CARTESIAN_POINT('Ctrl Pts',(31.1347020158755,0.999644296815675,21.4315078542742));
#67021=CARTESIAN_POINT('Ctrl Pts',(30.9976338252526,1.13646112591015,21.4419030181452));
#67022=CARTESIAN_POINT('Ctrl Pts',(30.6731866853066,1.35520814296552,21.4635892944733));
#67023=CARTESIAN_POINT('Ctrl Pts',(30.4872391020676,1.43261266999426,21.474685827494));
#67024=CARTESIAN_POINT('Ctrl Pts',(30.1032980730075,1.50870030742653,21.4952717443516));
#67025=CARTESIAN_POINT('Ctrl Pts',(29.9096173130592,1.50952898426713,21.5040838450456));
#67026=CARTESIAN_POINT('Ctrl Pts',(29.5302606487566,1.43771855687004,21.5243303851611));
#67027=CARTESIAN_POINT('Ctrl Pts',(29.3483375586665,1.36492268311026,21.5351052715185));
#67028=CARTESIAN_POINT('Ctrl Pts',(29.0184009025148,1.15151905747937,21.5569072347786));
#67029=CARTESIAN_POINT('Ctrl Pts',(28.8745521744234,1.01139585435745,21.5677204711336));
#67030=CARTESIAN_POINT('Ctrl Pts',(28.6549505368779,0.690580628714703,21.5871975938919));
#67031=CARTESIAN_POINT('Ctrl Pts',(28.5784089748082,0.514933598952509,21.596392577836));
#67032=CARTESIAN_POINT('Ctrl Pts',(28.4935139297613,0.138064010695691,21.6173297771836));
#67033=CARTESIAN_POINT('Ctrl Pts',(28.4883967455728,-0.0601274794615553,
21.6283404155257));
#67034=CARTESIAN_POINT('Ctrl Pts',(28.5553929405263,-0.450590041266374,
21.6500327800704));
#67035=CARTESIAN_POINT('Ctrl Pts',(28.6281760530356,-0.63873783180513,21.6600741404618));
#67036=CARTESIAN_POINT('Ctrl Pts',(28.8386308155265,-0.968434016466414,
21.6793578772949));
#67037=CARTESIAN_POINT('Ctrl Pts',(28.9715505605447,-1.10856330761102,21.6896454618184));
#67038=CARTESIAN_POINT('Ctrl Pts',(29.2889068065357,-1.33562316156644,21.7112214894881));
#67039=CARTESIAN_POINT('Ctrl Pts',(29.4720453487169,-1.41803231498314,21.7223218898575));
#67040=CARTESIAN_POINT('Ctrl Pts',(29.7757758521236,-1.48742065117207,21.7388625842992));
#67041=CARTESIAN_POINT('Ctrl Pts',(29.8878284604463,-1.50000000000001,21.7446031442869));
#67042=CARTESIAN_POINT('Ctrl Pts',(30.,-1.50000000000001,21.75));
#67043=CARTESIAN_POINT('Ctrl Pts',(29.9999999999998,-1.50000000000001,21.8125));
#67044=CARTESIAN_POINT('Ctrl Pts',(29.9405204451645,-1.50000000000001,21.8096382885837));
#67045=CARTESIAN_POINT('Ctrl Pts',(29.8809833669271,-1.49646250510709,21.8066755458243));
#67046=CARTESIAN_POINT('Ctrl Pts',(29.6241950912386,-1.46572084178495,21.7934668790576));
#67047=CARTESIAN_POINT('Ctrl Pts',(29.4333772164259,-1.40302797833686,21.782544681346));
#67048=CARTESIAN_POINT('Ctrl Pts',(29.0921865820648,-1.20964665656295,21.760757435914));
#67049=CARTESIAN_POINT('Ctrl Pts',(28.9439925649252,-1.08269733302756,21.7501010778418));
#67050=CARTESIAN_POINT('Ctrl Pts',(28.7038088414644,-0.77933430694382,21.7301184823344));
#67051=CARTESIAN_POINT('Ctrl Pts',(28.6141674942217,-0.605760578772268,
21.7211533654873));
#67052=CARTESIAN_POINT('Ctrl Pts',(28.5043846389733,-0.22927416638246,21.7002374536878));
#67053=CARTESIAN_POINT('Ctrl Pts',(28.4872031236976,-0.0294943674923172,
21.6891385759717));
#67054=CARTESIAN_POINT('Ctrl Pts',(28.5307959749546,0.357711165892058,21.6676271574504));
#67055=CARTESIAN_POINT('Ctrl Pts',(28.588271358922,0.541814389624386,21.6573992005764));
#67056=CARTESIAN_POINT('Ctrl Pts',(28.7738533380075,0.887068805374046,21.6382183997014));
#67057=CARTESIAN_POINT('Ctrl Pts',(28.903512180976,1.043112470525,21.6279461150529));
#67058=CARTESIAN_POINT('Ctrl Pts',(29.2128905056455,1.29185751769652,21.6061515588234));
#67059=CARTESIAN_POINT('Ctrl Pts',(29.3882998946744,1.38356922217579,21.5951646233122));
#67060=CARTESIAN_POINT('Ctrl Pts',(29.7586487303438,1.49259838475184,21.5743176187989));
#67061=CARTESIAN_POINT('Ctrl Pts',(29.9494126813103,1.51113463524617,21.5652431789286));
#67062=CARTESIAN_POINT('Ctrl Pts',(30.3366113826679,1.4752126287187,21.5456162392091));
#67063=CARTESIAN_POINT('Ctrl Pts',(30.5290112502297,1.41763409463152,21.5347599925404));
#67064=CARTESIAN_POINT('Ctrl Pts',(30.8756573292315,1.23320190987312,21.512958859045));
#67065=CARTESIAN_POINT('Ctrl Pts',(31.0275193143428,1.10985575574539,21.5022261138206));
#67066=CARTESIAN_POINT('Ctrl Pts',(31.2750461098143,0.813213213668382,21.4820769047076));
#67067=CARTESIAN_POINT('Ctrl Pts',(31.3687657636095,0.643070885011216,21.4732261602783));
#67068=CARTESIAN_POINT('Ctrl Pts',(31.4888227697242,0.270291882918073,21.4525162157176));
#67069=CARTESIAN_POINT('Ctrl Pts',(31.5115128952941,0.0704953149593227,
21.4414164063865));
#67070=CARTESIAN_POINT('Ctrl Pts',(31.4782054807328,-0.318770290439176,
21.4197905394199));
#67071=CARTESIAN_POINT('Ctrl Pts',(31.4254475382382,-0.504803416717179,
21.4094553657378));
#67072=CARTESIAN_POINT('Ctrl Pts',(31.2494901966584,-0.853416070021567,
21.3900879961098));
#67073=CARTESIAN_POINT('Ctrl Pts',(31.1254658116588,-1.01138492328729,21.3802216401301));
#67074=CARTESIAN_POINT('Ctrl Pts',(30.8246930412984,-1.26828298434064,21.3586146462176));
#67075=CARTESIAN_POINT('Ctrl Pts',(30.6515224369356,-1.36534975789868,21.347586672365));
#67076=CARTESIAN_POINT('Ctrl Pts',(30.3143398429227,-1.47517879246933,21.3283131607309));
#67077=CARTESIAN_POINT('Ctrl Pts',(30.1575657374829,-1.50000000000003,21.3200808850792));
#67078=CARTESIAN_POINT('Ctrl Pts',(29.9999999999998,-1.50000000000001,21.3125));
#67079=CARTESIAN_POINT('Origin',(30.,-1.32966554433622E-14,16.));
#67080=CARTESIAN_POINT('',(29.9999999999999,-1.50000000000001,20.75));
#67081=CARTESIAN_POINT('',(30.0000000238974,-1.50000000000001,20.8125000022995));
#67082=CARTESIAN_POINT('',(30.,-1.50000000000001,16.));
#67083=CARTESIAN_POINT('Ctrl Pts',(29.9999999999998,-1.50000000000001,20.75));
#67084=CARTESIAN_POINT('Ctrl Pts',(30.1355873378723,-1.50000000000003,20.7565234488349));
#67085=CARTESIAN_POINT('Ctrl Pts',(30.2707763371628,-1.48162130053548,20.7635382520255));
#67086=CARTESIAN_POINT('Ctrl Pts',(30.5905052894202,-1.39270558594719,20.7813910993741));
#67087=CARTESIAN_POINT('Ctrl Pts',(30.767029784006,-1.30383501600373,20.7923527650226));
#67088=CARTESIAN_POINT('Ctrl Pts',(31.0784013127494,-1.06141205266722,20.8140676058879));
#67089=CARTESIAN_POINT('Ctrl Pts',(31.2094059572181,-0.909300433903993,
20.8244833092276));
#67090=CARTESIAN_POINT('Ctrl Pts',(31.4005633760122,-0.569930140644686,
20.8433372144086));
#67091=CARTESIAN_POINT('Ctrl Pts',(31.4616108021312,-0.387386085525011,
20.8534785508042));
#67092=CARTESIAN_POINT('Ctrl Pts',(31.5130288281118,-0.00193915990322278,
20.8748922688942));
#67093=CARTESIAN_POINT('Ctrl Pts',(31.5000564049022,0.197728440072968,20.8859849133374));
#67094=CARTESIAN_POINT('Ctrl Pts',(31.3981909189968,0.576981524645895,20.907054529147));
#67095=CARTESIAN_POINT('Ctrl Pts',(31.3116775745975,0.753220156722293,20.9161479987326));
#67096=CARTESIAN_POINT('Ctrl Pts',(31.0770964939546,1.06165196611475,20.9360018364982));
#67097=CARTESIAN_POINT('Ctrl Pts',(30.9317342971964,1.19125838532521,20.946595756762));
#67098=CARTESIAN_POINT('Ctrl Pts',(30.5933406580028,1.39218994814601,20.9684581606193));
#67099=CARTESIAN_POINT('Ctrl Pts',(30.4020178812766,1.458987498605,20.9795186695191));
#67100=CARTESIAN_POINT('Ctrl Pts',(30.0144815741343,1.51197726610397,20.999635956776));
#67101=CARTESIAN_POINT('Ctrl Pts',(29.8225847199203,1.50160380579917,21.0084913464817));
#67102=CARTESIAN_POINT('Ctrl Pts',(29.4482673839794,1.40844186112423,21.0290885295006));
#67103=CARTESIAN_POINT('Ctrl Pts',(29.2698358143887,1.32475295725216,21.0399980141694));
#67104=CARTESIAN_POINT('Ctrl Pts',(28.9522277915389,1.09163995424434,21.0617542984881));
#67105=CARTESIAN_POINT('Ctrl Pts',(28.8169317835683,0.943334467611102,21.0723833275575));
#67106=CARTESIAN_POINT('Ctrl Pts',(28.6164713965323,0.609937924996611,21.0912889974983));
#67107=CARTESIAN_POINT('Ctrl Pts',(28.5503235834348,0.429720618453307,21.1011266323083));
#67108=CARTESIAN_POINT('Ctrl Pts',(28.4877747716401,0.0469249157698905,
21.1223930602351));
#67109=CARTESIAN_POINT('Ctrl Pts',(28.4947443957624,-0.152432728065059,
21.1334684848926));
#67110=CARTESIAN_POINT('Ctrl Pts',(28.585202717896,-0.535530466260377,21.1547516925701));
#67111=CARTESIAN_POINT('Ctrl Pts',(28.6672227696192,-0.715637129073743,
21.1640888680802));
#67112=CARTESIAN_POINT('Ctrl Pts',(28.8938150388557,-1.03121039122832,21.1837567176656));
#67113=CARTESIAN_POINT('Ctrl Pts',(29.0350964807726,-1.16446677665445,21.1942556904709));
#67114=CARTESIAN_POINT('Ctrl Pts',(29.3666683501557,-1.37437197910307,21.2160391495426));
#67115=CARTESIAN_POINT('Ctrl Pts',(29.5553884234738,-1.44649304249621,21.2271223111757));
#67116=CARTESIAN_POINT('Ctrl Pts',(29.8346137979128,-1.49316573714005,21.2418530120072));
#67117=CARTESIAN_POINT('Ctrl Pts',(29.917323692752,-1.50000000000001,21.2460222343129));
#67118=CARTESIAN_POINT('Ctrl Pts',(30.,-1.50000000000001,21.25));
#67119=CARTESIAN_POINT('Ctrl Pts',(29.9999999999998,-1.50000000000001,21.3125));
#67120=CARTESIAN_POINT('Ctrl Pts',(29.9681380540405,-1.50000000000001,21.3109670414103));
#67121=CARTESIAN_POINT('Ctrl Pts',(29.9362464291016,-1.4989848402199,21.3094044560071));
#67122=CARTESIAN_POINT('Ctrl Pts',(29.7059061051266,-1.48427038685078,21.2979134671869));
#67123=CARTESIAN_POINT('Ctrl Pts',(29.5119585810338,-1.43225099507769,21.2871371794785));
#67124=CARTESIAN_POINT('Ctrl Pts',(29.1596955105172,-1.25764065487782,21.2653386273684));
#67125=CARTESIAN_POINT('Ctrl Pts',(29.0039750821709,-1.13829559847059,21.2545313843106));
#67126=CARTESIAN_POINT('Ctrl Pts',(28.7485987477413,-0.848934521932683,
21.2342067770101));
#67127=CARTESIAN_POINT('Ctrl Pts',(28.6505388148689,-0.682384621723858,
21.2254102567623));
#67128=CARTESIAN_POINT('Ctrl Pts',(28.5196273945211,-0.313661198442873,
21.2049256221356));
#67129=CARTESIAN_POINT('Ctrl Pts',(28.4910680085409,-0.114008266472331,
21.1938337925817));
#67130=CARTESIAN_POINT('Ctrl Pts',(28.5133617159534,0.277152561451723,21.1721026354748));
#67131=CARTESIAN_POINT('Ctrl Pts',(28.5610406223868,0.465104578293146,21.1616608567614));
#67132=CARTESIAN_POINT('Ctrl Pts',(28.7268127368948,0.817191792877632,21.1421004559512));
#67133=CARTESIAN_POINT('Ctrl Pts',(28.8450160186508,0.977157792197407,21.1325925873729));
#67134=CARTESIAN_POINT('Ctrl Pts',(29.1366994431696,1.24242044599111,21.1111905550177));
#67135=CARTESIAN_POINT('Ctrl Pts',(29.3073536529405,1.34504122266248,21.1001293733922));
#67136=CARTESIAN_POINT('Ctrl Pts',(29.6718885684984,1.47596994041667,21.0789537702634));
#67137=CARTESIAN_POINT('Ctrl Pts',(29.8613546451375,1.5056180641301,21.0693266350828));
#67138=CARTESIAN_POINT('Ctrl Pts',(30.2499905035945,1.49232790599687,21.0502592125655));
#67139=CARTESIAN_POINT('Ctrl Pts',(30.4453612619354,1.44608660162569,21.0395749518952));
#67140=CARTESIAN_POINT('Ctrl Pts',(30.8031247707546,1.28178759217525,21.017798185678));
#67141=CARTESIAN_POINT('Ctrl Pts',(30.9627170127615,1.16669332668992,21.0069227374242));
#67142=CARTESIAN_POINT('Ctrl Pts',(31.2261252563514,0.884888124749317,20.9864215801195));
#67143=CARTESIAN_POINT('Ctrl Pts',(31.3286136134484,0.721936793997485,20.9776075996665));
#67144=CARTESIAN_POINT('Ctrl Pts',(31.4704956794702,0.357450862099888,20.9573583812278));
#67145=CARTESIAN_POINT('Ctrl Pts',(31.5050292215643,0.158114714869949,20.9462841508261));
#67146=CARTESIAN_POINT('Ctrl Pts',(31.4940038450927,-0.234658795010768,
20.9244634002772));
#67147=CARTESIAN_POINT('Ctrl Pts',(31.4515503117875,-0.4244189406881,20.9139211699618));
#67148=CARTESIAN_POINT('Ctrl Pts',(31.2960889353342,-0.779942120592769,
20.8941698821893));
#67149=CARTESIAN_POINT('Ctrl Pts',(31.1836334516182,-0.941901166431575,
20.8849503363697));
#67150=CARTESIAN_POINT('Ctrl Pts',(30.9011214218994,-1.21536636315781,20.8637617145378));
#67151=CARTESIAN_POINT('Ctrl Pts',(30.7331593249481,-1.323483412269,20.8526773830162));
#67152=CARTESIAN_POINT('Ctrl Pts',(30.374104697925,-1.46471715060753,20.8314791998208));
#67153=CARTESIAN_POINT('Ctrl Pts',(30.1878361111775,-1.49999999700053,20.821537269196));
#67154=CARTESIAN_POINT('Ctrl Pts',(30.0000000239529,-1.50000000000001,20.8125000011524));
#67155=CARTESIAN_POINT('Origin',(30.,-1.32966554433622E-14,16.));
#67156=CARTESIAN_POINT('',(29.9999999999999,-1.50000000000001,20.25));
#67157=CARTESIAN_POINT('',(30.0000000000001,-1.50000000000001,20.3125));
#67158=CARTESIAN_POINT('',(30.,-1.50000000000001,16.));
#67159=CARTESIAN_POINT('Ctrl Pts',(29.9999999999999,-1.50000000000001,20.25));
#67160=CARTESIAN_POINT('Ctrl Pts',(30.1641246040904,-1.50000000000003,20.257896448696));
#67161=CARTESIAN_POINT('Ctrl Pts',(30.3273129308388,-1.47306839847894,20.2664959507697));
#67162=CARTESIAN_POINT('Ctrl Pts',(30.6694540696788,-1.35668483193177,20.2861901008358));
#67163=CARTESIAN_POINT('Ctrl Pts',(30.8415535621189,-1.25719932144175,20.2972337279289));
#67164=CARTESIAN_POINT('Ctrl Pts',(31.1383891848058,-0.996648092240175,
20.3187527726287));
#67165=CARTESIAN_POINT('Ctrl Pts',(31.2598762410215,-0.837810488997904,
20.3284549728335));
#67166=CARTESIAN_POINT('Ctrl Pts',(31.4314249865634,-0.487683998530185,
20.3479064445261));
#67167=CARTESIAN_POINT('Ctrl Pts',(31.4819950779928,-0.300804420279551,
20.3582886433178));
#67168=CARTESIAN_POINT('Ctrl Pts',(31.5105507066295,0.0893179172321859,
20.3799621065129));
#67169=CARTESIAN_POINT('Ctrl Pts',(31.4853246402279,0.289072829407564,20.3910596016338));
#67170=CARTESIAN_POINT('Ctrl Pts',(31.3605672791737,0.660112394093701,20.411672910783));
#67171=CARTESIAN_POINT('Ctrl Pts',(31.2649722312571,0.828695575895264,20.4204916500332));
#67172=CARTESIAN_POINT('Ctrl Pts',(31.0140581775355,1.12220790918685,20.4407168784407));
#67173=CARTESIAN_POINT('Ctrl Pts',(30.8605226301063,1.24384616367647,20.4514827013131));
#67174=CARTESIAN_POINT('Ctrl Pts',(30.5114243415045,1.42407146100134,20.4732849588136));
#67175=CARTESIAN_POINT('Ctrl Pts',(30.3183380047095,1.47926213924964,20.4841079039198));
#67176=CARTESIAN_POINT('Ctrl Pts',(29.9307960888716,1.51038882263748,20.5036181531332));
#67177=CARTESIAN_POINT('Ctrl Pts',(29.7403288665302,1.48951380456358,20.5127847164407));
#67178=CARTESIAN_POINT('Ctrl Pts',(29.3711639835748,1.37589985350485,20.5337021132381));
#67179=CARTESIAN_POINT('Ctrl Pts',(29.1966946677341,1.28188655628153,20.5447077525887));
#67180=CARTESIAN_POINT('Ctrl Pts',(28.8909965958092,1.02962579258236,20.5664229013678));
#67181=CARTESIAN_POINT('Ctrl Pts',(28.7637626025144,0.872753791453066,20.5765136782526));
#67182=CARTESIAN_POINT('Ctrl Pts',(28.582295287402,0.526054660802727,20.5957747410665));
#67183=CARTESIAN_POINT('Ctrl Pts',(28.5268265400693,0.341112810094873,20.6060492883281));
#67184=CARTESIAN_POINT('Ctrl Pts',(28.4876154625531,-0.0470049788678421,
20.6276113877149));
#67185=CARTESIAN_POINT('Ctrl Pts',(28.5071470207889,-0.246809925970759,
20.6387116625539));
#67186=CARTESIAN_POINT('Ctrl Pts',(28.6213243381125,-0.621726643029005,
20.6595403690571));
#67187=CARTESIAN_POINT('Ctrl Pts',(28.7127069454602,-0.793828860292424,
20.6684492190444));
#67188=CARTESIAN_POINT('Ctrl Pts',(28.9560213000323,-1.09433750409046,20.6885031487146));
#67189=CARTESIAN_POINT('Ctrl Pts',(29.1057854975977,-1.21976733917156,20.6991928441151));
#67190=CARTESIAN_POINT('Ctrl Pts',(29.4493247586543,-1.40936219023255,20.7209879081598));
#67191=CARTESIAN_POINT('Ctrl Pts',(29.6408325610402,-1.46988527163767,20.7318830283038));
#67192=CARTESIAN_POINT('Ctrl Pts',(29.8922912775479,-1.4971028845898,20.7447373862468));
#67193=CARTESIAN_POINT('Ctrl Pts',(29.9461731363168,-1.50000000000001,20.7474102538136));
#67194=CARTESIAN_POINT('Ctrl Pts',(29.9999999999998,-1.50000000000001,20.75));
#67195=CARTESIAN_POINT('Ctrl Pts',(30.0000000239529,-1.50000000000001,20.8125000011524));
#67196=CARTESIAN_POINT('Ctrl Pts',(29.9974904007656,-1.50000000004009,20.8123792568517));
#67197=CARTESIAN_POINT('Ctrl Pts',(29.994980514477,-1.49999370187214,20.8122583249421));
#67198=CARTESIAN_POINT('Ctrl Pts',(29.7936662704942,-1.49898314378545,20.8025445178046));
#67199=CARTESIAN_POINT('Ctrl Pts',(29.5970666373285,-1.45847246315053,20.7919603168594));
#67200=CARTESIAN_POINT('Ctrl Pts',(29.2341811004286,-1.30450218441903,20.7702240261379));
#67201=CARTESIAN_POINT('Ctrl Pts',(29.0708854167951,-1.19371554978206,20.7592900523783));
#67202=CARTESIAN_POINT('Ctrl Pts',(28.7996246113049,-0.919409908918738,
20.738619409654));
#67203=CARTESIAN_POINT('Ctrl Pts',(28.6928036628702,-0.759898893507146,
20.7297166051949));
#67204=CARTESIAN_POINT('Ctrl Pts',(28.540323338491,-0.399638425423168,20.7097021347457));
#67205=CARTESIAN_POINT('Ctrl Pts',(28.4999872115666,-0.200774562873281,
20.6986541423819));
#67206=CARTESIAN_POINT('Ctrl Pts',(28.5000123038317,0.193260173251348,20.6767633237083));
#67207=CARTESIAN_POINT('Ctrl Pts',(28.5373370740434,0.384636586987589,20.6661313007229));
#67208=CARTESIAN_POINT('Ctrl Pts',(28.6828216865171,0.743407395273799,20.6461995891515));
#67209=CARTESIAN_POINT('Ctrl Pts',(28.7898502936129,0.90727948583588,20.637187813622));
#67210=CARTESIAN_POINT('Ctrl Pts',(29.0635269308615,1.18843769395866,20.6162105900475));
#67211=CARTESIAN_POINT('Ctrl Pts',(29.228755223573,1.30174519776628,20.6051136094466));
#67212=CARTESIAN_POINT('Ctrl Pts',(29.5868470804747,1.45456710532649,20.5836398539607));
#67213=CARTESIAN_POINT('Ctrl Pts',(29.7752048690842,1.49530975495507,20.5734457453635));
#67214=CARTESIAN_POINT('Ctrl Pts',(30.1648759814307,1.50410182396658,20.5544534610902));
#67215=CARTESIAN_POINT('Ctrl Pts',(30.3625681263815,1.46904639647318,20.544196110566));
#67216=CARTESIAN_POINT('Ctrl Pts',(30.7301648562918,1.32486538129436,20.5225050764527));
#67217=CARTESIAN_POINT('Ctrl Pts',(30.8968384149473,1.21823387618242,20.5115240048699));
#67218=CARTESIAN_POINT('Ctrl Pts',(31.1754315899033,0.951036194862134,20.4906980266758));
#67219=CARTESIAN_POINT('Ctrl Pts',(31.2863099173977,0.794671992670377,20.4816484440372));
#67220=CARTESIAN_POINT('Ctrl Pts',(31.4475104523221,0.440765387920731,20.4619869659956));
#67221=CARTESIAN_POINT('Ctrl Pts',(31.4931266838049,0.245180433281527,20.4511211351823));
#67222=CARTESIAN_POINT('Ctrl Pts',(31.505277935416,-0.147222207316758,20.4293209884824));
#67223=CARTESIAN_POINT('Ctrl Pts',(31.4737006088925,-0.340229130529765,
20.4185983816372));
#67224=CARTESIAN_POINT('Ctrl Pts',(31.339252899941,-0.702504700740186,20.39847196107));
#67225=CARTESIAN_POINT('Ctrl Pts',(31.2380795698328,-0.868488363198902,
20.3896091209879));
#67226=CARTESIAN_POINT('Ctrl Pts',(30.9741217873874,-1.15788922779948,20.3688705333532));
#67227=CARTESIAN_POINT('Ctrl Pts',(30.8120536546578,-1.27678494801521,20.3577703677868));
#67228=CARTESIAN_POINT('Ctrl Pts',(30.4578087067642,-1.44121172280179,20.3361593393739));
#67229=CARTESIAN_POINT('Ctrl Pts',(30.2702179556352,-1.48784534045563,20.3258384968839));
#67230=CARTESIAN_POINT('Ctrl Pts',(30.052598998323,-1.49930896382792,20.3150498659359));
#67231=CARTESIAN_POINT('Ctrl Pts',(30.0262877690999,-1.50000000000001,20.3137647708805));
#67232=CARTESIAN_POINT('Ctrl Pts',(30.0000000000001,-1.50000000000001,20.3125));
#67233=CARTESIAN_POINT('Origin',(30.,-1.32966554433622E-14,16.));
#67234=CARTESIAN_POINT('',(29.9999999508795,-1.50000000000001,19.7499999952734));
#67235=CARTESIAN_POINT('',(30.0000000000001,-1.50000000000001,19.8125));
#67236=CARTESIAN_POINT('',(30.,-1.50000000000001,16.));
#67237=CARTESIAN_POINT('Ctrl Pts',(29.9999999507652,-1.50000000000001,19.7499999976312));
#67238=CARTESIAN_POINT('Ctrl Pts',(30.0036354883629,-1.50000000011934,19.7501749125187));
#67239=CARTESIAN_POINT('Ctrl Pts',(30.007271600744,-1.4999867831078,19.7503502221899));
#67240=CARTESIAN_POINT('Ctrl Pts',(30.201622915749,-1.49857339489822,19.7597402149765));
#67241=CARTESIAN_POINT('Ctrl Pts',(30.3903004853368,-1.46082693625102,19.769866481516));
#67242=CARTESIAN_POINT('Ctrl Pts',(30.7502056783764,-1.31393443624912,19.7912627754119));
#67243=CARTESIAN_POINT('Ctrl Pts',(30.9169691324023,-1.2034971179945,19.8023538891195));
#67244=CARTESIAN_POINT('Ctrl Pts',(31.1955532827852,-0.926587489668503,
19.8234492094243));
#67245=CARTESIAN_POINT('Ctrl Pts',(31.305583357368,-0.763777918932018,19.8325678933928));
#67246=CARTESIAN_POINT('Ctrl Pts',(31.4566154175894,-0.406803589900389,
19.8523998005612));
#67247=CARTESIAN_POINT('Ctrl Pts',(31.4968003232487,-0.216309448389897,
19.8629828084229));
#67248=CARTESIAN_POINT('Ctrl Pts',(31.5029527191874,0.177060648076386,19.884836702671));
#67249=CARTESIAN_POINT('Ctrl Pts',(31.4658451495388,0.376207311237188,19.8959004061799));
#67250=CARTESIAN_POINT('Ctrl Pts',(31.3192558360179,0.738832237635632,19.9160462354243));
#67251=CARTESIAN_POINT('Ctrl Pts',(31.2148503942445,0.900251242918639,19.9248907954582));
#67252=CARTESIAN_POINT('Ctrl Pts',(30.9479657510409,1.17875033469753,19.9454673747239));
#67253=CARTESIAN_POINT('Ctrl Pts',(30.7867234803792,1.29195591113542,19.9563697464337));
#67254=CARTESIAN_POINT('Ctrl Pts',(30.4266603329508,1.45171184585212,19.9781309575447));
#67255=CARTESIAN_POINT('Ctrl Pts',(30.2307253625385,1.49542562590392,19.9887721548721));
#67256=CARTESIAN_POINT('Ctrl Pts',(29.8418323593176,1.50370934578551,20.0077128815434));
#67257=CARTESIAN_POINT('Ctrl Pts',(29.6526184508184,1.47157346290215,20.0175030286082));
#67258=CARTESIAN_POINT('Ctrl Pts',(29.2894512067405,1.33570909972092,20.038749930874));
#67259=CARTESIAN_POINT('Ctrl Pts',(29.1199599079427,1.2306626568369,20.0498225415362));
#67260=CARTESIAN_POINT('Ctrl Pts',(28.8323016398048,0.961771765690436,20.0711316978356));
#67261=CARTESIAN_POINT('Ctrl Pts',(28.7166359490173,0.80092922531751,20.0805039319268));
#67262=CARTESIAN_POINT('Ctrl Pts',(28.5553841103709,0.447325657819572,20.1001485745656));
#67263=CARTESIAN_POINT('Ctrl Pts',(28.5099861175222,0.258564005548656,20.1106353330251));
#67264=CARTESIAN_POINT('Ctrl Pts',(28.4926188058233,-0.133342134639988,
20.1324078963689));
#67265=CARTESIAN_POINT('Ctrl Pts',(28.5237938243712,-0.332877530953282,
20.1434931961641));
#67266=CARTESIAN_POINT('Ctrl Pts',(28.6595170927538,-0.699759711689848,
20.1638755395383));
#67267=CARTESIAN_POINT('Ctrl Pts',(28.759513047986,-0.864726488741114,20.1726705572702));
#67268=CARTESIAN_POINT('Ctrl Pts',(29.0184002150316,-1.15079879551533,20.1930727248681));
#67269=CARTESIAN_POINT('Ctrl Pts',(29.1758229214277,-1.26830528519454,20.2039107975187));
#67270=CARTESIAN_POINT('Ctrl Pts',(29.5305217931358,-1.4384406773805,20.2257022380569));
#67271=CARTESIAN_POINT('Ctrl Pts',(29.7251117157194,-1.4879453135066,20.2364395788536));
#67272=CARTESIAN_POINT('Ctrl Pts',(29.9491466954872,-1.49935402178859,20.2475353754067));
#67273=CARTESIAN_POINT('Ctrl Pts',(29.9745837219083,-1.50000000000001,20.2487771587502));
#67274=CARTESIAN_POINT('Ctrl Pts',(29.9999999999999,-1.50000000000001,20.25));
#67275=CARTESIAN_POINT('Ctrl Pts',(30.0000000000001,-1.50000000000001,20.3125));
#67276=CARTESIAN_POINT('Ctrl Pts',(29.8275998140085,-1.50000000000001,20.3042053921841));
#67277=CARTESIAN_POINT('Ctrl Pts',(29.6562870357889,-1.47028352574469,20.2951376446808));
#67278=CARTESIAN_POINT('Ctrl Pts',(29.3085931862514,-1.34558031058123,20.2749452383464));
#67279=CARTESIAN_POINT('Ctrl Pts',(29.1384186293223,-1.24350663328035,20.2639223312337));
#67280=CARTESIAN_POINT('Ctrl Pts',(28.8520258822514,-0.983987574399218,
20.242934391019));
#67281=CARTESIAN_POINT('Ctrl Pts',(28.7368098691781,-0.830906588856551,
20.2336614771587));
#67282=CARTESIAN_POINT('Ctrl Pts',(28.5656483010559,-0.481857271883387,
20.214269848438));
#67283=CARTESIAN_POINT('Ctrl Pts',(28.5144799811963,-0.287679235979695,
20.2034821797766));
#67284=CARTESIAN_POINT('Ctrl Pts',(28.4911007681834,0.104720249591022,20.181682208356));
#67285=CARTESIAN_POINT('Ctrl Pts',(28.5173310962609,0.299077411990059,20.1708845882228));
#67286=CARTESIAN_POINT('Ctrl Pts',(28.6416246239434,0.664496311411631,20.1505835382549));
#67287=CARTESIAN_POINT('Ctrl Pts',(28.7375408574377,0.832427515421977,20.1417837739438));
#67288=CARTESIAN_POINT('Ctrl Pts',(28.9926175512114,1.12917452204563,20.1212684183864));
#67289=CARTESIAN_POINT('Ctrl Pts',(29.1516633795811,1.2530630770023,20.1101749736523));
#67290=CARTESIAN_POINT('Ctrl Pts',(29.5021040725661,1.42792836972927,20.0884570187074));
#67291=CARTESIAN_POINT('Ctrl Pts',(29.6888418601191,1.47989191267207,20.0780291609664));
#67292=CARTESIAN_POINT('Ctrl Pts',(30.0769287467939,1.5109546306831,20.0584944686474));
#67293=CARTESIAN_POINT('Ctrl Pts',(30.2747213678695,1.48776626200004,20.0489426359701));
#67294=CARTESIAN_POINT('Ctrl Pts',(30.6499367323256,1.36617967610523,20.027512673167));
#67295=CARTESIAN_POINT('Ctrl Pts',(30.8236685705517,1.26902858360925,20.0164553547449));
#67296=CARTESIAN_POINT('Ctrl Pts',(31.1182297704941,1.01768973269335,19.9953016376572));
#67297=CARTESIAN_POINT('Ctrl Pts',(31.2380227260335,0.867983838688731,19.9857213243715));
#67298=CARTESIAN_POINT('Ctrl Pts',(31.4194655172301,0.52407745893419,19.9666154143852));
#67299=CARTESIAN_POINT('Ctrl Pts',(31.4763477416476,0.331530482038543,19.9559183601132));
#67300=CARTESIAN_POINT('Ctrl Pts',(31.5113890098208,-0.0605236259430762,
19.9341375763365));
#67301=CARTESIAN_POINT('Ctrl Pts',(31.4907606610887,-0.256127601642152,
19.9232706887976));
#67302=CARTESIAN_POINT('Ctrl Pts',(31.3770092904839,-0.62473058770716,19.9027927451274));
#67303=CARTESIAN_POINT('Ctrl Pts',(31.2864311739689,-0.794691675228615,
19.8939853466257));
#67304=CARTESIAN_POINT('Ctrl Pts',(31.0405043429371,-1.09883901947073,19.8737046491109));
#67305=CARTESIAN_POINT('Ctrl Pts',(30.8847013390568,-1.22775605549742,19.8626275448131));
#67306=CARTESIAN_POINT('Ctrl Pts',(30.5384592288504,-1.41320441242881,19.8408176202706));
#67307=CARTESIAN_POINT('Ctrl Pts',(30.3527481344157,-1.47060245170435,19.8302882010938));
#67308=CARTESIAN_POINT('Ctrl Pts',(30.1075898199807,-1.49710947656403,19.8177567099449));
#67309=CARTESIAN_POINT('Ctrl Pts',(30.0537655536404,-1.50000000000001,19.8150867964056));
#67310=CARTESIAN_POINT('Ctrl Pts',(30.0000000000003,-1.50000000000001,19.8125));
#67311=CARTESIAN_POINT('Origin',(30.,-1.32966554433622E-14,16.));
#67312=CARTESIAN_POINT('',(30.0000000000001,-1.50000000000001,19.25));
#67313=CARTESIAN_POINT('',(30.,-1.50000000000001,19.3125));
#67314=CARTESIAN_POINT('',(30.,-1.50000000000001,16.));
#67315=CARTESIAN_POINT('Ctrl Pts',(30.0000000000001,-1.50000000000001,19.25));
#67316=CARTESIAN_POINT('Ctrl Pts',(30.0322695745912,-1.50000000000001,19.2515525706314));
#67317=CARTESIAN_POINT('Ctrl Pts',(30.0645714825038,-1.49895869986435,19.2531356219044));
#67318=CARTESIAN_POINT('Ctrl Pts',(30.2882590679586,-1.48448482383795,19.2642998479893));
#67319=CARTESIAN_POINT('Ctrl Pts',(30.4754930135539,-1.43550485550641,19.2746687000727));
#67320=CARTESIAN_POINT('Ctrl Pts',(30.8281012978914,-1.26647563555772,19.2963288301724));
#67321=CARTESIAN_POINT('Ctrl Pts',(30.9888581275123,-1.14537453755813,19.3074271661326));
#67322=CARTESIAN_POINT('Ctrl Pts',(31.2489169787693,-0.852727854965852,
19.328068327964));
#67323=CARTESIAN_POINT('Ctrl Pts',(31.3477723438117,-0.685891580063111,
19.3368949122188));
#67324=CARTESIAN_POINT('Ctrl Pts',(31.4777710225729,-0.322229436301838,
19.35709836465));
#67325=CARTESIAN_POINT('Ctrl Pts',(31.5070120496637,-0.128613045958812,
19.3678548307802));
#67326=CARTESIAN_POINT('Ctrl Pts',(31.4899431617665,0.263827999699887,19.3896571110945));
#67327=CARTESIAN_POINT('Ctrl Pts',(31.4418890858574,0.458816520684437,19.4004898067048));
#67328=CARTESIAN_POINT('Ctrl Pts',(31.2763170645903,0.810606892156535,19.420033716231));
#67329=CARTESIAN_POINT('Ctrl Pts',(31.1635461572557,0.965528328551652,19.4291724240899));
#67330=CARTESIAN_POINT('Ctrl Pts',(30.8815440072885,1.22938524433353,19.4500696176279));
#67331=CARTESIAN_POINT('Ctrl Pts',(30.713328176096,1.33404197013925,19.4610700368521));
#67332=CARTESIAN_POINT('Ctrl Pts',(30.3423586225268,1.47407873960012,19.4828082280827));
#67333=CARTESIAN_POINT('Ctrl Pts',(30.1427440803289,1.50655371354715,19.4929501746347));
#67334=CARTESIAN_POINT('Ctrl Pts',(29.7515262729803,1.4915957790601,19.5121881483469));
#67335=CARTESIAN_POINT('Ctrl Pts',(29.563545020268,1.44778515274356,19.522449362427));
#67336=CARTESIAN_POINT('Ctrl Pts',(29.2074099124303,1.28891068317319,19.5439971005021));
#67337=CARTESIAN_POINT('Ctrl Pts',(29.0438038910602,1.17268375630169,19.5550971246218));
#67338=CARTESIAN_POINT('Ctrl Pts',(28.7751767012687,0.88721540741588,19.5759511326745));
#67339=CARTESIAN_POINT('Ctrl Pts',(28.6712044325382,0.722248138115754,19.5848751034381));
#67340=CARTESIAN_POINT('Ctrl Pts',(28.5314450700553,0.361647735614998,19.6049084591326));
#67341=CARTESIAN_POINT('Ctrl Pts',(28.4970926988021,0.169404578017586,19.6155886345547));
#67342=CARTESIAN_POINT('Ctrl Pts',(28.5033789257342,-0.222871075081128,
19.6373817263935));
#67343=CARTESIAN_POINT('Ctrl Pts',(28.5460751647458,-0.419126971559099,
19.6482848317533));
#67344=CARTESIAN_POINT('Ctrl Pts',(28.7020419000445,-0.77553505760853,19.6680852809783));
#67345=CARTESIAN_POINT('Ctrl Pts',(28.8106757232385,-0.933630997355151,
19.6770461367592));
#67346=CARTESIAN_POINT('Ctrl Pts',(29.0852161697017,-1.20477024704427,19.697786615973));
#67347=CARTESIAN_POINT('Ctrl Pts',(29.2500326897204,-1.31371406923191,19.7087425717726));
#67348=CARTESIAN_POINT('Ctrl Pts',(29.611734771314,-1.46197087611401,19.7302632159228));
#67349=CARTESIAN_POINT('Ctrl Pts',(29.8049901134984,-1.49999999359916,19.7406175822833));
#67350=CARTESIAN_POINT('Ctrl Pts',(29.9999999507652,-1.50000000000001,19.7499999976312));
#67351=CARTESIAN_POINT('Ctrl Pts',(30.0000000000003,-1.50000000000001,19.8125));
#67352=CARTESIAN_POINT('Ctrl Pts',(29.8589500630315,-1.50000000000001,19.8057137317435));
#67353=CARTESIAN_POINT('Ctrl Pts',(29.7183576297039,-1.48011045726929,19.7983969878431));
#67354=CARTESIAN_POINT('Ctrl Pts',(29.392433533781,-1.38562863633522,19.7800914624408));
#67355=CARTESIAN_POINT('Ctrl Pts',(29.2152602016442,-1.29355450601908,19.7690095917929));
#67356=CARTESIAN_POINT('Ctrl Pts',(28.9125224323809,-1.05055621120639,19.7476941614444));
#67357=CARTESIAN_POINT('Ctrl Pts',(28.7881027470448,-0.904173072558181,
19.7377318373643));
#67358=CARTESIAN_POINT('Ctrl Pts',(28.5965141205021,-0.565467385757126,
19.7189148547643));
#67359=CARTESIAN_POINT('Ctrl Pts',(28.5340212729776,-0.374707579896709,
19.708317087772));
#67360=CARTESIAN_POINT('Ctrl Pts',(28.4874198303467,0.0166598622973653,
19.6865744520946));
#67361=CARTESIAN_POINT('Ctrl Pts',(28.5024461232084,0.213342923270549,19.6756476153738));
#67362=CARTESIAN_POINT('Ctrl Pts',(28.605730933148,0.585021358101511,19.6549988134388));
#67363=CARTESIAN_POINT('Ctrl Pts',(28.6911262279336,0.757019946925095,19.6461115535275));
#67364=CARTESIAN_POINT('Ctrl Pts',(28.9280450078188,1.06829223859541,19.6260663408692));
#67365=CARTESIAN_POINT('Ctrl Pts',(29.0805347242822,1.20204064727676,19.6150144423906));
#67366=CARTESIAN_POINT('Ctrl Pts',(29.4223784266326,1.3977266885599,19.5931317562239));
#67367=CARTESIAN_POINT('Ctrl Pts',(29.6069366918152,1.46041214264913,19.5825109299366));
#67368=CARTESIAN_POINT('Ctrl Pts',(29.9906687655378,1.51247863508202,19.562602320475));
#67369=CARTESIAN_POINT('Ctrl Pts',(30.1862339040192,1.50100007477566,19.55356759697));
#67370=CARTESIAN_POINT('Ctrl Pts',(30.5662821795392,1.40308967236277,19.5325627823883));
#67371=CARTESIAN_POINT('Ctrl Pts',(30.7466285872712,1.31600734425417,19.5214669082421));
#67372=CARTESIAN_POINT('Ctrl Pts',(31.0570470506688,1.08124306107491,19.5000106628701));
#67373=CARTESIAN_POINT('Ctrl Pts',(31.185947420448,0.938076365153711,19.4898320882731));
#67374=CARTESIAN_POINT('Ctrl Pts',(31.387173884418,0.604359282145194,19.4708806565388));
#67375=CARTESIAN_POINT('Ctrl Pts',(31.4549913450499,0.415392173173207,19.460577342954));
#67376=CARTESIAN_POINT('Ctrl Pts',(31.5125364736871,0.0248207245632997,
19.4388789291423));
#67377=CARTESIAN_POINT('Ctrl Pts',(31.5028468405333,-0.172737498474235,
19.4279034723069));
#67378=CARTESIAN_POINT('Ctrl Pts',(31.4094808313587,-0.547250043493136,
19.4070972198059));
#67379=CARTESIAN_POINT('Ctrl Pts',(31.3288984144444,-0.721204660777261,
19.3980698586427));
#67380=CARTESIAN_POINT('Ctrl Pts',(31.1018991125715,-1.03700530321776,19.3783761095713));
#67381=CARTESIAN_POINT('Ctrl Pts',(30.9548507096631,-1.17379817492847,19.3675014379958));
#67382=CARTESIAN_POINT('Ctrl Pts',(30.6204358823266,-1.37933694163779,19.3457024869274));
#67383=CARTESIAN_POINT('Ctrl Pts',(30.4373267027344,-1.44785012953098,19.3349894983086));
#67384=CARTESIAN_POINT('Ctrl Pts',(30.1646733538461,-1.49322482781476,19.3206110496582));
#67385=CARTESIAN_POINT('Ctrl Pts',(30.0823180279059,-1.50000000000001,19.3164605279642));
#67386=CARTESIAN_POINT('Ctrl Pts',(30.,-1.50000000000001,19.3125));
#67387=CARTESIAN_POINT('Origin',(30.,-1.32966554433622E-14,16.));
#67388=CARTESIAN_POINT('',(30.0000000000001,-1.50000000000001,18.75));
#67389=CARTESIAN_POINT('',(30.,-1.50000000000001,18.8125));
#67390=CARTESIAN_POINT('',(30.,-1.50000000000001,16.));
#67391=CARTESIAN_POINT('Ctrl Pts',(30.0000000000002,-1.50000000000001,18.75));
#67392=CARTESIAN_POINT('Ctrl Pts',(30.0598815861698,-1.50000000000001,18.7528810541579));
#67393=CARTESIAN_POINT('Ctrl Pts',(30.1198247627216,-1.4964145214846,18.7558646682098));
#67394=CARTESIAN_POINT('Ctrl Pts',(30.3709807388755,-1.46613984657296,18.7687893789386));
#67395=CARTESIAN_POINT('Ctrl Pts',(30.5561899070999,-1.40635296128044,18.7793610060131));
#67396=CARTESIAN_POINT('Ctrl Pts',(30.9004833554958,-1.21627199481911,18.8012058591186));
#67397=CARTESIAN_POINT('Ctrl Pts',(31.054808880873,-1.08516465668695,18.8122727199239));
#67398=CARTESIAN_POINT('Ctrl Pts',(31.2966795386424,-0.777790002612556,
18.832447912207));
#67399=CARTESIAN_POINT('Ctrl Pts',(31.3849156897549,-0.606916752329299,
18.8412824026485));
#67400=CARTESIAN_POINT('Ctrl Pts',(31.4939654845851,-0.236921615045211,
18.8618376880532));
#67401=CARTESIAN_POINT('Ctrl Pts',(31.5120817444602,-0.0408132290769898,
18.8727325983848));
#67402=CARTESIAN_POINT('Ctrl Pts',(31.4718441015158,0.350974679810523,18.8944985933229));
#67403=CARTESIAN_POINT('Ctrl Pts',(31.4124332725198,0.54273929222595,18.9051521829016));
#67404=CARTESIAN_POINT('Ctrl Pts',(31.2264254338517,0.884320880490274,18.9241289378051));
#67405=CARTESIAN_POINT('Ctrl Pts',(31.1045648671413,1.03253115218655,18.9338713522791));
#67406=CARTESIAN_POINT('Ctrl Pts',(30.8063387149155,1.2801510812434,18.9550980960807));
#67407=CARTESIAN_POINT('Ctrl Pts',(30.6310491381331,1.37504484021148,18.9661676575249));
#67408=CARTESIAN_POINT('Ctrl Pts',(30.2546711108962,1.4912245976519,18.9875033692879));
#67409=CARTESIAN_POINT('Ctrl Pts',(30.05740041095,1.51172051693628,18.9969127515258));
#67410=CARTESIAN_POINT('Ctrl Pts',(29.6702738320324,1.47589654334487,19.0165334981157));
#67411=CARTESIAN_POINT('Ctrl Pts',(29.4839742576828,1.42150925053353,19.0270075986994));
#67412=CARTESIAN_POINT('Ctrl Pts',(29.1353660189379,1.24191643228194,19.048768709802));
#67413=CARTESIAN_POINT('Ctrl Pts',(28.9777462443354,1.1157773991078,19.059856056776));
#67414=CARTESIAN_POINT('Ctrl Pts',(28.7267374929236,0.815719209989595,19.0802676706567));
#67415=CARTESIAN_POINT('Ctrl Pts',(28.6332044534767,0.64688991790973,19.0890616712273));
#67416=CARTESIAN_POINT('Ctrl Pts',(28.5135873974093,0.280047942578678,19.109441780968));
#67417=CARTESIAN_POINT('Ctrl Pts',(28.4898364137009,0.0851180238092936,
19.1202712208996));
#67418=CARTESIAN_POINT('Ctrl Pts',(28.5183897482981,-0.307171243363851,
19.1420650690759));
#67419=CARTESIAN_POINT('Ctrl Pts',(28.5720998196786,-0.500646940480604,
19.1528137189157));
#67420=CARTESIAN_POINT('Ctrl Pts',(28.747829861517,-0.847427013151625,19.1720792785085));
#67421=CARTESIAN_POINT('Ctrl Pts',(28.8650664758991,-0.999006868470888,
19.1814790094866));
#67422=CARTESIAN_POINT('Ctrl Pts',(29.1550741400796,-1.25492382568339,19.2025408141021));
#67423=CARTESIAN_POINT('Ctrl Pts',(29.3268372187205,-1.35483766663846,19.2135801535473));
#67424=CARTESIAN_POINT('Ctrl Pts',(29.6699517271029,-1.47262040644266,19.2333600008011));
#67425=CARTESIAN_POINT('Ctrl Pts',(29.8345144389513,-1.50000000000001,19.2420380722318));
#67426=CARTESIAN_POINT('Ctrl Pts',(30.0000000000001,-1.50000000000001,19.25));
#67427=CARTESIAN_POINT('Ctrl Pts',(30.,-1.50000000000001,19.3125));
#67428=CARTESIAN_POINT('Ctrl Pts',(29.8904115959066,-1.50000000000001,19.3072274254497));
#67429=CARTESIAN_POINT('Ctrl Pts',(29.7809217474217,-1.48799325955223,19.3016260720903));
#67430=CARTESIAN_POINT('Ctrl Pts',(29.479267613868,-1.42071467340943,19.2852438812078));
#67431=CARTESIAN_POINT('Ctrl Pts',(29.2956191224553,-1.33919024824593,19.2741435216794));
#67432=CARTESIAN_POINT('Ctrl Pts',(28.9769843310201,-1.11359538988626,19.2525466742853));
#67433=CARTESIAN_POINT('Ctrl Pts',(28.8433197059369,-0.97404728751911,19.2422393958357));
#67434=CARTESIAN_POINT('Ctrl Pts',(28.6314369352188,-0.64558462894177,19.2229212185382));
#67435=CARTESIAN_POINT('Ctrl Pts',(28.5578261508896,-0.458159789494097,
19.2129533216385));
#67436=CARTESIAN_POINT('Ctrl Pts',(28.4887314396478,-0.0683254796838233,
19.1912958599824));
#67437=CARTESIAN_POINT('Ctrl Pts',(28.4927829468086,0.129998312926432,19.180277871504));
#67438=CARTESIAN_POINT('Ctrl Pts',(28.5757061903925,0.507408017565263,19.1593106656908));
#67439=CARTESIAN_POINT('Ctrl Pts',(28.6513157241137,0.683452060166118,19.1500704896955));
#67440=CARTESIAN_POINT('Ctrl Pts',(28.8692063981292,1.00541452618758,19.1306438179201));
#67441=CARTESIAN_POINT('Ctrl Pts',(29.0123062748592,1.14629480240063,19.119845580885));
#67442=CARTESIAN_POINT('Ctrl Pts',(29.3411837772215,1.36149831072911,19.0980445794436));
#67443=CARTESIAN_POINT('Ctrl Pts',(29.5228193452006,1.43527924918368,19.0872561635921));
#67444=CARTESIAN_POINT('Ctrl Pts',(29.9017346505858,1.50901487689319,19.0669773805809));
#67445=CARTESIAN_POINT('Ctrl Pts',(30.095243866884,1.50920856983617,19.0581733709244));
#67446=CARTESIAN_POINT('Ctrl Pts',(30.4795337547919,1.43522535350299,19.0376291257293));
#67447=CARTESIAN_POINT('Ctrl Pts',(30.6659951148259,1.35877256279477,19.0265343107311));
#67448=CARTESIAN_POINT('Ctrl Pts',(30.9917525251624,1.14161337833726,19.0048291004505));
#67449=CARTESIAN_POINT('Ctrl Pts',(31.12959203788,1.00543319777699,18.9944145110095));
#67450=CARTESIAN_POINT('Ctrl Pts',(31.3495099297643,0.683969951441068,18.9749041718824));
#67451=CARTESIAN_POINT('Ctrl Pts',(31.4277388995994,0.500572833869038,18.9653096018815));
#67452=CARTESIAN_POINT('Ctrl Pts',(31.5085610210805,0.114360476914036,18.9438533598284));
#67453=CARTESIAN_POINT('Ctrl Pts',(31.510521839189,-0.0846024989690804,
18.9327998611683));
#67454=CARTESIAN_POINT('Ctrl Pts',(31.4387139095947,-0.464995267712227,
18.9116669295714));
#67455=CARTESIAN_POINT('Ctrl Pts',(31.3683024334794,-0.643299822803022,
18.9021297086694));
#67456=CARTESIAN_POINT('Ctrl Pts',(31.1599775839064,-0.97159308723095,18.8829874173259));
#67457=CARTESIAN_POINT('Ctrl Pts',(31.021122395481,-1.11661364586043,18.8722783951071));
#67458=CARTESIAN_POINT('Ctrl Pts',(30.6983237124874,-1.34174379218127,18.8504941210548));
#67459=CARTESIAN_POINT('Ctrl Pts',(30.5183853004494,-1.42099198981035,18.8396354913461));
#67460=CARTESIAN_POINT('Ctrl Pts',(30.220307982392,-1.48785706899676,18.8234368763837));
#67461=CARTESIAN_POINT('Ctrl Pts',(30.1102084329115,-1.50000000000001,18.8178024057007));
#67462=CARTESIAN_POINT('Ctrl Pts',(30.,-1.50000000000001,18.8125));
#67463=CARTESIAN_POINT('Origin',(30.,-1.32966554433622E-14,16.));
#67464=CARTESIAN_POINT('',(30.,-1.50000000000001,18.25));
#67465=CARTESIAN_POINT('',(29.9999999999999,-1.50000000000001,18.3125));
#67466=CARTESIAN_POINT('',(30.,-1.50000000000001,16.));
#67467=CARTESIAN_POINT('Ctrl Pts',(30.,-1.50000000000001,18.25));
#67468=CARTESIAN_POINT('Ctrl Pts',(30.0882156275205,-1.50000000000001,18.254244276358));
#67469=CARTESIAN_POINT('Ctrl Pts',(30.1764501130872,-1.49221937550789,18.2587055884823));
#67470=CARTESIAN_POINT('Ctrl Pts',(30.4546079281867,-1.44254775409159,18.2734682298626));
#67471=CARTESIAN_POINT('Ctrl Pts',(30.6370980720641,-1.37175281599007,18.2842148170619));
#67472=CARTESIAN_POINT('Ctrl Pts',(30.9691525442989,-1.16201577961996,18.3060168240942));
#67473=CARTESIAN_POINT('Ctrl Pts',(31.1145075241426,-1.02344071977941,18.3168595260404));
#67474=CARTESIAN_POINT('Ctrl Pts',(31.3375735551139,-0.704962761586156,
18.3364384054093));
#67475=CARTESIAN_POINT('Ctrl Pts',(31.4160050795816,-0.530113102524481,
18.345549272082));
#67476=CARTESIAN_POINT('Ctrl Pts',(31.5048780292219,-0.154342998497877,
18.3664253889724));
#67477=CARTESIAN_POINT('Ctrl Pts',(31.5121437205665,0.0435642244476196,
18.3774202346916));
#67478=CARTESIAN_POINT('Ctrl Pts',(31.4493976248982,0.435280459623824,18.3991822477569));
#67479=CARTESIAN_POINT('Ctrl Pts',(31.3782925123276,0.624894161678516,18.4093783750732));
#67480=CARTESIAN_POINT('Ctrl Pts',(31.1707210215853,0.957071364942045,18.428592307613));
#67481=CARTESIAN_POINT('Ctrl Pts',(31.0393074800838,1.09835818528463,18.4388395784748));
#67482=CARTESIAN_POINT('Ctrl Pts',(30.7245434883219,1.32834442072559,18.4603721746294));
#67483=CARTESIAN_POINT('Ctrl Pts',(30.5424433469957,1.41252449906513,18.4714718072734));
#67484=CARTESIAN_POINT('Ctrl Pts',(30.1611576166725,1.50380428740964,18.492351975203));
#67485=CARTESIAN_POINT('Ctrl Pts',(29.9661847612145,1.51203572283979,18.5012926108002));
#67486=CARTESIAN_POINT('Ctrl Pts',(29.583743920727,1.45401144673963,18.5213045897645));
#67487=CARTESIAN_POINT('Ctrl Pts',(29.3999206687447,1.38827539073469,18.5319747916547));
#67488=CARTESIAN_POINT('Ctrl Pts',(29.0627111089636,1.18787072518152,18.5537655904295));
#67489=CARTESIAN_POINT('Ctrl Pts',(28.9136362676481,1.05327089433686,18.5646768412665));
#67490=CARTESIAN_POINT('Ctrl Pts',(28.6818733006966,0.740747545450625,18.5845087463487));
#67491=CARTESIAN_POINT('Ctrl Pts',(28.5986773683508,0.567862991064222,18.593452056052));
#67492=CARTESIAN_POINT('Ctrl Pts',(28.4999017481138,0.194886335563048,18.6141729813576));
#67493=CARTESIAN_POINT('Ctrl Pts',(28.4872987443723,-0.0022124298529334,
18.6251229127696));
#67494=CARTESIAN_POINT('Ctrl Pts',(28.538885584329,-0.393300822235859,18.6468500456797));
#67495=CARTESIAN_POINT('Ctrl Pts',(28.6038229043615,-0.583241208522858,
18.6573608761808));
#67496=CARTESIAN_POINT('Ctrl Pts',(28.7997809979745,-0.919686600601166,
18.6761346196911));
#67497=CARTESIAN_POINT('Ctrl Pts',(28.9262538190534,-1.06460970419426,18.6862451878989));
#67498=CARTESIAN_POINT('Ctrl Pts',(29.2324514589516,-1.30386842227857,18.7076232042196));
#67499=CARTESIAN_POINT('Ctrl Pts',(29.4110795308611,-1.39369344460164,18.7187125908454));
#67500=CARTESIAN_POINT('Ctrl Pts',(29.7319270119205,-1.48199126728517,18.7366020897721));
#67501=CARTESIAN_POINT('Ctrl Pts',(29.8657845574029,-1.50000000000001,18.7435425565073));
#67502=CARTESIAN_POINT('Ctrl Pts',(30.0000000000002,-1.50000000000001,18.75));
#67503=CARTESIAN_POINT('Ctrl Pts',(30.,-1.50000000000001,18.8125));
#67504=CARTESIAN_POINT('Ctrl Pts',(29.9200694828282,-1.50000000000001,18.8086543411995));
#67505=CARTESIAN_POINT('Ctrl Pts',(29.8400989517173,-1.4936120985387,18.8046293155201));
#67506=CARTESIAN_POINT('Ctrl Pts',(29.5632380932733,-1.44889785862683,18.7900667790378));
#67507=CARTESIAN_POINT('Ctrl Pts',(29.3740258977232,-1.377754564609,18.7789871004233));
#67508=CARTESIAN_POINT('Ctrl Pts',(29.041174726881,-1.16949277461302,18.7571877412774));
#67509=CARTESIAN_POINT('Ctrl Pts',(28.8991316339595,-1.03690216726548,18.7466706173565));
#67510=CARTESIAN_POINT('Ctrl Pts',(28.6710550609186,-0.722648191218263,
18.7269680010074));
#67511=CARTESIAN_POINT('Ctrl Pts',(28.5881967902834,-0.543266122771758,
18.717681451265));
#67512=CARTESIAN_POINT('Ctrl Pts',(28.4956085723343,-0.160873384602161,
18.6964374102556));
#67513=CARTESIAN_POINT('Ctrl Pts',(28.4875239735192,0.0385552236194734,
18.6853580431322));
#67514=CARTESIAN_POINT('Ctrl Pts',(28.5480104653806,0.421875716785893,18.6640624601785));
#67515=CARTESIAN_POINT('Ctrl Pts',(28.6132160700899,0.602522755625134,18.6541515963916));
#67516=CARTESIAN_POINT('Ctrl Pts',(28.8119377533085,0.937035677616922,18.635298569339));
#67517=CARTESIAN_POINT('Ctrl Pts',(28.9464389491764,1.08605274148643,18.6246880146503));
#67518=CARTESIAN_POINT('Ctrl Pts',(29.2628767471001,1.32090830831045,18.6029396282541));
#67519=CARTESIAN_POINT('Ctrl Pts',(29.4409618987283,1.40557199772365,18.5920197332512));
#67520=CARTESIAN_POINT('Ctrl Pts',(29.814809484317,1.50065373381321,18.5713918235674));
#67521=CARTESIAN_POINT('Ctrl Pts',(30.0065604479866,1.51202122412194,18.5625182831912));
#67522=CARTESIAN_POINT('Ctrl Pts',(30.3943911928229,1.4610824148403,18.5424438008558));
#67523=CARTESIAN_POINT('Ctrl Pts',(30.58616263238,1.39524271133166,18.5313883125152));
#67524=CARTESIAN_POINT('Ctrl Pts',(30.9257469654151,1.19593240245758,18.5095136562056));
#67525=CARTESIAN_POINT('Ctrl Pts',(31.0718264769195,1.06698913560375,18.4989036450188));
#67526=CARTESIAN_POINT('Ctrl Pts',(31.3078217753803,0.759832047419874,18.4790171745892));
#67527=CARTESIAN_POINT('Ctrl Pts',(31.3951262846915,0.584269865007977,18.4699594369449));
#67528=CARTESIAN_POINT('Ctrl Pts',(31.4989966927882,0.205709858638526,18.4489283254799));
#67529=CARTESIAN_POINT('Ctrl Pts',(31.5130318328004,0.00600577899638372,
18.4378336543887));
#67530=CARTESIAN_POINT('Ctrl Pts',(31.4635867359632,-0.379900299649008,
18.4163944277973));
#67531=CARTESIAN_POINT('Ctrl Pts',(31.4034385131977,-0.562844950250642,
18.4062308360972));
#67532=CARTESIAN_POINT('Ctrl Pts',(31.213924427377,-0.903263174389702,18.387318712534));
#67533=CARTESIAN_POINT('Ctrl Pts',(31.0836707542498,-1.05603307941032,18.3769705479341));
#67534=CARTESIAN_POINT('Ctrl Pts',(30.7734274797909,-1.30006438227702,18.3552653141303));
#67535=CARTESIAN_POINT('Ctrl Pts',(30.5972523067208,-1.389838711312,18.3442953508018));
#67536=CARTESIAN_POINT('Ctrl Pts',(30.27555179434,-1.4809632576453,18.3262862902852));
#67537=CARTESIAN_POINT('Ctrl Pts',(30.1379932399681,-1.50000000000003,18.3191392028535));
#67538=CARTESIAN_POINT('Ctrl Pts',(29.9999999999998,-1.50000000000001,18.3125));
#67539=CARTESIAN_POINT('Origin',(30.,-1.32966554433622E-14,16.));
#67540=CARTESIAN_POINT('',(30.,-1.50000000000001,17.75));
#67541=CARTESIAN_POINT('',(30.,-1.50000000000001,17.8125));
#67542=CARTESIAN_POINT('',(30.,-1.50000000000001,16.));
#67543=CARTESIAN_POINT('Ctrl Pts',(30.,-1.50000000000001,17.75));
#67544=CARTESIAN_POINT('Ctrl Pts',(30.1165214576707,-1.50000000000002,17.755606141246));
#67545=CARTESIAN_POINT('Ctrl Pts',(30.2328774102524,-1.48642630258387,17.7615813667753));
#67546=CARTESIAN_POINT('Ctrl Pts',(30.5364815251301,-1.41429282343802,17.778192234317));
#67547=CARTESIAN_POINT('Ctrl Pts',(30.7156172892318,-1.33263663661631,17.7890791351975));
#67548=CARTESIAN_POINT('Ctrl Pts',(31.0356297737271,-1.1031687507031,17.8108498509785));
#67549=CARTESIAN_POINT('Ctrl Pts',(31.1725674881258,-0.956358157459637,
17.8215163418689));
#67550=CARTESIAN_POINT('Ctrl Pts',(31.376639002963,-0.625293846242278,17.8405309680715));
#67551=CARTESIAN_POINT('Ctrl Pts',(31.4447439774106,-0.445961069817197,
17.8502243850103));
#67552=CARTESIAN_POINT('Ctrl Pts',(31.5115582160321,-0.0642628969545898,
17.8714298390582));
#67553=CARTESIAN_POINT('Ctrl Pts',(31.5068955968845,0.134928419608339,17.8824960233117));
#67554=CARTESIAN_POINT('Ctrl Pts',(31.4208614242251,0.519471460613856,17.9038595255897));
#67555=CARTESIAN_POINT('Ctrl Pts',(31.3405819882652,0.701086441059189,17.9133091757132));
#67556=CARTESIAN_POINT('Ctrl Pts',(31.1170623100669,1.01937978501502,17.9329047530211));
#67557=CARTESIAN_POINT('Ctrl Pts',(30.9773620677606,1.15399638378434,17.9433654340287));
#67558=CARTESIAN_POINT('Ctrl Pts',(30.6484546459992,1.36726868066811,17.9651142302054));
#67559=CARTESIAN_POINT('Ctrl Pts',(30.4607652253454,1.44139714446346,17.9762035656613));
#67560=CARTESIAN_POINT('Ctrl Pts',(30.0756449322311,1.51026934438856,17.9966457910675));
#67561=CARTESIAN_POINT('Ctrl Pts',(29.8825476840369,1.50759466650969,18.005439964228));
#67562=CARTESIAN_POINT('Ctrl Pts',(29.5047175214704,1.42916638864856,18.025796889674));
#67563=CARTESIAN_POINT('Ctrl Pts',(29.323805468645,1.35298625851431,18.0366171395998));
#67564=CARTESIAN_POINT('Ctrl Pts',(28.9975535579724,1.13341344377778,18.0584131868245));
#67565=CARTESIAN_POINT('Ctrl Pts',(28.8562978602342,0.990703384015885,18.0691735230773));
#67566=CARTESIAN_POINT('Ctrl Pts',(28.6425900107442,0.665955504210131,18.088476321219));
#67567=CARTESIAN_POINT('Ctrl Pts',(28.5692557712623,0.488931672930093,18.0978371292817));
#67568=CARTESIAN_POINT('Ctrl Pts',(28.4911736103312,0.110209786397706,18.118877234089));
#67569=CARTESIAN_POINT('Ctrl Pts',(28.4897399259643,-0.0884146511275797,
18.1299119250627));
#67570=CARTESIAN_POINT('Ctrl Pts',(28.563963673652,-0.476687925939349,18.1514826625522));
#67571=CARTESIAN_POINT('Ctrl Pts',(28.6395954743022,-0.662348456736596,
18.1612794083161));
#67572=CARTESIAN_POINT('Ctrl Pts',(28.8549808751967,-0.987772207975308,
18.1806816918938));
#67573=CARTESIAN_POINT('Ctrl Pts',(28.9904690556508,-1.12587258901724,18.1910364917109));
#67574=CARTESIAN_POINT('Ctrl Pts',(29.3122241078786,-1.34783032180127,18.2126824314563));
#67575=CARTESIAN_POINT('Ctrl Pts',(29.4971108100191,-1.42716337813628,18.2237814930698));
#67576=CARTESIAN_POINT('Ctrl Pts',(29.7935943795659,-1.48934588454492,18.2397733573052));
#67577=CARTESIAN_POINT('Ctrl Pts',(29.8967698772032,-1.50000000000001,18.2450333384012));
#67578=CARTESIAN_POINT('Ctrl Pts',(30.,-1.50000000000001,18.25));
#67579=CARTESIAN_POINT('Ctrl Pts',(29.9999999999998,-1.50000000000001,18.3125));
#67580=CARTESIAN_POINT('Ctrl Pts',(29.9486057940186,-1.50000000000001,18.3100272951118));
#67581=CARTESIAN_POINT('Ctrl Pts',(29.8971583803719,-1.4973588143077,18.3074786639994));
#67582=CARTESIAN_POINT('Ctrl Pts',(29.6480074739756,-1.47161947014145,18.294776403644));
#67583=CARTESIAN_POINT('Ctrl Pts',(29.4562105276991,-1.41203266981329,18.2838933798658));
#67584=CARTESIAN_POINT('Ctrl Pts',(29.1116733937691,-1.22407639141983,18.2620958215476));
#67585=CARTESIAN_POINT('Ctrl Pts',(28.9612380534891,-1.09930641465076,18.2513921651757));
#67586=CARTESIAN_POINT('Ctrl Pts',(28.7165798694464,-0.800027931931824,
18.231307751621));
#67587=CARTESIAN_POINT('Ctrl Pts',(28.6244510402799,-0.628553460673264,
18.2224196367041));
#67588=CARTESIAN_POINT('Ctrl Pts',(28.5083938755392,-0.254315567480426,
18.2016286426378));
#67589=CARTESIAN_POINT('Ctrl Pts',(28.4878541874048,-0.054508044740069,
18.1905282247078));
#67590=CARTESIAN_POINT('Ctrl Pts',(28.5251827599344,0.333985841156563,18.1689452310469));
#67591=CARTESIAN_POINT('Ctrl Pts',(28.5797880070138,0.519280463308488,18.1586510853718));
#67592=CARTESIAN_POINT('Ctrl Pts',(28.7594942565881,0.866593796413574,18.1393559001993));
#67593=CARTESIAN_POINT('Ctrl Pts',(28.8856977548396,1.02381782162173,18.1293391744996));
#67594=CARTESIAN_POINT('Ctrl Pts',(29.1898211855382,1.2775694571787,18.1076583725746));
#67595=CARTESIAN_POINT('Ctrl Pts',(29.3638803222543,1.37256230066096,18.096645258358));
#67596=CARTESIAN_POINT('Ctrl Pts',(29.732534735318,1.48813273455022,18.0756980748094));
#67597=CARTESIAN_POINT('Ctrl Pts',(29.9228794435952,1.51000349618475,18.066488339394));
#67598=CARTESIAN_POINT('Ctrl Pts',(30.3105607244676,1.48091384388274,18.0470279691741));
#67599=CARTESIAN_POINT('Ctrl Pts',(30.5039294602603,1.4267400893485,18.0362196850207));
#67600=CARTESIAN_POINT('Ctrl Pts',(30.8540539626656,1.24831186951753,18.0144179726049));
#67601=CARTESIAN_POINT('Ctrl Pts',(31.0082947964679,1.12740587313612,18.0036385571291));
#67602=CARTESIAN_POINT('Ctrl Pts',(31.2606439376435,0.835225571389926,17.9833812839205));
#67603=CARTESIAN_POINT('Ctrl Pts',(31.3570327509323,0.667298431844612,17.9745721351024));
#67604=CARTESIAN_POINT('Ctrl Pts',(31.4837741625619,0.297001147228916,17.9540000637349));
#67605=CARTESIAN_POINT('Ctrl Pts',(31.5100733842477,0.0972732161684081,
17.9429040675649));
#67606=CARTESIAN_POINT('Ctrl Pts',(31.4835317838137,-0.293194316444828,
17.9212114268642));
#67607=CARTESIAN_POINT('Ctrl Pts',(31.4338905957024,-0.480424140062753,
17.9108097699965));
#67608=CARTESIAN_POINT('Ctrl Pts',(31.2642037542022,-0.83118542637216,17.8913230318682));
#67609=CARTESIAN_POINT('Ctrl Pts',(31.14378015867,-0.99038786521744,17.8816860411746));
#67610=CARTESIAN_POINT('Ctrl Pts',(30.8486060826855,-1.25246692848107,17.8602044978428));
#67611=CARTESIAN_POINT('Ctrl Pts',(30.6769673305094,-1.35296725332812,17.8491548488382));
#67612=CARTESIAN_POINT('Ctrl Pts',(30.3327732686651,-1.47215364288648,17.8292840712733));
#67613=CARTESIAN_POINT('Ctrl Pts',(30.1668871533766,-1.50000000000002,17.8205293619105));
#67614=CARTESIAN_POINT('Ctrl Pts',(29.9999999999999,-1.50000000000001,17.8125));
#67615=CARTESIAN_POINT('Origin',(30.,-1.32966554433622E-14,16.));
#67616=CARTESIAN_POINT('',(29.9999999999999,-1.50000000000001,17.25));
#67617=CARTESIAN_POINT('',(30.,-1.50000000000001,17.3125));
#67618=CARTESIAN_POINT('',(30.,-1.50000000000001,16.));
#67619=CARTESIAN_POINT('Ctrl Pts',(29.9999999999998,-1.50000000000001,17.25));
#67620=CARTESIAN_POINT('Ctrl Pts',(30.1437406795734,-1.50000000000003,17.2569157266704));
#67621=CARTESIAN_POINT('Ctrl Pts',(30.2869532673798,-1.47934432155244,17.2643798143597));
#67622=CARTESIAN_POINT('Ctrl Pts',(30.6133040117111,-1.38286217393555,17.2827614315232));
#67623=CARTESIAN_POINT('Ctrl Pts',(30.7886268831202,-1.29093521604786,17.2937501837148));
#67624=CARTESIAN_POINT('Ctrl Pts',(31.0976621700988,-1.04186059007729,17.3155373905022));
#67625=CARTESIAN_POINT('Ctrl Pts',(31.2270940102629,-0.885739363684009,
17.3257922575731));
#67626=CARTESIAN_POINT('Ctrl Pts',(31.4122925189225,-0.540349731904653,
17.3449805704497));
#67627=CARTESIAN_POINT('Ctrl Pts',(31.4695815451721,-0.356167506723217,
17.3552129162933));
#67628=CARTESIAN_POINT('Ctrl Pts',(31.5127670349393,0.0311250181831806,
17.376729167677));
#67629=CARTESIAN_POINT('Ctrl Pts',(31.4953668358477,0.230908289106308,17.3878282382838));
#67630=CARTESIAN_POINT('Ctrl Pts',(31.3851742993692,0.607249385403804,17.408736076967));
#67631=CARTESIAN_POINT('Ctrl Pts',(31.2953707932844,0.78068569360338,17.4176954906944));
#67632=CARTESIAN_POINT('Ctrl Pts',(31.054895847731,1.08378386704463,17.4376847406135));
#67633=CARTESIAN_POINT('Ctrl Pts',(30.9065553840191,1.21059289157644,17.4483442474051));
#67634=CARTESIAN_POINT('Ctrl Pts',(30.5651448786952,1.40362381134034,17.4701323379946));
#67635=CARTESIAN_POINT('Ctrl Pts',(30.3742618691092,1.46611551598061,17.4810520817598));
#67636=CARTESIAN_POINT('Ctrl Pts',(29.9878426931301,1.51196372025337,17.5009172442622));
#67637=CARTESIAN_POINT('Ctrl Pts',(29.7964276873605,1.49824842026232,17.5098430324513));
#67638=CARTESIAN_POINT('Ctrl Pts',(29.423704438961,1.39861791618851,17.5305432021031));
#67639=CARTESIAN_POINT('Ctrl Pts',(29.2464613140656,1.31164870813791,17.5414866272603));
#67640=CARTESIAN_POINT('Ctrl Pts',(28.9327465597656,1.07261781027188,17.5632199825769));
#67641=CARTESIAN_POINT('Ctrl Pts',(28.8001758891987,0.921899105215767,17.5737833830436));
#67642=CARTESIAN_POINT('Ctrl Pts',(28.6055876448106,0.584753731199478,17.5925136816001));
#67643=CARTESIAN_POINT('Ctrl Pts',(28.5426610065469,0.403064732761888,17.6026075148466));
#67644=CARTESIAN_POINT('Ctrl Pts',(28.487113056257,0.0186136653436067,17.623965907481));
#67645=CARTESIAN_POINT('Ctrl Pts',(28.4978576022209,-0.180959534499292,
17.6350533074722));
#67646=CARTESIAN_POINT('Ctrl Pts',(28.5955062015491,-0.561653522812593,
17.6562029734896));
#67647=CARTESIAN_POINT('Ctrl Pts',(28.6803571582567,-0.739318323214391,
17.6653786075964));
#67648=CARTESIAN_POINT('Ctrl Pts',(28.9119736981394,-1.05041195534416,17.6851637533487));
#67649=CARTESIAN_POINT('Ctrl Pts',(29.0558270731865,-1.1813919096406,17.6957232341464));
#67650=CARTESIAN_POINT('Ctrl Pts',(29.3917078154049,-1.38569020760041,17.7175582566121));
#67651=CARTESIAN_POINT('Ctrl Pts',(29.5820781032457,-1.45448064464283,17.7286282968298));
#67652=CARTESIAN_POINT('Ctrl Pts',(29.8532284268276,-1.49461899708891,17.7427889770903));
#67653=CARTESIAN_POINT('Ctrl Pts',(29.9266397495672,-1.50000000000001,17.7464704533054));
#67654=CARTESIAN_POINT('Ctrl Pts',(30.,-1.50000000000001,17.75));
#67655=CARTESIAN_POINT('Ctrl Pts',(29.9999999999999,-1.50000000000001,17.8125));
#67656=CARTESIAN_POINT('Ctrl Pts',(29.9772840745252,-1.50000000000001,17.811407079526));
#67657=CARTESIAN_POINT('Ctrl Pts',(29.9545509622526,-1.49948399224778,17.8102989986031));
#67658=CARTESIAN_POINT('Ctrl Pts',(29.7331702393738,-1.48941079200354,17.7993680024896));
#67659=CARTESIAN_POINT('Ctrl Pts',(29.5383211874472,-1.44096198242896,17.7886475228419));
#67660=CARTESIAN_POINT('Ctrl Pts',(29.1826189299973,-1.27271128807371,17.7668601596023));
#67661=CARTESIAN_POINT('Ctrl Pts',(29.0244894301944,-1.15598200374574,17.7560096703756));
#67662=CARTESIAN_POINT('Ctrl Pts',(28.764135320164,-0.871290254073719,17.7355752732588));
#67663=CARTESIAN_POINT('Ctrl Pts',(28.6633306533142,-0.706980266162622,
17.7267766814534));
#67664=CARTESIAN_POINT('Ctrl Pts',(28.5256044330412,-0.340872542641299,
17.70643736348));
#67665=CARTESIAN_POINT('Ctrl Pts',(28.4933384090279,-0.141395913779689,
17.6953553285433));
#67666=CARTESIAN_POINT('Ctrl Pts',(28.5086475773052,0.250803035896437,17.6735664980057));
#67667=CARTESIAN_POINT('Ctrl Pts',(28.5530910089168,0.439894111123241,17.6630614382709));
#67668=CARTESIAN_POINT('Ctrl Pts',(28.7124602775381,0.794124581104987,17.6433819677164));
#67669=CARTESIAN_POINT('Ctrl Pts',(28.8270773285161,0.955330804312479,17.6340619682235));
#67670=CARTESIAN_POINT('Ctrl Pts',(29.1130611662184,1.22571784831621,17.6127918131944));
#67671=CARTESIAN_POINT('Ctrl Pts',(29.2820600929988,1.33176716482588,17.6017150341911));
#67672=CARTESIAN_POINT('Ctrl Pts',(29.6446531268203,1.46968030941703,17.5804388480344));
#67673=CARTESIAN_POINT('Ctrl Pts',(29.8337664889299,1.50284763615596,17.5705770145346));
#67674=CARTESIAN_POINT('Ctrl Pts',(30.2227595353817,1.49663210693258,17.5516889242716));
#67675=CARTESIAN_POINT('Ctrl Pts',(30.4189176611452,1.45396403183943,17.5410660377374));
#67676=CARTESIAN_POINT('Ctrl Pts',(30.7799134803451,1.29609345193241,17.5193123244018));
#67677=CARTESIAN_POINT('Ctrl Pts',(30.9418307309724,1.18367445855365,17.5083993272327));
#67678=CARTESIAN_POINT('Ctrl Pts',(31.2101475557693,0.906543829758461,17.4877918549585));
#67679=CARTESIAN_POINT('Ctrl Pts',(31.3153431699375,0.745751786456619,17.478930654803));
#67680=CARTESIAN_POINT('Ctrl Pts',(31.463864637894,0.383898047749162,17.4588276693193));
#67681=CARTESIAN_POINT('Ctrl Pts',(31.5020303054666,0.184838532612863,17.4477688073673));
#67682=CARTESIAN_POINT('Ctrl Pts',(31.4978841524782,-0.208759642694536,
17.4259022420724));
#67683=CARTESIAN_POINT('Ctrl Pts',(31.4586348080642,-0.399547636290809,
17.4153029090948));
#67684=CARTESIAN_POINT('Ctrl Pts',(31.3094217036004,-0.757113584921528,
17.3954381341709));
#67685=CARTESIAN_POINT('Ctrl Pts',(31.200380183046,-0.920271802442848,17.3863568795276));
#67686=CARTESIAN_POINT('Ctrl Pts',(30.923406682912,-1.19858244148629,17.3653001347046));
#67687=CARTESIAN_POINT('Ctrl Pts',(30.7571425046312,-1.30996529750999,17.3542067774745));
#67688=CARTESIAN_POINT('Ctrl Pts',(30.3978227489156,-1.45880886920802,17.3327844540089));
#67689=CARTESIAN_POINT('Ctrl Pts',(30.2092450764931,-1.49754020852369,17.3226356359777));
#67690=CARTESIAN_POINT('Ctrl Pts',(30.0122952852091,-1.49996221637769,17.3130926067305));
#67691=CARTESIAN_POINT('Ctrl Pts',(30.0061468402235,-1.50000000000001,17.3127957399881));
#67692=CARTESIAN_POINT('Ctrl Pts',(30.,-1.50000000000001,17.3125));
#67693=CARTESIAN_POINT('Origin',(30.,-1.32966554433622E-14,16.));
#67694=CARTESIAN_POINT('',(30.,-1.50000000000001,16.75));
#67695=CARTESIAN_POINT('',(30.0000000000001,-1.50000000000001,16.8125));
#67696=CARTESIAN_POINT('',(30.,-1.50000000000001,16.));
#67697=CARTESIAN_POINT('Ctrl Pts',(30.,-1.50000000000001,16.75));
#67698=CARTESIAN_POINT('Ctrl Pts',(30.1733135774153,-1.50000000000002,16.7583385533812));
#67699=CARTESIAN_POINT('Ctrl Pts',(30.3454665850143,-1.46996630625128,16.767455538092));
#67700=CARTESIAN_POINT('Ctrl Pts',(30.6943533649566,-1.34416445320596,16.7877358570363));
#67701=CARTESIAN_POINT('Ctrl Pts',(30.8648984846931,-1.24131259552183,16.7987982089822));
#67702=CARTESIAN_POINT('Ctrl Pts',(31.1561999433551,-0.975703692756434,
16.8201914820235));
#67703=CARTESIAN_POINT('Ctrl Pts',(31.2741613882488,-0.815654351280513,
16.8296858693734));
#67704=CARTESIAN_POINT('Ctrl Pts',(31.4395048489934,-0.463422668720622,
16.8492542961822));
#67705=CARTESIAN_POINT('Ctrl Pts',(31.4869681438372,-0.275392752547583,
16.8597004026363));
#67706=CARTESIAN_POINT('Ctrl Pts',(31.5087956503657,0.115841301406496,16.881435627856));
#67707=CARTESIAN_POINT('Ctrl Pts',(31.4799884843839,0.315484512989904,16.8925269173884));
#67708=CARTESIAN_POINT('Ctrl Pts',(31.3486206066034,0.684034451059388,16.9130019139478));
#67709=CARTESIAN_POINT('Ctrl Pts',(31.2503774147184,0.850433854559545,16.9217976845453));
#67710=CARTESIAN_POINT('Ctrl Pts',(30.994668844219,1.13948462780369,16.9421296570253));
#67711=CARTESIAN_POINT('Ctrl Pts',(30.8387866934565,1.25865700214481,16.9529398842324));
#67712=CARTESIAN_POINT('Ctrl Pts',(30.4862910667067,1.43284604521895,16.9747379225116));
#67713=CARTESIAN_POINT('Ctrl Pts',(30.2922814189341,1.48462820882751,16.9855106094757));
#67714=CARTESIAN_POINT('Ctrl Pts',(29.904287970164,1.50893843055208,17.0048532369201));
#67715=CARTESIAN_POINT('Ctrl Pts',(29.714222422622,1.48472560659638,17.014173768808));
#67716=CARTESIAN_POINT('Ctrl Pts',(29.3467837907597,1.36454370703768,17.0351905543248));
#67717=CARTESIAN_POINT('Ctrl Pts',(29.1737126610206,1.26724866527873,17.0462200829857));
#67718=CARTESIAN_POINT('Ctrl Pts',(28.8733100927186,1.01000510192613,17.0678188628294));
#67719=CARTESIAN_POINT('Ctrl Pts',(28.7495253450837,0.851954282658887,17.0776692065189));
#67720=CARTESIAN_POINT('Ctrl Pts',(28.5739823591041,0.503198698880474,17.0970445167289));
#67721=CARTESIAN_POINT('Ctrl Pts',(28.5214293436323,0.317084997718663,17.1073841667934));
#67722=CARTESIAN_POINT('Ctrl Pts',(28.4885674976081,-0.0722634762162506,
17.1290146375676));
#67723=CARTESIAN_POINT('Ctrl Pts',(28.5114956545415,-0.272057456078969,
17.1401143031155));
#67724=CARTESIAN_POINT('Ctrl Pts',(28.6319945909535,-0.644674063533988,
17.1608152257519));
#67725=CARTESIAN_POINT('Ctrl Pts',(28.7258902835189,-0.814669507709904,
17.1696624095652));
#67726=CARTESIAN_POINT('Ctrl Pts',(28.9737348011573,-1.1110192567928,17.1898187719544));
#67727=CARTESIAN_POINT('Ctrl Pts',(29.1257542814876,-1.2342064357884,17.2005546786951));
#67728=CARTESIAN_POINT('Ctrl Pts',(29.4726321438156,-1.41824610841819,17.2223560607564));
#67729=CARTESIAN_POINT('Ctrl Pts',(29.6650975807577,-1.47560141498182,17.2332092613688));
#67730=CARTESIAN_POINT('Ctrl Pts',(29.9087297050291,-1.49791971441829,17.2455509701752));
#67731=CARTESIAN_POINT('Ctrl Pts',(29.9543886563371,-1.50000000000001,17.2478055232048));
#67732=CARTESIAN_POINT('Ctrl Pts',(29.9999999999998,-1.50000000000001,17.25));
#67733=CARTESIAN_POINT('Ctrl Pts',(30.,-1.50000000000001,17.3125));
#67734=CARTESIAN_POINT('Ctrl Pts',(29.8075276745562,-1.50000000000001,17.3032396709245));
#67735=CARTESIAN_POINT('Ctrl Pts',(29.6167265402445,-1.46295509134636,17.2930307218294));
#67736=CARTESIAN_POINT('Ctrl Pts',(29.2565239800332,-1.31741270776536,17.2716576240826));
#67737=CARTESIAN_POINT('Ctrl Pts',(29.0910935230227,-1.20922562866616,17.2606931508671));
#67738=CARTESIAN_POINT('Ctrl Pts',(28.8152192771185,-0.939380042859163,
17.2399244343056));
#67739=CARTESIAN_POINT('Ctrl Pts',(28.7058473428781,-0.781856067083356,
17.2309364481713));
#67740=CARTESIAN_POINT('Ctrl Pts',(28.5481536416827,-0.426269472803969,
17.211181637378));
#67741=CARTESIAN_POINT('Ctrl Pts',(28.5044938401357,-0.230229772369996,
17.2002905429095));
#67742=CARTESIAN_POINT('Ctrl Pts',(28.4962752409133,0.162097483734217,17.178494584237));
#67743=CARTESIAN_POINT('Ctrl Pts',(28.5297146688179,0.3545967167103,17.167800182405));
#67744=CARTESIAN_POINT('Ctrl Pts',(28.6677231734513,0.715751667501951,17.1477360184722));
#67745=CARTESIAN_POINT('Ctrl Pts',(28.7707689938353,0.881053857184024,17.1388343527704));
#67746=CARTESIAN_POINT('Ctrl Pts',(29.0378553430027,1.16782543883526,17.1180182775366));
#67747=CARTESIAN_POINT('Ctrl Pts',(29.2009578477084,1.28493633443696,17.1069179241867));
#67748=CARTESIAN_POINT('Ctrl Pts',(29.5564777297123,1.44564779283652,17.0853487587108));
#67749=CARTESIAN_POINT('Ctrl Pts',(29.7443345881639,1.49039149544099,17.0750676107666));
#67750=CARTESIAN_POINT('Ctrl Pts',(30.1352017346056,1.50720082969336,17.0557950804638));
#67751=CARTESIAN_POINT('Ctrl Pts',(30.3346031531762,1.47580805773789,17.0457293998907));
#67752=CARTESIAN_POINT('Ctrl Pts',(30.7060862860091,1.33790450333634,17.02402575504));
#67753=CARTESIAN_POINT('Ctrl Pts',(30.8749553104054,1.23409963004519,17.0130175716131));
#67754=CARTESIAN_POINT('Ctrl Pts',(31.1584137835032,0.971677105747927,16.9920901549037));
#67755=CARTESIAN_POINT('Ctrl Pts',(31.271994699923,0.817368296550736,16.9829093498084));
#67756=CARTESIAN_POINT('Ctrl Pts',(31.4394257557863,0.466485221859018,16.9634158456588));
#67757=CARTESIAN_POINT('Ctrl Pts',(31.488516036617,0.271760297088586,16.9525977942827));
#67758=CARTESIAN_POINT('Ctrl Pts',(31.5076810248584,-0.120678265071266,
16.9307956519405));
#67759=CARTESIAN_POINT('Ctrl Pts',(31.4794384691607,-0.314545865899112,
16.9200252296723));
#67760=CARTESIAN_POINT('Ctrl Pts',(31.3513352758344,-0.678794152386266,
16.8997892137563));
#67761=CARTESIAN_POINT('Ctrl Pts',(31.2534603041453,-0.845994238167287,
16.890973963719));
#67762=CARTESIAN_POINT('Ctrl Pts',(30.9950590391717,-1.14001068930543,16.8703745034186));
#67763=CARTESIAN_POINT('Ctrl Pts',(30.8348670617779,-1.26204295887652,16.8592774780469));
#67764=CARTESIAN_POINT('Ctrl Pts',(30.4829704713108,-1.43301939771413,16.8375974999208));
#67765=CARTESIAN_POINT('Ctrl Pts',(30.2958966065637,-1.48299380376918,16.8272087264607));
#67766=CARTESIAN_POINT('Ctrl Pts',(30.0696474084832,-1.49878860163674,16.8158845624575));
#67767=CARTESIAN_POINT('Ctrl Pts',(30.0348056486057,-1.50000000000001,16.8141745875493));
#67768=CARTESIAN_POINT('Ctrl Pts',(30.0000000000002,-1.50000000000001,16.8125));
#67769=CARTESIAN_POINT('Origin',(30.,-1.32966554433622E-14,16.));
#67770=CARTESIAN_POINT('',(30.0000000000023,1.33373412263454,16.1584936490537));
#67771=CARTESIAN_POINT('',(30.,1.1752404735808,16.));
#67772=CARTESIAN_POINT('',(30.,1.17524047358083,16.));
#67773=CARTESIAN_POINT('',(30.,-1.17524047358085,16.));
#67774=CARTESIAN_POINT('Ctrl Pts',(30.,-1.17524047358083,16.));
#67775=CARTESIAN_POINT('Ctrl Pts',(30.0938726776238,-1.17889502189498,16.0036545483141));
#67776=CARTESIAN_POINT('Ctrl Pts',(30.2222715669962,-1.17292308708929,16.0088746896198));
#67777=CARTESIAN_POINT('Ctrl Pts',(30.4821758748939,-1.10061359842964,16.0205734257761));
#67778=CARTESIAN_POINT('Ctrl Pts',(30.5904809486724,-1.05245648363552,16.0257840816621));
#67779=CARTESIAN_POINT('Ctrl Pts',(30.8133642274912,-0.91102859460423,16.0372929849601));
#67780=CARTESIAN_POINT('Ctrl Pts',(30.9213977318432,-0.810903247446717,
16.0434573291476));
#67781=CARTESIAN_POINT('Ctrl Pts',(31.1067869536601,-0.562636269482013,
16.0555173993883));
#67782=CARTESIAN_POINT('Ctrl Pts',(31.1779495349821,-0.411557996758087,
16.0617064115579));
#67783=CARTESIAN_POINT('Ctrl Pts',(31.2569648094213,-0.0966670523057213,
16.075198195417));
#67784=CARTESIAN_POINT('Ctrl Pts',(31.2657685184509,0.0650399419384585,
16.0820144838088));
#67785=CARTESIAN_POINT('Ctrl Pts',(31.2286447980599,0.334175553677255,16.0931820826379));
#67786=CARTESIAN_POINT('Ctrl Pts',(31.1927617340632,0.495209878479218,16.0995752755442));
#67787=CARTESIAN_POINT('Ctrl Pts',(31.0046982036223,0.825162649859306,16.1133508913014));
#67788=CARTESIAN_POINT('Ctrl Pts',(30.8901527526008,0.956864086379422,16.1201881413696));
#67789=CARTESIAN_POINT('Ctrl Pts',(30.6234294043457,1.16264469041258,16.1337830625282));
#67790=CARTESIAN_POINT('Ctrl Pts',(30.4758334589096,1.2374906559331,16.1404068749596));
#67791=CARTESIAN_POINT('Ctrl Pts',(30.2026344427889,1.31649705751482,16.1513204506313));
#67792=CARTESIAN_POINT('Ctrl Pts',(30.094862299376,1.33047991225226,16.1552394386714));
#67793=CARTESIAN_POINT('Ctrl Pts',(30.0000000000046,1.33373412263454,16.1584936490537));
#67794=CARTESIAN_POINT('Origin',(30.,-1.32966554433622E-14,16.));
#67795=CARTESIAN_POINT('Origin',(30.,-1.21864324187371E-14,15.78125));
#67796=CARTESIAN_POINT('',(30.0000000000002,-1.17524047358085,16.0625));
#67797=CARTESIAN_POINT('',(30.,-1.17524047358085,15.78125));
#67798=CARTESIAN_POINT('',(29.1765921258349,-0.838564036615843,16.));
#67799=CARTESIAN_POINT('Ctrl Pts',(30.0000000000004,-1.17524047358085,16.0625));
#67800=CARTESIAN_POINT('Ctrl Pts',(29.8936372832897,-1.17524047358089,16.0559685129868));
#67801=CARTESIAN_POINT('Ctrl Pts',(29.7875857388152,-1.16080842474563,16.0489444642731));
#67802=CARTESIAN_POINT('Ctrl Pts',(29.5893382840682,-1.10559796441283,16.034813132098));
#67803=CARTESIAN_POINT('Ctrl Pts',(29.4977179176601,-1.06709869274158,16.0278219954706));
#67804=CARTESIAN_POINT('Ctrl Pts',(29.3263212626278,-0.968061456605931,
16.0137856854629));
#67805=CARTESIAN_POINT('Ctrl Pts',(29.2472234502441,-0.90791877416947,16.0067961899552));
#67806=CARTESIAN_POINT('Ctrl Pts',(29.176592125834,-0.838564036614912,15.9999999999999));
#67807=CARTESIAN_POINT('Origin',(30.,-1.32966554433622E-14,16.));
#67808=CARTESIAN_POINT('Origin',(30.,-1.21864324187371E-14,15.78125));
#67809=CARTESIAN_POINT('',(30.0000000000002,-1.17524047358085,16.5625));
#67810=CARTESIAN_POINT('',(30.,-1.17524047358085,16.5));
#67811=CARTESIAN_POINT('',(30.,-1.17524047358085,15.78125));
#67812=CARTESIAN_POINT('Ctrl Pts',(30.0000000000004,-1.17524047358085,16.5625));
#67813=CARTESIAN_POINT('Ctrl Pts',(29.8712710011335,-1.17524047358089,16.5545950516279));
#67814=CARTESIAN_POINT('Ctrl Pts',(29.7432544697015,-1.15409887958747,16.5459843057103));
#67815=CARTESIAN_POINT('Ctrl Pts',(29.4749058017838,-1.06268366571272,16.5262646272929));
#67816=CARTESIAN_POINT('Ctrl Pts',(29.3400104190766,-0.984598569044377,
16.515212607152));
#67817=CARTESIAN_POINT('Ctrl Pts',(29.1121607207208,-0.784303734398693,
16.4941196868072));
#67818=CARTESIAN_POINT('Ctrl Pts',(29.0200231478196,-0.665589512335134,
16.4846952710458));
#67819=CARTESIAN_POINT('Ctrl Pts',(28.8817974975863,-0.393869611486594,
16.465428299239));
#67820=CARTESIAN_POINT('Ctrl Pts',(28.83947486215,-0.242215228858268,16.4546748700446));
#67821=CARTESIAN_POINT('Ctrl Pts',(28.8167032491755,0.0653802904577292,
16.4328640487538));
#67822=CARTESIAN_POINT('Ctrl Pts',(28.8351718353917,0.218291541824621,16.422021498172));
#67823=CARTESIAN_POINT('Ctrl Pts',(28.9287391651494,0.506051914833821,16.4016171370023));
#67824=CARTESIAN_POINT('Ctrl Pts',(29.0019741006921,0.638460005621421,16.3928173224174));
#67825=CARTESIAN_POINT('Ctrl Pts',(29.1986594960153,0.873851822283252,16.3723938102577));
#67826=CARTESIAN_POINT('Ctrl Pts',(29.3222166226463,0.972810188230982,16.3612980106481));
#67827=CARTESIAN_POINT('Ctrl Pts',(29.5955374213776,1.11370354874836,16.3395188200451));
#67828=CARTESIAN_POINT('Ctrl Pts',(29.7416409158841,1.1563714827732,16.3290342066007));
#67829=CARTESIAN_POINT('Ctrl Pts',(30.0452139523297,1.18442751027465,16.309397801581));
#67830=CARTESIAN_POINT('Ctrl Pts',(30.1998697024494,1.16832333055968,16.2999812279383));
#67831=CARTESIAN_POINT('Ctrl Pts',(30.4949641982123,1.07710916023858,16.2786262781941));
#67832=CARTESIAN_POINT('Ctrl Pts',(30.6323783558426,1.00262103976947,16.2675471121926));
#67833=CARTESIAN_POINT('Ctrl Pts',(30.8661146099677,0.80826573510396,16.246303290685));
#67834=CARTESIAN_POINT('Ctrl Pts',(30.9615634972897,0.691955855651338,16.2365648418493));
#67835=CARTESIAN_POINT('Ctrl Pts',(31.1071384709944,0.423965303495795,16.217562308738));
#67836=CARTESIAN_POINT('Ctrl Pts',(31.153539286677,0.273539680121433,16.2068960077584));
#67837=CARTESIAN_POINT('Ctrl Pts',(31.1846742020807,-0.0336925499575308,
16.1851109463897));
#67838=CARTESIAN_POINT('Ctrl Pts',(31.1702391074247,-0.187447361382806,
16.174208581095));
#67839=CARTESIAN_POINT('Ctrl Pts',(31.0842361864784,-0.477469105777865,
16.1536438717926));
#67840=CARTESIAN_POINT('Ctrl Pts',(31.0147909316618,-0.611342914691707,
16.1448082262658));
#67841=CARTESIAN_POINT('Ctrl Pts',(30.8246452237759,-0.851973319529638,
16.1246005735716));
#67842=CARTESIAN_POINT('Ctrl Pts',(30.7034471847234,-0.954486386541281,
16.1135236126058));
#67843=CARTESIAN_POINT('Ctrl Pts',(30.4332129266933,-1.10289061678379,16.0916676708875));
#67844=CARTESIAN_POINT('Ctrl Pts',(30.2878849143487,-1.14942616400118,16.0810935566577));
#67845=CARTESIAN_POINT('Ctrl Pts',(30.0919105154022,-1.17254804866719,16.0682394674743));
#67846=CARTESIAN_POINT('Ctrl Pts',(30.0459321343385,-1.17524047358084,16.0653205855228));
#67847=CARTESIAN_POINT('Ctrl Pts',(30.0000000000004,-1.17524047358085,16.0625));
#67848=CARTESIAN_POINT('Ctrl Pts',(29.9999999999986,-1.17524047358085,15.9999999999999));
#67849=CARTESIAN_POINT('Ctrl Pts',(30.1214028111116,-1.17524047358099,16.0074550642242));
#67850=CARTESIAN_POINT('Ctrl Pts',(30.2421537204218,-1.15643017464734,16.0155369920666));
#67851=CARTESIAN_POINT('Ctrl Pts',(30.4776301337898,-1.08113291233427,16.0326666201836));
#67852=CARTESIAN_POINT('Ctrl Pts',(30.5903997908,-1.02391620718435,16.0416200885134));
#67853=CARTESIAN_POINT('Ctrl Pts',(30.8179173133188,-0.858187726048923,
16.0614671043063));
#67854=CARTESIAN_POINT('Ctrl Pts',(30.9244135286053,-0.742266950950034,
16.0721166138301));
#67855=CARTESIAN_POINT('Ctrl Pts',(31.0824458543846,-0.481384401141323,
16.0910702726526));
#67856=CARTESIAN_POINT('Ctrl Pts',(31.1347636661213,-0.340257482296023,
16.1008732014181));
#67857=CARTESIAN_POINT('Ctrl Pts',(31.1847167047507,-0.0402726429290417,
16.1221443686182));
#67858=CARTESIAN_POINT('Ctrl Pts',(31.1797095913038,0.116033015525934,16.1332276080324));
#67859=CARTESIAN_POINT('Ctrl Pts',(31.1096057651028,0.416692954381308,16.1545466448319));
#67860=CARTESIAN_POINT('Ctrl Pts',(31.0456145958404,0.558153128413804,16.1639131875247));
#67861=CARTESIAN_POINT('Ctrl Pts',(30.868452148125,0.806074678480504,16.1835820667589));
#67862=CARTESIAN_POINT('Ctrl Pts',(30.7578944192075,0.910792535772415,16.1940837990854));
#67863=CARTESIAN_POINT('Ctrl Pts',(30.4982839285527,1.07586594639843,16.2158783446996));
#67864=CARTESIAN_POINT('Ctrl Pts',(30.350445183185,1.13268560339106,16.2269712473271));
#67865=CARTESIAN_POINT('Ctrl Pts',(30.0480054721768,1.18378716120051,16.2473551076386));
#67866=CARTESIAN_POINT('Ctrl Pts',(29.8968386090012,1.18026105605562,16.2561569026374));
#67867=CARTESIAN_POINT('Ctrl Pts',(29.6011798659176,1.11599305250821,16.276591159187));
#67868=CARTESIAN_POINT('Ctrl Pts',(29.4597499374869,1.05480717934155,16.2874453099545));
#67869=CARTESIAN_POINT('Ctrl Pts',(29.2055652972218,0.87997645163687,16.3092526000714));
#67870=CARTESIAN_POINT('Ctrl Pts',(29.0959568884663,0.766951615708884,16.3199905502909));
#67871=CARTESIAN_POINT('Ctrl Pts',(28.9310246543964,0.510549118020342,16.3392090818415));
#67872=CARTESIAN_POINT('Ctrl Pts',(28.8749728808886,0.371095429589151,16.348686560472));
#67873=CARTESIAN_POINT('Ctrl Pts',(28.8169184420094,0.0732292943615943,
16.3698074957134));
#67874=CARTESIAN_POINT('Ctrl Pts',(28.817543647408,-0.0827153411142831,
16.3808651359001));
#67875=CARTESIAN_POINT('Ctrl Pts',(28.8792006517981,-0.386085589929172,
16.4023763539327));
#67876=CARTESIAN_POINT('Ctrl Pts',(28.9398691853048,-0.530428612710414,
16.4120388426041));
#67877=CARTESIAN_POINT('Ctrl Pts',(29.1111806434797,-0.783487027051828,
16.4315305472161));
#67878=CARTESIAN_POINT('Ctrl Pts',(29.2187204550675,-0.890749010718532,
16.441937155047));
#67879=CARTESIAN_POINT('Ctrl Pts',(29.4732317621912,-1.06214794881238,16.4636428352494));
#67880=CARTESIAN_POINT('Ctrl Pts',(29.6190899112583,-1.1227476098516,16.4747481293347));
#67881=CARTESIAN_POINT('Ctrl Pts',(29.8476395120001,-1.16783357420714,16.490381294589));
#67882=CARTESIAN_POINT('Ctrl Pts',(29.9238084968367,-1.17524047358085,16.4953212570267));
#67883=CARTESIAN_POINT('Ctrl Pts',(30.,-1.17524047358085,16.5));
#67884=CARTESIAN_POINT('Origin',(30.,-1.21864324187371E-14,15.78125));
#67885=CARTESIAN_POINT('',(30.,-1.17524047358085,17.0625));
#67886=CARTESIAN_POINT('',(30.0000000000001,-1.17524047358085,17.));
#67887=CARTESIAN_POINT('',(30.,-1.17524047358085,15.78125));
#67888=CARTESIAN_POINT('Ctrl Pts',(30.,-1.17524047358085,17.0625));
#67889=CARTESIAN_POINT('Ctrl Pts',(29.8500434788821,-1.17524047358086,17.0532915188657));
#67890=CARTESIAN_POINT('Ctrl Pts',(29.7013448813168,-1.14654165820119,17.0431428036379));
#67891=CARTESIAN_POINT('Ctrl Pts',(29.4194581258723,-1.03331719487298,17.0218185633632));
#67892=CARTESIAN_POINT('Ctrl Pts',(29.2895397758247,-0.948696042884902,
17.0108404436342));
#67893=CARTESIAN_POINT('Ctrl Pts',(29.0728347660888,-0.737413048700427,
16.9900423213744));
#67894=CARTESIAN_POINT('Ctrl Pts',(28.9869014388118,-0.614031092098323,
16.9810393937031));
#67895=CARTESIAN_POINT('Ctrl Pts',(28.8628735458866,-0.335358890642938,
16.9612794518217));
#67896=CARTESIAN_POINT('Ctrl Pts',(28.82846267168,-0.181667965469806,16.9503816165397));
#67897=CARTESIAN_POINT('Ctrl Pts',(28.8217124648996,0.125982959524893,16.9285668665722));
#67898=CARTESIAN_POINT('Ctrl Pts',(28.8478169965895,0.276986540894418,16.9178595840512));
#67899=CARTESIAN_POINT('Ctrl Pts',(28.9558731518301,0.560261316962501,16.89777328523));
#67900=CARTESIAN_POINT('Ctrl Pts',(29.0365906245512,0.68988311408331,16.8888684608487));
#67901=CARTESIAN_POINT('Ctrl Pts',(29.2459337687842,0.914815990147539,16.868038474302));
#67902=CARTESIAN_POINT('Ctrl Pts',(29.3738173058995,1.00667300394252,16.8569287693601));
#67903=CARTESIAN_POINT('Ctrl Pts',(29.6525904034611,1.13269913332434,16.8353418646716));
#67904=CARTESIAN_POINT('Ctrl Pts',(29.7999172965718,1.16777128086699,16.825051424181));
#67905=CARTESIAN_POINT('Ctrl Pts',(30.1064062467105,1.18085135988937,16.8057669130232));
#67906=CARTESIAN_POINT('Ctrl Pts',(30.2627337376109,1.15617395633467,16.7956901530542));
#67907=CARTESIAN_POINT('Ctrl Pts',(30.5539694020395,1.04785975388265,16.7739659051239));
#67908=CARTESIAN_POINT('Ctrl Pts',(30.6863296582614,0.96635719030164,16.7629483992302));
#67909=CARTESIAN_POINT('Ctrl Pts',(30.9084297587183,0.760352988428474,16.7420061299136));
#67910=CARTESIAN_POINT('Ctrl Pts',(30.9973576321623,0.639251123876904,16.7328276824508));
#67911=CARTESIAN_POINT('Ctrl Pts',(31.1283061935881,0.363925745860841,16.7133050553655));
#67912=CARTESIAN_POINT('Ctrl Pts',(31.1665770325591,0.21117202309341,16.7024736747387));
#67913=CARTESIAN_POINT('Ctrl Pts',(31.1811107740607,-0.0965571386816749,
16.6806533771987));
#67914=CARTESIAN_POINT('Ctrl Pts',(31.1587010998539,-0.248535347285279,
16.6698769863224));
#67915=CARTESIAN_POINT('Ctrl Pts',(31.0576874952353,-0.534014859537023,
16.6496343552276));
#67916=CARTESIAN_POINT('Ctrl Pts',(30.9806443499075,-0.664990212129755,
16.6408093669374));
#67917=CARTESIAN_POINT('Ctrl Pts',(30.7774744062741,-0.895077677115282,
16.6201757128395));
#67918=CARTESIAN_POINT('Ctrl Pts',(30.6516599935628,-0.990433515302137,
16.6090690216144));
#67919=CARTESIAN_POINT('Ctrl Pts',(30.3754577665479,-1.12376244747141,16.5873810764564));
#67920=CARTESIAN_POINT('Ctrl Pts',(30.2286809422177,-1.16255586785604,16.5769924813814));
#67921=CARTESIAN_POINT('Ctrl Pts',(30.0523684587312,-1.17436628643519,16.5657468184328));
#67922=CARTESIAN_POINT('Ctrl Pts',(30.0261713894288,-1.17524047358084,16.5641071241452));
#67923=CARTESIAN_POINT('Ctrl Pts',(30.0000000000004,-1.17524047358085,16.5625));
#67924=CARTESIAN_POINT('Ctrl Pts',(30.,-1.17524047358085,16.5));
#67925=CARTESIAN_POINT('Ctrl Pts',(30.073608323754,-1.17524047358085,16.5045201159347));
#67926=CARTESIAN_POINT('Ctrl Pts',(30.1472072638744,-1.16832718018639,16.5092847577281));
#67927=CARTESIAN_POINT('Ctrl Pts',(30.369441082132,-1.12600740446215,16.5244320137475));
#67928=CARTESIAN_POINT('Ctrl Pts',(30.5120596783037,-1.06872004059094,16.5352209411127));
#67929=CARTESIAN_POINT('Ctrl Pts',(30.770540092832,-0.900978381413799,16.5570406907631));
#67930=CARTESIAN_POINT('Ctrl Pts',(30.8831588051698,-0.790914789141215,
16.5678585095693));
#67931=CARTESIAN_POINT('Ctrl Pts',(31.0548992370084,-0.539025681589464,
16.5873351001607));
#67932=CARTESIAN_POINT('Ctrl Pts',(31.1146464335618,-0.40117702528207,16.5965535505072));
#67933=CARTESIAN_POINT('Ctrl Pts',(31.1805926646682,-0.105443065986663,
16.6175232985392));
#67934=CARTESIAN_POINT('Ctrl Pts',(31.1842348048322,0.0500317177053629,
16.6285476227227));
#67935=CARTESIAN_POINT('Ctrl Pts',(31.1309192517252,0.355959076743607,16.650240158982));
#67936=CARTESIAN_POINT('Ctrl Pts',(31.0735350939833,0.503164977113694,16.6602491192277));
#67937=CARTESIAN_POINT('Ctrl Pts',(30.9079406905516,0.761174069707616,16.6795652728517));
#67938=CARTESIAN_POINT('Ctrl Pts',(30.8033709986449,0.870813111599809,16.6898737681392));
#67939=CARTESIAN_POINT('Ctrl Pts',(30.5539282192807,1.04817985026245,16.7114797826742));
#67940=CARTESIAN_POINT('Ctrl Pts',(30.4100715847777,1.1123704677318,16.7225894812308));
#67941=CARTESIAN_POINT('Ctrl Pts',(30.1103488398163,1.179778360742,16.7433846194973));
#67942=CARTESIAN_POINT('Ctrl Pts',(29.957856215253,1.1841771173115,16.7522711143702));
#67943=CARTESIAN_POINT('Ctrl Pts',(29.6587896018035,1.13483145500942,16.7723855875496));
#67944=CARTESIAN_POINT('Ctrl Pts',(29.5151366653971,1.08127741557342,16.7831056710399));
#67945=CARTESIAN_POINT('Ctrl Pts',(29.252747940286,0.920389087589127,16.80492244475));
#67946=CARTESIAN_POINT('Ctrl Pts',(29.137337166046,0.813224513877345,16.8158089365411));
#67947=CARTESIAN_POINT('Ctrl Pts',(28.9591466935998,0.565701034789473,16.8355268312788));
#67948=CARTESIAN_POINT('Ctrl Pts',(28.8958814901205,0.429333298679841,16.8445570602832));
#67949=CARTESIAN_POINT('Ctrl Pts',(28.8225467136217,0.135655218439199,16.8653810311245));
#67950=CARTESIAN_POINT('Ctrl Pts',(28.8149165149687,-0.0192736957647923,
16.8763666490815));
#67951=CARTESIAN_POINT('Ctrl Pts',(28.8600359901893,-0.325574492875678,
16.8980856648912));
#67952=CARTESIAN_POINT('Ctrl Pts',(28.9132427466147,-0.473736863683124,
16.908393840582));
#67953=CARTESIAN_POINT('Ctrl Pts',(29.0711075417097,-0.735375844223955,
16.9273640300312));
#67954=CARTESIAN_POINT('Ctrl Pts',(29.1722563389189,-0.847605887640186,
16.9375543168196));
#67955=CARTESIAN_POINT('Ctrl Pts',(29.4158032201734,-1.03154789820323,16.9590313959273));
#67956=CARTESIAN_POINT('Ctrl Pts',(29.5572939812199,-1.09972494823153,16.97013714563));
#67957=CARTESIAN_POINT('Ctrl Pts',(29.8035947514828,-1.1629117021743,16.9875021095456));
#67958=CARTESIAN_POINT('Ctrl Pts',(29.9016938547886,-1.17524047358087,16.9939632483014));
#67959=CARTESIAN_POINT('Ctrl Pts',(30.0000000000002,-1.17524047358085,17.));
#67960=CARTESIAN_POINT('Origin',(30.,-1.21864324187371E-14,15.78125));
#67961=CARTESIAN_POINT('',(30.,-1.17524047358085,17.5625));
#67962=CARTESIAN_POINT('',(30.0000000000003,-1.17524047358085,17.5));
#67963=CARTESIAN_POINT('',(30.,-1.17524047358085,15.78125));
#67964=CARTESIAN_POINT('Ctrl Pts',(29.9999999999999,-1.17524047358085,17.5625));
#67965=CARTESIAN_POINT('Ctrl Pts',(29.9853039952848,-1.17524047358085,17.5615975525362));
#67966=CARTESIAN_POINT('Ctrl Pts',(29.9705988101993,-1.17496482223763,17.560684768457));
#67967=CARTESIAN_POINT('Ctrl Pts',(29.8000675583885,-1.16856010727206,17.5499857698916));
#67968=CARTESIAN_POINT('Ctrl Pts',(29.6469974366404,-1.13175546252589,17.53928122759));
#67969=CARTESIAN_POINT('Ctrl Pts',(29.3669883306193,-1.00191414640604,17.51748315987));
#67970=CARTESIAN_POINT('Ctrl Pts',(29.2422159979844,-0.911212372037981,
17.5066054643129));
#67971=CARTESIAN_POINT('Ctrl Pts',(29.0365009193432,-0.689398438610156,
17.4861088470066));
#67972=CARTESIAN_POINT('Ctrl Pts',(28.9566358845376,-0.561238966410083,
17.477296037423));
#67973=CARTESIAN_POINT('Ctrl Pts',(28.8466374529962,-0.274946499836391,
17.4569957617908));
#67974=CARTESIAN_POINT('Ctrl Pts',(28.8202715815142,-0.118602529031394,
17.4459098057446));
#67975=CARTESIAN_POINT('Ctrl Pts',(28.8303001790337,0.189193535952347,17.4240847642671));
#67976=CARTESIAN_POINT('Ctrl Pts',(28.8642598713376,0.337792935402822,17.413547956213));
#67977=CARTESIAN_POINT('Ctrl Pts',(28.9875332190235,0.616132121834573,17.3938116275857));
#67978=CARTESIAN_POINT('Ctrl Pts',(29.0764632180064,0.742831294355827,17.3845427667776));
#67979=CARTESIAN_POINT('Ctrl Pts',(29.2992557500629,0.956131495581886,17.3632993064049));
#67980=CARTESIAN_POINT('Ctrl Pts',(29.431365525465,1.04013508414132,17.3522085112739));
#67981=CARTESIAN_POINT('Ctrl Pts',(29.7152659077079,1.14996876403328,17.3308808348058));
#67982=CARTESIAN_POINT('Ctrl Pts',(29.8634965281812,1.17678287245723,17.3209370444755));
#67983=CARTESIAN_POINT('Ctrl Pts',(30.1685869462377,1.17348866615416,17.3020853596773));
#67984=CARTESIAN_POINT('Ctrl Pts',(30.3225567032231,1.14080144678595,17.291471550985));
#67985=CARTESIAN_POINT('Ctrl Pts',(30.6062809135034,1.01837161133764,17.269708112041));
#67986=CARTESIAN_POINT('Ctrl Pts',(30.7337302229979,0.930754504232001,17.2587753925441));
#67987=CARTESIAN_POINT('Ctrl Pts',(30.9451039338725,0.714326579760782,17.2381222459404));
#67988=CARTESIAN_POINT('Ctrl Pts',(31.0280898505948,0.588650269560749,17.2292397036887));
#67989=CARTESIAN_POINT('Ctrl Pts',(31.1457356989614,0.305390771140385,17.209154488167));
#67990=CARTESIAN_POINT('Ctrl Pts',(31.1762844162632,0.149369866697047,17.1980914399405));
#67991=CARTESIAN_POINT('Ctrl Pts',(31.1741828829317,-0.159374372954329,
17.1761991657924));
#67992=CARTESIAN_POINT('Ctrl Pts',(31.1439148549186,-0.309160960295119,
17.1655781772438));
#67993=CARTESIAN_POINT('Ctrl Pts',(31.0278391895685,-0.589863984020037,
17.1456742348851));
#67994=CARTESIAN_POINT('Ctrl Pts',(30.9428415818715,-0.717947604052165,
17.1366104494432));
#67995=CARTESIAN_POINT('Ctrl Pts',(30.7264277284841,-0.936836489561928,
17.1155605491468));
#67996=CARTESIAN_POINT('Ctrl Pts',(30.5962729133073,-1.02460346942682,17.10445637729));
#67997=CARTESIAN_POINT('Ctrl Pts',(30.3147671476396,-1.1421454095557,17.0830024620243));
#67998=CARTESIAN_POINT('Ctrl Pts',(30.1669216238945,-1.17291749944691,17.0728326267459));
#67999=CARTESIAN_POINT('Ctrl Pts',(30.0114948569556,-1.17519832475422,17.06320736676));
#68000=CARTESIAN_POINT('Ctrl Pts',(30.0057465951805,-1.17524047358085,17.0628528850424));
#68001=CARTESIAN_POINT('Ctrl Pts',(30.,-1.17524047358085,17.0625));
#68002=CARTESIAN_POINT('Ctrl Pts',(30.0000000000002,-1.17524047358085,17.));
#68003=CARTESIAN_POINT('Ctrl Pts',(30.0532026451947,-1.17524047358084,17.0032670506819));
#68004=CARTESIAN_POINT('Ctrl Pts',(30.1064500803375,-1.17162840402792,17.0066649131742));
#68005=CARTESIAN_POINT('Ctrl Pts',(30.3094843531048,-1.14383638948677,17.0201181063427));
#68006=CARTESIAN_POINT('Ctrl Pts',(30.4541770343026,-1.0944632219883,17.0307538106078));
#68007=CARTESIAN_POINT('Ctrl Pts',(30.7220117324143,-0.94057404805184,17.0526568626846));
#68008=CARTESIAN_POINT('Ctrl Pts',(30.8414109395085,-0.835479490322757,
17.0637148850572));
#68009=CARTESIAN_POINT('Ctrl Pts',(31.0267110546809,-0.591037021798696,
17.0837601330781));
#68010=CARTESIAN_POINT('Ctrl Pts',(31.0933788874677,-0.456058910657645,
17.0926620146465));
#68011=CARTESIAN_POINT('Ctrl Pts',(31.1737387540124,-0.16438811954927,17.1133436536858));
#68012=CARTESIAN_POINT('Ctrl Pts',(31.1851490819135,-0.0100732318962758,
17.1242857325711));
#68013=CARTESIAN_POINT('Ctrl Pts',(31.1477867853133,0.296739304676255,17.1460410345334));
#68014=CARTESIAN_POINT('Ctrl Pts',(31.0983725298423,0.446176311422578,17.156637235205));
#68015=CARTESIAN_POINT('Ctrl Pts',(30.9473434585081,0.711342976495719,17.1754395336164));
#68016=CARTESIAN_POINT('Ctrl Pts',(30.8493881217234,0.825870653120103,17.1854545855523));
#68017=CARTESIAN_POINT('Ctrl Pts',(30.6112318646727,1.01569990967513,17.2068093638384));
#68018=CARTESIAN_POINT('Ctrl Pts',(30.4719800604887,1.0874234537732,17.2179033608764));
#68019=CARTESIAN_POINT('Ctrl Pts',(30.1755334231398,1.17210985582506,17.2391099087106));
#68020=CARTESIAN_POINT('Ctrl Pts',(30.0214941231326,1.18498177307235,17.2483347304275));
#68021=CARTESIAN_POINT('Ctrl Pts',(29.7191034448427,1.1511421779865,17.2681035786673));
#68022=CARTESIAN_POINT('Ctrl Pts',(29.5735822533488,1.10552321949792,17.2786570590835));
#68023=CARTESIAN_POINT('Ctrl Pts',(29.3025973986068,0.958895356196027,17.3004961143537));
#68024=CARTESIAN_POINT('Ctrl Pts',(29.1808306521913,0.85722095928387,17.3115782643265));
#68025=CARTESIAN_POINT('Ctrl Pts',(28.9891285746956,0.617827320312939,17.3318376420863));
#68026=CARTESIAN_POINT('Ctrl Pts',(28.918785924397,0.484304768960115,17.3406591721831));
#68027=CARTESIAN_POINT('Ctrl Pts',(28.8309775509286,0.194817478373176,17.361185984716));
#68028=CARTESIAN_POINT('Ctrl Pts',(28.8155773691905,0.0412543792472424,
17.3720747561758));
#68029=CARTESIAN_POINT('Ctrl Pts',(28.8447173912596,-0.266085346871024,
17.3938674398171));
#68030=CARTESIAN_POINT('Ctrl Pts',(28.8901486797617,-0.416814366578493,
17.4045552538642));
#68031=CARTESIAN_POINT('Ctrl Pts',(29.0339735284972,-0.685700945089528,
17.423621321941));
#68032=CARTESIAN_POINT('Ctrl Pts',(29.1286271803726,-0.802582950507819,
17.4332789203108));
#68033=CARTESIAN_POINT('Ctrl Pts',(29.3609543925255,-0.998368963070605,
17.45448693977));
#68034=CARTESIAN_POINT('Ctrl Pts',(29.4977729352126,-1.07372697749091,17.4655603714348));
#68035=CARTESIAN_POINT('Ctrl Pts',(29.7602131749374,-1.15682002764215,17.484622175217));
#68036=CARTESIAN_POINT('Ctrl Pts',(29.879837116137,-1.1752404735809,17.4926210768238));
#68037=CARTESIAN_POINT('Ctrl Pts',(30.0000000000005,-1.17524047358085,17.5));
#68038=CARTESIAN_POINT('Origin',(30.,-1.21864324187371E-14,15.78125));
#68039=CARTESIAN_POINT('',(29.9999999999998,-1.17524047358085,18.0625));
#68040=CARTESIAN_POINT('',(30.,-1.17524047358085,18.));
#68041=CARTESIAN_POINT('',(30.,-1.17524047358085,15.78125));
#68042=CARTESIAN_POINT('Ctrl Pts',(29.9999999999995,-1.17524047358085,18.0625));
#68043=CARTESIAN_POINT('Ctrl Pts',(29.9645254254169,-1.17524047358085,18.0603215888955));
#68044=CARTESIAN_POINT('Ctrl Pts',(29.929015100466,-1.17363438891304,18.0580840407407));
#68045=CARTESIAN_POINT('Ctrl Pts',(29.7382382629168,-1.15628718990462,18.0457538558988));
#68046=CARTESIAN_POINT('Ctrl Pts',(29.5872914572777,-1.11138228831714,18.0348925171245));
#68047=CARTESIAN_POINT('Ctrl Pts',(29.315235711072,-0.96715790012321,18.0130729130751));
#68048=CARTESIAN_POINT('Ctrl Pts',(29.1959940490486,-0.870565282945587,
18.0023259907432));
#68049=CARTESIAN_POINT('Ctrl Pts',(29.0016396885941,-0.638155310236294,
17.9821513395236));
#68050=CARTESIAN_POINT('Ctrl Pts',(28.9280461950896,-0.504858426874225,
17.9732982357813));
#68051=CARTESIAN_POINT('Ctrl Pts',(28.8336569152641,-0.212647772939916,
17.9525783164326));
#68052=CARTESIAN_POINT('Ctrl Pts',(28.8157570812338,-0.0559802507924535,
17.9414694181781));
#68053=CARTESIAN_POINT('Ctrl Pts',(28.841716723376,0.249283949869151,17.9198239048041));
#68054=CARTESIAN_POINT('Ctrl Pts',(28.8830393993721,0.395199804389445,17.9094773801424));
#68055=CARTESIAN_POINT('Ctrl Pts',(29.0209639808548,0.668562290928518,17.8900939367334));
#68056=CARTESIAN_POINT('Ctrl Pts',(29.1181759703235,0.792402282110926,17.8802238069267));
#68057=CARTESIAN_POINT('Ctrl Pts',(29.3540263292146,0.993822233016871,17.8585996950535));
#68058=CARTESIAN_POINT('Ctrl Pts',(29.4898462594122,1.06991069869815,17.8475616886318));
#68059=CARTESIAN_POINT('Ctrl Pts',(29.7781387158762,1.16368326761588,17.8265337315072));
#68060=CARTESIAN_POINT('Ctrl Pts',(29.9272121099849,1.18239624377936,17.817223433802));
#68061=CARTESIAN_POINT('Ctrl Pts',(30.231427568808,1.16273575019751,17.7978452321702));
#68062=CARTESIAN_POINT('Ctrl Pts',(30.3834744853667,1.1218012564522,17.7870571039388));
#68063=CARTESIAN_POINT('Ctrl Pts',(30.6595367886018,0.984593855649311,17.7652402449678));
#68064=CARTESIAN_POINT('Ctrl Pts',(30.78153371397,0.890859052478792,17.7544254485094));
#68065=CARTESIAN_POINT('Ctrl Pts',(30.9814968973686,0.663646825098318,17.7340906520159));
#68066=CARTESIAN_POINT('Ctrl Pts',(31.0581916579204,0.532910080900297,17.7252873077101));
#68067=CARTESIAN_POINT('Ctrl Pts',(31.1603311881744,0.243593094566313,17.7047725710215));
#68068=CARTESIAN_POINT('Ctrl Pts',(31.1824208985569,0.0870303935487086,
17.6936711053685));
#68069=CARTESIAN_POINT('Ctrl Pts',(31.1643265939555,-0.219589452433675,
17.6719294666093));
#68070=CARTESIAN_POINT('Ctrl Pts',(31.126629625228,-0.366880394031282,17.6614854379963));
#68071=CARTESIAN_POINT('Ctrl Pts',(30.9959732548856,-0.642739672382233,
17.6419249533869));
#68072=CARTESIAN_POINT('Ctrl Pts',(30.9029171297163,-0.76800751067264,17.6323839709445));
#68073=CARTESIAN_POINT('Ctrl Pts',(30.6735549835348,-0.97540763183831,17.6109462657373));
#68074=CARTESIAN_POINT('Ctrl Pts',(30.5395284406378,-1.05546393695081,17.5998777123224));
#68075=CARTESIAN_POINT('Ctrl Pts',(30.2672665806154,-1.15230702152505,17.5797252955804));
#68076=CARTESIAN_POINT('Ctrl Pts',(30.1340643685791,-1.17524047358085,17.5707325810151));
#68077=CARTESIAN_POINT('Ctrl Pts',(29.9999999999999,-1.17524047358085,17.5625));
#68078=CARTESIAN_POINT('Ctrl Pts',(30.0000000000005,-1.17524047358085,17.5));
#68079=CARTESIAN_POINT('Ctrl Pts',(30.033668671514,-1.17524047358084,17.5020675147979));
#68080=CARTESIAN_POINT('Ctrl Pts',(30.0673733741507,-1.17379373295066,17.504188534545));
#68081=CARTESIAN_POINT('Ctrl Pts',(30.2512194694897,-1.15793171152857,17.5160404635345));
#68082=CARTESIAN_POINT('Ctrl Pts',(30.3974945854731,-1.11619705184184,17.5265025277916));
#68083=CARTESIAN_POINT('Ctrl Pts',(30.6715286389123,-0.977122112696594,
17.5482610478741));
#68084=CARTESIAN_POINT('Ctrl Pts',(30.7956391457863,-0.8790277241657,17.559360198049));
#68085=CARTESIAN_POINT('Ctrl Pts',(30.9938921656194,-0.644908297614295,
17.579834863399));
#68086=CARTESIAN_POINT('Ctrl Pts',(31.0680432549382,-0.51284781086492,17.5886352571811));
#68087=CARTESIAN_POINT('Ctrl Pts',(31.1634155774875,-0.225635628704456,
17.6090007475224));
#68088=CARTESIAN_POINT('Ctrl Pts',(31.1828424433655,-0.0729412614644995,
17.6198279193986));
#68089=CARTESIAN_POINT('Ctrl Pts',(31.1620678214981,0.234707081573543,17.6416424862861));
#68090=CARTESIAN_POINT('Ctrl Pts',(31.120724241081,0.386638085314584,17.6524155299848));
#68091=CARTESIAN_POINT('Ctrl Pts',(30.9842587758127,0.659238100700609,17.6717449084903));
#68092=CARTESIAN_POINT('Ctrl Pts',(30.8929036275603,0.778529076192667,17.6811039637465));
#68093=CARTESIAN_POINT('Ctrl Pts',(30.6664518626416,0.98022024209091,17.7021605454119));
#68094=CARTESIAN_POINT('Ctrl Pts',(30.5321662358965,1.05914504613978,17.7132048926221));
#68095=CARTESIAN_POINT('Ctrl Pts',(30.2394356343315,1.16107865610412,17.7347947253164));
#68096=CARTESIAN_POINT('Ctrl Pts',(30.0837395746803,1.18253750639866,17.7445990404306));
#68097=CARTESIAN_POINT('Ctrl Pts',(29.7783085058998,1.16389753061854,17.7640157086725));
#68098=CARTESIAN_POINT('Ctrl Pts',(29.6313883618284,1.12601470121935,17.7743808208261));
#68099=CARTESIAN_POINT('Ctrl Pts',(29.3545393068819,0.994469365010162,17.7960452510406));
#68100=CARTESIAN_POINT('Ctrl Pts',(29.2282096618696,0.899966183720928,17.8071533516094));
#68101=CARTESIAN_POINT('Ctrl Pts',(29.0235241701317,0.671134004766118,17.8278355674102));
#68102=CARTESIAN_POINT('Ctrl Pts',(28.9455840780504,0.540492245953914,17.8366750601186));
#68103=CARTESIAN_POINT('Ctrl Pts',(28.8428376707835,0.255550540540784,17.8568795566889));
#68104=CARTESIAN_POINT('Ctrl Pts',(28.819515816648,0.103803872119581,17.8676395296357));
#68105=CARTESIAN_POINT('Ctrl Pts',(28.8321334408652,-0.203924479248023,
17.8894597697118));
#68106=CARTESIAN_POINT('Ctrl Pts',(28.8694569005926,-0.356918085677502,
17.9003081598831));
#68107=CARTESIAN_POINT('Ctrl Pts',(28.9987062002081,-0.633072693900888,
17.9198895855878));
#68108=CARTESIAN_POINT('Ctrl Pts',(29.0868937988439,-0.754733453808526,
17.9290197269592));
#68109=CARTESIAN_POINT('Ctrl Pts',(29.3076626510103,-0.962047131353844,
17.9499266732212));
#68110=CARTESIAN_POINT('Ctrl Pts',(29.439425880769,-1.04432722335896,17.9609350833968));
#68111=CARTESIAN_POINT('Ctrl Pts',(29.7165797609128,-1.14942800619046,17.981680673977));
#68112=CARTESIAN_POINT('Ctrl Pts',(29.857771536572,-1.17524047358086,17.9912660809114));
#68113=CARTESIAN_POINT('Ctrl Pts',(30.0000000000001,-1.17524047358085,18.));
#68114=CARTESIAN_POINT('Origin',(30.,-1.21864324187371E-14,15.78125));
#68115=CARTESIAN_POINT('',(29.9999999999999,-1.17524047358085,18.5625));
#68116=CARTESIAN_POINT('',(30.,-1.17524047358085,18.5));
#68117=CARTESIAN_POINT('',(30.,-1.17524047358085,15.78125));
#68118=CARTESIAN_POINT('Ctrl Pts',(29.9999999999998,-1.17524047358085,18.5625));
#68119=CARTESIAN_POINT('Ctrl Pts',(29.9448799883238,-1.17524047358085,18.5591152083026));
#68120=CARTESIAN_POINT('Ctrl Pts',(29.8897199177939,-1.17136342891428,18.5555905009623));
#68121=CARTESIAN_POINT('Ctrl Pts',(29.6792216999803,-1.14149919812993,18.5416054964814));
#68122=CARTESIAN_POINT('Ctrl Pts',(29.5295600411529,-1.08838822549331,18.5305321396985));
#68123=CARTESIAN_POINT('Ctrl Pts',(29.2651715824486,-0.929562358041593,
18.5086656889335));
#68124=CARTESIAN_POINT('Ctrl Pts',(29.1517563578462,-0.827380506823195,
18.4980783953365));
#68125=CARTESIAN_POINT('Ctrl Pts',(28.9690035888602,-0.584433789122884,
18.4782426038757));
#68126=CARTESIAN_POINT('Ctrl Pts',(28.9018681826973,-0.445680079983302,
18.4691020486872));
#68127=CARTESIAN_POINT('Ctrl Pts',(28.8237798560613,-0.147691887525462,
18.4479724586759));
#68128=CARTESIAN_POINT('Ctrl Pts',(28.8145788645707,0.00884554058040183,
18.4368727850612));
#68129=CARTESIAN_POINT('Ctrl Pts',(28.8567482751501,0.310649796974269,18.4154726075955));
#68130=CARTESIAN_POINT('Ctrl Pts',(28.9054833559201,0.453415390787842,18.4053494599629));
#68131=CARTESIAN_POINT('Ctrl Pts',(29.0569965845258,0.718468314308288,18.3865552266777));
#68132=CARTESIAN_POINT('Ctrl Pts',(29.1604683184012,0.83707730034545,18.3760428358642));
#68133=CARTESIAN_POINT('Ctrl Pts',(29.4058248734932,1.0255154952049,18.3542952223602));
#68134=CARTESIAN_POINT('Ctrl Pts',(29.544631443668,1.0942445155017,18.3433347331662));
#68135=CARTESIAN_POINT('Ctrl Pts',(29.8366929775619,1.17335763361873,18.3225950580774));
#68136=CARTESIAN_POINT('Ctrl Pts',(29.986714530993,1.18458952273488,18.3136472884771));
#68137=CARTESIAN_POINT('Ctrl Pts',(30.2898186404183,1.14957783224746,18.2937930749288));
#68138=CARTESIAN_POINT('Ctrl Pts',(30.4396462258347,1.10100720458506,18.2828705011767));
#68139=CARTESIAN_POINT('Ctrl Pts',(30.7078144176317,0.95036138884417,18.2610619591969));
#68140=CARTESIAN_POINT('Ctrl Pts',(30.8244348872713,0.851181456147988,18.250384268188));
#68141=CARTESIAN_POINT('Ctrl Pts',(31.0135314789776,0.613960284599869,18.2303619093383));
#68142=CARTESIAN_POINT('Ctrl Pts',(31.0842069749077,0.478217809229905,18.2214092168781));
#68143=CARTESIAN_POINT('Ctrl Pts',(31.1712537448649,0.183351777827692,18.2005010114207));
#68144=CARTESIAN_POINT('Ctrl Pts',(31.1852144107931,0.026684835425868,18.1893921542744));
#68145=CARTESIAN_POINT('Ctrl Pts',(31.151894218573,-0.277120859310672,18.1678500598715));
#68146=CARTESIAN_POINT('Ctrl Pts',(31.1071955868466,-0.421659698179358,
18.1576011759113));
#68147=CARTESIAN_POINT('Ctrl Pts',(30.9623980704004,-0.692609521716023,
18.1383888083414));
#68148=CARTESIAN_POINT('Ctrl Pts',(30.8611688824271,-0.815074867780112,
18.1281515944925));
#68149=CARTESIAN_POINT('Ctrl Pts',(30.6191698348665,-1.010677278137,18.1063561595037));
#68150=CARTESIAN_POINT('Ctrl Pts',(30.481744547401,-1.08294295672688,18.0953551039148));
#68151=CARTESIAN_POINT('Ctrl Pts',(30.2255864017037,-1.15894806928573,18.0769303627887));
#68152=CARTESIAN_POINT('Ctrl Pts',(30.1130100641695,-1.17524047358085,18.0694396851576));
#68153=CARTESIAN_POINT('Ctrl Pts',(29.9999999999995,-1.17524047358085,18.0625));
#68154=CARTESIAN_POINT('Ctrl Pts',(30.0000000000001,-1.17524047358085,18.));
#68155=CARTESIAN_POINT('Ctrl Pts',(30.0145244311397,-1.17524047358085,18.0008919115297));
#68156=CARTESIAN_POINT('Ctrl Pts',(30.0290585224951,-1.1749712210064,18.0017939622806));
#68157=CARTESIAN_POINT('Ctrl Pts',(30.1935181174434,-1.16886648233729,18.0121094792412));
#68158=CARTESIAN_POINT('Ctrl Pts',(30.3409577753235,-1.13464684718278,18.022376619604));
#68159=CARTESIAN_POINT('Ctrl Pts',(30.6202928748417,-1.01029888563142,18.0439385382044));
#68160=CARTESIAN_POINT('Ctrl Pts',(30.7486368752819,-0.919248747112441,
18.055047912384));
#68161=CARTESIAN_POINT('Ctrl Pts',(30.9593869332128,-0.695506306327382,
18.0759220888488));
#68162=CARTESIAN_POINT('Ctrl Pts',(31.0409497614259,-0.566191331080132,
18.084852802908));
#68163=CARTESIAN_POINT('Ctrl Pts',(31.1506054030915,-0.283424289026694,
18.1049030995926));
#68164=CARTESIAN_POINT('Ctrl Pts',(31.1775442736485,-0.132654402671248,
18.1155938113905));
#68165=CARTESIAN_POINT('Ctrl Pts',(31.1725598607287,0.174951078257229,18.1374053390341));
#68166=CARTESIAN_POINT('Ctrl Pts',(31.1390289434739,0.328840847644919,18.148317273857));
#68167=CARTESIAN_POINT('Ctrl Pts',(31.0165781905916,0.608264397522364,18.1681304919571));
#68168=CARTESIAN_POINT('Ctrl Pts',(30.9313199722933,0.732167484063905,18.1771012136858));
#68169=CARTESIAN_POINT('Ctrl Pts',(30.7158345492886,0.944633593585631,18.1978663898215));
#68170=CARTESIAN_POINT('Ctrl Pts',(30.5864762504196,1.02994768568734,18.208834685427));
#68171=CARTESIAN_POINT('Ctrl Pts',(30.3000115977578,1.14695518635867,18.2305741665317));
#68172=CARTESIAN_POINT('Ctrl Pts',(30.1454149851266,1.17656763909288,18.2410233510493));
#68173=CARTESIAN_POINT('Ctrl Pts',(29.8400425266379,1.17387642244061,18.2598709770579));
#68174=CARTESIAN_POINT('Ctrl Pts',(29.6921041520777,1.14400535739554,18.2700145693908));
#68175=CARTESIAN_POINT('Ctrl Pts',(29.4100579886469,1.02824734385133,18.2914384223622));
#68176=CARTESIAN_POINT('Ctrl Pts',(29.2794434337127,0.941343746808855,18.3025402156205));
#68177=CARTESIAN_POINT('Ctrl Pts',(29.061555804029,0.723734320476339,18.3236352554819));
#68178=CARTESIAN_POINT('Ctrl Pts',(28.9756558249342,0.595970538008072,18.3327412345668));
#68179=CARTESIAN_POINT('Ctrl Pts',(28.8579142725366,0.315809924655313,18.3526067159761));
#68180=CARTESIAN_POINT('Ctrl Pts',(28.8267878271973,0.166290213657428,18.3632087809973));
#68181=CARTESIAN_POINT('Ctrl Pts',(28.8228465258246,-0.142252171918218,
18.3850867421828));
#68182=CARTESIAN_POINT('Ctrl Pts',(28.8524261916584,-0.298357527348321,
18.3961557786154));
#68183=CARTESIAN_POINT('Ctrl Pts',(28.9683032793772,-0.582326286319503,
18.4162912860112));
#68184=CARTESIAN_POINT('Ctrl Pts',(29.0505638845767,-0.708574806470949,
18.4251522948912));
#68185=CARTESIAN_POINT('Ctrl Pts',(29.2606233813178,-0.926260402003281,
18.4457693278011));
#68186=CARTESIAN_POINT('Ctrl Pts',(29.3874559625716,-1.01460273580079,18.4566898874478));
#68187=CARTESIAN_POINT('Ctrl Pts',(29.670332667393,-1.13876808411125,18.4784628134696));
#68188=CARTESIAN_POINT('Ctrl Pts',(29.8241031351402,-1.17241612945781,18.4890984491449));
#68189=CARTESIAN_POINT('Ctrl Pts',(29.9866645216768,-1.17518374723239,18.4991790881359));
#68190=CARTESIAN_POINT('Ctrl Pts',(29.9933333092278,-1.17524047358085,18.4995906140276));
#68191=CARTESIAN_POINT('Ctrl Pts',(30.,-1.17524047358085,18.5));
#68192=CARTESIAN_POINT('Origin',(30.,-1.21864324187371E-14,15.78125));
#68193=CARTESIAN_POINT('',(30.,-1.17524047358085,19.0625));
#68194=CARTESIAN_POINT('',(29.9999999999998,-1.17524047358085,18.9999999999999));
#68195=CARTESIAN_POINT('',(30.,-1.17524047358085,15.78125));
#68196=CARTESIAN_POINT('Ctrl Pts',(30.,-1.17524047358085,19.0625));
#68197=CARTESIAN_POINT('Ctrl Pts',(29.9235115354988,-1.17524047358085,19.0578030213218));
#68198=CARTESIAN_POINT('Ctrl Pts',(29.84704716558,-1.16777574293408,19.0528428696387));
#68199=CARTESIAN_POINT('Ctrl Pts',(29.6182505756017,-1.12246086107485,19.0371864213689));
#68200=CARTESIAN_POINT('Ctrl Pts',(29.4724485773796,-1.06175746863862,19.0260808977107));
#68201=CARTESIAN_POINT('Ctrl Pts',(29.2180805672544,-0.890185564352666,
19.0043778847458));
#68202=CARTESIAN_POINT('Ctrl Pts',(29.1106251205818,-0.782854361416016,
18.9939740034863));
#68203=CARTESIAN_POINT('Ctrl Pts',(28.9394765622835,-0.529653947083613,
18.9744872677464));
#68204=CARTESIAN_POINT('Ctrl Pts',(28.8789010658566,-0.385229961133875,
18.9648156834562));
#68205=CARTESIAN_POINT('Ctrl Pts',(28.8174805423046,-0.0817855742350542,
18.9432992084794));
#68206=CARTESIAN_POINT('Ctrl Pts',(28.8169771571136,0.0741472763924911,
18.9322424039265));
#68207=CARTESIAN_POINT('Ctrl Pts',(28.8752567923883,0.371953492557534,18.9111257173945));
#68208=CARTESIAN_POINT('Ctrl Pts',(28.9314131886074,0.511361040736907,18.9016564371649));
#68209=CARTESIAN_POINT('Ctrl Pts',(29.0965385184593,0.767636822695621,18.8824305405978));
#68210=CARTESIAN_POINT('Ctrl Pts',(29.2062331582591,0.880579083863968,18.8716902227143));
#68211=CARTESIAN_POINT('Ctrl Pts',(29.4605419802015,1.05521085002794,18.8498823608196));
#68212=CARTESIAN_POINT('Ctrl Pts',(29.6020069692685,1.11628678080371,18.8390299549287));
#68213=CARTESIAN_POINT('Ctrl Pts',(29.8977163387384,1.18033932535056,18.8186002283572));
#68214=CARTESIAN_POINT('Ctrl Pts',(30.0489012110254,1.18375239923791,18.8097988699583));
#68215=CARTESIAN_POINT('Ctrl Pts',(30.351304458352,1.13241772416719,18.7894089839185));
#68216=CARTESIAN_POINT('Ctrl Pts',(30.4990888608278,1.07549105419273,18.7783156243515));
#68217=CARTESIAN_POINT('Ctrl Pts',(30.7585582244441,0.910237971254531,18.7565233749656));
#68218=CARTESIAN_POINT('Ctrl Pts',(30.869032001546,0.80544751578808,18.7460242240482));
#68219=CARTESIAN_POINT('Ctrl Pts',(31.0460310070461,0.557381504027199,18.7263602597134));
#68220=CARTESIAN_POINT('Ctrl Pts',(31.1099298338315,0.41584148204013,18.7169862690792));
#68221=CARTESIAN_POINT('Ctrl Pts',(31.1797989523814,0.115104609901925,18.6956617771348));
#68222=CARTESIAN_POINT('Ctrl Pts',(31.1846835245906,-0.0411926090939851,
18.6845791361414));
#68223=CARTESIAN_POINT('Ctrl Pts',(31.134503841219,-0.341119161052378,18.6633121019541));
#68224=CARTESIAN_POINT('Ctrl Pts',(31.082082323541,-0.482198917475646,18.6535190714213));
#68225=CARTESIAN_POINT('Ctrl Pts',(30.9238582069445,-0.74295817680152,18.6345580062792));
#68226=CARTESIAN_POINT('Ctrl Pts',(30.8172746962663,-0.85879990158245,18.6239059387776));
#68227=CARTESIAN_POINT('Ctrl Pts',(30.5674863902569,-1.04046451233651,18.6021263306283));
#68228=CARTESIAN_POINT('Ctrl Pts',(30.4273223446806,-1.10544579712631,18.5912153532567));
#68229=CARTESIAN_POINT('Ctrl Pts',(30.1872213612661,-1.164041447155,18.5743938756203));
#68230=CARTESIAN_POINT('Ctrl Pts',(30.0936931422672,-1.17524047358085,18.5682534779185));
#68231=CARTESIAN_POINT('Ctrl Pts',(29.9999999999998,-1.17524047358085,18.5625));
#68232=CARTESIAN_POINT('Ctrl Pts',(30.,-1.17524047358085,18.5));
#68233=CARTESIAN_POINT('Ctrl Pts',(30.1423690472132,-1.17524047358085,18.5087425520117));
#68234=CARTESIAN_POINT('Ctrl Pts',(30.2836710124158,-1.14937338085773,18.5183366621019));
#68235=CARTESIAN_POINT('Ctrl Pts',(30.561858730089,-1.04379601878612,18.5391626347549));
#68236=CARTESIAN_POINT('Ctrl Pts',(30.6944274791866,-0.96071277520592,18.550248984724));
#68237=CARTESIAN_POINT('Ctrl Pts',(30.9187624839086,-0.748784365111015,
18.5715385296331));
#68238=CARTESIAN_POINT('Ctrl Pts',(31.0086541273172,-0.622420436396325,
18.5808657390843));
#68239=CARTESIAN_POINT('Ctrl Pts',(31.1336634286392,-0.344659292163419,
18.6005610801994));
#68240=CARTESIAN_POINT('Ctrl Pts',(31.1685065373813,-0.196359387070609,
18.6110766518651));
#68241=CARTESIAN_POINT('Ctrl Pts',(31.1804379609257,0.111178530247992,18.6328833887437));
#68242=CARTESIAN_POINT('Ctrl Pts',(31.1550790566304,0.267584160665563,18.6439737169172));
#68243=CARTESIAN_POINT('Ctrl Pts',(31.0469271232095,0.554595748580105,18.6643249836272));
#68244=CARTESIAN_POINT('Ctrl Pts',(30.9678100781097,0.68335841703765,18.6731299773448));
#68245=CARTESIAN_POINT('Ctrl Pts',(30.763452167876,0.90645295543942,18.6935886563282));
#68246=CARTESIAN_POINT('Ctrl Pts',(30.6393299618342,0.997879761179756,18.7044521341951));
#68247=CARTESIAN_POINT('Ctrl Pts',(30.3602369836734,1.12947461105548,18.7262561139589));
#68248=CARTESIAN_POINT('Ctrl Pts',(30.207398548302,1.16725893034935,18.7369811620628));
#68249=CARTESIAN_POINT('Ctrl Pts',(29.9028111520737,1.18064726329168,18.7561598319717));
#68250=CARTESIAN_POINT('Ctrl Pts',(29.7540809815473,1.15884794274813,18.7656824913455));
#68251=CARTESIAN_POINT('Ctrl Pts',(29.4674235177593,1.05897426017317,18.7868263546523));
#68252=CARTESIAN_POINT('Ctrl Pts',(29.332959967187,0.979858413005439,18.7978884009434));
#68253=CARTESIAN_POINT('Ctrl Pts',(29.1020498086111,0.773870883761844,18.8193710843283));
#68254=CARTESIAN_POINT('Ctrl Pts',(29.0080096312967,0.648942084974305,18.8289851559772));
#68255=CARTESIAN_POINT('Ctrl Pts',(28.8756172989166,0.373674108747255,18.8485037128466));
#68256=CARTESIAN_POINT('Ctrl Pts',(28.8370493704244,0.226703861544607,18.85892500183));
#68257=CARTESIAN_POINT('Ctrl Pts',(28.8170693542027,-0.0796098764074361,
18.8806449352421));
#68258=CARTESIAN_POINT('Ctrl Pts',(28.838156352639,-0.236207536581086,18.8917488797605));
#68259=CARTESIAN_POINT('Ctrl Pts',(28.9384458248014,-0.526222673597261,
18.9123131205504));
#68260=CARTESIAN_POINT('Ctrl Pts',(29.0143989785152,-0.657569956199922,
18.921123179589));
#68261=CARTESIAN_POINT('Ctrl Pts',(29.2130173163762,-0.886033452067211,
18.9414197543903));
#68262=CARTESIAN_POINT('Ctrl Pts',(29.3343580168877,-0.980462303689547,
18.9522188602181));
#68263=CARTESIAN_POINT('Ctrl Pts',(29.609473809437,-1.11936682716347,18.9740377655105));
#68264=CARTESIAN_POINT('Ctrl Pts',(29.7612660994758,-1.16125829944545,18.9848441861849));
#68265=CARTESIAN_POINT('Ctrl Pts',(29.9445511530895,-1.1742603871282,18.9965602675684));
#68266=CARTESIAN_POINT('Ctrl Pts',(29.9722886221142,-1.17524047358085,18.998298308746));
#68267=CARTESIAN_POINT('Ctrl Pts',(29.9999999999996,-1.17524047358085,18.9999999999999));
#68268=CARTESIAN_POINT('Origin',(30.,-1.21864324187371E-14,15.78125));
#68269=CARTESIAN_POINT('',(30.0000000000001,-1.17524047358085,19.5625));
#68270=CARTESIAN_POINT('',(29.9999999999998,-1.17524047358085,19.4999999999999));
#68271=CARTESIAN_POINT('',(30.,-1.17524047358085,15.78125));
#68272=CARTESIAN_POINT('Ctrl Pts',(30.0000000000003,-1.17524047358085,19.5625));
#68273=CARTESIAN_POINT('Ctrl Pts',(29.9013941092948,-1.17524047358088,19.5564448416279));
#68274=CARTESIAN_POINT('Ctrl Pts',(29.8029987638489,-1.16283641906691,19.549962842264));
#68275=CARTESIAN_POINT('Ctrl Pts',(29.5564668004839,-1.09938994466242,19.5325744732568));
#68276=CARTESIAN_POINT('Ctrl Pts',(29.415037771559,-1.03111229808663,19.5214689478566));
#68277=CARTESIAN_POINT('Ctrl Pts',(29.1716434679328,-0.847005065425004,
19.4999953804452));
#68278=CARTESIAN_POINT('Ctrl Pts',(29.0705827398005,-0.734710314058229,
19.4898082076353));
#68279=CARTESIAN_POINT('Ctrl Pts',(28.9129094963582,-0.472970867922037,
19.4708462190468));
#68280=CARTESIAN_POINT('Ctrl Pts',(28.8598073237114,-0.32477237703938,19.4605287888834));
#68281=CARTESIAN_POINT('Ctrl Pts',(28.8149047814539,-0.0184511328725056,
19.4388083232246));
#68282=CARTESIAN_POINT('Ctrl Pts',(28.8226412643137,0.136461808695805,19.4278238378469));
#68283=CARTESIAN_POINT('Ctrl Pts',(28.8961732267534,0.430084241574931,19.4070038128194));
#68284=CARTESIAN_POINT('Ctrl Pts',(28.9595331463533,0.5664127336681,19.3979778677293));
#68285=CARTESIAN_POINT('Ctrl Pts',(29.137896746023,0.813817787616469,19.3782535402653));
#68286=CARTESIAN_POINT('Ctrl Pts',(29.2533816215898,0.92090330809607,19.3673653008166));
#68287=CARTESIAN_POINT('Ctrl Pts',(29.5158730245192,1.08160589182486,19.3455488072285));
#68288=CARTESIAN_POINT('Ctrl Pts',(29.6595524720356,1.13505921849913,19.3348306663965));
#68289=CARTESIAN_POINT('Ctrl Pts',(29.9586626554596,1.18420822106571,19.3147204900089));
#68290=CARTESIAN_POINT('Ctrl Pts',(30.1111738123977,1.17970362181747,19.305831310076));
#68291=CARTESIAN_POINT('Ctrl Pts',(30.4108580361143,1.11207867833533,19.2850308420592));
#68292=CARTESIAN_POINT('Ctrl Pts',(30.5546592354692,1.0477915906526,19.2739211274165));
#68293=CARTESIAN_POINT('Ctrl Pts',(30.8039627363725,0.870265103601911,19.2523180019705));
#68294=CARTESIAN_POINT('Ctrl Pts',(30.9084512058835,0.760562755820576,19.242012249931));
#68295=CARTESIAN_POINT('Ctrl Pts',(31.0738897348627,0.502419631313023,19.2227009162624));
#68296=CARTESIAN_POINT('Ctrl Pts',(31.1311837638208,0.355135076925594,19.2126817312365));
#68297=CARTESIAN_POINT('Ctrl Pts',(31.1842706831827,0.04913932312708,19.1909843452775));
#68298=CARTESIAN_POINT('Ctrl Pts',(31.1805124566442,-0.106321035688241,
19.1799610439256));
#68299=CARTESIAN_POINT('Ctrl Pts',(31.1143513914742,-0.401996025434437,
19.1589954772754));
#68300=CARTESIAN_POINT('Ctrl Pts',(31.0545027280943,-0.539801328735837,
19.1497832518808));
#68301=CARTESIAN_POINT('Ctrl Pts',(30.8825757787308,-0.791565442014421,
19.1302996391962));
#68302=CARTESIAN_POINT('Ctrl Pts',(30.7698754890686,-0.90154647307845,19.1194797380197));
#68303=CARTESIAN_POINT('Ctrl Pts',(30.5112798180774,-1.06909180183037,19.0976598713853));
#68304=CARTESIAN_POINT('Ctrl Pts',(30.3686300461772,-1.12627173763864,19.0868728383175));
#68305=CARTESIAN_POINT('Ctrl Pts',(30.146651557919,-1.16837939048486,19.071748782068));
#68306=CARTESIAN_POINT('Ctrl Pts',(30.0733297917687,-1.17524047358085,19.0670030119334));
#68307=CARTESIAN_POINT('Ctrl Pts',(30.,-1.17524047358085,19.0625));
#68308=CARTESIAN_POINT('Ctrl Pts',(29.9999999999996,-1.17524047358085,18.9999999999999));
#68309=CARTESIAN_POINT('Ctrl Pts',(30.1208018343283,-1.17524047358085,19.0074181596379));
#68310=CARTESIAN_POINT('Ctrl Pts',(30.2410273417982,-1.15662316578329,19.0154609815185));
#68311=CARTESIAN_POINT('Ctrl Pts',(30.5033214237856,-1.07312795539109,19.0345280681775));
#68312=CARTESIAN_POINT('Ctrl Pts',(30.6395388198866,-0.997960158889978,
19.0455578408927));
#68313=CARTESIAN_POINT('Ctrl Pts',(30.876878941369,-0.797935916319293,19.067223952545));
#68314=CARTESIAN_POINT('Ctrl Pts',(30.9750570407496,-0.674426741281125,
19.0771781033725));
#68315=CARTESIAN_POINT('Ctrl Pts',(31.1146479426385,-0.401644540658674,
19.0965204001729));
#68316=CARTESIAN_POINT('Ctrl Pts',(31.1567939343853,-0.256055794064216,
19.1068437304378));
#68317=CARTESIAN_POINT('Ctrl Pts',(31.1845453028865,0.0488704061743495,
19.1284652770555));
#68318=CARTESIAN_POINT('Ctrl Pts',(31.1676027188842,0.205546638234067,19.1395747929079));
#68319=CARTESIAN_POINT('Ctrl Pts',(31.0749923240704,0.498408501569657,19.1603408878703));
#68320=CARTESIAN_POINT('Ctrl Pts',(31.0021074917097,0.632295920687204,19.1692134966416));
#68321=CARTESIAN_POINT('Ctrl Pts',(30.8090318381138,0.865881565613648,19.1893513074212));
#68322=CARTESIAN_POINT('Ctrl Pts',(30.6904244547157,0.963111668252584,19.2000818814201));
#68323=CARTESIAN_POINT('Ctrl Pts',(30.419302827982,1.10891198567697,19.2218999959461));
#68324=CARTESIAN_POINT('Ctrl Pts',(30.2686205389783,1.15471361101177,19.232776883577));
#68325=CARTESIAN_POINT('Ctrl Pts',(29.9650775926592,1.18413115670169,19.2524597117397));
#68326=CARTESIAN_POINT('Ctrl Pts',(29.8154193388389,1.17018311968912,19.2615139711268));
#68327=CARTESIAN_POINT('Ctrl Pts',(29.5246945745281,1.08577187830739,19.2823593965739));
#68328=CARTESIAN_POINT('Ctrl Pts',(29.3869225275025,1.01437069769904,19.2933510961767));
#68329=CARTESIAN_POINT('Ctrl Pts',(29.1449076103833,0.821179121928182,19.3150620325829));
#68330=CARTESIAN_POINT('Ctrl Pts',(29.0436548787038,0.700625409307818,19.3253204220004));
#68331=CARTESIAN_POINT('Ctrl Pts',(28.8969987915807,0.43246305184088,19.3443351373923));
#68332=CARTESIAN_POINT('Ctrl Pts',(28.8509250755758,0.288512534702925,19.3545423049446));
#68333=CARTESIAN_POINT('Ctrl Pts',(28.8145962917767,-0.0146433580687103,
19.3760383235316));
#68334=CARTESIAN_POINT('Ctrl Pts',(28.8269416915671,-0.171282191603316,
19.3871451875491));
#68335=CARTESIAN_POINT('Ctrl Pts',(28.9109596159865,-0.467218400914038,
19.4081292766188));
#68336=CARTESIAN_POINT('Ctrl Pts',(28.9804361831083,-0.603975745967944,
19.4171374882925));
#68337=CARTESIAN_POINT('Ctrl Pts',(29.167379298401,-0.843150163563664,19.4370968570367));
#68338=CARTESIAN_POINT('Ctrl Pts',(29.2829166096857,-0.943363871775425,
19.447744685016));
#68339=CARTESIAN_POINT('Ctrl Pts',(29.5508199561077,-1.09737775425148,19.4696563740096));
#68340=CARTESIAN_POINT('Ctrl Pts',(29.7018004358378,-1.14764798506443,19.4807100016028));
#68341=CARTESIAN_POINT('Ctrl Pts',(29.9053565213586,-1.17238533019257,19.4940869386326));
#68342=CARTESIAN_POINT('Ctrl Pts',(29.9526999581129,-1.17524047358085,19.4970954144566));
#68343=CARTESIAN_POINT('Ctrl Pts',(29.9999999999997,-1.17524047358085,19.4999999999999));
#68344=CARTESIAN_POINT('Origin',(30.,-1.21864324187371E-14,15.78125));
#68345=CARTESIAN_POINT('',(30.0000000000003,-1.17524047358085,20.0625));
#68346=CARTESIAN_POINT('',(30.,-1.17524047358085,20.));
#68347=CARTESIAN_POINT('',(30.,-1.17524047358085,15.78125));
#68348=CARTESIAN_POINT('Ctrl Pts',(30.0000000000005,-1.17524047358085,20.0625));
#68349=CARTESIAN_POINT('Ctrl Pts',(29.8795085612599,-1.17524047358091,20.0551009010331));
#68350=CARTESIAN_POINT('Ctrl Pts',(29.7595622632698,-1.15671912815303,20.0470786269818));
#68351=CARTESIAN_POINT('Ctrl Pts',(29.4968909328774,-1.07331217196907,20.0279915033172));
#68352=CARTESIAN_POINT('Ctrl Pts',(29.3601452160293,-0.997848639613717,
20.0169188027128));
#68353=CARTESIAN_POINT('Ctrl Pts',(29.1279895360134,-0.801888849412877,
19.9957151555763));
#68354=CARTESIAN_POINT('Ctrl Pts',(29.0334325756294,-0.684937055319331,
19.9860671564471));
#68355=CARTESIAN_POINT('Ctrl Pts',(28.8898211655935,-0.415941538872162,
19.9669933638564));
#68356=CARTESIAN_POINT('Ctrl Pts',(28.8445081931777,-0.265175978908636,
19.956302958832));
#68357=CARTESIAN_POINT('Ctrl Pts',(28.8156113317766,0.0421759568632406,
19.934509409435));
#68358=CARTESIAN_POINT('Ctrl Pts',(28.8311290214712,0.195715280521655,19.9236223238335));
#68359=CARTESIAN_POINT('Ctrl Pts',(28.9191574051752,0.485137216573778,19.9031001454256));
#68360=CARTESIAN_POINT('Ctrl Pts',(28.9896097101006,0.618617028321211,19.8942800985803));
#68361=CARTESIAN_POINT('Ctrl Pts',(29.1815016413357,0.8578593810217,19.8740144260076));
#68362=CARTESIAN_POINT('Ctrl Pts',(29.3033374545183,0.95943115864218,19.8629316730427));
#68363=CARTESIAN_POINT('Ctrl Pts',(29.5744131919249,1.10584185120943,19.8410947363937));
#68364=CARTESIAN_POINT('Ctrl Pts',(29.7199575824398,1.1513488317962,19.8305438014147));
#68365=CARTESIAN_POINT('Ctrl Pts',(30.0223936436952,1.18496921575338,19.8107799381662));
#68366=CARTESIAN_POINT('Ctrl Pts',(30.17645595477,1.17197553997772,19.8015484961906));
#68367=CARTESIAN_POINT('Ctrl Pts',(30.4728526803367,1.08704252391974,19.7803362699347));
#68368=CARTESIAN_POINT('Ctrl Pts',(30.6120360120599,1.01521369720442,19.7692427449689));
#68369=CARTESIAN_POINT('Ctrl Pts',(30.8500255075595,0.825212607475584,19.7478921149936));
#68370=CARTESIAN_POINT('Ctrl Pts',(30.9478859340228,0.710618012755788,19.7378881282691));
#68371=CARTESIAN_POINT('Ctrl Pts',(31.0987101974267,0.445344450081356,19.7190782500187));
#68372=CARTESIAN_POINT('Ctrl Pts',(31.148011535677,0.295869142851177,19.7084793335565));
#68373=CARTESIAN_POINT('Ctrl Pts',(31.1851397417262,-0.0109614779842622,
19.6867227492848));
#68374=CARTESIAN_POINT('Ctrl Pts',(31.1736153786499,-0.165256365490512,
19.6757820885594));
#68375=CARTESIAN_POINT('Ctrl Pts',(31.093043155488,-0.456865689692268,19.6551048079831));
#68376=CARTESIAN_POINT('Ctrl Pts',(31.0262715370984,-0.591802059151614,
19.6462060198927));
#68377=CARTESIAN_POINT('Ctrl Pts',(30.8407896047275,-0.836102523209368,
19.6261546414896));
#68378=CARTESIAN_POINT('Ctrl Pts',(30.7213221432726,-0.941101033293042,
19.6150958330235));
#68379=CARTESIAN_POINT('Ctrl Pts',(30.4533957183897,-1.09478566221008,19.5931944001043));
#68380=CARTESIAN_POINT('Ctrl Pts',(30.3086782810935,-1.14405280540599,19.5825609345826));
#68381=CARTESIAN_POINT('Ctrl Pts',(30.1059062370161,-1.17166523878134,19.5691302110914));
#68382=CARTESIAN_POINT('Ctrl Pts',(30.0529306288365,-1.17524047358084,19.5657503467901));
#68383=CARTESIAN_POINT('Ctrl Pts',(30.0000000000003,-1.17524047358085,19.5625));
#68384=CARTESIAN_POINT('Ctrl Pts',(29.9999999999997,-1.17524047358085,19.4999999999999));
#68385=CARTESIAN_POINT('Ctrl Pts',(30.1013134091967,-1.17524047358085,19.5062214207844));
#68386=CARTESIAN_POINT('Ctrl Pts',(30.2023703512557,-1.16214610944681,19.5128913366607));
#68387=CARTESIAN_POINT('Ctrl Pts',(30.4489451189351,-1.0968832859302,19.530346730545));
#68388=CARTESIAN_POINT('Ctrl Pts',(30.5880725807912,-1.02901377075515,19.5412964522821));
#68389=CARTESIAN_POINT('Ctrl Pts',(30.8343712795547,-0.842194481571482,
19.5630445243813));
#68390=CARTESIAN_POINT('Ctrl Pts',(30.9385897374703,-0.724253666071193,
19.5736257801046));
#68391=CARTESIAN_POINT('Ctrl Pts',(31.0916505061583,-0.460199205120922,
19.5923866032744));
#68392=CARTESIAN_POINT('Ctrl Pts',(31.1412805360793,-0.317836464065441,
19.6024630191855));
#68393=CARTESIAN_POINT('Ctrl Pts',(31.1853286010408,-0.0163533735884271,
19.6238404235873));
#68394=CARTESIAN_POINT('Ctrl Pts',(31.1771308821554,0.140138676220234,19.6349368795415));
#68395=CARTESIAN_POINT('Ctrl Pts',(31.1009443941398,0.438772825443172,19.6561122727154));
#68396=CARTESIAN_POINT('Ctrl Pts',(31.0345585763112,0.578169376036336,19.6653017627446));
#68397=CARTESIAN_POINT('Ctrl Pts',(30.8531427469532,0.82231181712456,19.6850978487155));
#68398=CARTESIAN_POINT('Ctrl Pts',(30.7404083067898,0.925109501957493,19.6956651705268));
#68399=CARTESIAN_POINT('Ctrl Pts',(30.4771535858122,1.08544747135218,19.7175156107599));
#68400=CARTESIAN_POINT('Ctrl Pts',(30.3279214291812,1.13945389596675,19.7285943399309));
#68401=CARTESIAN_POINT('Ctrl Pts',(30.0245530133835,1.1844610145353,19.7488191591971));
#68402=CARTESIAN_POINT('Ctrl Pts',(29.8738446796079,1.17798106878653,19.7576497404222));
#68403=CARTESIAN_POINT('Ctrl Pts',(29.5795308296296,1.10805786067705,19.7782019083499));
#68404=CARTESIAN_POINT('Ctrl Pts',(29.4390520876789,1.04399036655414,19.7890998131999));
#68405=CARTESIAN_POINT('Ctrl Pts',(29.1881857877585,0.86396490371117,19.8108875045287));
#68406=CARTESIAN_POINT('Ctrl Pts',(29.0808654270878,0.748795351686304,19.8215609892382));
#68407=CARTESIAN_POINT('Ctrl Pts',(28.9210185508111,0.489082061917269,19.8405846207479));
#68408=CARTESIAN_POINT('Ctrl Pts',(28.8677194354805,0.348399842158546,19.8502958472478));
#68409=CARTESIAN_POINT('Ctrl Pts',(28.8156254684423,0.0489678765559477,
19.8715278115659));
#68410=CARTESIAN_POINT('Ctrl Pts',(28.8194748723048,-0.107254256712007,
19.88260512842));
#68411=CARTESIAN_POINT('Ctrl Pts',(28.8873579337553,-0.408638429267571,
19.9039755188019));
#68412=CARTESIAN_POINT('Ctrl Pts',(28.9504754704978,-0.550854728104584,
19.9134143320288));
#68413=CARTESIAN_POINT('Ctrl Pts',(29.1260934520651,-0.800139160205639,
19.9330366884507));
#68414=CARTESIAN_POINT('Ctrl Pts',(29.2358570179041,-0.905539531949709,
19.9435138507578));
#68415=CARTESIAN_POINT('Ctrl Pts',(29.4941308064619,-1.07230397107708,19.9652862658853));
#68416=CARTESIAN_POINT('Ctrl Pts',(29.6414537313008,-1.13013161490591,19.9763832300743));
#68417=CARTESIAN_POINT('Ctrl Pts',(29.8633704190017,-1.16928660340085,19.9913988083098));
#68418=CARTESIAN_POINT('Ctrl Pts',(29.9316910379181,-1.17524047358085,19.9958053055382));
#68419=CARTESIAN_POINT('Ctrl Pts',(30.,-1.17524047358085,20.));
#68420=CARTESIAN_POINT('Origin',(30.,-1.21864324187371E-14,15.78125));
#68421=CARTESIAN_POINT('',(30.,-1.17524047358085,20.5625));
#68422=CARTESIAN_POINT('',(30.,-1.17524047358085,20.5));
#68423=CARTESIAN_POINT('',(30.,-1.17524047358085,15.78125));
#68424=CARTESIAN_POINT('Ctrl Pts',(30.0000000000001,-1.17524047358085,20.5625));
#68425=CARTESIAN_POINT('Ctrl Pts',(29.857466677664,-1.17524047358086,20.5537473602351));
#68426=CARTESIAN_POINT('Ctrl Pts',(29.7159780885029,-1.14931710991913,20.5441397949867));
#68427=CARTESIAN_POINT('Ctrl Pts',(29.4386327044728,-1.04389937724848,20.5233712075421));
#68428=CARTESIAN_POINT('Ctrl Pts',(29.3069416102485,-0.961526015490682,
20.5123639202805));
#68429=CARTESIAN_POINT('Ctrl Pts',(29.086333053172,-0.75405497378,20.4914612382194));
#68430=CARTESIAN_POINT('Ctrl Pts',(28.998234525789,-0.632326756560098,20.4823366930552));
#68431=CARTESIAN_POINT('Ctrl Pts',(28.8691902031313,-0.356072447869899,
20.4627481978422));
#68432=CARTESIAN_POINT('Ctrl Pts',(28.8319810448841,-0.203050335093991,
20.4518977863579));
#68433=CARTESIAN_POINT('Ctrl Pts',(28.8195943462911,0.104677105391675,20.4300776108702));
#68434=CARTESIAN_POINT('Ctrl Pts',(28.8430260194231,0.256395499280261,20.419319642799));
#68435=CARTESIAN_POINT('Ctrl Pts',(28.9459812899286,0.541272174450661,20.399119757359));
#68436=CARTESIAN_POINT('Ctrl Pts',(29.0240298052411,0.671873753047622,20.3902782906932));
#68437=CARTESIAN_POINT('Ctrl Pts',(29.2288981247322,0.900554058537053,20.3695902323474));
#68438=CARTESIAN_POINT('Ctrl Pts',(29.3552896087803,0.99495410007641,20.3584819910769));
#68439=CARTESIAN_POINT('Ctrl Pts',(29.6322160097862,1.12628386030684,20.3368204541948));
#68440=CARTESIAN_POINT('Ctrl Pts',(29.7791530812878,1.16405670631925,20.3264582018892));
#68441=CARTESIAN_POINT('Ctrl Pts',(30.0846260087116,1.18247957174534,20.3070466605788));
#68442=CARTESIAN_POINT('Ctrl Pts',(30.2403465146444,1.16089584876694,20.297232309072));
#68443=CARTESIAN_POINT('Ctrl Pts',(30.5330201521523,1.05871377596515,20.2756371654718));
#68444=CARTESIAN_POINT('Ctrl Pts',(30.6672316693715,0.979687699230499,20.2645937786601));
#68445=CARTESIAN_POINT('Ctrl Pts',(30.8935142020877,0.777827856358351,20.2435416089216));
#68446=CARTESIAN_POINT('Ctrl Pts',(30.9847747247484,0.658466900361099,20.2341902246224));
#68447=CARTESIAN_POINT('Ctrl Pts',(31.1210267097183,0.385760488516485,20.2148533018128));
#68448=CARTESIAN_POINT('Ctrl Pts',(31.1622514979646,0.233796400148884,20.2040779121667));
#68449=CARTESIAN_POINT('Ctrl Pts',(31.1827840987885,-0.0738574566284658,
20.1822629543138));
#68450=CARTESIAN_POINT('Ctrl Pts',(31.1632412224874,-0.226525134572718,
20.1714376749082));
#68451=CARTESIAN_POINT('Ctrl Pts',(31.0676501608268,-0.513670659031922,
20.1510769110961));
#68452=CARTESIAN_POINT('Ctrl Pts',(30.9933877261944,-0.645689071009633,
20.1422762056128));
#68453=CARTESIAN_POINT('Ctrl Pts',(30.7949445520148,-0.879653706050947,
20.1217953512642));
#68454=CARTESIAN_POINT('Ctrl Pts',(30.670767244765,-0.977642983856647,20.1106958256016));
#68455=CARTESIAN_POINT('Ctrl Pts',(30.3966473841018,-1.11649688166864,20.0889398730384));
#68456=CARTESIAN_POINT('Ctrl Pts',(30.2503518300705,-1.15811817698529,20.0784805729189));
#68457=CARTESIAN_POINT('Ctrl Pts',(30.0667947188483,-1.17381847353791,20.0666521235228));
#68458=CARTESIAN_POINT('Ctrl Pts',(30.0333795266192,-1.17524047358084,20.0645497590825));
#68459=CARTESIAN_POINT('Ctrl Pts',(30.0000000000005,-1.17524047358085,20.0625));
#68460=CARTESIAN_POINT('Ctrl Pts',(30.,-1.17524047358085,20.));
#68461=CARTESIAN_POINT('Ctrl Pts',(30.0810461612404,-1.17524047358085,20.0049768562329));
#68462=CARTESIAN_POINT('Ctrl Pts',(30.1620390634994,-1.16685998246121,20.0102475616837));
#68463=CARTESIAN_POINT('Ctrl Pts',(30.3910188268312,-1.11873616439623,20.0260148454886));
#68464=CARTESIAN_POINT('Ctrl Pts',(30.5327757448135,-1.05858684074315,20.0368523263699));
#68465=CARTESIAN_POINT('Ctrl Pts',(30.7881241531233,-0.885634167315425,
20.0586644967329));
#68466=CARTESIAN_POINT('Ctrl Pts',(30.8985424642913,-0.773390023616368,
20.0694245027186));
#68467=CARTESIAN_POINT('Ctrl Pts',(31.0652926267422,-0.518183463935382,
20.0887122685505));
#68468=CARTESIAN_POINT('Ctrl Pts',(31.1223297618129,-0.379162720763723,
20.0981145292327));
#68469=CARTESIAN_POINT('Ctrl Pts',(31.182501138976,-0.0818619977066759,
20.1191953725253));
#68470=CARTESIAN_POINT('Ctrl Pts',(31.1830210318339,0.0739680814447177,
20.1302448898124));
#68471=CARTESIAN_POINT('Ctrl Pts',(31.1235906320717,0.378032609170699,20.1518053374088));
#68472=CARTESIAN_POINT('Ctrl Pts',(31.0637982215859,0.523138441463073,20.1615551718639));
#68473=CARTESIAN_POINT('Ctrl Pts',(30.8940186419568,0.777530022608243,20.1810000731231));
#68474=CARTESIAN_POINT('Ctrl Pts',(30.7872728375238,0.885439479392022,20.1913808781633));
#68475=CARTESIAN_POINT('Ctrl Pts',(30.5341117586616,1.05845819784869,20.2130610712561));
#68476=CARTESIAN_POINT('Ctrl Pts',(30.3887837233288,1.12003007025227,20.2241682808161));
#68477=CARTESIAN_POINT('Ctrl Pts',(30.0880464072922,1.18158358213937,20.2448181618436));
#68478=CARTESIAN_POINT('Ctrl Pts',(29.9360438868879,1.18313176496437,20.2536476203627));
#68479=CARTESIAN_POINT('Ctrl Pts',(29.6381705506099,1.1284628410545,20.2738775466838));
#68480=CARTESIAN_POINT('Ctrl Pts',(29.4952627894061,1.07218329111658,20.2846485002308));
#68481=CARTESIAN_POINT('Ctrl Pts',(29.2357076507194,0.906285518142771,20.3064688735353));
#68482=CARTESIAN_POINT('Ctrl Pts',(29.1223265216238,0.796998466553187,20.3173059793119));
#68483=CARTESIAN_POINT('Ctrl Pts',(28.94883850375,0.546283376626024,20.3368482617845));
#68484=CARTESIAN_POINT('Ctrl Pts',(28.8881400415123,0.408839661433748,20.3460102123335));
#68485=CARTESIAN_POINT('Ctrl Pts',(28.8201837019616,0.113659356458156,20.3669407021362));
#68486=CARTESIAN_POINT('Ctrl Pts',(28.8154556440784,-0.0416770716817043,
20.377955215877));
#68487=CARTESIAN_POINT('Ctrl Pts',(28.8666287496698,-0.348241759389233,
20.3996929435023));
#68488=CARTESIAN_POINT('Ctrl Pts',(28.923168044506,-0.496185032937023,20.4097992015263));
#68489=CARTESIAN_POINT('Ctrl Pts',(29.0873034963183,-0.755446668555585,
20.4290701716561));
#68490=CARTESIAN_POINT('Ctrl Pts',(29.1911125253156,-0.865675121623956,
20.4393528532326));
#68491=CARTESIAN_POINT('Ctrl Pts',(29.4392495659902,-1.04453090441881,20.4609314775711));
#68492=CARTESIAN_POINT('Ctrl Pts',(29.5825856119781,-1.10962145963742,20.4720411141544));
#68493=CARTESIAN_POINT('Ctrl Pts',(29.8217321396476,-1.16509155071327,20.4886931681386));
#68494=CARTESIAN_POINT('Ctrl Pts',(29.9108091908387,-1.17524047358086,20.4945229998842));
#68495=CARTESIAN_POINT('Ctrl Pts',(30.0000000000001,-1.17524047358085,20.5));
#68496=CARTESIAN_POINT('Origin',(30.,-1.21864324187371E-14,15.78125));
#68497=CARTESIAN_POINT('',(30.,-1.17524047358085,21.0625));
#68498=CARTESIAN_POINT('',(30.0000000000003,-1.17524047358085,21.));
#68499=CARTESIAN_POINT('',(30.,-1.17524047358085,15.78125));
#68500=CARTESIAN_POINT('Ctrl Pts',(30.,-1.17524047358085,21.0625));
#68501=CARTESIAN_POINT('Ctrl Pts',(29.9930425354756,-1.17524047358085,21.062072758288));
#68502=CARTESIAN_POINT('Ctrl Pts',(29.9860827950433,-1.17517869098314,21.0616431863938));
#68503=CARTESIAN_POINT('Ctrl Pts',(29.8232316065342,-1.17228514735699,21.0515402867957));
#68504=CARTESIAN_POINT('Ctrl Pts',(29.6694853244495,-1.13852257202281,21.0409020757897));
#68505=CARTESIAN_POINT('Ctrl Pts',(29.3867104280309,-1.01415059452875,21.0191280758083));
#68506=CARTESIAN_POINT('Ctrl Pts',(29.2599516823908,-0.925722033008617,
21.0082089931399));
#68507=CARTESIAN_POINT('Ctrl Pts',(29.0500490851207,-0.707886564567504,
20.9875962815068));
#68508=CARTESIAN_POINT('Ctrl Pts',(28.9678750474644,-0.58156955059427,20.9787376277926));
#68509=CARTESIAN_POINT('Ctrl Pts',(28.852209421352,-0.297516308143681,20.9585961298867));
#68510=CARTESIAN_POINT('Ctrl Pts',(28.8227455494544,-0.141401249035421,
20.9475264053908));
#68511=CARTESIAN_POINT('Ctrl Pts',(28.8269065561122,0.16711629798966,20.9256502054441));
#68512=CARTESIAN_POINT('Ctrl Pts',(28.8581354481118,0.316603790040456,20.915050424987));
#68513=CARTESIAN_POINT('Ctrl Pts',(28.9760761175465,0.596699382404322,20.8951895540518));
#68514=CARTESIAN_POINT('Ctrl Pts',(29.0620842641545,0.724424918144287,20.8860783197069));
#68515=CARTESIAN_POINT('Ctrl Pts',(29.2801481558297,0.941880855388224,20.8649778977684));
#68516=CARTESIAN_POINT('Ctrl Pts',(29.4108173740059,1.02868094436595,20.8538764175153));
#68517=CARTESIAN_POINT('Ctrl Pts',(29.6929274853784,1.14422525088517,20.8324562143623));
#68518=CARTESIAN_POINT('Ctrl Pts',(29.8408766090356,1.17398844910975,20.8223157862342));
#68519=CARTESIAN_POINT('Ctrl Pts',(30.146238089068,1.17646530253954,20.8034764343644));
#68520=CARTESIAN_POINT('Ctrl Pts',(30.3008127704194,1.14674523024735,20.7930175246536));
#68521=CARTESIAN_POINT('Ctrl Pts',(30.5871854304481,1.02954198948055,20.7712767528846));
#68522=CARTESIAN_POINT('Ctrl Pts',(30.7164764357369,0.944145175747713,20.7603096568304));
#68523=CARTESIAN_POINT('Ctrl Pts',(30.9318157386174,0.731537563311469,20.7395484367846));
#68524=CARTESIAN_POINT('Ctrl Pts',(31.0169931096024,0.607571893797524,20.7305813882675));
#68525=CARTESIAN_POINT('Ctrl Pts',(31.1392545858023,0.328058458126713,20.7107617965928));
#68526=CARTESIAN_POINT('Ctrl Pts',(31.1726798971535,0.174145191638854,20.6998481956499));
#68527=CARTESIAN_POINT('Ctrl Pts',(31.177452605602,-0.133454152417299,20.6780371031564));
#68528=CARTESIAN_POINT('Ctrl Pts',(31.1504138008343,-0.284195707834949,
20.6673484002337));
#68529=CARTESIAN_POINT('Ctrl Pts',(31.0405663350578,-0.566901684154618,
20.647302433566));
#68530=CARTESIAN_POINT('Ctrl Pts',(30.9589018497076,-0.696179869646961,
20.6383684206626));
#68531=CARTESIAN_POINT('Ctrl Pts',(30.7479829469593,-0.919779045347213,
20.6174889551129));
#68532=CARTESIAN_POINT('Ctrl Pts',(30.6195839675717,-1.0107321163549,20.6063796462101));
#68533=CARTESIAN_POINT('Ctrl Pts',(30.3401820261614,-1.13487834149049,20.5848207753144));
#68534=CARTESIAN_POINT('Ctrl Pts',(30.1927291526794,-1.16899555973842,20.5745564544744));
#68535=CARTESIAN_POINT('Ctrl Pts',(30.02853673898,-1.17498080122699,20.5642615811144));
#68536=CARTESIAN_POINT('Ctrl Pts',(30.0142636931895,-1.17524047358085,20.5633759002187));
#68537=CARTESIAN_POINT('Ctrl Pts',(30.0000000000001,-1.17524047358085,20.5625));
#68538=CARTESIAN_POINT('Ctrl Pts',(30.0000000000001,-1.17524047358085,20.5));
#68539=CARTESIAN_POINT('Ctrl Pts',(30.0615320920417,-1.17524047358085,20.5037785426368));
#68540=CARTESIAN_POINT('Ctrl Pts',(30.1230970944725,-1.17040913175211,20.5077303953467));
#68541=CARTESIAN_POINT('Ctrl Pts',(30.3340845761439,-1.13693724894346,20.5218733491291));
#68542=CARTESIAN_POINT('Ctrl Pts',(30.4779822284686,-1.08432359797014,20.5325751197693));
#68543=CARTESIAN_POINT('Ctrl Pts',(30.7413240882277,-0.925171378815601,
20.5543888717152));
#68544=CARTESIAN_POINT('Ctrl Pts',(30.8574242886598,-0.818746672756081,
20.5652914684918));
#68545=CARTESIAN_POINT('Ctrl Pts',(31.0372296037246,-0.572330389441825,
20.5850692727305));
#68546=CARTESIAN_POINT('Ctrl Pts',(31.1013789298939,-0.436327710632643,
20.5940611041994));
#68547=CARTESIAN_POINT('Ctrl Pts',(31.1765507195451,-0.143169609179877,
20.6148482046583));
#68548=CARTESIAN_POINT('Ctrl Pts',(31.1851707108535,0.0116076749541518,
20.6258230709101));
#68549=CARTESIAN_POINT('Ctrl Pts',(31.1420730921553,0.318093458162843,20.6475552036167));
#68550=CARTESIAN_POINT('Ctrl Pts',(31.0898417933348,0.466589648702242,20.6579510306787));
#68551=CARTESIAN_POINT('Ctrl Pts',(30.9337645237733,0.729159361106415,20.6768444502657));
#68552=CARTESIAN_POINT('Ctrl Pts',(30.8334379992983,0.84198975683026,20.6870055279311));
#68553=CARTESIAN_POINT('Ctrl Pts',(30.591317195237,1.02746666327729,20.7084494527507));
#68554=CARTESIAN_POINT('Ctrl Pts',(30.4504043784541,1.09657907803444,20.7195528744157));
#68555=CARTESIAN_POINT('Ctrl Pts',(30.1527579068286,1.17519666342875,20.7406179390521));
#68556=CARTESIAN_POINT('Ctrl Pts',(29.9992772327099,1.18508027808452,20.7496955256169));
#68557=CARTESIAN_POINT('Ctrl Pts',(29.6980213394833,1.14582802600215,20.7695865882633));
#68558=CARTESIAN_POINT('Ctrl Pts',(29.5531012936116,1.09744171629364,20.7802012666676));
#68559=CARTESIAN_POINT('Ctrl Pts',(29.2844190436536,0.945457598499347,20.8020888235724));
#68560=CARTESIAN_POINT('Ctrl Pts',(29.1643876737344,0.84125826030012,20.8131539267157));
#68561=CARTESIAN_POINT('Ctrl Pts',(28.9773975743441,0.59813879267389,20.8332560474103));
#68562=CARTESIAN_POINT('Ctrl Pts',(28.9097638018428,0.463547729800393,20.8421310013978));
#68563=CARTESIAN_POINT('Ctrl Pts',(28.8274319674294,0.172449502758382,20.8627720413655));
#68564=CARTESIAN_POINT('Ctrl Pts',(28.8149632933605,0.0183235810432114,
20.8737007211534));
#68565=CARTESIAN_POINT('Ctrl Pts',(28.850150967155,-0.288650006351519,20.8954674428227));
#68566=CARTESIAN_POINT('Ctrl Pts',(28.898515176706,-0.438439388541448,20.906088629547));
#68567=CARTESIAN_POINT('Ctrl Pts',(29.047641063206,-0.704596833168998,20.9249611816339));
#68568=CARTESIAN_POINT('Ctrl Pts',(29.1447168471359,-0.819746341645053,
20.9348754556746));
#68569=CARTESIAN_POINT('Ctrl Pts',(29.381325819526,-1.01116668011756,20.9561916286088));
#68570=CARTESIAN_POINT('Ctrl Pts',(29.5199396968772,-1.08386414625954,20.96728098122));
#68571=CARTESIAN_POINT('Ctrl Pts',(29.7764916553148,-1.15925176815251,20.9857080131187));
#68572=CARTESIAN_POINT('Ctrl Pts',(29.8880479255875,-1.1752404735809,20.9931252835322));
#68573=CARTESIAN_POINT('Ctrl Pts',(30.0000000000005,-1.17524047358085,21.));
#68574=CARTESIAN_POINT('Origin',(30.,-1.21864324187371E-14,15.78125));
#68575=CARTESIAN_POINT('',(29.9999999999998,-1.17524047358085,21.5625));
#68576=CARTESIAN_POINT('',(30.0000000000001,-1.17524047358085,21.5));
#68577=CARTESIAN_POINT('',(30.,-1.17524047358085,15.78125));
#68578=CARTESIAN_POINT('Ctrl Pts',(29.9999999999996,-1.17524047358085,21.5625));
#68579=CARTESIAN_POINT('Ctrl Pts',(29.9719988088573,-1.17524047358085,21.5607805119881));
#68580=CARTESIAN_POINT('Ctrl Pts',(29.9439711363572,-1.17423978092491,21.5590239195234));
#68581=CARTESIAN_POINT('Ctrl Pts',(29.7604047377572,-1.16108096387714,21.547285004757));
#68582=CARTESIAN_POINT('Ctrl Pts',(29.6086428973266,-1.11907669828182,21.5364764549777));
#68583=CARTESIAN_POINT('Ctrl Pts',(29.3336394628651,-0.979972388454951,
21.5146573661612));
#68584=CARTESIAN_POINT('Ctrl Pts',(29.2123764352237,-0.885461951955829,
21.503860137555));
#68585=CARTESIAN_POINT('Ctrl Pts',(29.0139169118187,-0.656850944948416,
21.4835680853588));
#68586=CARTESIAN_POINT('Ctrl Pts',(28.9380513713638,-0.525431379870783,
21.4747570119112));
#68587=CARTESIAN_POINT('Ctrl Pts',(28.8379806985326,-0.235334014126339,
21.4541869404899));
#68588=CARTESIAN_POINT('Ctrl Pts',(28.81701218115,-0.0787326333033737,21.4430827321496));
#68589=CARTESIAN_POINT('Ctrl Pts',(28.8372148732154,0.227544173701852,21.4213654174177));
#68590=CARTESIAN_POINT('Ctrl Pts',(28.8758855793473,0.374476178993786,21.4109468400715));
#68591=CARTESIAN_POINT('Ctrl Pts',(29.008483168462,0.64967403277934,21.3914332554072));
#68592=CARTESIAN_POINT('Ctrl Pts',(29.1026400510551,0.774562668949264,21.3818103125428));
#68593=CARTESIAN_POINT('Ctrl Pts',(29.3337333173752,0.980382528955385,21.3603223294383));
#68594=CARTESIAN_POINT('Ctrl Pts',(29.4682481852686,1.05938687455618,21.3492610850172));
#68595=CARTESIAN_POINT('Ctrl Pts',(29.7549668128984,1.15903498567807,21.3281214631321));
#68596=CARTESIAN_POINT('Ctrl Pts',(29.9037091563498,1.1807204220266,21.3186072813687));
#68597=CARTESIAN_POINT('Ctrl Pts',(30.2082836909242,1.16710140483065,21.2994212226452));
#68598=CARTESIAN_POINT('Ctrl Pts',(30.3610942123922,1.12920096767185,21.2886937718569));
#68599=CARTESIAN_POINT('Ctrl Pts',(30.6400777787282,0.99739853025376,21.2668891510646));
#68600=CARTESIAN_POINT('Ctrl Pts',(30.7641225887122,0.905886016702667,21.2560273872475));
#68601=CARTESIAN_POINT('Ctrl Pts',(30.9683193471767,0.682639701404097,21.2355732231612));
#68602=CARTESIAN_POINT('Ctrl Pts',(31.0473475790777,0.553805208866279,21.2267689284532));
#68603=CARTESIAN_POINT('Ctrl Pts',(31.1552799375254,0.266708452111841,21.2064116226359));
#68604=CARTESIAN_POINT('Ctrl Pts',(31.1805191858716,0.110295910456217,21.195320804404));
#68605=CARTESIAN_POINT('Ctrl Pts',(31.1683617956532,-0.197210560675315,
21.173516297295));
#68606=CARTESIAN_POINT('Ctrl Pts',(31.1334138492448,-0.345474524238407,
21.1630032741523));
#68607=CARTESIAN_POINT('Ctrl Pts',(31.0081981695942,-0.623166742222595,
21.1433128204234));
#68608=CARTESIAN_POINT('Ctrl Pts',(30.9181918552343,-0.749490769431124,
21.1339784439808));
#68609=CARTESIAN_POINT('Ctrl Pts',(30.6936733778382,-0.961255467276285,
21.1126834366527));
#68610=CARTESIAN_POINT('Ctrl Pts',(30.5610503971428,-1.04422897430134,21.1015976470182));
#68611=CARTESIAN_POINT('Ctrl Pts',(30.283074075588,-1.14948332004627,21.080796107845));
#68612=CARTESIAN_POINT('Ctrl Pts',(30.1420666819575,-1.17524047358085,21.0712239844648));
#68613=CARTESIAN_POINT('Ctrl Pts',(30.,-1.17524047358085,21.0625));
#68614=CARTESIAN_POINT('Ctrl Pts',(30.0000000000005,-1.17524047358085,21.));
#68615=CARTESIAN_POINT('Ctrl Pts',(30.0409368563611,-1.17524047358083,21.0025138371222));
#68616=CARTESIAN_POINT('Ctrl Pts',(30.0819173014533,-1.17310176285816,21.0051061762144));
#68617=CARTESIAN_POINT('Ctrl Pts',(30.2729829235624,-1.15303120950392,21.0175506477331));
#68618=CARTESIAN_POINT('Ctrl Pts',(30.4187156327833,-1.10844931428969,21.0280803491923));
#68619=CARTESIAN_POINT('Ctrl Pts',(30.6905353954506,-0.963834030798816,
21.0498993207407));
#68620=CARTESIAN_POINT('Ctrl Pts',(30.8129383742835,-0.863111359129209,
21.0609867980498));
#68621=CARTESIAN_POINT('Ctrl Pts',(31.0063964161767,-0.625120486728277,
21.0813042721815));
#68622=CARTESIAN_POINT('Ctrl Pts',(31.0777548462909,-0.49199236060375,21.0901140644785));
#68623=CARTESIAN_POINT('Ctrl Pts',(31.1675962416571,-0.203110857145286,
21.1105979221763));
#68624=CARTESIAN_POINT('Ctrl Pts',(31.1840814343856,-0.0497708726068158,
21.1214708731443));
#68625=CARTESIAN_POINT('Ctrl Pts',(31.1571888276141,0.257674311285982,21.14327103453));
#68626=CARTESIAN_POINT('Ctrl Pts',(31.1128522255693,0.408737402730974,21.1539825367601));
#68627=CARTESIAN_POINT('Ctrl Pts',(30.9710010878299,0.678628541040232,21.1731198356347));
#68628=CARTESIAN_POINT('Ctrl Pts',(30.8772391714915,0.796156039182743,21.1826908232652));
#68629=CARTESIAN_POINT('Ctrl Pts',(30.6464955823919,0.993543206250726,21.2038583630273));
#68630=CARTESIAN_POINT('Ctrl Pts',(30.5103519798164,1.06987223749504,21.214924774365));
#68631=CARTESIAN_POINT('Ctrl Pts',(30.2162079552513,1.16549604568273,21.2363776960251));
#68632=CARTESIAN_POINT('Ctrl Pts',(30.061127965963,1.18379547472913,21.2459429670447));
#68633=CARTESIAN_POINT('Ctrl Pts',(29.7567781749822,1.15962478754955,21.2654893209196));
#68634=CARTESIAN_POINT('Ctrl Pts',(29.6103180879013,1.11893466526318,21.2759257110673));
#68635=CARTESIAN_POINT('Ctrl Pts',(29.3355002124366,0.981897695520532,21.2976601102058));
#68636=CARTESIAN_POINT('Ctrl Pts',(29.2107776319456,0.884773136393355,21.3087624623211));
#68637=CARTESIAN_POINT('Ctrl Pts',(29.0107746609087,0.652081932742376,21.3292939522647));
#68638=CARTESIAN_POINT('Ctrl Pts',(28.9355970901093,0.52040794626517,21.3380991870768));
#68639=CARTESIAN_POINT('Ctrl Pts',(28.8382134265824,0.233810524699486,21.3584210862971));
#68640=CARTESIAN_POINT('Ctrl Pts',(28.8177208295725,0.0813648692728661,
21.3692306226469));
#68641=CARTESIAN_POINT('Ctrl Pts',(28.8362699803681,-0.22632694032349,21.3910482716382));
#68642=CARTESIAN_POINT('Ctrl Pts',(28.8765201026755,-0.378558584509325,
21.4018426329915));
#68643=CARTESIAN_POINT('Ctrl Pts',(29.0110211856253,-0.652134791815677,
21.4212412308003));
#68644=CARTESIAN_POINT('Ctrl Pts',(29.1015077791443,-0.772069972681635,
21.4305317818752));
#68645=CARTESIAN_POINT('Ctrl Pts',(29.3264048767426,-0.975307798634206,
21.4515477299157));
#68646=CARTESIAN_POINT('Ctrl Pts',(29.4600073333855,-1.05515984377402,21.4625829994009));
#68647=CARTESIAN_POINT('Ctrl Pts',(29.7321091399909,-1.15220558787994,21.4827327726726));
#68648=CARTESIAN_POINT('Ctrl Pts',(29.8656344449969,-1.17524047358088,21.4917489238272));
#68649=CARTESIAN_POINT('Ctrl Pts',(30.0000000000003,-1.17524047358085,21.5));
#68650=CARTESIAN_POINT('Origin',(30.,-1.21864324187371E-14,15.78125));
#68651=CARTESIAN_POINT('',(29.9999999999998,-1.17524047358085,22.0625));
#68652=CARTESIAN_POINT('',(30.000000003784,-1.17524047358085,22.0000000004647));
#68653=CARTESIAN_POINT('',(30.,-1.17524047358085,15.78125));
#68654=CARTESIAN_POINT('Ctrl Pts',(29.9999999999997,-1.17524047358085,22.0625));
#68655=CARTESIAN_POINT('Ctrl Pts',(29.9524010211782,-1.17524047358085,22.0595770574349));
#68656=CARTESIAN_POINT('Ctrl Pts',(29.9047586284152,-1.17234913259513,22.0565489400777));
#68657=CARTESIAN_POINT('Ctrl Pts',(29.7009349924679,-1.1474210952591,22.0431488126472));
#68658=CARTESIAN_POINT('Ctrl Pts',(29.5500039838267,-1.09704169086814,22.0320943523472));
#68659=CARTESIAN_POINT('Ctrl Pts',(29.2822334508411,-0.942842462410207,
22.01018424791));
#68660=CARTESIAN_POINT('Ctrl Pts',(29.1667766500969,-0.842552714869588,
21.9995386680174));
#68661=CARTESIAN_POINT('Ctrl Pts',(28.9799931885339,-0.603233884932394,
21.9795839832802));
#68662=CARTESIAN_POINT('Ctrl Pts',(28.910605612196,-0.466400997640195,21.9705713166174));
#68663=CARTESIAN_POINT('Ctrl Pts',(28.8268127379948,-0.170385863417145,
21.9495816311816));
#68664=CARTESIAN_POINT('Ctrl Pts',(28.8145871174915,-0.0137497615287427,
21.9384749608582));
#68665=CARTESIAN_POINT('Ctrl Pts',(28.85113877829,0.289356743861303,21.9169824442057));
#68666=CARTESIAN_POINT('Ctrl Pts',(28.8973142483913,0.433263084581444,21.9067784090915));
#68667=CARTESIAN_POINT('Ctrl Pts',(29.0441562961032,0.701308793511537,21.8877719649526));
#68668=CARTESIAN_POINT('Ctrl Pts',(29.145494108998,0.821789237943167,21.8775043861745));
#68669=CARTESIAN_POINT('Ctrl Pts',(29.3876377187977,1.01480099788269,21.8557919221934));
#68670=CARTESIAN_POINT('Ctrl Pts',(29.5254500415353,1.08610079854932,21.8448013436507));
#68671=CARTESIAN_POINT('Ctrl Pts',(29.8162261597603,1.17031056565349,21.8239599076952));
#68672=CARTESIAN_POINT('Ctrl Pts',(29.965897796871,1.18415559330363,21.814910211276));
#68673=CARTESIAN_POINT('Ctrl Pts',(30.2694248477664,1.15452627142302,21.7952208509568));
#68674=CARTESIAN_POINT('Ctrl Pts',(30.4200757340443,1.10861951539323,21.7843421644183));
#68675=CARTESIAN_POINT('Ctrl Pts',(30.6910871340011,0.962634653497324,21.762524275871));
#68676=CARTESIAN_POINT('Ctrl Pts',(30.8096198631452,0.865330005993902,21.7517956433222));
#68677=CARTESIAN_POINT('Ctrl Pts',(31.0025452942337,0.631606479581076,21.7316621689435));
#68678=CARTESIAN_POINT('Ctrl Pts',(31.075346835895,0.497649504779323,21.7227870693252));
#68679=CARTESIAN_POINT('Ctrl Pts',(31.1677479593254,0.204711362167963,21.7020155655921));
#68680=CARTESIAN_POINT('Ctrl Pts',(31.1845780485819,0.0480344792828584,
21.6909060035913));
#68681=CARTESIAN_POINT('Ctrl Pts',(31.1566162472742,-0.256851307753155,
21.6692873225717));
#68682=CARTESIAN_POINT('Ctrl Pts',(31.1143736239456,-0.402401296420415,
21.6589667405334));
#68683=CARTESIAN_POINT('Ctrl Pts',(30.9745867433069,-0.675115053903835,
21.6396292968631));
#68684=CARTESIAN_POINT('Ctrl Pts',(30.8762946890393,-0.798585224220405,
21.6296650545771));
#68685=CARTESIAN_POINT('Ctrl Pts',(30.6387793080734,-0.998444700485959,
21.6079940222289));
#68686=CARTESIAN_POINT('Ctrl Pts',(30.5025155082578,-1.07350395293815,21.5969652482617));
#68687=CARTESIAN_POINT('Ctrl Pts',(30.2404480736925,-1.15671325182863,21.5779222161248));
#68688=CARTESIAN_POINT('Ctrl Pts',(30.1205093503255,-1.17524047358085,21.5699001988757));
#68689=CARTESIAN_POINT('Ctrl Pts',(29.9999999999996,-1.17524047358085,21.5625));
#68690=CARTESIAN_POINT('Ctrl Pts',(30.0000000000003,-1.17524047358085,21.5));
#68691=CARTESIAN_POINT('Ctrl Pts',(30.0212839202784,-1.17524047358085,21.5013069960338));
#68692=CARTESIAN_POINT('Ctrl Pts',(30.0425864419315,-1.17466229796956,21.5026356328208));
#68693=CARTESIAN_POINT('Ctrl Pts',(30.2139454930837,-1.16533366693515,21.5134891283695));
#68694=CARTESIAN_POINT('Ctrl Pts',(30.3610177391346,-1.12845915530085,21.523827832119));
#68695=CARTESIAN_POINT('Ctrl Pts',(30.6385696146112,-0.998891400827412,
21.5454653082446));
#68696=CARTESIAN_POINT('Ctrl Pts',(30.7654630357173,-0.905335035089088,
21.5565744608423));
#68697=CARTESIAN_POINT('Ctrl Pts',(30.9718229035628,-0.677897335355307,
21.5773100566854));
#68698=CARTESIAN_POINT('Ctrl Pts',(31.0507577571561,-0.547623084998762,
21.5861694304673));
#68699=CARTESIAN_POINT('Ctrl Pts',(31.1570604439752,-0.258809326298121,
21.6066484845527));
#68700=CARTESIAN_POINT('Ctrl Pts',(31.1812214838473,-0.102338491331391,
21.6177434360859));
#68701=CARTESIAN_POINT('Ctrl Pts',(31.1670292938221,0.204877234262332,21.6395273271632));
#68702=CARTESIAN_POINT('Ctrl Pts',(31.1311379778152,0.352813947812694,21.6500171458341));
#68703=CARTESIAN_POINT('Ctrl Pts',(31.0040616369159,0.629882761963365,21.6696633955718));
#68704=CARTESIAN_POINT('Ctrl Pts',(30.9130181373807,0.755846555951633,21.6790645983814));
#68705=CARTESIAN_POINT('Ctrl Pts',(30.6868446220844,0.966129203413541,21.7004086935125));
#68706=CARTESIAN_POINT('Ctrl Pts',(30.553735937256,1.0481102897547,21.711489124086));
#68707=CARTESIAN_POINT('Ctrl Pts',(30.2686762405413,1.15380487275931,21.7327412449065));
#68708=CARTESIAN_POINT('Ctrl Pts',(30.1202468756007,1.17853792824007,21.7424990119962));
#68709=CARTESIAN_POINT('Ctrl Pts',(29.8153503696085,1.17107054155024,21.7614867439455));
#68710=CARTESIAN_POINT('Ctrl Pts',(29.661826921183,1.13627251461424,21.7721479818837));
#68711=CARTESIAN_POINT('Ctrl Pts',(29.3799800833098,1.01003478165367,21.7939311399523));
#68712=CARTESIAN_POINT('Ctrl Pts',(29.253891997555,0.920828765085568,21.8048366026441));
#68713=CARTESIAN_POINT('Ctrl Pts',(29.0454103417907,0.701638656512355,21.8254100846196));
#68714=CARTESIAN_POINT('Ctrl Pts',(28.9640200854668,0.5746995746724,21.8342495048467));
#68715=CARTESIAN_POINT('Ctrl Pts',(28.8502724171258,0.289883112959693,21.8544451207025));
#68716=CARTESIAN_POINT('Ctrl Pts',(28.8218581810328,0.133683866085342,21.8655208147403));
#68717=CARTESIAN_POINT('Ctrl Pts',(28.8280094580603,-0.174601530686287,
21.8873805534988));
#68718=CARTESIAN_POINT('Ctrl Pts',(28.8601657562679,-0.323793761637004,
21.8979593977371));
#68719=CARTESIAN_POINT('Ctrl Pts',(28.9799119697649,-0.603297917389521,
21.9177783313962));
#68720=CARTESIAN_POINT('Ctrl Pts',(29.0669039974813,-0.730676428244075,
21.9269392883002));
#68721=CARTESIAN_POINT('Ctrl Pts',(29.2865672059309,-0.946735069741176,
21.9480883812055));
#68722=CARTESIAN_POINT('Ctrl Pts',(29.4177292577255,-1.03259356038437,21.9591867420451));
#68723=CARTESIAN_POINT('Ctrl Pts',(29.7004129009365,-1.14619538664958,21.98057329627));
#68724=CARTESIAN_POINT('Ctrl Pts',(29.8484560704769,-1.17497884076058,21.9906847639469));
#68725=CARTESIAN_POINT('Ctrl Pts',(29.9986381885534,-1.17523988185415,21.9999163533479));
#68726=CARTESIAN_POINT('Ctrl Pts',(29.9993191103818,-1.17524047358524,21.9999581881525));
#68727=CARTESIAN_POINT('Ctrl Pts',(30.0000000075681,-1.17524047358085,22.0000000004647));
#68728=CARTESIAN_POINT('Origin',(30.,-1.21864324187371E-14,15.78125));
#68729=CARTESIAN_POINT('',(30.,-1.17524047358085,22.5625));
#68730=CARTESIAN_POINT('',(29.9999999999999,-1.17524047358085,22.4999999999999));
#68731=CARTESIAN_POINT('',(30.,-1.17524047358085,15.78125));
#68732=CARTESIAN_POINT('Ctrl Pts',(30.,-1.17524047358085,22.5625));
#68733=CARTESIAN_POINT('Ctrl Pts',(29.9313687068489,-1.17524047358085,22.5582855119371));
#68734=CARTESIAN_POINT('Ctrl Pts',(29.8627268799626,-1.16923029327301,22.55385729367));
#68735=CARTESIAN_POINT('Ctrl Pts',(29.6405360439417,-1.12983827415446,22.5388164770024));
#68736=CARTESIAN_POINT('Ctrl Pts',(29.4932720438495,-1.07189657475161,22.5277190875488));
#68737=CARTESIAN_POINT('Ctrl Pts',(29.2351505504649,-0.904940984815958,
22.505949247503));
#68738=CARTESIAN_POINT('Ctrl Pts',(29.125477326134,-0.799463570556349,22.4954749014128));
#68739=CARTESIAN_POINT('Ctrl Pts',(28.9500348086396,-0.550024618450246,
22.4758578415198));
#68740=CARTESIAN_POINT('Ctrl Pts',(28.8870166724079,-0.407722193677489,
22.4664105508506));
#68741=CARTESIAN_POINT('Ctrl Pts',(28.8193863135494,-0.106256134735224,
22.4450343541119));
#68742=CARTESIAN_POINT('Ctrl Pts',(28.8156683957017,0.0499559751614321,
22.4339577479897));
#68743=CARTESIAN_POINT('Ctrl Pts',(28.8680054797788,0.349324836623415,22.4127302582268));
#68744=CARTESIAN_POINT('Ctrl Pts',(28.9214162690158,0.489956671932254,22.4030291896045));
#68745=CARTESIAN_POINT('Ctrl Pts',(29.0814696037689,0.749536525817022,22.3839976107609));
#68746=CARTESIAN_POINT('Ctrl Pts',(29.1888834831425,0.864620134172483,22.3733214303097));
#68747=CARTESIAN_POINT('Ctrl Pts',(29.4398862783311,1.04443640573476,22.3515327737366));
#68748=CARTESIAN_POINT('Ctrl Pts',(29.5804046735503,1.10838743829029,22.3406365628695));
#68749=CARTESIAN_POINT('Ctrl Pts',(29.874773559948,1.17808176091705,22.320089130129));
#68750=CARTESIAN_POINT('Ctrl Pts',(30.0254999210416,1.18444262102585,22.3112603596819));
#68751=CARTESIAN_POINT('Ctrl Pts',(30.3288317944626,1.13918974891494,22.2910290715165));
#68752=CARTESIAN_POINT('Ctrl Pts',(30.4780087858284,1.08506931516396,22.2799496878662));
#68753=CARTESIAN_POINT('Ctrl Pts',(30.7411182596149,0.924538989516088,22.2581013471772));
#68754=CARTESIAN_POINT('Ctrl Pts',(30.8537656083098,0.82166305580017,22.2475365992352));
#68755=CARTESIAN_POINT('Ctrl Pts',(31.0350106463268,0.577368135111118,22.2277455951917));
#68756=CARTESIAN_POINT('Ctrl Pts',(31.1013006049905,0.437889260334813,22.2185496213456));
#68757=CARTESIAN_POINT('Ctrl Pts',(31.1772437890897,0.139172903087767,22.1973683990083));
#68758=CARTESIAN_POINT('Ctrl Pts',(31.185313349087,-0.0173128950364053,
22.1862723863453));
#68759=CARTESIAN_POINT('Ctrl Pts',(31.1410279217834,-0.318736522964712,
22.1648991982826));
#68760=CARTESIAN_POINT('Ctrl Pts',(31.0912903592309,-0.461049327500964,
22.1548343474741));
#68761=CARTESIAN_POINT('Ctrl Pts',(30.9380306919572,-0.724977765907907,
22.136065778375));
#68762=CARTESIAN_POINT('Ctrl Pts',(30.8337205687989,-0.842838844072579,
22.1254817206889));
#68763=CARTESIAN_POINT('Ctrl Pts',(30.5872857957992,-1.02946130111843,22.1037322710222));
#68764=CARTESIAN_POINT('Ctrl Pts',(30.4481174203718,-1.09722011431045,22.0927839616769));
#68765=CARTESIAN_POINT('Ctrl Pts',(30.2017882631029,-1.16222172164091,22.0753529112466));
#68766=CARTESIAN_POINT('Ctrl Pts',(30.1010204315162,-1.17524047358085,22.0687034297066));
#68767=CARTESIAN_POINT('Ctrl Pts',(29.9999999999997,-1.17524047358085,22.0625));
#68768=CARTESIAN_POINT('Ctrl Pts',(30.0000000075681,-1.17524047358085,22.0000000004647));
#68769=CARTESIAN_POINT('Ctrl Pts',(30.1550617076756,-1.17524047258231,22.0095219788006));
#68770=CARTESIAN_POINT('Ctrl Pts',(30.3087125624576,-1.14455036320512,22.020045399438));
#68771=CARTESIAN_POINT('Ctrl Pts',(30.5936146237504,-1.02583437646268,22.0417494976575));
#68772=CARTESIAN_POINT('Ctrl Pts',(30.7222919834293,-0.9396884903777,22.0527054685765));
#68773=CARTESIAN_POINT('Ctrl Pts',(30.9363028934711,-0.725796874489648,
22.0734306378289));
#68774=CARTESIAN_POINT('Ctrl Pts',(31.0207456221836,-0.60126080890756,22.0823661148205));
#68775=CARTESIAN_POINT('Ctrl Pts',(31.1412832329984,-0.320931550152795,
22.1022435544492));
#68776=CARTESIAN_POINT('Ctrl Pts',(31.1737467539974,-0.166807893544759,
22.1131720736242));
#68777=CARTESIAN_POINT('Ctrl Pts',(31.1765934878998,0.140728845238564,22.1349787269359));
#68778=CARTESIAN_POINT('Ctrl Pts',(31.148646481366,0.291209583454888,22.1456489359696));
#68779=CARTESIAN_POINT('Ctrl Pts',(31.0370532707971,0.573358102978206,22.165655374784));
#68780=CARTESIAN_POINT('Ctrl Pts',(30.9544609034821,0.702301510156061,22.1746213225474));
#68781=CARTESIAN_POINT('Ctrl Pts',(30.7420042686145,0.924591934894812,22.1955488165371));
#68782=CARTESIAN_POINT('Ctrl Pts',(30.6131073712558,1.01465868002552,22.2066572778597));
#68783=CARTESIAN_POINT('Ctrl Pts',(30.3331026676289,1.1369643062698,22.228187906872));
#68784=CARTESIAN_POINT('Ctrl Pts',(30.1855325771707,1.17014774287538,22.2384263196851));
#68785=CARTESIAN_POINT('Ctrl Pts',(29.8783465649041,1.17947691083341,22.2576206519922));
#68786=CARTESIAN_POINT('Ctrl Pts',(29.7215875906434,1.15260328305267,22.2678992314176));
#68787=CARTESIAN_POINT('Ctrl Pts',(29.4314038660401,1.03996407151785,22.2897122199048));
#68788=CARTESIAN_POINT('Ctrl Pts',(29.3003745517226,0.9567417174806,22.3007089687507));
#68789=CARTESIAN_POINT('Ctrl Pts',(29.0812311411824,0.747835374300097,22.3215725663721));
#68790=CARTESIAN_POINT('Ctrl Pts',(28.9939461402353,0.625488946274541,22.3306481587999));
#68791=CARTESIAN_POINT('Ctrl Pts',(28.866779072646,0.34832483100282,22.3503011660994));
#68792=CARTESIAN_POINT('Ctrl Pts',(28.8306169080572,0.195045951299282,22.3611697842779));
#68793=CARTESIAN_POINT('Ctrl Pts',(28.8203429359976,-0.112665031360941,
22.3829887927828));
#68794=CARTESIAN_POINT('Ctrl Pts',(28.844778193878,-0.264121048518041,22.3937281563827));
#68795=CARTESIAN_POINT('Ctrl Pts',(28.9496447173484,-0.548400594969454,
22.4138857009336));
#68796=CARTESIAN_POINT('Ctrl Pts',(29.0286885091485,-0.678634752036216,
22.4227474921567));
#68797=CARTESIAN_POINT('Ctrl Pts',(29.2352313232766,-0.905919594975383,
22.4434889029608));
#68798=CARTESIAN_POINT('Ctrl Pts',(29.3621859947411,-0.999372204838993,
22.454598138267));
#68799=CARTESIAN_POINT('Ctrl Pts',(29.6398139077013,-1.12872343697434,22.4762326071516));
#68800=CARTESIAN_POINT('Ctrl Pts',(29.7869023742936,-1.1654876328242,22.4865683958599));
#68801=CARTESIAN_POINT('Ctrl Pts',(29.9579757834663,-1.17467745886044,22.4973994296432));
#68802=CARTESIAN_POINT('Ctrl Pts',(29.9789969929607,-1.17524047358085,22.4987102541947));
#68803=CARTESIAN_POINT('Ctrl Pts',(29.9999999999997,-1.17524047358085,22.4999999999999));
#68804=CARTESIAN_POINT('Origin',(30.,-1.21864324187371E-14,15.78125));
#68805=CARTESIAN_POINT('',(30.,-1.17524047358085,23.0625));
#68806=CARTESIAN_POINT('',(29.9999999999997,-1.17524047358085,22.9999999999999));
#68807=CARTESIAN_POINT('',(30.,-1.17524047358085,15.78125));
#68808=CARTESIAN_POINT('Ctrl Pts',(30.0000000000001,-1.17524047358085,23.0625));
#68809=CARTESIAN_POINT('Ctrl Pts',(29.9105144759955,-1.17524047358086,23.0570049021313));
#68810=CARTESIAN_POINT('Ctrl Pts',(29.8211453329131,-1.16502438899623,23.0511547525684));
#68811=CARTESIAN_POINT('Ctrl Pts',(29.5817638222111,-1.10931034878277,23.0344796199141));
#68812=CARTESIAN_POINT('Ctrl Pts',(29.4384864599594,-1.04411918186912,23.0233700199021));
#68813=CARTESIAN_POINT('Ctrl Pts',(29.1904963016638,-0.865097093142698,
23.001794519102));
#68814=CARTESIAN_POINT('Ctrl Pts',(29.0867727283959,-0.754802905276228,
22.9915147546188));
#68815=CARTESIAN_POINT('Ctrl Pts',(28.9228010666229,-0.495400927229172,
22.9722488667908));
#68816=CARTESIAN_POINT('Ctrl Pts',(28.8663568012591,-0.347374707529959,
22.9621314630453));
#68817=CARTESIAN_POINT('Ctrl Pts',(28.8154245654916,-0.0407388679671123,
22.9403886902216));
#68818=CARTESIAN_POINT('Ctrl Pts',(28.820274444704,0.114581560721945,22.9293753109615));
#68819=CARTESIAN_POINT('Ctrl Pts',(28.8884563534747,0.409699470717337,22.9084492454292));
#68820=CARTESIAN_POINT('Ctrl Pts',(28.9492618301764,0.547097841052301,22.8992933904858));
#68821=CARTESIAN_POINT('Ctrl Pts',(29.1229462954904,0.797680554149997,22.8797437378863));
#68822=CARTESIAN_POINT('Ctrl Pts',(29.2364128570735,0.906879897838648,22.8689044954722));
#68823=CARTESIAN_POINT('Ctrl Pts',(29.4960880788397,1.07256979024568,22.8470841182882));
#68824=CARTESIAN_POINT('Ctrl Pts',(29.6390279331417,1.12873587584898,22.8363152167134));
#68825=CARTESIAN_POINT('Ctrl Pts',(29.9369514995214,1.18318311725145,22.8160900653519));
#68826=CARTESIAN_POINT('Ctrl Pts',(30.0889739777062,1.18151676550276,22.8072588330028));
#68827=CARTESIAN_POINT('Ctrl Pts',(30.3896701123462,1.11972025811827,22.7866028657307));
#68828=CARTESIAN_POINT('Ctrl Pts',(30.5349379950004,1.05803905954289,22.7754954739854));
#68829=CARTESIAN_POINT('Ctrl Pts',(30.7879462278465,0.88483838172195,22.7538182156715));
#68830=CARTESIAN_POINT('Ctrl Pts',(30.894602280459,0.776856295524231,22.7434403470977));
#68831=CARTESIAN_POINT('Ctrl Pts',(31.0642088755634,0.522314474535101,22.7240007418519));
#68832=CARTESIAN_POINT('Ctrl Pts',(31.1239021773863,0.377122301428262,22.7142407897863));
#68833=CARTESIAN_POINT('Ctrl Pts',(31.1830807507881,0.07297978420699,22.6926748121518));
#68834=CARTESIAN_POINT('Ctrl Pts',(31.1824316194307,-0.0828368341019099,
22.681626249339));
#68835=CARTESIAN_POINT('Ctrl Pts',(31.1220212984731,-0.380073436416841,
22.6605499526862));
#68836=CARTESIAN_POINT('Ctrl Pts',(31.0648726782981,-0.5190454232441,22.6511559208149));
#68837=CARTESIAN_POINT('Ctrl Pts',(30.897916936256,-0.774116322820778,22.6318603404761));
#68838=CARTESIAN_POINT('Ctrl Pts',(30.7874073117601,-0.886271721025917,
22.6210978735108));
#68839=CARTESIAN_POINT('Ctrl Pts',(30.5319280571356,-1.05901132752472,22.5992852221989));
#68840=CARTESIAN_POINT('Ctrl Pts',(30.390134598554,-1.11904322637321,22.5884496605924));
#68841=CARTESIAN_POINT('Ctrl Pts',(30.1614293865023,-1.16692310230727,22.5727078850032));
#68842=CARTESIAN_POINT('Ctrl Pts',(30.0807402688424,-1.17524047358085,22.5674580720923));
#68843=CARTESIAN_POINT('Ctrl Pts',(30.,-1.17524047358085,22.5625));
#68844=CARTESIAN_POINT('Ctrl Pts',(29.9999999999997,-1.17524047358085,22.4999999999999));
#68845=CARTESIAN_POINT('Ctrl Pts',(30.1346907701741,-1.17524047358085,22.5082710468799));
#68846=CARTESIAN_POINT('Ctrl Pts',(30.2685335864829,-1.15209385827977,22.5173106568969));
#68847=CARTESIAN_POINT('Ctrl Pts',(30.5408486178537,-1.05471955701661,22.5374851723845));
#68848=CARTESIAN_POINT('Ctrl Pts',(30.6743758210798,-0.974766233245233,
22.5485194114384));
#68849=CARTESIAN_POINT('Ctrl Pts',(30.8991023951896,-0.771359157149707,
22.5695308885782));
#68850=CARTESIAN_POINT('Ctrl Pts',(30.9894938192057,-0.651353133995038,
22.5788141945814));
#68851=CARTESIAN_POINT('Ctrl Pts',(31.1237789969096,-0.377670022359416,
22.598220372706));
#68852=CARTESIAN_POINT('Ctrl Pts',(31.1639088895479,-0.225405854113982,
22.6090170402582));
#68853=CARTESIAN_POINT('Ctrl Pts',(31.1822136536976,0.0822897394418652,
22.6308349575606));
#68854=CARTESIAN_POINT('Ctrl Pts',(31.1616041653703,0.234707632570292,22.6416425253559));
#68855=CARTESIAN_POINT('Ctrl Pts',(31.0639996311159,0.521237294982461,22.6619596199458));
#68856=CARTESIAN_POINT('Ctrl Pts',(30.9887089758802,0.652868889710107,22.6707656569643));
#68857=CARTESIAN_POINT('Ctrl Pts',(30.7885136410845,0.885402585167096,22.6913033752648));
#68858=CARTESIAN_POINT('Ctrl Pts',(30.6637241461389,0.982420191755087,22.7024060445739));
#68859=CARTESIAN_POINT('Ctrl Pts',(30.38882091141,1.11923262290395,22.724137724694));
#68860=CARTESIAN_POINT('Ctrl Pts',(30.2423409189137,1.15980775171446,22.7345712602384));
#68861=CARTESIAN_POINT('Ctrl Pts',(29.9379463484727,1.1837522744206,22.75411234554));
#68862=CARTESIAN_POINT('Ctrl Pts',(29.7828414350779,1.1653244529442,22.7636867623073));
#68863=CARTESIAN_POINT('Ctrl Pts',(29.4887538037787,1.06944336967731,22.7851453423512));
#68864=CARTESIAN_POINT('Ctrl Pts',(29.3526850446683,0.993007607592932,22.7962109417328));
#68865=CARTESIAN_POINT('Ctrl Pts',(29.1221162292212,0.795444169323972,22.8173739985243));
#68866=CARTESIAN_POINT('Ctrl Pts',(29.0284526004007,0.677845266859518,22.8269357043589));
#68867=CARTESIAN_POINT('Ctrl Pts',(28.8868197290406,0.407843425299078,22.8460808529214));
#68868=CARTESIAN_POINT('Ctrl Pts',(28.8426042638403,0.256743916657897,22.8567949374029));
#68869=CARTESIAN_POINT('Ctrl Pts',(28.8159600292804,-0.0507119050410385,
22.8785958530886));
#68870=CARTESIAN_POINT('Ctrl Pts',(28.8325649861531,-0.204026768591548,
22.8894670227908));
#68871=CARTESIAN_POINT('Ctrl Pts',(28.9226310063267,-0.492841082076786,
22.9099461162173));
#68872=CARTESIAN_POINT('Ctrl Pts',(28.994102015515,-0.625925698199416,22.918754883105));
#68873=CARTESIAN_POINT('Ctrl Pts',(29.1877542901984,-0.863760919482141,
22.9390787662067));
#68874=CARTESIAN_POINT('Ctrl Pts',(29.3102272892874,-0.964377961033194,
22.9501667983144));
#68875=CARTESIAN_POINT('Ctrl Pts',(29.5821386201159,-1.10877008329771,22.9719834809511));
#68876=CARTESIAN_POINT('Ctrl Pts',(29.7278943046296,-1.1532370774207,22.9825105195965));
#68877=CARTESIAN_POINT('Ctrl Pts',(29.9186700556686,-1.17313232338821,22.9949309755051));
#68878=CARTESIAN_POINT('Ctrl Pts',(29.9593567068785,-1.17524047358085,22.9975041899134));
#68879=CARTESIAN_POINT('Ctrl Pts',(29.9999999999995,-1.17524047358085,22.9999999999999));
#68880=CARTESIAN_POINT('Origin',(30.,-1.21864324187371E-14,15.78125));
#68881=CARTESIAN_POINT('',(30.0000000000003,-1.17524047358085,23.5625));
#68882=CARTESIAN_POINT('',(30.,-1.17524047358085,23.5));
#68883=CARTESIAN_POINT('',(30.,-1.17524047358085,15.78125));
#68884=CARTESIAN_POINT('Ctrl Pts',(30.0000000000005,-1.17524047358085,23.5625));
#68885=CARTESIAN_POINT('Ctrl Pts',(29.8877180837681,-1.1752404735809,23.5556050287134));
#68886=CARTESIAN_POINT('Ctrl Pts',(29.7758372881673,-1.15915740880452,23.548164484563));
#68887=CARTESIAN_POINT('Ctrl Pts',(29.5190446425994,-1.08346545175016,23.5297118828087));
#68888=CARTESIAN_POINT('Ctrl Pts',(29.3805019669677,-1.01066023747548,23.5186230824555));
#68889=CARTESIAN_POINT('Ctrl Pts',(29.1440648218203,-0.81906365611398,23.4973112125635));
#68890=CARTESIAN_POINT('Ctrl Pts',(29.0470865676084,-0.703844960553528,
23.4874078682461));
#68891=CARTESIAN_POINT('Ctrl Pts',(28.8981724330839,-0.43757763652763,23.4685275248886));
#68892=CARTESIAN_POINT('Ctrl Pts',(28.8499251562346,-0.287749538271772,
23.4579035929059));
#68893=CARTESIAN_POINT('Ctrl Pts',(28.8149793372208,0.0192409990811535,
23.4361356693579));
#68894=CARTESIAN_POINT('Ctrl Pts',(28.8275655785823,0.173345465604893,23.4252085109033));
#68895=CARTESIAN_POINT('Ctrl Pts',(28.9101166290744,0.46437979734691,23.4045720015899));
#68896=CARTESIAN_POINT('Ctrl Pts',(28.9778580847147,0.598927911512345,23.3956997913279));
#68897=CARTESIAN_POINT('Ctrl Pts',(29.1650362747697,0.841899704480849,23.3755913560416));
#68898=CARTESIAN_POINT('Ctrl Pts',(29.2851376881026,0.945999066866448,23.3645254962114));
#68899=CARTESIAN_POINT('Ctrl Pts',(29.5539135664443,1.09777062977422,23.3426397256705));
#68900=CARTESIAN_POINT('Ctrl Pts',(29.6988585362439,1.14604691671332,23.3320274174642));
#68901=CARTESIAN_POINT('Ctrl Pts',(30.0001600354305,1.18508412542801,23.3121411783529));
#68902=CARTESIAN_POINT('Ctrl Pts',(30.1536625413848,1.17508243739145,23.3030583378086));
#68903=CARTESIAN_POINT('Ctrl Pts',(30.4512625228178,1.09622449574564,23.2819876064994));
#68904=CARTESIAN_POINT('Ctrl Pts',(30.592110439614,1.02700793469459,23.2708844778163));
#68905=CARTESIAN_POINT('Ctrl Pts',(30.8340714315268,0.841360319080231,23.2494443144111));
#68906=CARTESIAN_POINT('Ctrl Pts',(30.9343059293982,0.728463261371192,23.2392865244689));
#68907=CARTESIAN_POINT('Ctrl Pts',(31.0901832738534,0.465790392750319,23.2204017245443));
#68908=CARTESIAN_POINT('Ctrl Pts',(31.1423055420081,0.317257314781848,23.2099959148018));
#68909=CARTESIAN_POINT('Ctrl Pts',(31.1851773743111,0.010751647338072,23.1882623721543));
#68910=CARTESIAN_POINT('Ctrl Pts',(31.1764469607209,-0.144008319910697,
23.1772887337992));
#68911=CARTESIAN_POINT('Ctrl Pts',(31.1010701340243,-0.437108167734962,
23.1565057639579));
#68912=CARTESIAN_POINT('Ctrl Pts',(31.0368218842674,-0.573070176242618,
23.1475180074206));
#68913=CARTESIAN_POINT('Ctrl Pts',(30.8568360573785,-0.819362332337596,
23.1277335191445));
#68914=CARTESIAN_POINT('Ctrl Pts',(30.7406590361852,-0.925703986430565,
23.1168291494862));
#68915=CARTESIAN_POINT('Ctrl Pts',(30.477211273408,-1.08466164141258,23.0950157923094));
#68916=CARTESIAN_POINT('Ctrl Pts',(30.3332866239118,-1.13717003604433,23.0843160955662));
#68917=CARTESIAN_POINT('Ctrl Pts',(30.1225555529996,-1.17045159552602,23.0701956350453));
#68918=CARTESIAN_POINT('Ctrl Pts',(30.0612610274847,-1.17524047358085,23.066261897193));
#68919=CARTESIAN_POINT('Ctrl Pts',(30.0000000000001,-1.17524047358085,23.0625));
#68920=CARTESIAN_POINT('Ctrl Pts',(29.9999999999995,-1.17524047358085,22.9999999999999));
#68921=CARTESIAN_POINT('Ctrl Pts',(30.1122819160637,-1.17524047358085,23.0068949712763));
#68922=CARTESIAN_POINT('Ctrl Pts',(30.2241627114991,-1.15915740885253,23.0143355154149));
#68923=CARTESIAN_POINT('Ctrl Pts',(30.4809553569443,-1.08346545195345,23.0327881171562));
#68924=CARTESIAN_POINT('Ctrl Pts',(30.6194980326123,-1.01066023773368,23.0438769175097));
#68925=CARTESIAN_POINT('Ctrl Pts',(30.8559351778473,-0.819063656461988,
23.0651887874038));
#68926=CARTESIAN_POINT('Ctrl Pts',(30.952913432109,-0.703844960936813,23.0750921317269));
#68927=CARTESIAN_POINT('Ctrl Pts',(31.1018275667414,-0.437577636966923,
23.0939724750804));
#68928=CARTESIAN_POINT('Ctrl Pts',(31.1500748436503,-0.287749538730812,
23.1045964070617));
#68929=CARTESIAN_POINT('Ctrl Pts',(31.1850206627874,0.0192409986134863,
23.126364330609));
#68930=CARTESIAN_POINT('Ctrl Pts',(31.1724344214858,0.173345465148191,23.1372914890643));
#68931=CARTESIAN_POINT('Ctrl Pts',(31.0898833711054,0.464379796922714,23.15792799838));
#68932=CARTESIAN_POINT('Ctrl Pts',(31.0221419155201,0.598927911110121,23.1668002086434));
#68933=CARTESIAN_POINT('Ctrl Pts',(30.8349637255609,0.841899704153978,23.1869086439265));
#68934=CARTESIAN_POINT('Ctrl Pts',(30.7148623122637,0.945999066590532,23.1979745037564));
#68935=CARTESIAN_POINT('Ctrl Pts',(30.4460864339697,1.09777062960664,23.2198602742982));
#68936=CARTESIAN_POINT('Ctrl Pts',(30.3011414641827,1.1460469166018,23.2304725825058));
#68937=CARTESIAN_POINT('Ctrl Pts',(29.9998399650194,1.18508412542607,23.2503588216195));
#68938=CARTESIAN_POINT('Ctrl Pts',(29.8463374590763,1.17508243744973,23.2594416621611));
#68939=CARTESIAN_POINT('Ctrl Pts',(29.5487374776195,1.09622449592641,23.2805123934674));
#68940=CARTESIAN_POINT('Ctrl Pts',(29.4078895607902,1.02700793492841,23.2916155221506));
#68941=CARTESIAN_POINT('Ctrl Pts',(29.1659285687959,0.841360319401014,23.3130556855578));
#68942=CARTESIAN_POINT('Ctrl Pts',(29.0656940708777,0.72846326172594,23.3232134755017));
#68943=CARTESIAN_POINT('Ctrl Pts',(28.9098167263205,0.465790393157422,23.3420982754308));
#68944=CARTESIAN_POINT('Ctrl Pts',(28.8576944581104,0.317257315207477,23.3525040851682));
#68945=CARTESIAN_POINT('Ctrl Pts',(28.8148226256923,0.0107516477743395,
23.3742376278149));
#68946=CARTESIAN_POINT('Ctrl Pts',(28.8235530392262,-0.144008319483296,
23.3852112661707));
#68947=CARTESIAN_POINT('Ctrl Pts',(28.8989298658185,-0.437108167337535,
23.4059942360141));
#68948=CARTESIAN_POINT('Ctrl Pts',(28.9631781155251,-0.573070175865714,
23.4149819925535));
#68949=CARTESIAN_POINT('Ctrl Pts',(29.1431639423218,-0.819362332023802,
23.4347664808262));
#68950=CARTESIAN_POINT('Ctrl Pts',(29.2593409634759,-0.925703986159073,
23.4456708504836));
#68951=CARTESIAN_POINT('Ctrl Pts',(29.5227887261992,-1.08466164124026,23.4674842076606));
#68952=CARTESIAN_POINT('Ctrl Pts',(29.6667133756817,-1.13717003592563,23.4781839044047));
#68953=CARTESIAN_POINT('Ctrl Pts',(29.8774444467245,-1.17045159550418,23.4923043649371));
#68954=CARTESIAN_POINT('Ctrl Pts',(29.9387389723772,-1.17524047358085,23.4962381027985));
#68955=CARTESIAN_POINT('Ctrl Pts',(29.9999999999999,-1.17524047358085,23.5));
#68956=CARTESIAN_POINT('Origin',(30.,-1.21864324187371E-14,15.78125));
#68957=CARTESIAN_POINT('',(30.0000000000001,-1.17524047358085,24.0625));
#68958=CARTESIAN_POINT('',(30.,-1.17524047358085,24.));
#68959=CARTESIAN_POINT('',(30.,-1.17524047358085,15.78125));
#68960=CARTESIAN_POINT('Ctrl Pts',(30.0000000000002,-1.17524047358085,24.0625));
#68961=CARTESIAN_POINT('Ctrl Pts',(29.8653092296601,-1.17524047358088,24.0542289531099));
#68962=CARTESIAN_POINT('Ctrl Pts',(29.7314664131893,-1.15209385822287,24.045189343081));
#68963=CARTESIAN_POINT('Ctrl Pts',(29.4591513817099,-1.05471955679206,24.0250148275808));
#68964=CARTESIAN_POINT('Ctrl Pts',(29.3256241785221,-0.974766232969058,
24.0139805885274));
#68965=CARTESIAN_POINT('Ctrl Pts',(29.1008976044993,-0.771359156787199,
23.99296911139));
#68966=CARTESIAN_POINT('Ctrl Pts',(29.0105061805318,-0.651353133596405,
23.9836858053905));
#68967=CARTESIAN_POINT('Ctrl Pts',(28.876221002938,-0.377670021906335,23.9642796272619));
#68968=CARTESIAN_POINT('Ctrl Pts',(28.8360911103609,-0.225405853644338,
23.9534829597086));
#68969=CARTESIAN_POINT('Ctrl Pts',(28.8177863463358,0.0822897399134218,
23.931665042406));
#68970=CARTESIAN_POINT('Ctrl Pts',(28.8383958347227,0.234707633027682,23.9208574746117));
#68971=CARTESIAN_POINT('Ctrl Pts',(28.9360003690899,0.521237295405437,23.9005403800242));
#68972=CARTESIAN_POINT('Ctrl Pts',(29.0112910243832,0.652868890111379,23.8917343430053));
#68973=CARTESIAN_POINT('Ctrl Pts',(29.211486359277,0.885402585487968,23.8711966247017));
#68974=CARTESIAN_POINT('Ctrl Pts',(29.3362758542566,0.98242019202142,23.8600939553924));
#68975=CARTESIAN_POINT('Ctrl Pts',(29.611179089029,1.11923262305578,23.8383622752737));
#68976=CARTESIAN_POINT('Ctrl Pts',(29.7576590815354,1.15980775180767,23.8279287397307));
#68977=CARTESIAN_POINT('Ctrl Pts',(30.0620536519992,1.1837522743985,23.8083876544318));
#68978=CARTESIAN_POINT('Ctrl Pts',(30.2171585654068,1.16532445285658,23.7988132376599));
#68979=CARTESIAN_POINT('Ctrl Pts',(30.5112461966771,1.06944336945855,23.7773546576131));
#68980=CARTESIAN_POINT('Ctrl Pts',(30.6473149557494,0.993007607319778,23.7662890582319));
#68981=CARTESIAN_POINT('Ctrl Pts',(30.8778837711073,0.795444168961031,23.7451260014428));
#68982=CARTESIAN_POINT('Ctrl Pts',(30.9715473998777,0.67784526646015,23.735564295613));
#68983=CARTESIAN_POINT('Ctrl Pts',(31.1131802711266,0.407843424843195,23.7164191470464));
#68984=CARTESIAN_POINT('Ctrl Pts',(31.1573957362652,0.25674391618342,23.7057050625635));
#68985=CARTESIAN_POINT('Ctrl Pts',(31.1840399706984,-0.0507119055208601,
23.6839041468775));
#68986=CARTESIAN_POINT('Ctrl Pts',(31.1674350137646,-0.204026769058537,
23.6730329771762));
#68987=CARTESIAN_POINT('Ctrl Pts',(31.0773689934766,-0.492841082509219,
23.6525538837521));
#68988=CARTESIAN_POINT('Ctrl Pts',(31.0058979842309,-0.625925698609867,
23.643745116865));
#68989=CARTESIAN_POINT('Ctrl Pts',(30.8122457094484,-0.863760919813326,
23.62342123376));
#68990=CARTESIAN_POINT('Ctrl Pts',(30.6897727103237,-0.964377961310509,
23.612333201652));
#68991=CARTESIAN_POINT('Ctrl Pts',(30.4178613794486,-1.10877008346121,23.5905165190165));
#68992=CARTESIAN_POINT('Ctrl Pts',(30.2721056949232,-1.15323707752562,23.5799894803724));
#68993=CARTESIAN_POINT('Ctrl Pts',(30.081329944032,-1.17313232340388,23.5675690244761));
#68994=CARTESIAN_POINT('Ctrl Pts',(30.0406432929718,-1.17524047358083,23.5649958100773));
#68995=CARTESIAN_POINT('Ctrl Pts',(30.0000000000005,-1.17524047358085,23.5625));
#68996=CARTESIAN_POINT('Ctrl Pts',(29.9999999999999,-1.17524047358085,23.5));
#68997=CARTESIAN_POINT('Ctrl Pts',(30.0894855238544,-1.17524047358085,23.5054950978594));
#68998=CARTESIAN_POINT('Ctrl Pts',(30.178854666788,-1.16502438903023,23.5113452474122));
#68999=CARTESIAN_POINT('Ctrl Pts',(30.4182361773703,-1.10931034894115,23.5280203800546));
#69000=CARTESIAN_POINT('Ctrl Pts',(30.5615135396518,-1.04411918207875,23.5391299800668));
#69001=CARTESIAN_POINT('Ctrl Pts',(30.8095036980223,-0.865097093436967,
23.5607054808684));
#69002=CARTESIAN_POINT('Ctrl Pts',(30.9132272713337,-0.75480290560396,23.5709852453531));
#69003=CARTESIAN_POINT('Ctrl Pts',(31.0771989331901,-0.495400927628404,
23.5902511331837));
#69004=CARTESIAN_POINT('Ctrl Pts',(31.1336431986023,-0.347374707971562,
23.6003685369235));
#69005=CARTESIAN_POINT('Ctrl Pts',(31.1845754344926,-0.0407388684447008,
23.6221113097446));
#69006=CARTESIAN_POINT('Ctrl Pts',(31.1797255553422,0.114581560252514,23.6331246890053));
#69007=CARTESIAN_POINT('Ctrl Pts',(31.1115436466863,0.409699470279596,23.6540507545398));
#69008=CARTESIAN_POINT('Ctrl Pts',(31.0507381700391,0.547097840637693,23.6632066094863));
#69009=CARTESIAN_POINT('Ctrl Pts',(30.877053704825,0.797680553802843,23.6827562620821));
#69010=CARTESIAN_POINT('Ctrl Pts',(30.7635871432854,0.906879897536129,23.6935955044951));
#69011=CARTESIAN_POINT('Ctrl Pts',(30.5039119215803,1.07256979004896,23.7154158816792));
#69012=CARTESIAN_POINT('Ctrl Pts',(30.3609720672946,1.12873587571,23.726184783255));
#69013=CARTESIAN_POINT('Ctrl Pts',(30.0630485009405,1.18318311722529,23.7464099346189));
#69014=CARTESIAN_POINT('Ctrl Pts',(29.9110260227659,1.18151676553675,23.755241166967));
#69015=CARTESIAN_POINT('Ctrl Pts',(29.6103298881048,1.1197202582759,23.7758971342361));
#69016=CARTESIAN_POINT('Ctrl Pts',(29.46506200542,1.05803905975613,23.7870045259814));
#69017=CARTESIAN_POINT('Ctrl Pts',(29.2120537724961,0.884838382027716,23.8086817842968));
#69018=CARTESIAN_POINT('Ctrl Pts',(29.1053977198379,0.776856295866943,23.8190596528721));
#69019=CARTESIAN_POINT('Ctrl Pts',(28.9357911246459,0.52231447495466,23.8384992581206));
#69020=CARTESIAN_POINT('Ctrl Pts',(28.8760978227722,0.377122301892393,23.8482592101808));
#69021=CARTESIAN_POINT('Ctrl Pts',(28.816919249242,0.0729797847098555,23.8698251878126));
#69022=CARTESIAN_POINT('Ctrl Pts',(28.8175683805337,-0.0828368336059415,
23.8808737506258));
#69023=CARTESIAN_POINT('Ctrl Pts',(28.8779787013698,-0.380073435953635,
23.9019500472809));
#69024=CARTESIAN_POINT('Ctrl Pts',(28.9351273214881,-0.519045422805617,
23.9113440791565));
#69025=CARTESIAN_POINT('Ctrl Pts',(29.1020830634255,-0.774116322451291,
23.9306396594913));
#69026=CARTESIAN_POINT('Ctrl Pts',(29.212592687875,-0.88627172070161,23.9414021264554));
#69027=CARTESIAN_POINT('Ctrl Pts',(29.4680719424329,-1.05901132730886,23.963214777767));
#69028=CARTESIAN_POINT('Ctrl Pts',(29.609865400996,-1.11904322621712,23.9740503393744));
#69029=CARTESIAN_POINT('Ctrl Pts',(29.8385706131875,-1.1669231022752,23.9897921149766));
#69030=CARTESIAN_POINT('Ctrl Pts',(29.9192597310019,-1.17524047358085,23.9950419278981));
#69031=CARTESIAN_POINT('Ctrl Pts',(30.,-1.17524047358085,24.));
#69032=CARTESIAN_POINT('Origin',(30.,-1.21864324187371E-14,15.78125));
#69033=CARTESIAN_POINT('',(29.9999999962159,-1.17524047358085,24.5624999995353));
#69034=CARTESIAN_POINT('',(30.0000000000002,-1.17524047358085,24.5));
#69035=CARTESIAN_POINT('',(30.,-1.17524047358085,15.78125));
#69036=CARTESIAN_POINT('Ctrl Pts',(29.9999999924319,-1.17524047358085,24.5624999995353));
#69037=CARTESIAN_POINT('Ctrl Pts',(29.8449382921852,-1.17524047258231,24.5529780211908));
#69038=CARTESIAN_POINT('Ctrl Pts',(29.6912874372683,-1.14455036315003,24.5424546005433));
#69039=CARTESIAN_POINT('Ctrl Pts',(29.4063853758944,-1.0258343762565,24.5207505023134));
#69040=CARTESIAN_POINT('Ctrl Pts',(29.2777080162496,-0.939688490130196,
24.5097945313951));
#69041=CARTESIAN_POINT('Ctrl Pts',(29.0636971062813,-0.72579687417109,24.4890693621447));
#69042=CARTESIAN_POINT('Ctrl Pts',(28.9792543776096,-0.601260808557374,
24.4801338851547));
#69043=CARTESIAN_POINT('Ctrl Pts',(28.8587167668904,-0.3209315497576,24.4602564455228));
#69044=CARTESIAN_POINT('Ctrl Pts',(28.8262532459446,-0.166807893138082,
24.449327926347));
#69045=CARTESIAN_POINT('Ctrl Pts',(28.823406512149,0.140728845641508,24.4275212730356));
#69046=CARTESIAN_POINT('Ctrl Pts',(28.851353518733,0.291209583843224,24.4168510640028));
#69047=CARTESIAN_POINT('Ctrl Pts',(28.9629467293987,0.573358103335639,24.3968446251906));
#69048=CARTESIAN_POINT('Ctrl Pts',(29.0455390967654,0.702301510494977,24.3878786774254));
#69049=CARTESIAN_POINT('Ctrl Pts',(29.2579957317181,0.924591935160839,24.3669511834331));
#69050=CARTESIAN_POINT('Ctrl Pts',(29.3868926291043,1.01465868024229,24.3558427221105));
#69051=CARTESIAN_POINT('Ctrl Pts',(29.6668973327643,1.13696430638437,24.3343120930999));
#69052=CARTESIAN_POINT('Ctrl Pts',(29.8144674232288,1.17014774293813,24.3240736802882));
#69053=CARTESIAN_POINT('Ctrl Pts',(30.1216534355145,1.17947691079308,24.3048793479835));
#69054=CARTESIAN_POINT('Ctrl Pts',(30.2784124097871,1.15260328295164,24.2946007685524));
#69055=CARTESIAN_POINT('Ctrl Pts',(30.5685961343608,1.03996407129779,24.2727877800628));
#69056=CARTESIAN_POINT('Ctrl Pts',(30.6996254486415,0.956741717213513,24.2617910312175));
#69057=CARTESIAN_POINT('Ctrl Pts',(30.9187688591,0.747835373953449,24.2409274335984));
#69058=CARTESIAN_POINT('Ctrl Pts',(31.006053860002,0.625488945893405,24.2318518411732));
#69059=CARTESIAN_POINT('Ctrl Pts',(31.1332209274868,0.348324830571042,24.2121988338701));
#69060=CARTESIAN_POINT('Ctrl Pts',(31.1693830920172,0.195045950853365,24.2013302156905));
#69061=CARTESIAN_POINT('Ctrl Pts',(31.1796570639592,-0.112665031805443,
24.1795112071857));
#69062=CARTESIAN_POINT('Ctrl Pts',(31.1552218060231,-0.264121048947789,
24.1687718435869));
#69063=CARTESIAN_POINT('Ctrl Pts',(31.0503552824464,-0.548400595365726,
24.1486142990383));
#69064=CARTESIAN_POINT('Ctrl Pts',(30.9713114905908,-0.678634752411996,
24.1397525078141));
#69065=CARTESIAN_POINT('Ctrl Pts',(30.7647686763693,-0.905919595273436,
24.119011097007));
#69066=CARTESIAN_POINT('Ctrl Pts',(30.6378140048735,-0.999372205084128,
24.1079018617007));
#69067=CARTESIAN_POINT('Ctrl Pts',(30.3601860918747,-1.12872343710904,24.0862673928177));
#69068=CARTESIAN_POINT('Ctrl Pts',(30.2130976252741,-1.16548763290266,24.0759316041108));
#69069=CARTESIAN_POINT('Ctrl Pts',(30.042024216247,-1.17467745886824,24.065100570339));
#69070=CARTESIAN_POINT('Ctrl Pts',(30.021003006896,-1.17524047358085,24.0637897457965));
#69071=CARTESIAN_POINT('Ctrl Pts',(30.0000000000002,-1.17524047358085,24.0625));
#69072=CARTESIAN_POINT('Ctrl Pts',(30.,-1.17524047358085,24.));
#69073=CARTESIAN_POINT('Ctrl Pts',(30.068631292987,-1.17524047358085,24.0042144880528));
#69074=CARTESIAN_POINT('Ctrl Pts',(30.1372731197099,-1.16923029330172,24.0086427063088));
#69075=CARTESIAN_POINT('Ctrl Pts',(30.3594639555913,-1.12983827430394,24.0236835229636));
#69076=CARTESIAN_POINT('Ctrl Pts',(30.5067279557135,-1.07189657495913,24.034780912417));
#69077=CARTESIAN_POINT('Ctrl Pts',(30.7648494491756,-0.904940985120749,
24.0565507524641));
#69078=CARTESIAN_POINT('Ctrl Pts',(30.8745226735525,-0.799463570900332,
24.0670250985558));
#69079=CARTESIAN_POINT('Ctrl Pts',(31.0499651911362,-0.550024618872908,
24.0866421584515));
#69080=CARTESIAN_POINT('Ctrl Pts',(31.1129833274185,-0.407722194144101,
24.0960894491163));
#69081=CARTESIAN_POINT('Ctrl Pts',(31.1806136864057,-0.106256135243321,
24.117465645852));
#69082=CARTESIAN_POINT('Ctrl Pts',(31.1843316043204,0.0499559746584703,
24.1285422519746));
#69083=CARTESIAN_POINT('Ctrl Pts',(31.131994520367,0.349324836152535,24.1497697417397));
#69084=CARTESIAN_POINT('Ctrl Pts',(31.0785837311869,0.489956671487056,24.1594708103671));
#69085=CARTESIAN_POINT('Ctrl Pts',(30.9185303965388,0.749536525439823,24.1785023892068));
#69086=CARTESIAN_POINT('Ctrl Pts',(30.8111165172128,0.864620133839068,24.1891785696567));
#69087=CARTESIAN_POINT('Ctrl Pts',(30.5601137220937,1.04443640550787,24.2109672262292));
#69088=CARTESIAN_POINT('Ctrl Pts',(30.4195953268947,1.10838743812269,24.2218634370972));
#69089=CARTESIAN_POINT('Ctrl Pts',(30.125226440525,1.17808176086598,24.2424108698401));
#69090=CARTESIAN_POINT('Ctrl Pts',(29.9745000794406,1.18444262103543,24.2512396402881));
#69091=CARTESIAN_POINT('Ctrl Pts',(29.671168206001,1.13918974904968,24.2714709284502));
#69092=CARTESIAN_POINT('Ctrl Pts',(29.5219912146071,1.08506931535676,24.2825503121002));
#69093=CARTESIAN_POINT('Ctrl Pts',(29.2588817407465,0.924538989806815,24.3043986527903));
#69094=CARTESIAN_POINT('Ctrl Pts',(29.1462343920073,0.821663056130735,24.3149634007337));
#69095=CARTESIAN_POINT('Ctrl Pts',(28.9649893539032,0.577368135519195,24.3347544047798));
#69096=CARTESIAN_POINT('Ctrl Pts',(28.8986993951907,0.437889260784583,24.3439503786226));
#69097=CARTESIAN_POINT('Ctrl Pts',(28.8227562109677,0.139172903579825,24.3651316009568));
#69098=CARTESIAN_POINT('Ctrl Pts',(28.814686650905,-0.0173128945475468,
24.3762276136201));
#69099=CARTESIAN_POINT('Ctrl Pts',(28.8589720780878,-0.318736522506238,
24.3976008016849));
#69100=CARTESIAN_POINT('Ctrl Pts',(28.9087096405855,-0.46104932706788,24.4076656524993));
#69101=CARTESIAN_POINT('Ctrl Pts',(29.0619693077579,-0.724977765539007,
24.4264342215945));
#69102=CARTESIAN_POINT('Ctrl Pts',(29.1662794308695,-0.84283884374432,24.4370182792792));
#69103=CARTESIAN_POINT('Ctrl Pts',(29.4127142037999,-1.0294613008905,24.4587677289451));
#69104=CARTESIAN_POINT('Ctrl Pts',(29.5518825792064,-1.09722011413893,24.4697160382912));
#69105=CARTESIAN_POINT('Ctrl Pts',(29.7982117366005,-1.1622217216024,24.4871470887339));
#69106=CARTESIAN_POINT('Ctrl Pts',(29.8989795683345,-1.17524047358088,24.4937965702842));
#69107=CARTESIAN_POINT('Ctrl Pts',(30.0000000000003,-1.17524047358085,24.5));
#69108=CARTESIAN_POINT('Origin',(30.,-1.21864324187371E-14,15.78125));
#69109=CARTESIAN_POINT('',(29.9999999999999,-1.17524047358085,25.0625));
#69110=CARTESIAN_POINT('',(30.0000000000002,-1.17524047358085,25.));
#69111=CARTESIAN_POINT('',(30.,-1.17524047358085,15.78125));
#69112=CARTESIAN_POINT('Ctrl Pts',(29.9999999999998,-1.17524047358085,25.0625));
#69113=CARTESIAN_POINT('Ctrl Pts',(29.9787160795735,-1.17524047358085,25.0611930039571));
#69114=CARTESIAN_POINT('Ctrl Pts',(29.9574135577721,-1.17466229796152,25.0598643671606));
#69115=CARTESIAN_POINT('Ctrl Pts',(29.7860545064693,-1.16533366685381,25.0490108716001));
#69116=CARTESIAN_POINT('Ctrl Pts',(29.638982260427,-1.12845915516134,25.0386721678491));
#69117=CARTESIAN_POINT('Ctrl Pts',(29.3614303849904,-0.998891400573746,
25.0170346917219));
#69118=CARTESIAN_POINT('Ctrl Pts',(29.2345369639167,-0.905335034780717,
25.0059255391243));
#69119=CARTESIAN_POINT('Ctrl Pts',(29.0281770961676,-0.677897334966365,
24.9851899432843));
#69120=CARTESIAN_POINT('Ctrl Pts',(28.9492422426318,-0.547623084588669,
24.9763305695037));
#69121=CARTESIAN_POINT('Ctrl Pts',(28.8429395559285,-0.25880932586385,24.9558515154165));
#69122=CARTESIAN_POINT('Ctrl Pts',(28.8187785161156,-0.102338490894112,
24.9447565638831));
#69123=CARTESIAN_POINT('Ctrl Pts',(28.8329707062525,0.20487723468326,24.9229726728069));
#69124=CARTESIAN_POINT('Ctrl Pts',(28.8688620223111,0.352813948215486,24.9124828541373));
#69125=CARTESIAN_POINT('Ctrl Pts',(28.9959383633127,0.629882762331914,24.8928366044019));
#69126=CARTESIAN_POINT('Ctrl Pts',(29.0869818629053,0.755846556300386,24.8834354015886));
#69127=CARTESIAN_POINT('Ctrl Pts',(29.3131553782924,0.966129203680405,24.8620913064548));
#69128=CARTESIAN_POINT('Ctrl Pts',(29.4462640631474,1.04811028996687,24.8510108758816));
#69129=CARTESIAN_POINT('Ctrl Pts',(29.731323759893,1.1538048728599,24.8297587550632));
#69130=CARTESIAN_POINT('Ctrl Pts',(29.8797531248391,1.17853792828451,24.8200009879783));
#69131=CARTESIAN_POINT('Ctrl Pts',(30.1846496308258,1.17107054148177,24.8010132560253));
#69132=CARTESIAN_POINT('Ctrl Pts',(30.3381730792388,1.13627251448872,24.7903520180859));
#69133=CARTESIAN_POINT('Ctrl Pts',(30.6200199170605,1.01003478142549,24.7685688600169));
#69134=CARTESIAN_POINT('Ctrl Pts',(30.7461080027782,0.920828764814659,24.7576633973259));
#69135=CARTESIAN_POINT('Ctrl Pts',(30.954589658464,0.701638656166971,24.7370899153526));
#69136=CARTESIAN_POINT('Ctrl Pts',(31.0359799147447,0.574699574292555,24.7282504951265));
#69137=CARTESIAN_POINT('Ctrl Pts',(31.1497275829798,0.289883112537678,24.7080548792676));
#69138=CARTESIAN_POINT('Ctrl Pts',(31.1781418190148,0.133683865658838,24.6969791852295));
#69139=CARTESIAN_POINT('Ctrl Pts',(31.1719905418774,-0.174601531099527,
24.6751194464719));
#69140=CARTESIAN_POINT('Ctrl Pts',(31.1398342436188,-0.323793762033814,
24.6645406022347));
#69141=CARTESIAN_POINT('Ctrl Pts',(31.020088030022,-0.603297917753395,24.644721668578));
#69142=CARTESIAN_POINT('Ctrl Pts',(30.9330960022514,-0.730676428588708,
24.6355607116713));
#69143=CARTESIAN_POINT('Ctrl Pts',(30.7134327937131,-0.946735070008641,
24.6144116187632));
#69144=CARTESIAN_POINT('Ctrl Pts',(30.5822707418913,-1.03259356059966,24.6033132579239));
#69145=CARTESIAN_POINT('Ctrl Pts',(30.299587098649,-1.14619538675731,24.5819267037008));
#69146=CARTESIAN_POINT('Ctrl Pts',(30.1515439291036,-1.17497884081411,24.5718152360255));
#69147=CARTESIAN_POINT('Ctrl Pts',(30.0013618111703,-1.17523988185447,24.5625836466351));
#69148=CARTESIAN_POINT('Ctrl Pts',(30.0006808894801,-1.17524047358524,24.5625418118389));
#69149=CARTESIAN_POINT('Ctrl Pts',(29.9999999924319,-1.17524047358085,24.5624999995353));
#69150=CARTESIAN_POINT('Ctrl Pts',(30.0000000000003,-1.17524047358085,24.5));
#69151=CARTESIAN_POINT('Ctrl Pts',(30.0475989786694,-1.17524047358084,24.5029229425557));
#69152=CARTESIAN_POINT('Ctrl Pts',(30.0952413712801,-1.17234913261358,24.5059510599029));
#69153=CARTESIAN_POINT('Ctrl Pts',(30.2990650070911,-1.14742109537484,24.5193511873216));
#69154=CARTESIAN_POINT('Ctrl Pts',(30.4499960157575,-1.0970416910395,24.5304056476212));
#69155=CARTESIAN_POINT('Ctrl Pts',(30.7177665488108,-0.942842462676014,
24.5523157520592));
#69156=CARTESIAN_POINT('Ctrl Pts',(30.833223349596,-0.842552715174129,24.5629613319529));
#69157=CARTESIAN_POINT('Ctrl Pts',(31.0200068112404,-0.603233885310555,
24.5829160166926));
#69158=CARTESIAN_POINT('Ctrl Pts',(31.0893943876237,-0.466400998056969,
24.591928683353));
#69159=CARTESIAN_POINT('Ctrl Pts',(31.1731872619397,-0.170385863873932,
24.612918368786));
#69160=CARTESIAN_POINT('Ctrl Pts',(31.185412882504,-0.0137497619841131,
24.6240250391094));
#69161=CARTESIAN_POINT('Ctrl Pts',(31.1488612218191,0.289356743431089,24.6455175557638));
#69162=CARTESIAN_POINT('Ctrl Pts',(31.1026857517696,0.433263084173784,24.6557215908795));
#69163=CARTESIAN_POINT('Ctrl Pts',(30.9558437041525,0.701308793163264,24.6747280350226));
#69164=CARTESIAN_POINT('Ctrl Pts',(30.8545058913013,0.821789237632239,24.6849956137961));
#69165=CARTESIAN_POINT('Ctrl Pts',(30.6123622815668,1.01480099766359,24.7067080777764));
#69166=CARTESIAN_POINT('Ctrl Pts',(30.4745499588497,1.08610079838188,24.7176986563197));
#69167=CARTESIAN_POINT('Ctrl Pts',(30.1837738406509,1.17031056558872,24.7385400922772));
#69168=CARTESIAN_POINT('Ctrl Pts',(30.0341022035471,1.18415559329136,24.7475897886987));
#69169=CARTESIAN_POINT('Ctrl Pts',(29.7305751526436,1.15452627151871,24.7672791490145));
#69170=CARTESIAN_POINT('Ctrl Pts',(29.5799242663497,1.10861951554252,24.7781578355522));
#69171=CARTESIAN_POINT('Ctrl Pts',(29.3089128663366,0.962634653740643,24.7999757240996));
#69172=CARTESIAN_POINT('Ctrl Pts',(29.1903801371545,0.865330006275208,24.8107043566494));
#69173=CARTESIAN_POINT('Ctrl Pts',(28.9974547059893,0.631606479932577,24.8308378310304));
#69174=CARTESIAN_POINT('Ctrl Pts',(28.9246531642855,0.497649505166107,24.8397129306474));
#69175=CARTESIAN_POINT('Ctrl Pts',(28.8322520407485,0.204711362593916,24.8604844343777));
#69176=CARTESIAN_POINT('Ctrl Pts',(28.8154219514347,0.0480344797090969,
24.8715939963785));
#69177=CARTESIAN_POINT('Ctrl Pts',(28.8433837526351,-0.256851307347509,
24.8932126773996));
#69178=CARTESIAN_POINT('Ctrl Pts',(28.8856263759144,-0.402401296034548,
24.9035332594392));
#69179=CARTESIAN_POINT('Ctrl Pts',(29.0254132564532,-0.675115053553108,
24.9228707031121));
#69180=CARTESIAN_POINT('Ctrl Pts',(29.1237053106631,-0.798585223889617,
24.932834945393));
#69181=CARTESIAN_POINT('Ctrl Pts',(29.3612206915393,-0.998444700238917,
24.9545059777387));
#69182=CARTESIAN_POINT('Ctrl Pts',(29.4974844913312,-1.07350395274647,24.9655347517064));
#69183=CARTESIAN_POINT('Ctrl Pts',(29.7595519260122,-1.15671325178265,24.9845777838555));
#69184=CARTESIAN_POINT('Ctrl Pts',(29.8794906495254,-1.17524047358089,24.9925998011151));
#69185=CARTESIAN_POINT('Ctrl Pts',(30.0000000000004,-1.17524047358085,25.));
#69186=CARTESIAN_POINT('Origin',(30.,-1.21864324187371E-14,15.78125));
#69187=CARTESIAN_POINT('',(29.9999999999997,-1.17524047358085,25.5625));
#69188=CARTESIAN_POINT('',(30.,-1.17524047358085,25.5));
#69189=CARTESIAN_POINT('',(30.,-1.17524047358085,15.78125));
#69190=CARTESIAN_POINT('Ctrl Pts',(29.9999999999995,-1.17524047358085,25.5625));
#69191=CARTESIAN_POINT('Ctrl Pts',(29.9590631434842,-1.17524047358085,25.5599861628683));
#69192=CARTESIAN_POINT('Ctrl Pts',(29.9180826982373,-1.17310176284205,25.557393823766));
#69193=CARTESIAN_POINT('Ctrl Pts',(29.7270170759755,-1.15303120939534,25.5449493522346));
#69194=CARTESIAN_POINT('Ctrl Pts',(29.5812843667667,-1.10844931412058,25.534419650774));
#69195=CARTESIAN_POINT('Ctrl Pts',(29.3094646041477,-0.963834030512161,
25.5126006792245));
#69196=CARTESIAN_POINT('Ctrl Pts',(29.1870616253517,-0.863111358786919,
25.5015132019157));
#69197=CARTESIAN_POINT('Ctrl Pts',(28.9936035835609,-0.625120486304078,
25.4811957277874));
#69198=CARTESIAN_POINT('Ctrl Pts',(28.922245153506,-0.491992360156719,25.4723859354899));
#69199=CARTESIAN_POINT('Ctrl Pts',(28.8324037582581,-0.203110856662721,
25.4519020777895));
#69200=CARTESIAN_POINT('Ctrl Pts',(28.8159185655927,-0.0497708721110285,
25.4410291268206));
#69201=CARTESIAN_POINT('Ctrl Pts',(28.8428111724951,0.257674311776114,25.4192289654353));
#69202=CARTESIAN_POINT('Ctrl Pts',(28.8871477746036,0.408737403201897,25.4085174632064));
#69203=CARTESIAN_POINT('Ctrl Pts',(29.028998912458,0.678628541452795,25.389380164336));
#69204=CARTESIAN_POINT('Ctrl Pts',(29.1227608288482,0.796156039557689,25.3798091767006));
#69205=CARTESIAN_POINT('Ctrl Pts',(29.3535044180399,0.99354320653279,25.3586416369362));
#69206=CARTESIAN_POINT('Ctrl Pts',(29.4896480206548,1.06987223772086,25.3475752255981));
#69207=CARTESIAN_POINT('Ctrl Pts',(29.7837920452496,1.16549604577304,25.326122303941));
#69208=CARTESIAN_POINT('Ctrl Pts',(29.9388720345248,1.18379547475176,25.3165570329261));
#69209=CARTESIAN_POINT('Ctrl Pts',(30.243221825482,1.15962478745302,25.2970106790485));
#69210=CARTESIAN_POINT('Ctrl Pts',(30.3896819125524,1.11893466510606,25.2865742888993));
#69211=CARTESIAN_POINT('Ctrl Pts',(30.664499787972,0.981897695245122,25.2648398897594));
#69212=CARTESIAN_POINT('Ctrl Pts',(30.7892223684277,0.884773136061606,25.2537375376443));
#69213=CARTESIAN_POINT('Ctrl Pts',(30.9892253393634,0.652081932327525,25.233206047704));
#69214=CARTESIAN_POINT('Ctrl Pts',(31.0644029101032,0.520407945827758,25.2244008128923));
#69215=CARTESIAN_POINT('Ctrl Pts',(31.1617865735135,0.233810524226684,25.2040789136694));
#69216=CARTESIAN_POINT('Ctrl Pts',(31.1822791704619,0.0813648687854731,
25.1932693773186));
#69217=CARTESIAN_POINT('Ctrl Pts',(31.1637300195375,-0.226326940808914,
25.1714517283273));
#69218=CARTESIAN_POINT('Ctrl Pts',(31.1234798971667,-0.378558584977568,
25.1606573669753));
#69219=CARTESIAN_POINT('Ctrl Pts',(30.9889788141031,-0.652134792227603,
25.1412587691706));
#69220=CARTESIAN_POINT('Ctrl Pts',(30.8984922205339,-0.772069973056249,
25.1319682180917));
#69221=CARTESIAN_POINT('Ctrl Pts',(30.6735951228457,-0.975307798919531,
25.1109522700489));
#69222=CARTESIAN_POINT('Ctrl Pts',(30.5399926661631,-1.05515984400593,25.0999170005632));
#69223=CARTESIAN_POINT('Ctrl Pts',(30.2678908596704,-1.15220558793873,25.0797672273045));
#69224=CARTESIAN_POINT('Ctrl Pts',(30.1343655548317,-1.17524047358085,25.0707510761622));
#69225=CARTESIAN_POINT('Ctrl Pts',(29.9999999999998,-1.17524047358085,25.0625));
#69226=CARTESIAN_POINT('Ctrl Pts',(30.0000000000004,-1.17524047358085,25.));
#69227=CARTESIAN_POINT('Ctrl Pts',(30.0280011909949,-1.17524047358084,25.0017194880028));
#69228=CARTESIAN_POINT('Ctrl Pts',(30.056028863347,-1.17423978093536,25.0034760804581));
#69229=CARTESIAN_POINT('Ctrl Pts',(30.2395952618035,-1.16108096396762,25.0152149952129));
#69230=CARTESIAN_POINT('Ctrl Pts',(30.3913571022497,-1.11907669842983,25.0260235449911));
#69231=CARTESIAN_POINT('Ctrl Pts',(30.6663605367685,-0.979972388704826,
25.0478426338075));
#69232=CARTESIAN_POINT('Ctrl Pts',(30.7876235644496,-0.885461952247295,
25.0586398624147));
#69233=CARTESIAN_POINT('Ctrl Pts',(30.9860830879355,-0.656850945315206,
25.0789319146131));
#69234=CARTESIAN_POINT('Ctrl Pts',(31.0619486284351,-0.525431380274417,
25.0877429880603));
#69235=CARTESIAN_POINT('Ctrl Pts',(31.162019301378,-0.235334014571736,25.1083130594786));
#69236=CARTESIAN_POINT('Ctrl Pts',(31.182987818821,-0.0787326337506094,
25.1194172678187));
#69237=CARTESIAN_POINT('Ctrl Pts',(31.162785126869,0.227544173273347,25.1411345825519));
#69238=CARTESIAN_POINT('Ctrl Pts',(31.1241144207896,0.374476178584838,25.1515531598995));
#69239=CARTESIAN_POINT('Ctrl Pts',(30.9915168317796,0.649674032406111,25.1710667445663));
#69240=CARTESIAN_POINT('Ctrl Pts',(30.8973599492461,0.774562668596496,25.1806896874262));
#69241=CARTESIAN_POINT('Ctrl Pts',(30.6662666830193,0.980382528688255,25.202177670528));
#69242=CARTESIAN_POINT('Ctrl Pts',(30.531751815152,1.05938687434591,25.2132389149495));
#69243=CARTESIAN_POINT('Ctrl Pts',(30.2450331875533,1.15903498558282,25.2343785368368));
#69244=CARTESIAN_POINT('Ctrl Pts',(30.0962908441082,1.18072042198942,25.2438927186044));
#69245=CARTESIAN_POINT('Ctrl Pts',(29.7917163095273,1.16710140491111,25.2630787773242));
#69246=CARTESIAN_POINT('Ctrl Pts',(29.638905788045,1.12920096781154,25.2738062281113));
#69247=CARTESIAN_POINT('Ctrl Pts',(29.3599222216531,0.997398530499289,25.2956108489033));
#69248=CARTESIAN_POINT('Ctrl Pts',(29.2358774116296,0.905886016991888,25.3064726127214));
#69249=CARTESIAN_POINT('Ctrl Pts',(29.0316806530828,0.682639701770527,25.32692677681));
#69250=CARTESIAN_POINT('Ctrl Pts',(28.9526524211366,0.553805209269406,25.3357310715183));
#69251=CARTESIAN_POINT('Ctrl Pts',(28.844720062577,0.266708452558536,25.3560883773325));
#69252=CARTESIAN_POINT('Ctrl Pts',(28.8194808141697,0.110295910906438,25.3671791955642));
#69253=CARTESIAN_POINT('Ctrl Pts',(28.8316382042729,-0.197210560241239,
25.3889837026743));
#69254=CARTESIAN_POINT('Ctrl Pts',(28.8665861506279,-0.345474523822663,
25.3994967258182));
#69255=CARTESIAN_POINT('Ctrl Pts',(28.9918018301732,-0.623166741842213,
25.4191871795497));
#69256=CARTESIAN_POINT('Ctrl Pts',(29.081808144475,-0.749490769071139,25.4285215559887));
#69257=CARTESIAN_POINT('Ctrl Pts',(29.3063266217772,-0.961255466999539,
25.449816563314));
#69258=CARTESIAN_POINT('Ctrl Pts',(29.438949602445,-1.04422897408056,25.4609023529488));
#69259=CARTESIAN_POINT('Ctrl Pts',(29.7169259241077,-1.14948331999011,25.4817038921344));
#69260=CARTESIAN_POINT('Ctrl Pts',(29.8579333178884,-1.17524047358086,25.4912760155257));
#69261=CARTESIAN_POINT('Ctrl Pts',(30.,-1.17524047358085,25.5));
#69262=CARTESIAN_POINT('Origin',(30.,-1.21864324187371E-14,15.78125));
#69263=CARTESIAN_POINT('',(30.,-1.17524047358085,26.0625));
#69264=CARTESIAN_POINT('',(30.,-1.17524047358085,26.));
#69265=CARTESIAN_POINT('',(30.,-1.17524047358085,15.78125));
#69266=CARTESIAN_POINT('Ctrl Pts',(29.9999999999999,-1.17524047358085,26.0625));
#69267=CARTESIAN_POINT('Ctrl Pts',(29.9384679078155,-1.17524047358085,26.0587214573544));
#69268=CARTESIAN_POINT('Ctrl Pts',(29.8769029052424,-1.17040913172972,26.054769604635));
#69269=CARTESIAN_POINT('Ctrl Pts',(29.6659154234359,-1.13693724882076,26.0406266508408));
#69270=CARTESIAN_POINT('Ctrl Pts',(29.5220177711255,-1.084323597792,26.0299248801994));
#69271=CARTESIAN_POINT('Ctrl Pts',(29.2586759114222,-0.925171378535031,
26.0081111282534));
#69272=CARTESIAN_POINT('Ctrl Pts',(29.1425757110306,-0.818746672431791,
25.9972085314777));
#69273=CARTESIAN_POINT('Ctrl Pts',(28.9627703960609,-0.572330389052239,
25.9774307272425));
#69274=CARTESIAN_POINT('Ctrl Pts',(28.8986210699436,-0.436327710221708,
25.9684388957715));
#69275=CARTESIAN_POINT('Ctrl Pts',(28.8234492804003,-0.143169608738148,
25.9476517953103));
#69276=CARTESIAN_POINT('Ctrl Pts',(28.8148292891501,0.0116076754049962,
25.936676929058));
#69277=CARTESIAN_POINT('Ctrl Pts',(28.8579269079672,0.318093458602922,25.9149447963521));
#69278=CARTESIAN_POINT('Ctrl Pts',(28.910158206845,0.466589649123026,25.9045489692953));
#69279=CARTESIAN_POINT('Ctrl Pts',(29.0662354765119,0.729159361472922,25.8856555497038));
#69280=CARTESIAN_POINT('Ctrl Pts',(29.1665620010353,0.841989757161643,25.8754944720367));
#69281=CARTESIAN_POINT('Ctrl Pts',(29.4086828051808,1.02746666351878,25.8540505472151));
#69282=CARTESIAN_POINT('Ctrl Pts',(29.5495956219979,1.09657907822105,25.84294712555));
#69283=CARTESIAN_POINT('Ctrl Pts',(29.8472420936479,1.17519666348882,25.8218820609165));
#69284=CARTESIAN_POINT('Ctrl Pts',(30.000722767755,1.18508027808238,25.8128044743545));
#69285=CARTESIAN_POINT('Ctrl Pts',(30.3019786609575,1.14582802588677,25.7929134117055));
#69286=CARTESIAN_POINT('Ctrl Pts',(30.4468987068161,1.09744171612032,25.7822987333));
#69287=CARTESIAN_POINT('Ctrl Pts',(30.7155809567247,0.94545759821414,25.7604111763944));
#69288=CARTESIAN_POINT('Ctrl Pts',(30.835612326607,0.841258259962285,25.7493460732515));
#69289=CARTESIAN_POINT('Ctrl Pts',(31.0226024258984,0.598138792258194,25.7292439525602));
#69290=CARTESIAN_POINT('Ctrl Pts',(31.0902361983429,0.463547729361891,25.7203689985712));
#69291=CARTESIAN_POINT('Ctrl Pts',(31.1725680326408,0.172449502286477,25.6997279586011));
#69292=CARTESIAN_POINT('Ctrl Pts',(31.1850367066478,0.0183235805600113,
25.6887992788123));
#69293=CARTESIAN_POINT('Ctrl Pts',(31.149849032726,-0.288650006825612,25.6670325571437));
#69294=CARTESIAN_POINT('Ctrl Pts',(31.1014848231134,-0.438439388995189,
25.6564113704209));
#69295=CARTESIAN_POINT('Ctrl Pts',(30.9523589365019,-0.704596833564904,
25.637538818338));
#69296=CARTESIAN_POINT('Ctrl Pts',(30.8552831525205,-0.819746342004528,
25.6276245442916));
#69297=CARTESIAN_POINT('Ctrl Pts',(30.6186741800399,-1.01116668038418,25.6063083713552));
#69298=CARTESIAN_POINT('Ctrl Pts',(30.4800603026513,-1.08386414646939,25.5952190187437));
#69299=CARTESIAN_POINT('Ctrl Pts',(30.2235083443405,-1.15925176820215,25.5767919868584));
#69300=CARTESIAN_POINT('Ctrl Pts',(30.1119520742388,-1.17524047358085,25.5693747164571));
#69301=CARTESIAN_POINT('Ctrl Pts',(29.9999999999995,-1.17524047358085,25.5625));
#69302=CARTESIAN_POINT('Ctrl Pts',(30.,-1.17524047358085,25.5));
#69303=CARTESIAN_POINT('Ctrl Pts',(30.0069574643761,-1.17524047358085,25.5004272417029));
#69304=CARTESIAN_POINT('Ctrl Pts',(30.01391720466,-1.17517869098561,25.5008568135879));
#69305=CARTESIAN_POINT('Ctrl Pts',(30.1767683930213,-1.17228514742378,25.5109597131747));
#69306=CARTESIAN_POINT('Ctrl Pts',(30.3305146751184,-1.13852257214804,25.5215979241794));
#69307=CARTESIAN_POINT('Ctrl Pts',(30.613289571589,-1.01415059475931,25.5433719241602));
#69308=CARTESIAN_POINT('Ctrl Pts',(30.7400483172667,-0.925722033283128,
25.5542910068295));
#69309=CARTESIAN_POINT('Ctrl Pts',(30.9499509146168,-0.707886564918499,
25.5749037184647));
#69310=CARTESIAN_POINT('Ctrl Pts',(31.0321249523172,-0.581569550980178,
25.5837623721801));
#69311=CARTESIAN_POINT('Ctrl Pts',(31.1477905785375,-0.297516308572578,
25.6039038700829));
#69312=CARTESIAN_POINT('Ctrl Pts',(31.1772544504942,-0.141401249469257,
25.6149735945785));
#69313=CARTESIAN_POINT('Ctrl Pts',(31.1730934439483,0.167116297568546,25.636849794526));
#69314=CARTESIAN_POINT('Ctrl Pts',(31.1418645520009,0.316603789635784,25.6474495749843));
#69315=CARTESIAN_POINT('Ctrl Pts',(31.0239238826678,0.596699382032703,25.6673104459219));
#69316=CARTESIAN_POINT('Ctrl Pts',(30.9379157361151,0.724424917792123,25.6764216802641));
#69317=CARTESIAN_POINT('Ctrl Pts',(30.7198518445296,0.941880855114492,25.6975221021999));
#69318=CARTESIAN_POINT('Ctrl Pts',(30.5891826263813,1.02868094414498,25.7086235824532));
#69319=CARTESIAN_POINT('Ctrl Pts',(30.3070725150413,1.14422525077315,25.730043785608));
#69320=CARTESIAN_POINT('Ctrl Pts',(30.1591233913896,1.1739884490527,25.7401842137377));
#69321=CARTESIAN_POINT('Ctrl Pts',(29.8537619113516,1.17646530259176,25.7590235656117));
#69322=CARTESIAN_POINT('Ctrl Pts',(29.6991872299891,1.1467452303545,25.7694824753175));
#69323=CARTESIAN_POINT('Ctrl Pts',(29.4128145699134,1.02954198968741,25.7912232470859));
#69324=CARTESIAN_POINT('Ctrl Pts',(29.2835235645903,0.944145175996724,25.8021903431407));
#69325=CARTESIAN_POINT('Ctrl Pts',(29.0681842616351,0.731537563632497,25.8229515631887));
#69326=CARTESIAN_POINT('Ctrl Pts',(28.9830068906091,0.607571894150497,25.8319186117076));
#69327=CARTESIAN_POINT('Ctrl Pts',(28.8607454143127,0.328058458525624,25.851738203379));
#69328=CARTESIAN_POINT('Ctrl Pts',(28.8273201029076,0.174145192049772,25.8626518043211));
#69329=CARTESIAN_POINT('Ctrl Pts',(28.8225473943512,-0.133454152009573,
25.8844628968148));
#69330=CARTESIAN_POINT('Ctrl Pts',(28.849586199068,-0.284195707441678,25.8951515997385));
#69331=CARTESIAN_POINT('Ctrl Pts',(28.9594336647467,-0.566901683792667,
25.9151975664084));
#69332=CARTESIAN_POINT('Ctrl Pts',(29.0410981500453,-0.696179869303813,
25.9241315793102));
#69333=CARTESIAN_POINT('Ctrl Pts',(29.2520170527073,-0.919779045076863,
25.9450110448572));
#69334=CARTESIAN_POINT('Ctrl Pts',(29.3804160320669,-1.01073211613404,25.95612035376));
#69335=CARTESIAN_POINT('Ctrl Pts',(29.6598179734432,-1.13487834137248,25.9776792246572));
#69336=CARTESIAN_POINT('Ctrl Pts',(29.8072708469184,-1.1689955596726,25.9879435454987));
#69337=CARTESIAN_POINT('Ctrl Pts',(29.9714632607541,-1.17498080122199,25.9982384188692));
#69338=CARTESIAN_POINT('Ctrl Pts',(29.9857363066776,-1.17524047358085,25.9991240997731));
#69339=CARTESIAN_POINT('Ctrl Pts',(29.9999999999999,-1.17524047358085,26.));
#69340=CARTESIAN_POINT('Origin',(30.,-1.21864324187371E-14,15.78125));
#69341=CARTESIAN_POINT('',(30.,-1.17524047358085,26.5625));
#69342=CARTESIAN_POINT('',(29.9999999999997,-1.17524047358085,26.4999999999999));
#69343=CARTESIAN_POINT('',(30.,-1.17524047358085,15.78125));
#69344=CARTESIAN_POINT('Ctrl Pts',(30.,-1.17524047358085,26.5625));
#69345=CARTESIAN_POINT('Ctrl Pts',(29.9189538385986,-1.17524047358085,26.5575231437572));
#69346=CARTESIAN_POINT('Ctrl Pts',(29.8379609361797,-1.16685998242801,26.5522524382954));
#69347=CARTESIAN_POINT('Ctrl Pts',(29.6089811727034,-1.1187361642345,26.5364851544771));
#69348=CARTESIAN_POINT('Ctrl Pts',(29.4672242547403,-1.05858684051961,26.5256476735947));
#69349=CARTESIAN_POINT('Ctrl Pts',(29.2118758464994,-0.885634166979752,
26.5038355032321));
#69350=CARTESIAN_POINT('Ctrl Pts',(29.1014575353795,-0.773390023233997,
26.4930754972477));
#69351=CARTESIAN_POINT('Ctrl Pts',(28.9347073730369,-0.518183463481665,
26.4737877314199));
#69352=CARTESIAN_POINT('Ctrl Pts',(28.8776702380248,-0.379162720284378,
26.4643854707334));
#69353=CARTESIAN_POINT('Ctrl Pts',(28.8174988609875,-0.0818619971934983,
26.4433046274383));
#69354=CARTESIAN_POINT('Ctrl Pts',(28.8169789681977,0.0739680819649894,
26.4322551101507));
#69355=CARTESIAN_POINT('Ctrl Pts',(28.8764093680924,0.378032609649621,26.4106946625572));
#69356=CARTESIAN_POINT('Ctrl Pts',(28.9362017786302,0.523138441896699,26.4009448281074));
#69357=CARTESIAN_POINT('Ctrl Pts',(29.1059813583505,0.777530022962841,26.3814999268455));
#69358=CARTESIAN_POINT('Ctrl Pts',(29.2127271628307,0.885439479708375,26.3711191218038));
#69359=CARTESIAN_POINT('Ctrl Pts',(29.4658882417733,1.05845819806925,26.3494389287095));
#69360=CARTESIAN_POINT('Ctrl Pts',(29.6112162771377,1.12003007041528,26.3383317191495));
#69361=CARTESIAN_POINT('Ctrl Pts',(29.9119535931961,1.18158358217449,26.3176818381253));
#69362=CARTESIAN_POINT('Ctrl Pts',(30.0639561135899,1.18313176493728,26.308852379607));
#69363=CARTESIAN_POINT('Ctrl Pts',(30.3618294498414,1.12846284091072,26.2886224532834));
#69364=CARTESIAN_POINT('Ctrl Pts',(30.5047372110283,1.07218329091309,26.2778514997354));
#69365=CARTESIAN_POINT('Ctrl Pts',(30.7642923496518,0.906285517829887,26.2560311264309));
#69366=CARTESIAN_POINT('Ctrl Pts',(30.8776734787023,0.796998466194141,26.2451940206555));
#69367=CARTESIAN_POINT('Ctrl Pts',(31.0511614964728,0.546283376197254,26.2256517381869));
#69368=CARTESIAN_POINT('Ctrl Pts',(31.1118599586541,0.408839660981002,26.2164897876345));
#69369=CARTESIAN_POINT('Ctrl Pts',(31.179816298086,0.113659355972694,26.1955592978295));
#69370=CARTESIAN_POINT('Ctrl Pts',(31.1845443559052,-0.0416770721755796,
26.1845447840881));
#69371=CARTESIAN_POINT('Ctrl Pts',(31.1333712501869,-0.348241759846019,
26.1628070564654));
#69372=CARTESIAN_POINT('Ctrl Pts',(31.0768319553006,-0.496185033349922,
26.1527007984472));
#69373=CARTESIAN_POINT('Ctrl Pts',(30.9126965034022,-0.755446668894444,
26.1334298283147));
#69374=CARTESIAN_POINT('Ctrl Pts',(30.8088874743598,-0.865675121928193,
26.1231471467367));
#69375=CARTESIAN_POINT('Ctrl Pts',(30.5607504336079,-1.04453090463544,26.1015685223966));
#69376=CARTESIAN_POINT('Ctrl Pts',(30.4174143875892,-1.10962145980108,26.0904588858133));
#69377=CARTESIAN_POINT('Ctrl Pts',(30.1782678600435,-1.16509155074858,26.0738068318412));
#69378=CARTESIAN_POINT('Ctrl Pts',(30.0891908090061,-1.17524047358085,26.0679770001062));
#69379=CARTESIAN_POINT('Ctrl Pts',(29.9999999999999,-1.17524047358085,26.0625));
#69380=CARTESIAN_POINT('Ctrl Pts',(29.9999999999999,-1.17524047358085,26.));
#69381=CARTESIAN_POINT('Ctrl Pts',(30.1425333221801,-1.17524047358085,26.0087526397553));
#69382=CARTESIAN_POINT('Ctrl Pts',(30.2840219111895,-1.14931710997616,26.0183602049923));
#69383=CARTESIAN_POINT('Ctrl Pts',(30.561367295123,-1.04389937746679,26.0391287924253));
#69384=CARTESIAN_POINT('Ctrl Pts',(30.6930583893841,-0.961526015756511,
26.0501360796874));
#69385=CARTESIAN_POINT('Ctrl Pts',(30.9136669465422,-0.754054974126117,
26.0710387617507));
#69386=CARTESIAN_POINT('Ctrl Pts',(31.0017654739708,-0.632326756940585,
26.0801633069178));
#69387=CARTESIAN_POINT('Ctrl Pts',(31.130809796733,-0.356072448301099,26.0997518021271));
#69388=CARTESIAN_POINT('Ctrl Pts',(31.1680189550385,-0.20305033553964,26.1106022136104));
#69389=CARTESIAN_POINT('Ctrl Pts',(31.1804056537492,0.10467710494643,26.1324223890981));
#69390=CARTESIAN_POINT('Ctrl Pts',(31.1569739806732,0.256395498849484,26.1431803571703));
#69391=CARTESIAN_POINT('Ctrl Pts',(31.0540187102742,0.541272174052999,26.1633802426127));
#69392=CARTESIAN_POINT('Ctrl Pts',(30.9759701950171,0.671873752670431,26.1722217092774));
#69393=CARTESIAN_POINT('Ctrl Pts',(30.7711018756191,0.900554058237447,26.1929097676203));
#69394=CARTESIAN_POINT('Ctrl Pts',(30.6447103916025,0.994954099829424,26.2040180088908));
#69395=CARTESIAN_POINT('Ctrl Pts',(30.3677839906361,1.12628386016982,26.2256795457743));
#69396=CARTESIAN_POINT('Ctrl Pts',(30.2208469191431,1.16405670623833,26.2360417980814));
#69397=CARTESIAN_POINT('Ctrl Pts',(29.9153739917407,1.18247957177519,26.2554533393943));
#69398=CARTESIAN_POINT('Ctrl Pts',(29.7596534858204,1.16089584886057,26.265267690896));
#69399=CARTESIAN_POINT('Ctrl Pts',(29.4669798482834,1.05871377618554,26.2868628344935));
#69400=CARTESIAN_POINT('Ctrl Pts',(29.3327683310263,0.97968769950255,26.2979062213058));
#69401=CARTESIAN_POINT('Ctrl Pts',(29.1064857982236,0.777827856716442,26.3189583910466));
#69402=CARTESIAN_POINT('Ctrl Pts',(29.0152252755147,0.658466900754918,26.3283097753497));
#69403=CARTESIAN_POINT('Ctrl Pts',(28.8789732904358,0.385760488964649,26.3476466981555));
#69404=CARTESIAN_POINT('Ctrl Pts',(28.8377485021289,0.233796400613908,26.3584220878003));
#69405=CARTESIAN_POINT('Ctrl Pts',(28.8172159011814,-0.0738574561607104,
26.3802370456529));
#69406=CARTESIAN_POINT('Ctrl Pts',(28.8367587774233,-0.226525134118623,
26.3910623250595));
#69407=CARTESIAN_POINT('Ctrl Pts',(28.9323498389723,-0.513670658612161,
26.411423088874));
#69408=CARTESIAN_POINT('Ctrl Pts',(29.0066122735479,-0.645689070611162,
26.4202237943573));
#69409=CARTESIAN_POINT('Ctrl Pts',(29.2050554476303,-0.879653705731429,
26.4407046487027));
#69410=CARTESIAN_POINT('Ctrl Pts',(29.329232754846,-0.977642983590833,26.4518041743651));
#69411=CARTESIAN_POINT('Ctrl Pts',(29.6033526154654,-1.11649688151574,26.4735601269295));
#69412=CARTESIAN_POINT('Ctrl Pts',(29.7496481694863,-1.15811817689029,26.4840194270505));
#69413=CARTESIAN_POINT('Ctrl Pts',(29.9332052808561,-1.1738184735254,26.4958478764586));
#69414=CARTESIAN_POINT('Ctrl Pts',(29.9666204732331,-1.17524047358085,26.4979502409084));
#69415=CARTESIAN_POINT('Ctrl Pts',(29.9999999999995,-1.17524047358085,26.4999999999999));
#69416=CARTESIAN_POINT('Origin',(30.,-1.21864324187371E-14,15.78125));
#69417=CARTESIAN_POINT('',(30.0000000000002,-1.17524047358085,27.0625));
#69418=CARTESIAN_POINT('',(29.9999999999999,-1.17524047358085,26.9999999999999));
#69419=CARTESIAN_POINT('',(30.,-1.17524047358085,15.78125));
#69420=CARTESIAN_POINT('Ctrl Pts',(30.0000000000003,-1.17524047358085,27.0625));
#69421=CARTESIAN_POINT('Ctrl Pts',(29.898686590649,-1.17524047358088,27.0562785792061));
#69422=CARTESIAN_POINT('Ctrl Pts',(29.7976296484377,-1.16214610940709,27.0496086633191));
#69423=CARTESIAN_POINT('Ctrl Pts',(29.5510548806291,-1.0968832857528,27.032153269422));
#69424=CARTESIAN_POINT('Ctrl Pts',(29.4119274187945,-1.02901377051944,27.0212035476842));
#69425=CARTESIAN_POINT('Ctrl Pts',(29.1656287201027,-0.842194481232163,
26.9994554755857));
#69426=CARTESIAN_POINT('Ctrl Pts',(29.0614102622354,-0.72425366568988,26.9888742198639));
#69427=CARTESIAN_POINT('Ctrl Pts',(28.9083494936521,-0.460199204673261,
26.9701133966982));
#69428=CARTESIAN_POINT('Ctrl Pts',(28.8587194637877,-0.317836463591476,
26.960036980781));
#69429=CARTESIAN_POINT('Ctrl Pts',(28.8146713989512,-0.0163533730831442,
26.9386595763769));
#69430=CARTESIAN_POINT('Ctrl Pts',(28.8228691179041,0.140138676728786,26.9275631204225));
#69431=CARTESIAN_POINT('Ctrl Pts',(28.8990556060477,0.438772825908234,26.9063877272517));
#69432=CARTESIAN_POINT('Ctrl Pts',(28.9654414239268,0.578169376458166,26.8971982372258));
#69433=CARTESIAN_POINT('Ctrl Pts',(29.1468572533747,0.822311817466142,26.8774021512523));
#69434=CARTESIAN_POINT('Ctrl Pts',(29.259591693584,0.925109502257862,26.8668348294397));
#69435=CARTESIAN_POINT('Ctrl Pts',(29.522846414638,1.08544747155122,26.8449843892055));
#69436=CARTESIAN_POINT('Ctrl Pts',(29.672078571298,1.13945389610578,26.8339056600349));
#69437=CARTESIAN_POINT('Ctrl Pts',(29.9754469871149,1.18446101454497,26.813680840772));
#69438=CARTESIAN_POINT('Ctrl Pts',(30.1261553208811,1.17798106873351,26.804850259546));
#69439=CARTESIAN_POINT('Ctrl Pts',(30.4204691708303,1.10805786050355,26.7842980916158));
#69440=CARTESIAN_POINT('Ctrl Pts',(30.5609479127602,1.04399036631935,26.7734001867649));
#69441=CARTESIAN_POINT('Ctrl Pts',(30.8118142126087,0.8639649033663,26.7516124954367));
#69442=CARTESIAN_POINT('Ctrl Pts',(30.9191345732301,0.748795351296203,26.7409390107287));
#69443=CARTESIAN_POINT('Ctrl Pts',(31.0789814493982,0.489082061456906,26.7219153792232));
#69444=CARTESIAN_POINT('Ctrl Pts',(31.13228056467,0.348399841671576,26.7122041527178));
#69445=CARTESIAN_POINT('Ctrl Pts',(31.1843745315803,0.0489678760358684,
26.6909721883974));
#69446=CARTESIAN_POINT('Ctrl Pts',(31.1805251276485,-0.10725425723734,26.6798948715428));
#69447=CARTESIAN_POINT('Ctrl Pts',(31.112642066065,-0.408638429750164,26.658524481164));
#69448=CARTESIAN_POINT('Ctrl Pts',(31.04952452927,-0.550854728541633,26.6490856679416));
#69449=CARTESIAN_POINT('Ctrl Pts',(30.8739065476105,-0.80013916056119,26.6294633115169));
#69450=CARTESIAN_POINT('Ctrl Pts',(30.7641429817239,-0.90553953226469,26.6189861492083));
#69451=CARTESIAN_POINT('Ctrl Pts',(30.5058691930861,-1.0723039712914,26.5972137340794));
#69452=CARTESIAN_POINT('Ctrl Pts',(30.3585462682162,-1.13013161506019,26.5861167698907));
#69453=CARTESIAN_POINT('Ctrl Pts',(30.1366295806596,-1.1692866034305,26.5711011916684));
#69454=CARTESIAN_POINT('Ctrl Pts',(30.0683089619122,-1.17524047358085,26.5666946944513));
#69455=CARTESIAN_POINT('Ctrl Pts',(30.,-1.17524047358085,26.5625));
#69456=CARTESIAN_POINT('Ctrl Pts',(29.9999999999995,-1.17524047358085,26.4999999999999));
#69457=CARTESIAN_POINT('Ctrl Pts',(30.1204914385722,-1.17524047358085,26.5073990989566));
#69458=CARTESIAN_POINT('Ctrl Pts',(30.2404377363977,-1.1567191282047,26.5154213729959));
#69459=CARTESIAN_POINT('Ctrl Pts',(30.503109066672,-1.07331217218126,26.5345084966475));
#69460=CARTESIAN_POINT('Ctrl Pts',(30.6398547835573,-0.997848639879795,
26.5455811972524));
#69461=CARTESIAN_POINT('Ctrl Pts',(30.8720104636609,-0.801888849767787,
26.566784844391));
#69462=CARTESIAN_POINT('Ctrl Pts',(30.9665674240944,-0.684937055709897,
26.5764328435252));
#69463=CARTESIAN_POINT('Ctrl Pts',(31.1101788342394,-0.415941539318355,
26.595506636112));
#69464=CARTESIAN_POINT('Ctrl Pts',(31.1554918067157,-0.265175979373474,
26.606197041135));
#69465=CARTESIAN_POINT('Ctrl Pts',(31.184388668241,0.0421759563922281,26.6279905905315));
#69466=CARTESIAN_POINT('Ctrl Pts',(31.1688709786064,0.195715280062819,26.6388776761339));
#69467=CARTESIAN_POINT('Ctrl Pts',(31.080842595015,0.4851372161482,26.6593998545441));
#69468=CARTESIAN_POINT('Ctrl Pts',(31.0103902901456,0.618617027917578,26.6682199013902));
#69469=CARTESIAN_POINT('Ctrl Pts',(30.8184983590075,0.857859380695496,26.6884855739597));
#69470=CARTESIAN_POINT('Ctrl Pts',(30.6966625458602,0.959431158368461,26.6995683269243));
#69471=CARTESIAN_POINT('Ctrl Pts',(30.4255868085001,1.10584185104675,26.7214052635744));
#69472=CARTESIAN_POINT('Ctrl Pts',(30.280042417997,1.15134883169079,26.7319561985547));
#69473=CARTESIAN_POINT('Ctrl Pts',(29.9776063567648,1.18496921576007,26.7517200618056));
#69474=CARTESIAN_POINT('Ctrl Pts',(29.8235440457018,1.17197554004672,26.7609515037779));
#69475=CARTESIAN_POINT('Ctrl Pts',(29.5271473201095,1.08704252411486,26.7821637300309));
#69476=CARTESIAN_POINT('Ctrl Pts',(29.3879639883513,1.01521369745337,26.7932572549969));
#69477=CARTESIAN_POINT('Ctrl Pts',(29.1499744927664,0.825212607812385,26.8146078849744));
#69478=CARTESIAN_POINT('Ctrl Pts',(29.0521140662545,0.710618013126823,26.8246118717047));
#69479=CARTESIAN_POINT('Ctrl Pts',(28.9012898027458,0.445344450507133,26.8434217499511));
#69480=CARTESIAN_POINT('Ctrl Pts',(28.8519884644377,0.295869143296566,26.8540206664119));
#69481=CARTESIAN_POINT('Ctrl Pts',(28.8148602582687,-0.0109614775297701,
26.8757772506829));
#69482=CARTESIAN_POINT('Ctrl Pts',(28.8263846212866,-0.165256365046284,
26.886717911409));
#69483=CARTESIAN_POINT('Ctrl Pts',(28.90695684434,-0.456865689279699,26.9073951919876));
#69484=CARTESIAN_POINT('Ctrl Pts',(28.9737284626765,-0.591802058760263,
26.9162939800796));
#69485=CARTESIAN_POINT('Ctrl Pts',(29.1592103949543,-0.836102522890621,
26.9363453584795));
#69486=CARTESIAN_POINT('Ctrl Pts',(29.2786778563743,-0.94110103302348,26.9474041669452));
#69487=CARTESIAN_POINT('Ctrl Pts',(29.5466042812102,-1.09478566204523,26.9693055998652));
#69488=CARTESIAN_POINT('Ctrl Pts',(29.6913217184938,-1.14405280529544,26.9799390653881));
#69489=CARTESIAN_POINT('Ctrl Pts',(29.8940937627055,-1.17166523876262,26.9933697888908));
#69490=CARTESIAN_POINT('Ctrl Pts',(29.9470693710243,-1.17524047358085,26.9967496532013));
#69491=CARTESIAN_POINT('Ctrl Pts',(29.9999999999997,-1.17524047358085,26.9999999999999));
#69492=CARTESIAN_POINT('Origin',(30.,-1.21864324187371E-14,15.78125));
#69493=CARTESIAN_POINT('',(30.0000000000002,-1.17524047358085,27.5625));
#69494=CARTESIAN_POINT('',(30.,-1.17524047358085,27.5));
#69495=CARTESIAN_POINT('',(30.,-1.17524047358085,15.78125));
#69496=CARTESIAN_POINT('Ctrl Pts',(30.0000000000004,-1.17524047358085,27.5625));
#69497=CARTESIAN_POINT('Ctrl Pts',(29.8791981655177,-1.17524047358089,27.5550818403526));
#69498=CARTESIAN_POINT('Ctrl Pts',(29.7589726578968,-1.15662316573575,27.547039018461));
#69499=CARTESIAN_POINT('Ctrl Pts',(29.4966785757901,-1.0731279551929,27.5279719317893));
#69500=CARTESIAN_POINT('Ctrl Pts',(29.3604611797136,-0.99796015863462,27.5169421590736));
#69501=CARTESIAN_POINT('Ctrl Pts',(29.1231210583237,-0.797935915977368,
27.495276047424));
#69502=CARTESIAN_POINT('Ctrl Pts',(29.0249429590029,-0.674426740918645,
27.4853218966019));
#69503=CARTESIAN_POINT('Ctrl Pts',(28.8853520572172,-0.401644540260052,
27.4659795997989));
#69504=CARTESIAN_POINT('Ctrl Pts',(28.8432060655213,-0.256055793645229,
27.4556562695324));
#69505=CARTESIAN_POINT('Ctrl Pts',(28.8154546971309,0.0488704066146756,
27.4340347229132));
#69506=CARTESIAN_POINT('Ctrl Pts',(28.8323972811925,0.205546638674019,27.4229252070608));
#69507=CARTESIAN_POINT('Ctrl Pts',(28.9250076761164,0.498408501969224,27.4021591121013));
#69508=CARTESIAN_POINT('Ctrl Pts',(28.997892508521,0.632295921050251,27.3932865033313));
#69509=CARTESIAN_POINT('Ctrl Pts',(29.1909681621961,0.865881565904131,27.3731486925495));
#69510=CARTESIAN_POINT('Ctrl Pts',(29.3095755456334,0.963111668503783,27.3624181185496));
#69511=CARTESIAN_POINT('Ctrl Pts',(29.5806971724252,1.10891198583092,27.3406000040234));
#69512=CARTESIAN_POINT('Ctrl Pts',(29.7313794614454,1.15471361111034,27.3297231163935));
#69513=CARTESIAN_POINT('Ctrl Pts',(30.0349224077729,1.1841311566887,27.3100402882342));
#69514=CARTESIAN_POINT('Ctrl Pts',(30.1845806615862,1.17018311962186,27.3009860288447));
#69515=CARTESIAN_POINT('Ctrl Pts',(30.4753054258698,1.08577187813399,27.2801406033955));
#69516=CARTESIAN_POINT('Ctrl Pts',(30.6130774728742,1.01437069747224,27.2691489037921));
#69517=CARTESIAN_POINT('Ctrl Pts',(30.8550923899249,0.82117912160722,27.2474379673869));
#69518=CARTESIAN_POINT('Ctrl Pts',(30.9563451215602,0.700625408948211,27.2371795779744));
#69519=CARTESIAN_POINT('Ctrl Pts',(31.1030012085855,0.43246305141941,27.218164862578));
#69520=CARTESIAN_POINT('Ctrl Pts',(31.1490749245368,0.288512534258167,27.207957695024));
#69521=CARTESIAN_POINT('Ctrl Pts',(31.1854037082186,-0.0146433585393976,
27.1864616764351));
#69522=CARTESIAN_POINT('Ctrl Pts',(31.173058308365,-0.171282192075426,27.1753548124176));
#69523=CARTESIAN_POINT('Ctrl Pts',(31.089040383827,-0.467218401344852,27.1543707233508));
#69524=CARTESIAN_POINT('Ctrl Pts',(31.0195638166583,-0.603975746358807,
27.1453625116794));
#69525=CARTESIAN_POINT('Ctrl Pts',(30.8326207012815,-0.843150163878356,
27.1254031429327));
#69526=CARTESIAN_POINT('Ctrl Pts',(30.7170833899544,-0.943363872050058,
27.1147553149523));
#69527=CARTESIAN_POINT('Ctrl Pts',(30.4491800434626,-1.09737775442843,27.0928436259578));
#69528=CARTESIAN_POINT('Ctrl Pts',(30.2981995637065,-1.14764798518389,27.0817899983651));
#69529=CARTESIAN_POINT('Ctrl Pts',(30.0946434783266,-1.17238533021172,27.0684130613475));
#69530=CARTESIAN_POINT('Ctrl Pts',(30.0473000417297,-1.17524047358084,27.0654045855337));
#69531=CARTESIAN_POINT('Ctrl Pts',(30.0000000000003,-1.17524047358085,27.0625));
#69532=CARTESIAN_POINT('Ctrl Pts',(29.9999999999997,-1.17524047358085,26.9999999999999));
#69533=CARTESIAN_POINT('Ctrl Pts',(30.0986058905517,-1.17524047358085,27.0060551583626));
#69534=CARTESIAN_POINT('Ctrl Pts',(30.197001235846,-1.16283641910558,27.0125371577158));
#69535=CARTESIAN_POINT('Ctrl Pts',(30.4435331990926,-1.0993899448342,27.029925526711));
#69536=CARTESIAN_POINT('Ctrl Pts',(30.5849622280491,-1.0311122983099,27.0410310521114));
#69537=CARTESIAN_POINT('Ctrl Pts',(30.8283565317534,-0.84700506573289,27.0625046195245));
#69538=CARTESIAN_POINT('Ctrl Pts',(30.9294172599309,-0.734710314399227,
27.0726917923361));
#69539=CARTESIAN_POINT('Ctrl Pts',(31.0870905034712,-0.472970868314495,
27.0916537809288));
#69540=CARTESIAN_POINT('Ctrl Pts',(31.1401926761717,-0.324772377450416,
27.1019712110874));
#69541=CARTESIAN_POINT('Ctrl Pts',(31.1850952185403,-0.0184511332937437,
27.1236916767454));
#69542=CARTESIAN_POINT('Ctrl Pts',(31.1773587357349,0.136461808282747,27.1346761621237));
#69543=CARTESIAN_POINT('Ctrl Pts',(31.1038267733963,0.430084241190232,27.1554961871532));
#69544=CARTESIAN_POINT('Ctrl Pts',(31.0404668538449,0.566412733303589,27.1645221322455));
#69545=CARTESIAN_POINT('Ctrl Pts',(30.8621032542639,0.813817787312719,27.1842464597062));
#69546=CARTESIAN_POINT('Ctrl Pts',(30.746618378735,0.920903307832853,27.195134699154));
#69547=CARTESIAN_POINT('Ctrl Pts',(30.4841269758582,1.08160589165682,27.2169511927423));
#69548=CARTESIAN_POINT('Ctrl Pts',(30.3404475283553,1.13505921838268,27.2276693335753));
#69549=CARTESIAN_POINT('Ctrl Pts',(30.0413373449537,1.18420822105003,27.2477795099651));
#69550=CARTESIAN_POINT('Ctrl Pts',(29.8888261880251,1.17970362185606,27.2566686898965));
#69551=CARTESIAN_POINT('Ctrl Pts',(29.5891419642887,1.11207867848515,27.2774691579106));
#69552=CARTESIAN_POINT('Ctrl Pts',(29.4453407649054,1.04779159085184,27.2885788725534));
#69553=CARTESIAN_POINT('Ctrl Pts',(29.1960372639306,0.870265103883027,27.3101819980009));
#69554=CARTESIAN_POINT('Ctrl Pts',(29.091548794378,0.760562756134129,27.3204877500418));
#69555=CARTESIAN_POINT('Ctrl Pts',(28.9261102653187,0.502419631695097,27.3397990837129));
#69556=CARTESIAN_POINT('Ctrl Pts',(28.8688162363146,0.355135077347701,27.3498182687336));
#69557=CARTESIAN_POINT('Ctrl Pts',(28.8157293168355,0.0491393235848099,
27.3715156546901));
#69558=CARTESIAN_POINT('Ctrl Pts',(28.8194875433144,-0.106321035237959,
27.3825389560425));
#69559=CARTESIAN_POINT('Ctrl Pts',(28.8856486083743,-0.401996025014571,
27.4035045226948));
#69560=CARTESIAN_POINT('Ctrl Pts',(28.9454972717022,-0.539801328338099,
27.4127167480926));
#69561=CARTESIAN_POINT('Ctrl Pts',(29.11742422097,-0.791565441680741,27.4322003607736));
#69562=CARTESIAN_POINT('Ctrl Pts',(29.2301245105903,-0.901546472787143,
27.4430202619491));
#69563=CARTESIAN_POINT('Ctrl Pts',(29.4887201815225,-1.06909180163981,27.4648401285834));
#69564=CARTESIAN_POINT('Ctrl Pts',(29.6313699534066,-1.1262717375032,27.4756271616522));
#69565=CARTESIAN_POINT('Ctrl Pts',(29.853348441796,-1.16837939045814,27.4907512179135));
#69566=CARTESIAN_POINT('Ctrl Pts',(29.9266702080884,-1.17524047358085,27.4954969880578));
#69567=CARTESIAN_POINT('Ctrl Pts',(30.,-1.17524047358085,27.5));
#69568=CARTESIAN_POINT('Origin',(30.,-1.21864324187371E-14,15.78125));
#69569=CARTESIAN_POINT('',(30.,-1.17524047358085,28.0625));
#69570=CARTESIAN_POINT('',(30.0000000000001,-1.17524047358085,28.));
#69571=CARTESIAN_POINT('',(30.,-1.17524047358085,15.78125));
#69572=CARTESIAN_POINT('Ctrl Pts',(30.,-1.17524047358085,28.0625));
#69573=CARTESIAN_POINT('Ctrl Pts',(29.8576309526277,-1.17524047358085,28.0537574479785));
#69574=CARTESIAN_POINT('Ctrl Pts',(29.7163289872701,-1.14937338079985,28.0441633378768));
#69575=CARTESIAN_POINT('Ctrl Pts',(29.4381412694858,-1.0437960185582,28.0233373652109));
#69576=CARTESIAN_POINT('Ctrl Pts',(29.3055725204167,-0.960712774920266,
28.0122510152415));
#69577=CARTESIAN_POINT('Ctrl Pts',(29.0812375157914,-0.748784364739409,
27.9909614703353));
#69578=CARTESIAN_POINT('Ctrl Pts',(28.991345872443,-0.622420436003701,27.9816342608879));
#69579=CARTESIAN_POINT('Ctrl Pts',(28.8663365712296,-0.344659291734443,
27.9619389197703));
#69580=CARTESIAN_POINT('Ctrl Pts',(28.8314934625426,-0.196359386622749,
27.9514233481032));
#69581=CARTESIAN_POINT('Ctrl Pts',(28.8195620391171,0.111178530712451,27.9296166112233));
#69582=CARTESIAN_POINT('Ctrl Pts',(28.8449209434754,0.267584161126331,27.9185262830501));
#69583=CARTESIAN_POINT('Ctrl Pts',(28.9530728770119,0.554595748995939,27.8981750163432));
#69584=CARTESIAN_POINT('Ctrl Pts',(29.0321899221582,0.683358417415679,27.8893700226253));
#69585=CARTESIAN_POINT('Ctrl Pts',(29.2365478324768,0.90645295573766,27.8689113436395));
#69586=CARTESIAN_POINT('Ctrl Pts',(29.3606700385593,0.997879761432882,27.8580478657718));
#69587=CARTESIAN_POINT('Ctrl Pts',(29.6397630167776,1.12947461119937,27.8362438860083));
#69588=CARTESIAN_POINT('Ctrl Pts',(29.7926014521638,1.16725893043214,27.8255188379057));
#69589=CARTESIAN_POINT('Ctrl Pts',(30.0971888483988,1.18064726325309,27.8063401680006));
#69590=CARTESIAN_POINT('Ctrl Pts',(30.2459190189188,1.15884794264961,27.7968175086224));
#69591=CARTESIAN_POINT('Ctrl Pts',(30.5325764826745,1.05897425995597,27.7756736453134));
#69592=CARTESIAN_POINT('Ctrl Pts',(30.6670400332198,0.979858412729581,27.7646115990219));
#69593=CARTESIAN_POINT('Ctrl Pts',(30.8979501916997,0.773870883397489,27.7431289156398));
#69594=CARTESIAN_POINT('Ctrl Pts',(30.9919903689524,0.648942084588862,27.7335148439956));
#69595=CARTESIAN_POINT('Ctrl Pts',(31.1243827012244,0.373674108325156,27.7139962871235));
#69596=CARTESIAN_POINT('Ctrl Pts',(31.1629506296625,0.226703861102418,27.7035749981386));
#69597=CARTESIAN_POINT('Ctrl Pts',(31.182930645767,-0.0796098768690557,
27.6818550647252));
#69598=CARTESIAN_POINT('Ctrl Pts',(31.1618436472684,-0.236207537040712,
27.6707511202069));
#69599=CARTESIAN_POINT('Ctrl Pts',(31.0615541749908,-0.526222674013738,
27.6501868794201));
#69600=CARTESIAN_POINT('Ctrl Pts',(30.9856010212307,-0.657569956578418,
27.641376820382));
#69601=CARTESIAN_POINT('Ctrl Pts',(30.7869826832863,-0.886033452367878,
27.6210802455783));
#69602=CARTESIAN_POINT('Ctrl Pts',(30.6656419827339,-0.980462303947253,
27.6102811397496));
#69603=CARTESIAN_POINT('Ctrl Pts',(30.3905261901255,-1.11936682731598,27.5884622344572));
#69604=CARTESIAN_POINT('Ctrl Pts',(30.2387339000707,-1.16125829953858,27.5776558137839));
#69605=CARTESIAN_POINT('Ctrl Pts',(30.0554488466051,-1.17426038713893,27.5659397324124));
#69606=CARTESIAN_POINT('Ctrl Pts',(30.0277113777332,-1.17524047358084,27.5642016912446));
#69607=CARTESIAN_POINT('Ctrl Pts',(30.0000000000004,-1.17524047358085,27.5625));
#69608=CARTESIAN_POINT('Ctrl Pts',(30.,-1.17524047358085,27.5));
#69609=CARTESIAN_POINT('Ctrl Pts',(30.0764884643488,-1.17524047358085,27.5046969786688));
#69610=CARTESIAN_POINT('Ctrl Pts',(30.1529528341161,-1.16777574296381,27.5096571303415));
#69611=CARTESIAN_POINT('Ctrl Pts',(30.3817494239676,-1.12246086122216,27.5253135785994));
#69612=CARTESIAN_POINT('Ctrl Pts',(30.5275514222186,-1.06175746883915,27.5364191022575));
#69613=CARTESIAN_POINT('Ctrl Pts',(30.7819194324173,-0.890185564641921,
27.5581221152238));
#69614=CARTESIAN_POINT('Ctrl Pts',(30.8893748791333,-0.782854361740771,
27.5685259964847));
#69615=CARTESIAN_POINT('Ctrl Pts',(31.0605234375151,-0.529653947481304,
27.5880127322271));
#69616=CARTESIAN_POINT('Ctrl Pts',(31.1210989339899,-0.385229961573254,
27.5976843165126));
#69617=CARTESIAN_POINT('Ctrl Pts',(31.1825194576632,-0.0817855747122669,
27.6192007914867));
#69618=CARTESIAN_POINT('Ctrl Pts',(31.1830228429167,0.0741472759213479,
27.63025759604));
#69619=CARTESIAN_POINT('Ctrl Pts',(31.1247432077576,0.371953492117145,27.6513742825742));
#69620=CARTESIAN_POINT('Ctrl Pts',(31.0685868115923,0.511361040320207,27.6608435628079));
#69621=CARTESIAN_POINT('Ctrl Pts',(30.9034614818395,0.767636822344003,27.6800694593713));
#69622=CARTESIAN_POINT('Ctrl Pts',(30.7937668420839,0.880579083554765,27.6908097772536));
#69623=CARTESIAN_POINT('Ctrl Pts',(30.5394580202052,1.05521084982092,27.712617639148));
#69624=CARTESIAN_POINT('Ctrl Pts',(30.3979930311562,1.11628678065312,27.7234700450399));
#69625=CARTESIAN_POINT('Ctrl Pts',(30.102283661711,1.18033932531086,27.7438997716137));
#69626=CARTESIAN_POINT('Ctrl Pts',(29.9510987894339,1.18375239925559,27.752701130013));
#69627=CARTESIAN_POINT('Ctrl Pts',(29.6486955420892,1.13241772430468,27.7730910160496));
#69628=CARTESIAN_POINT('Ctrl Pts',(29.5009111395855,1.07549105438516,27.7841843756164));
#69629=CARTESIAN_POINT('Ctrl Pts',(29.2414417758967,0.910237971539166,27.8059766250036));
#69630=CARTESIAN_POINT('Ctrl Pts',(29.1309679987517,0.805447516109976,27.8164757759223));
#69631=CARTESIAN_POINT('Ctrl Pts',(28.9539689931679,0.557381504423619,27.8361397402596));
#69632=CARTESIAN_POINT('Ctrl Pts',(28.8900701663349,0.415841482478183,27.8455137308899));
#69633=CARTESIAN_POINT('Ctrl Pts',(28.8202010476643,0.115104610378523,27.8668382228314));
#69634=CARTESIAN_POINT('Ctrl Pts',(28.8153164753922,-0.0411926086217122,
27.8779208638252));
#69635=CARTESIAN_POINT('Ctrl Pts',(28.8654961586475,-0.341119160610214,
27.8991878980145));
#69636=CARTESIAN_POINT('Ctrl Pts',(28.9179176762722,-0.482198917057609,
27.9089809285524));
#69637=CARTESIAN_POINT('Ctrl Pts',(29.0761417927703,-0.742958176446737,
27.9279419936907));
#69638=CARTESIAN_POINT('Ctrl Pts',(29.1827253034037,-0.858799901268264,
27.938594061191));
#69639=CARTESIAN_POINT('Ctrl Pts',(29.4325136093474,-1.04046451212148,27.9603736693398));
#69640=CARTESIAN_POINT('Ctrl Pts',(29.5726776549044,-1.10544579696665,27.9712846467122));
#69641=CARTESIAN_POINT('Ctrl Pts',(29.8127786384444,-1.16404144712018,27.9881061243607));
#69642=CARTESIAN_POINT('Ctrl Pts',(29.9063068575872,-1.17524047358087,27.9942465220726));
#69643=CARTESIAN_POINT('Ctrl Pts',(30.0000000000002,-1.17524047358085,28.));
#69644=CARTESIAN_POINT('Origin',(30.,-1.21864324187371E-14,15.78125));
#69645=CARTESIAN_POINT('',(30.,-1.17524047358085,28.5625));
#69646=CARTESIAN_POINT('',(30.0000000000002,-1.17524047358085,28.5));
#69647=CARTESIAN_POINT('',(30.,-1.17524047358085,15.78125));
#69648=CARTESIAN_POINT('Ctrl Pts',(29.9999999999999,-1.17524047358085,28.5625));
#69649=CARTESIAN_POINT('Ctrl Pts',(29.9854755687231,-1.17524047358085,28.5616080884619));
#69650=CARTESIAN_POINT('Ctrl Pts',(29.9709414772303,-1.17497122100143,28.5607060377023));
#69651=CARTESIAN_POINT('Ctrl Pts',(29.8064818821414,-1.16886648226933,28.5503905207309));
#69652=CARTESIAN_POINT('Ctrl Pts',(29.6590422242683,-1.13464684706092,28.5401233803667));
#69653=CARTESIAN_POINT('Ctrl Pts',(29.3797071247853,-1.01029888540339,28.5185614617647));
#69654=CARTESIAN_POINT('Ctrl Pts',(29.251363124374,-0.919248746833339,28.507452087585));
#69655=CARTESIAN_POINT('Ctrl Pts',(29.0406130665321,-0.695506305973089,
28.486577911123));
#69656=CARTESIAN_POINT('Ctrl Pts',(28.9590502383724,-0.56619133070644,28.4776471970656));
#69657=CARTESIAN_POINT('Ctrl Pts',(28.8493945968077,-0.283424288620792,
28.4575969003786));
#69658=CARTESIAN_POINT('Ctrl Pts',(28.8224557263032,-0.132654402250458,
28.4469061885797));
#69659=CARTESIAN_POINT('Ctrl Pts',(28.8274401393345,0.174951078681269,28.4250946609358));
#69660=CARTESIAN_POINT('Ctrl Pts',(28.8609710566448,0.328840848056597,28.4141827261138));
#69661=CARTESIAN_POINT('Ctrl Pts',(28.9834218096268,0.608264397886715,28.394369508017));
#69662=CARTESIAN_POINT('Ctrl Pts',(29.0686800279675,0.732167484395331,28.3853987862865));
#69663=CARTESIAN_POINT('Ctrl Pts',(29.2841654510491,0.944633593842617,28.3646336101487));
#69664=CARTESIAN_POINT('Ctrl Pts',(29.4135237499535,1.0299476859008,28.3536653145426));
#69665=CARTESIAN_POINT('Ctrl Pts',(29.6999884026637,1.14695518646917,28.3319258334386));
#69666=CARTESIAN_POINT('Ctrl Pts',(29.8545850153065,1.1765676391467,28.321476648926));
#69667=CARTESIAN_POINT('Ctrl Pts',(30.1599574738008,1.17387642238167,28.3026290229131));
#69668=CARTESIAN_POINT('Ctrl Pts',(30.3078958483554,1.14400535727984,28.2924854305785));
#69669=CARTESIAN_POINT('Ctrl Pts',(30.5899420117525,1.02824734362325,28.2710615776053));
#69670=CARTESIAN_POINT('Ctrl Pts',(30.7205565666579,0.941343746526345,28.2599597843468));
#69671=CARTESIAN_POINT('Ctrl Pts',(30.9384441962492,0.723734320112842,28.2388647444883));
#69672=CARTESIAN_POINT('Ctrl Pts',(31.0243441752868,0.5959705376245,28.2297587654061));
#69673=CARTESIAN_POINT('Ctrl Pts',(31.1420857275796,0.315809924237744,28.2098932839944));
#69674=CARTESIAN_POINT('Ctrl Pts',(31.1732121728651,0.166290213222924,28.1992912189719));
#69675=CARTESIAN_POINT('Ctrl Pts',(31.1771534741222,-0.14225217236566,28.1774132577855));
#69676=CARTESIAN_POINT('Ctrl Pts',(31.1475738082276,-0.298357527790664,
28.1663442213532));
#69677=CARTESIAN_POINT('Ctrl Pts',(31.0316967203975,-0.582326286717529,
28.1462087139606));
#69678=CARTESIAN_POINT('Ctrl Pts',(30.9494361151523,-0.708574806833004,
28.1373477050794));
#69679=CARTESIAN_POINT('Ctrl Pts',(30.7393766183288,-0.926260402286338,
28.1167306721673));
#69680=CARTESIAN_POINT('Ctrl Pts',(30.6125440370362,-1.01460273603848,28.1058101125197));
#69681=CARTESIAN_POINT('Ctrl Pts',(30.3296673321613,-1.13876808424026,28.0840371864985));
#69682=CARTESIAN_POINT('Ctrl Pts',(30.1758968644013,-1.17241612952657,28.0734015508245));
#69683=CARTESIAN_POINT('Ctrl Pts',(30.0133354780172,-1.17518374723503,28.0633209118452));
#69684=CARTESIAN_POINT('Ctrl Pts',(30.0066666906193,-1.17524047358085,28.0629093859629));
#69685=CARTESIAN_POINT('Ctrl Pts',(30.,-1.17524047358085,28.0625));
#69686=CARTESIAN_POINT('Ctrl Pts',(30.0000000000002,-1.17524047358085,28.));
#69687=CARTESIAN_POINT('Ctrl Pts',(30.055120011526,-1.17524047358084,28.0033847916881));
#69688=CARTESIAN_POINT('Ctrl Pts',(30.1102800819057,-1.17136342893539,28.0069094990185));
#69689=CARTESIAN_POINT('Ctrl Pts',(30.320778299587,-1.14149919825233,28.0208945034877));
#69690=CARTESIAN_POINT('Ctrl Pts',(30.4704399584402,-1.08838822567003,28.0319678602702));
#69691=CARTESIAN_POINT('Ctrl Pts',(30.7348284172129,-0.929562358310031,
28.0538343110362));
#69692=CARTESIAN_POINT('Ctrl Pts',(30.8482436418564,-0.827380507129033,
28.0644216046344));
#69693=CARTESIAN_POINT('Ctrl Pts',(31.0309964109232,-0.58443378950115,28.0842573960977));
#69694=CARTESIAN_POINT('Ctrl Pts',(31.0981318171314,-0.445680080400429,
28.0933979512832));
#69695=CARTESIAN_POINT('Ctrl Pts',(31.1762201438822,-0.147691887981632,
28.1145275412917));
#69696=CARTESIAN_POINT('Ctrl Pts',(31.1854211354334,0.00884554012676132,
28.1256272149066));
#69697=CARTESIAN_POINT('Ctrl Pts',(31.1432517249665,0.310649796547867,28.1470273923742));
#69698=CARTESIAN_POINT('Ctrl Pts',(31.0945166442476,0.453415390384783,28.1571505400084));
#69699=CARTESIAN_POINT('Ctrl Pts',(30.9430034157352,0.718468313966014,28.1759447732979));
#69700=CARTESIAN_POINT('Ctrl Pts',(30.8395316819024,0.837077300041102,28.1864571641064));
#69701=CARTESIAN_POINT('Ctrl Pts',(30.594175126874,1.02551549499305,28.2082047776097));
#69702=CARTESIAN_POINT('Ctrl Pts',(30.4553685567187,1.0942445153416,28.2191652668043));
#69703=CARTESIAN_POINT('Ctrl Pts',(30.1633070228503,1.17335763356101,28.2399049418951));
#69704=CARTESIAN_POINT('Ctrl Pts',(30.0132854694265,1.18458952272981,28.2488527114972));
#69705=CARTESIAN_POINT('Ctrl Pts',(29.7101813599922,1.14957783235101,28.2687069250423));
#69706=CARTESIAN_POINT('Ctrl Pts',(29.5603537745588,1.10100720474222,28.2796294987935));
#69707=CARTESIAN_POINT('Ctrl Pts',(29.2921855827035,0.950361389094781,28.3014380407736));
#69708=CARTESIAN_POINT('Ctrl Pts',(29.1755651130251,0.851181456436058,28.3121157317836));
#69709=CARTESIAN_POINT('Ctrl Pts',(28.9864685212412,0.613960284958293,28.3321380906356));
#69710=CARTESIAN_POINT('Ctrl Pts',(28.9157930252681,0.478217809624506,28.341090783094));
#69711=CARTESIAN_POINT('Ctrl Pts',(28.8287462552022,0.18335177826131,28.3619989885486));
#69712=CARTESIAN_POINT('Ctrl Pts',(28.8147855892159,0.0266848358587583,
28.3731078456949));
#69713=CARTESIAN_POINT('Ctrl Pts',(28.8481057813277,-0.277120858900621,
28.3946499400995));
#69714=CARTESIAN_POINT('Ctrl Pts',(28.8928044130046,-0.421659697790202,
28.4048988240612));
#69715=CARTESIAN_POINT('Ctrl Pts',(29.0376019293491,-0.692609521363159,
28.4241111916336));
#69716=CARTESIAN_POINT('Ctrl Pts',(29.1388311172626,-0.815074867447836,
28.4343484054768));
#69717=CARTESIAN_POINT('Ctrl Pts',(29.3808301647318,-1.01067727789171,28.456143840463));
#69718=CARTESIAN_POINT('Ctrl Pts',(29.5182554521743,-1.08294295653866,28.4671448960526));
#69719=CARTESIAN_POINT('Ctrl Pts',(29.7744135979937,-1.15894806924162,28.4855696371912));
#69720=CARTESIAN_POINT('Ctrl Pts',(29.8869899356779,-1.1752404735809,28.493060314833));
#69721=CARTESIAN_POINT('Ctrl Pts',(30.0000000000005,-1.17524047358085,28.5));
#69722=CARTESIAN_POINT('Origin',(30.,-1.21864324187371E-14,15.78125));
#69723=CARTESIAN_POINT('',(29.9999999999997,-1.17524047358085,29.0625));
#69724=CARTESIAN_POINT('',(30.,-1.17524047358085,29.));
#69725=CARTESIAN_POINT('',(30.,-1.17524047358085,15.78125));
#69726=CARTESIAN_POINT('Ctrl Pts',(29.9999999999995,-1.17524047358085,29.0625));
#69727=CARTESIAN_POINT('Ctrl Pts',(29.9663313283337,-1.17524047358085,29.0604324851927));
#69728=CARTESIAN_POINT('Ctrl Pts',(29.9326266255446,-1.17379373293774,29.0583114654359));
#69729=CARTESIAN_POINT('Ctrl Pts',(29.7487805300534,-1.15793171143038,29.046459536434));
#69730=CARTESIAN_POINT('Ctrl Pts',(29.6025054140808,-1.11619705168394,29.0359974721754));
#69731=CARTESIAN_POINT('Ctrl Pts',(29.3284713606868,-0.977122112422326,
29.0142389520917));
#69732=CARTESIAN_POINT('Ctrl Pts',(29.204360853848,-0.879027723836093,29.003139801917));
#69733=CARTESIAN_POINT('Ctrl Pts',(29.0061078341151,-0.644908297203287,
28.9826651365702));
#69734=CARTESIAN_POINT('Ctrl Pts',(28.9319567448549,-0.512847810431858,
28.9738647427883));
#69735=CARTESIAN_POINT('Ctrl Pts',(28.8365844224207,-0.225635628236165,
28.9534992524445));
#69736=CARTESIAN_POINT('Ctrl Pts',(28.8171575566038,-0.0729412609821712,
28.9426720805673));
#69737=CARTESIAN_POINT('Ctrl Pts',(28.8379321785986,0.234707082052963,28.92085751368));
#69738=CARTESIAN_POINT('Ctrl Pts',(28.8792757590782,0.386638085776581,28.9100844699825));
#69739=CARTESIAN_POINT('Ctrl Pts',(29.0157412244589,0.659238101106546,28.8907550914809));
#69740=CARTESIAN_POINT('Ctrl Pts',(29.107096372761,0.778529076561771,28.8813960362208));
#69741=CARTESIAN_POINT('Ctrl Pts',(29.3335481377689,0.980220242371224,28.8603394545531));
#69742=CARTESIAN_POINT('Ctrl Pts',(29.4678337645529,1.05914504636678,28.8492951073424));
#69743=CARTESIAN_POINT('Ctrl Pts',(29.760564366148,1.1610786562004,28.8277052746509));
#69744=CARTESIAN_POINT('Ctrl Pts',(29.9162604257863,1.18253750642917,28.8179009595418));
#69745=CARTESIAN_POINT('Ctrl Pts',(30.2216914945448,1.16389753053477,28.7984842912973));
#69746=CARTESIAN_POINT('Ctrl Pts',(30.3686116386073,1.12601470107769,28.7881191791422));
#69747=CARTESIAN_POINT('Ctrl Pts',(30.645460693513,0.994469364755083,28.7664547489262));
#69748=CARTESIAN_POINT('Ctrl Pts',(30.7717903384927,0.899966183411579,28.7553466483575));
#69749=CARTESIAN_POINT('Ctrl Pts',(30.9764758301347,0.671134004376585,28.7346644325598));
#69750=CARTESIAN_POINT('Ctrl Pts',(31.0544159221586,0.540492245543279,28.7258249398524));
#69751=CARTESIAN_POINT('Ctrl Pts',(31.1571623293156,0.255550540096121,28.7056204432797));
#69752=CARTESIAN_POINT('Ctrl Pts',(31.1804841833933,0.103803871660056,28.6948604703318));
#69753=CARTESIAN_POINT('Ctrl Pts',(31.1678665590545,-0.203924479708025,
28.6730402302557));
#69754=CARTESIAN_POINT('Ctrl Pts',(31.130543099267,-0.356918086122505,28.6621918400855));
#69755=CARTESIAN_POINT('Ctrl Pts',(31.0012937995436,-0.633072694293491,
28.6426104143845));
#69756=CARTESIAN_POINT('Ctrl Pts',(30.9131062008608,-0.754733454165662,
28.6334802730101));
#69757=CARTESIAN_POINT('Ctrl Pts',(30.6923373486102,-0.962047131628042,
28.6125733267459));
#69758=CARTESIAN_POINT('Ctrl Pts',(30.5605741188135,-1.04432722358406,28.6015649165697));
#69759=CARTESIAN_POINT('Ctrl Pts',(30.2834202387706,-1.14942800624881,28.5808193260016));
#69760=CARTESIAN_POINT('Ctrl Pts',(30.1422284632676,-1.17524047358085,28.5712339190787));
#69761=CARTESIAN_POINT('Ctrl Pts',(29.9999999999999,-1.17524047358085,28.5625));
#69762=CARTESIAN_POINT('Ctrl Pts',(30.0000000000005,-1.17524047358085,28.5));
#69763=CARTESIAN_POINT('Ctrl Pts',(30.0354745744302,-1.17524047358084,28.5021784110951));
#69764=CARTESIAN_POINT('Ctrl Pts',(30.070984899228,-1.17363438892678,28.50441595924));
#69765=CARTESIAN_POINT('Ctrl Pts',(30.2617617366305,-1.15628719000694,28.5167461440698));
#69766=CARTESIAN_POINT('Ctrl Pts',(30.4127085422869,-1.11138228847866,28.527607482843));
#69767=CARTESIAN_POINT('Ctrl Pts',(30.6847642885538,-0.967157900388871,
28.5494270868925));
#69768=CARTESIAN_POINT('Ctrl Pts',(30.804005950619,-0.870565283253422,28.5601740092255));
#69769=CARTESIAN_POINT('Ctrl Pts',(30.9983603111577,-0.638155310621775,
28.5803486604476));
#69770=CARTESIAN_POINT('Ctrl Pts',(31.0719538047089,-0.504858427298666,
28.5892017641887));
#69771=CARTESIAN_POINT('Ctrl Pts',(31.1663430846515,-0.212647773407092,
28.6099216835343));
#69772=CARTESIAN_POINT('Ctrl Pts',(31.1842429187448,-0.0559802512603478,
28.6210305817888));
#69773=CARTESIAN_POINT('Ctrl Pts',(31.1582832767207,0.249283949423046,28.6426760951642));
#69774=CARTESIAN_POINT('Ctrl Pts',(31.1169606007789,0.395199803964739,28.6530226198275));
#69775=CARTESIAN_POINT('Ctrl Pts',(30.9790360194058,0.668562290541804,28.6724060632391));
#69776=CARTESIAN_POINT('Ctrl Pts',(30.8818240300007,0.792402281745908,28.6822761930404));
#69777=CARTESIAN_POINT('Ctrl Pts',(30.6459736712074,0.993822232743541,28.7039003049109));
#69778=CARTESIAN_POINT('Ctrl Pts',(30.5101537410361,1.06991069848525,28.7149383113331));
#69779=CARTESIAN_POINT('Ctrl Pts',(30.2218612846042,1.16368326752433,28.7359662684601));
#69780=CARTESIAN_POINT('Ctrl Pts',(30.0727878905027,1.18239624374933,28.7452765661691));
#69781=CARTESIAN_POINT('Ctrl Pts',(29.7685724316717,1.16273575029291,28.764654767797));
#69782=CARTESIAN_POINT('Ctrl Pts',(29.6165255150965,1.12180125661046,28.7754428960271));
#69783=CARTESIAN_POINT('Ctrl Pts',(29.3404632117996,0.984593855919108,28.797259754998));
#69784=CARTESIAN_POINT('Ctrl Pts',(29.2184662863885,0.890859052794272,28.8080745514575));
#69785=CARTESIAN_POINT('Ctrl Pts',(29.0185031029016,0.663646825495766,28.8284093479536));
#69786=CARTESIAN_POINT('Ctrl Pts',(28.9418083423014,0.532910081337728,28.8372126922591));
#69787=CARTESIAN_POINT('Ctrl Pts',(28.8396688119263,0.243593095049782,28.8577274289443));
#69788=CARTESIAN_POINT('Ctrl Pts',(28.8175791014781,0.0870303940346913,
28.8688288945971));
#69789=CARTESIAN_POINT('Ctrl Pts',(28.8356734059559,-0.219589451967425,
28.8905705333577));
#69790=CARTESIAN_POINT('Ctrl Pts',(28.8733703746263,-0.366880393585839,
28.9010145619721));
#69791=CARTESIAN_POINT('Ctrl Pts',(29.0040267448551,-0.642739671975603,
28.9205750465844));
#69792=CARTESIAN_POINT('Ctrl Pts',(29.0970828699605,-0.768007510288218,
28.9301160290222));
#69793=CARTESIAN_POINT('Ctrl Pts',(29.3264450160403,-0.975407631545752,
28.9515537342264));
#69794=CARTESIAN_POINT('Ctrl Pts',(29.4604715589085,-1.05546393671967,28.9626222876417));
#69795=CARTESIAN_POINT('Ctrl Pts',(29.7327334190531,-1.15230702146743,28.9827747043974));
#69796=CARTESIAN_POINT('Ctrl Pts',(29.8659356312532,-1.17524047358086,28.9917674189746));
#69797=CARTESIAN_POINT('Ctrl Pts',(30.0000000000001,-1.17524047358085,29.));
#69798=CARTESIAN_POINT('Origin',(30.,-1.21864324187371E-14,15.78125));
#69799=CARTESIAN_POINT('',(29.9999999999999,-1.17524047358085,29.5625));
#69800=CARTESIAN_POINT('',(30.,-1.17524047358085,29.5));
#69801=CARTESIAN_POINT('',(30.,-1.17524047358085,15.78125));
#69802=CARTESIAN_POINT('Ctrl Pts',(29.9999999999998,-1.17524047358085,29.5625));
#69803=CARTESIAN_POINT('Ctrl Pts',(29.9467973546619,-1.17524047358085,29.5592329493093));
#69804=CARTESIAN_POINT('Ctrl Pts',(29.8935499193759,-1.17162840400865,29.5558350868076));
#69805=CARTESIAN_POINT('Ctrl Pts',(29.6905156464705,-1.14383638937277,29.5423818936273));
#69806=CARTESIAN_POINT('Ctrl Pts',(29.5458229652857,-1.09446322181842,29.531746189361));
#69807=CARTESIAN_POINT('Ctrl Pts',(29.2779882672223,-0.940574047774209,
29.5098431372833));
#69808=CARTESIAN_POINT('Ctrl Pts',(29.1585890601641,-0.835479489994527,
29.4987851149112));
#69809=CARTESIAN_POINT('Ctrl Pts',(28.9732889450876,-0.591037021395749,
29.4787398668936));
#69810=CARTESIAN_POINT('Ctrl Pts',(28.9066211123554,-0.456058910232785,
29.4698379853235));
#69811=CARTESIAN_POINT('Ctrl Pts',(28.8262612459225,-0.164388119091858,
29.4491563462818));
#69812=CARTESIAN_POINT('Ctrl Pts',(28.8148509180816,-0.0100732314283097,
29.4382142673958));
#69813=CARTESIAN_POINT('Ctrl Pts',(28.852213214805,0.296739305134607,29.4164589654342));
#69814=CARTESIAN_POINT('Ctrl Pts',(28.9016274703356,0.446176311860775,29.405862764764));
#69815=CARTESIAN_POINT('Ctrl Pts',(29.0526565417776,0.711342976877612,29.3870604663565));
#69816=CARTESIAN_POINT('Ctrl Pts',(29.1506118786123,0.825870653466757,29.3770454144149));
#69817=CARTESIAN_POINT('Ctrl Pts',(29.3887681357508,1.01569990993121,29.3556906361267));
#69818=CARTESIAN_POINT('Ctrl Pts',(29.5280199399709,1.08742345397384,29.3445966390884));
#69819=CARTESIAN_POINT('Ctrl Pts',(29.8244665773462,1.17210985589585,29.3233900912571));
#69820=CARTESIAN_POINT('Ctrl Pts',(29.9785058773413,1.18498177307898,29.3141652695437));
#69821=CARTESIAN_POINT('Ctrl Pts',(30.2808965556073,1.15114217787766,29.2943964213012));
#69822=CARTESIAN_POINT('Ctrl Pts',(30.4264177470889,1.1055232193301,29.2838429408837));
#69823=CARTESIAN_POINT('Ctrl Pts',(30.697402601783,0.95889535591386,29.2620038856125));
#69824=CARTESIAN_POINT('Ctrl Pts',(30.819169348162,0.85722095894767,29.2509217356401));
#69825=CARTESIAN_POINT('Ctrl Pts',(31.0108714255578,0.617827319896978,29.2306623578836));
#69826=CARTESIAN_POINT('Ctrl Pts',(31.0812140757987,0.48430476852144,29.221840827786));
#69827=CARTESIAN_POINT('Ctrl Pts',(31.1690224491511,0.194817477900372,29.2013140152506));
#69828=CARTESIAN_POINT('Ctrl Pts',(31.1844226308274,0.0412543787619307,
29.1904252437899));
#69829=CARTESIAN_POINT('Ctrl Pts',(31.1552826086302,-0.266085347349785,
29.1686325601491));
#69830=CARTESIAN_POINT('Ctrl Pts',(31.1098513200658,-0.416814367038074,
29.1579447461033));
#69831=CARTESIAN_POINT('Ctrl Pts',(30.9660264712179,-0.685700945491834,
29.1388786780306));
#69832=CARTESIAN_POINT('Ctrl Pts',(30.8713728192914,-0.802582950873403,
29.1292210796557));
#69833=CARTESIAN_POINT('Ctrl Pts',(30.6390456070483,-0.99836896334456,29.1080130601942));
#69834=CARTESIAN_POINT('Ctrl Pts',(30.5022270643229,-1.07372697770931,29.0969396285291));
#69835=CARTESIAN_POINT('Ctrl Pts',(30.2397868247199,-1.15682002769535,29.0778778247601));
#69836=CARTESIAN_POINT('Ctrl Pts',(30.1201628836901,-1.17524047358085,29.0698789231656));
#69837=CARTESIAN_POINT('Ctrl Pts',(29.9999999999995,-1.17524047358085,29.0625));
#69838=CARTESIAN_POINT('Ctrl Pts',(30.0000000000001,-1.17524047358085,29.));
#69839=CARTESIAN_POINT('Ctrl Pts',(30.0146960045521,-1.17524047358085,29.0009024474538));
#69840=CARTESIAN_POINT('Ctrl Pts',(30.0294011894743,-1.17496482224357,29.0018152315228));
#69841=CARTESIAN_POINT('Ctrl Pts',(30.199932441124,-1.16856010735523,29.0125142300756));
#69842=CARTESIAN_POINT('Ctrl Pts',(30.353002562887,-1.13175546267305,29.0232187723758));
#69843=CARTESIAN_POINT('Ctrl Pts',(30.6330116689674,-1.00191414666784,29.0450168400954));
#69844=CARTESIAN_POINT('Ctrl Pts',(30.7577840016447,-0.911212372347243,
29.0558945356534));
#69845=CARTESIAN_POINT('Ctrl Pts',(30.9634990803743,-0.689398439003151,
29.0763911529622));
#69846=CARTESIAN_POINT('Ctrl Pts',(31.0433641152287,-0.561238966842274,
29.0852039625465));
#69847=CARTESIAN_POINT('Ctrl Pts',(31.1533625468904,-0.274946500315461,
29.1055042381753));
#69848=CARTESIAN_POINT('Ctrl Pts',(31.1797284184379,-0.118602529514694,
29.1165901942211));
#69849=CARTESIAN_POINT('Ctrl Pts',(31.1696998210424,0.189193535485508,29.1384152356998));
#69850=CARTESIAN_POINT('Ctrl Pts',(31.1357401287962,0.337792934955289,29.1489520437553));
#69851=CARTESIAN_POINT('Ctrl Pts',(31.0124667812232,0.616132121424454,29.1686883723852));
#69852=CARTESIAN_POINT('Ctrl Pts',(30.9235367823029,0.742831293967475,29.1779572331897));
#69853=CARTESIAN_POINT('Ctrl Pts',(30.7007442503466,0.956131495282673,29.1992006935594));
#69854=CARTESIAN_POINT('Ctrl Pts',(30.5686344749746,1.04013508390185,29.2102914886907));
#69855=CARTESIAN_POINT('Ctrl Pts',(30.2847340927663,1.14996876391647,29.231619165161));
#69856=CARTESIAN_POINT('Ctrl Pts',(30.1365034722987,1.17678287240203,29.241562955497));
#69857=CARTESIAN_POINT('Ctrl Pts',(29.8314130542368,1.17348866622216,29.2604146402912));
#69858=CARTESIAN_POINT('Ctrl Pts',(29.6774432972388,1.14080144691636,29.271028448982));
#69859=CARTESIAN_POINT('Ctrl Pts',(29.3937190869037,1.01837161158084,29.2927918879254));
#69860=CARTESIAN_POINT('Ctrl Pts',(29.2662697773694,0.930754504522398,29.3037246074232));
#69861=CARTESIAN_POINT('Ctrl Pts',(29.0548960664095,0.714326580132712,29.3243777540292));
#69862=CARTESIAN_POINT('Ctrl Pts',(28.9719101496403,0.588650269969742,29.3332602962825));
#69863=CARTESIAN_POINT('Ctrl Pts',(28.8542643011592,0.305390771595589,29.3533455118009));
#69864=CARTESIAN_POINT('Ctrl Pts',(28.8237155837947,0.14936986715794,29.3644085600269));
#69865=CARTESIAN_POINT('Ctrl Pts',(28.8258171170069,-0.159374372506235,
29.386300834176));
#69866=CARTESIAN_POINT('Ctrl Pts',(28.8560851449643,-0.309160959864127,
29.3969218227258));
#69867=CARTESIAN_POINT('Ctrl Pts',(28.9721608102066,-0.589863983624277,
29.416825765087));
#69868=CARTESIAN_POINT('Ctrl Pts',(29.0571584178456,-0.717947603677171,
29.4258895505263));
#69869=CARTESIAN_POINT('Ctrl Pts',(29.2735722711375,-0.936836489269234,
29.4469394508198));
#69870=CARTESIAN_POINT('Ctrl Pts',(29.4037270862843,-1.02460346918986,29.4580436226767));
#69871=CARTESIAN_POINT('Ctrl Pts',(29.6852328519168,-1.14214540943397,29.4794975379443));
#69872=CARTESIAN_POINT('Ctrl Pts',(29.8330783756557,-1.1729174993834,29.4896673732243));
#69873=CARTESIAN_POINT('Ctrl Pts',(29.9885051427478,-1.17519832475183,29.4992926332218));
#69874=CARTESIAN_POINT('Ctrl Pts',(29.9942534046712,-1.17524047358085,29.4996471149485));
#69875=CARTESIAN_POINT('Ctrl Pts',(30.,-1.17524047358085,29.5));
#69876=CARTESIAN_POINT('Origin',(30.,-1.21864324187371E-14,15.78125));
#69877=CARTESIAN_POINT('',(30.,-1.17524047358085,30.0625));
#69878=CARTESIAN_POINT('',(29.9999999999998,-1.17524047358085,29.9999999999999));
#69879=CARTESIAN_POINT('',(30.,-1.17524047358085,15.78125));
#69880=CARTESIAN_POINT('Ctrl Pts',(30.,-1.17524047358085,30.0625));
#69881=CARTESIAN_POINT('Ctrl Pts',(29.9263916760993,-1.17524047358085,30.0579798840563));
#69882=CARTESIAN_POINT('Ctrl Pts',(29.8527927358329,-1.1683271801588,30.0532152422529));
#69883=CARTESIAN_POINT('Ctrl Pts',(29.6305589174408,-1.12600740432272,30.0380679862212));
#69884=CARTESIAN_POINT('Ctrl Pts',(29.4879403212856,-1.06872004039491,30.0272790588551));
#69885=CARTESIAN_POINT('Ctrl Pts',(29.229459906818,-0.900978381114361,30.0054593092048));
#69886=CARTESIAN_POINT('Ctrl Pts',(29.1168411945232,-0.790914788798306,
29.9946414903997));
#69887=CARTESIAN_POINT('Ctrl Pts',(28.9451007627829,-0.539025681180781,
29.975164899812));
#69888=CARTESIAN_POINT('Ctrl Pts',(28.885353566283,-0.401177024850609,29.9659464494622));
#69889=CARTESIAN_POINT('Ctrl Pts',(28.8194073352897,-0.10544306552401,29.944976701428));
#69890=CARTESIAN_POINT('Ctrl Pts',(28.8157651951869,0.0500317181756064,
29.9339523772439));
#69891=CARTESIAN_POINT('Ctrl Pts',(28.8690807484143,0.355959077177534,29.9122598409872));
#69892=CARTESIAN_POINT('Ctrl Pts',(28.9264649062036,0.503164977506288,29.9022508807468));
#69893=CARTESIAN_POINT('Ctrl Pts',(29.0920593097175,0.761174070029624,29.8829347271204));
#69894=CARTESIAN_POINT('Ctrl Pts',(29.1966290016669,0.870813111888444,29.8726262318314));
#69895=CARTESIAN_POINT('Ctrl Pts',(29.4460717811045,1.04817985046692,29.851020217295));
#69896=CARTESIAN_POINT('Ctrl Pts',(29.5899284156368,1.11237046788542,29.8399105187383));
#69897=CARTESIAN_POINT('Ctrl Pts',(29.8896511606184,1.17977836078127,29.8191153804746));
#69898=CARTESIAN_POINT('Ctrl Pts',(30.042143785172,1.18417711729498,29.810228885603));
#69899=CARTESIAN_POINT('Ctrl Pts',(30.3412103985985,1.13483145488925,29.7901144124214));
#69900=CARTESIAN_POINT('Ctrl Pts',(30.484863334991,1.08127741540018,29.7793943289302));
#69901=CARTESIAN_POINT('Ctrl Pts',(30.7472520600478,0.920389087318013,29.7575775552199));
#69902=CARTESIAN_POINT('Ctrl Pts',(30.8626628342488,0.813224513564577,29.7466910634298));
#69903=CARTESIAN_POINT('Ctrl Pts',(31.0408533066038,0.565701034414209,29.7269731686955));
#69904=CARTESIAN_POINT('Ctrl Pts',(31.1041185100332,0.42933329828376,29.7179429396888));
#69905=CARTESIAN_POINT('Ctrl Pts',(31.1774532864279,0.13565521801398,29.6971189688454));
#69906=CARTESIAN_POINT('Ctrl Pts',(31.185083485025,-0.0192736961984122,
29.6861333508878));
#69907=CARTESIAN_POINT('Ctrl Pts',(31.1399640096901,-0.325574493297471,
29.6644143350789));
#69908=CARTESIAN_POINT('Ctrl Pts',(31.0867572532099,-0.473736864086508,
29.654106159393));
#69909=CARTESIAN_POINT('Ctrl Pts',(30.9288924580137,-0.735375844574816,
29.6351359699395));
#69910=CARTESIAN_POINT('Ctrl Pts',(30.827743660758,-0.847605887956935,29.6249456831495));
#69911=CARTESIAN_POINT('Ctrl Pts',(30.5841967794232,-1.03154789843284,29.6034686040399));
#69912=CARTESIAN_POINT('Ctrl Pts',(30.4427060183441,-1.0997249484081,29.5923628543371));
#69913=CARTESIAN_POINT('Ctrl Pts',(30.1964052482032,-1.16291170221409,29.5749978904338));
#69914=CARTESIAN_POINT('Ctrl Pts',(30.0983061450535,-1.17524047358085,29.5685367516888));
#69915=CARTESIAN_POINT('Ctrl Pts',(29.9999999999998,-1.17524047358085,29.5625));
#69916=CARTESIAN_POINT('Ctrl Pts',(30.,-1.17524047358085,29.5));
#69917=CARTESIAN_POINT('Ctrl Pts',(30.1499565209686,-1.17524047358085,29.5092084811251));
#69918=CARTESIAN_POINT('Ctrl Pts',(30.2986551183888,-1.14654165825818,29.5193571963421));
#69919=CARTESIAN_POINT('Ctrl Pts',(30.5805418737435,-1.03331719508937,29.5406814366056));
#69920=CARTESIAN_POINT('Ctrl Pts',(30.7104602238272,-0.948696043146186,
29.5516595563353));
#69921=CARTESIAN_POINT('Ctrl Pts',(30.9271652336418,-0.73741304903825,29.5724576785973));
#69922=CARTESIAN_POINT('Ctrl Pts',(31.0130985609625,-0.614031092469691,
29.5814606062707));
#69923=CARTESIAN_POINT('Ctrl Pts',(31.1371264539894,-0.335358891062759,
29.6012205481486));
#69924=CARTESIAN_POINT('Ctrl Pts',(31.1715373282526,-0.181667965902616,
29.6121183834297));
#69925=CARTESIAN_POINT('Ctrl Pts',(31.1782875351469,0.125982959094587,29.6339331333974));
#69926=CARTESIAN_POINT('Ctrl Pts',(31.1521830035108,0.27698654047903,29.6446404159195));
#69927=CARTESIAN_POINT('Ctrl Pts',(31.0441268483734,0.560261316579686,29.6647267147429));
#69928=CARTESIAN_POINT('Ctrl Pts',(30.9634093757068,0.689883113720223,29.6736315391227));
#69929=CARTESIAN_POINT('Ctrl Pts',(30.7540662315648,0.914815989860588,29.6944615256665));
#69930=CARTESIAN_POINT('Ctrl Pts',(30.6261826944801,1.0066730037076,29.7055712306082));
#69931=CARTESIAN_POINT('Ctrl Pts',(30.3474095969538,1.1326991331979,29.7271581352984));
#69932=CARTESIAN_POINT('Ctrl Pts',(30.2000827038505,1.16777128079541,29.7374485757904));
#69933=CARTESIAN_POINT('Ctrl Pts',(29.8935937537322,1.18085135992657,29.7567330869508));
#69934=CARTESIAN_POINT('Ctrl Pts',(29.7372662628443,1.15617395643532,29.7668098469142));
#69935=CARTESIAN_POINT('Ctrl Pts',(29.4460305983855,1.04785975410839,29.7885340948419));
#69936=CARTESIAN_POINT('Ctrl Pts',(29.3136703421255,0.966357190577468,29.7995516007362));
#69937=CARTESIAN_POINT('Ctrl Pts',(29.091570241583,0.760352988788506,29.8204938700552));
#69938=CARTESIAN_POINT('Ctrl Pts',(29.0026423680915,0.639251124272773,29.8296723175212));
#69939=CARTESIAN_POINT('Ctrl Pts',(28.8716938065568,0.363925746310141,29.8491949446027));
#69940=CARTESIAN_POINT('Ctrl Pts',(28.8334229675251,0.211172023558316,29.8600263252283));
#69941=CARTESIAN_POINT('Ctrl Pts',(28.8188892259004,-0.0965571382164996,
29.8818466227683));
#69942=CARTESIAN_POINT('Ctrl Pts',(28.8412989000486,-0.248535346834791,
29.8926230136456));
#69943=CARTESIAN_POINT('Ctrl Pts',(28.942312504556,-0.5340148591211,29.9128656447428));
#69944=CARTESIAN_POINT('Ctrl Pts',(29.0193556498266,-0.664990211735325,
29.9216906330323));
#69945=CARTESIAN_POINT('Ctrl Pts',(29.2225255933627,-0.895077676800941,
29.9423242871271));
#69946=CARTESIAN_POINT('Ctrl Pts',(29.3483400060408,-0.990433515042349,
29.9534309783521));
#69947=CARTESIAN_POINT('Ctrl Pts',(29.6245422330139,-1.1237624473258,29.9751189235115));
#69948=CARTESIAN_POINT('Ctrl Pts',(29.7713190573348,-1.16255586776877,29.985507518588));
#69949=CARTESIAN_POINT('Ctrl Pts',(29.9476315409713,-1.1743662864253,29.9967531815485));
#69950=CARTESIAN_POINT('Ctrl Pts',(29.9738286104226,-1.17524047358085,29.9983928758457));
#69951=CARTESIAN_POINT('Ctrl Pts',(29.9999999999996,-1.17524047358085,29.9999999999999));
#69952=CARTESIAN_POINT('Origin',(30.,-1.21864324187371E-14,15.78125));
#69953=CARTESIAN_POINT('',(30.,-1.17524047358085,30.5625));
#69954=CARTESIAN_POINT('',(29.9999999999998,-1.17524047358085,30.4999999999999));
#69955=CARTESIAN_POINT('',(30.,-1.17524047358085,15.78125));
#69956=CARTESIAN_POINT('Ctrl Pts',(29.9999999999999,-1.17524047358085,30.5625));
#69957=CARTESIAN_POINT('Ctrl Pts',(29.87859718881,-1.17524047358085,30.555044935771));
#69958=CARTESIAN_POINT('Ctrl Pts',(29.7578462794256,-1.15643017462348,30.5469630079231));
#69959=CARTESIAN_POINT('Ctrl Pts',(29.5223698659242,-1.08113291221706,30.5298333797947));
#69960=CARTESIAN_POINT('Ctrl Pts',(29.4096002088597,-1.02391620699781,30.5208799114591));
#69961=CARTESIAN_POINT('Ctrl Pts',(29.1820826863431,-0.858187725726655,
30.5010328956616));
#69962=CARTESIAN_POINT('Ctrl Pts',(29.0755864711026,-0.74226695058618,30.4903833861391));
#69963=CARTESIAN_POINT('Ctrl Pts',(28.9175541454242,-0.481384400712606,
30.4714297273205));
#69964=CARTESIAN_POINT('Ctrl Pts',(28.8652363337421,-0.340257481842474,
30.4616267985498));
#69965=CARTESIAN_POINT('Ctrl Pts',(28.815283295232,-0.0402726424447981,
30.4403556313474));
#69966=CARTESIAN_POINT('Ctrl Pts',(28.8202904087434,0.116033016014593,30.4292723919329));
#69967=CARTESIAN_POINT('Ctrl Pts',(28.8903942350679,0.41669295482916,30.4079533551363));
#69968=CARTESIAN_POINT('Ctrl Pts',(28.9543854043788,0.558153128819785,30.3985868124474));
#69969=CARTESIAN_POINT('Ctrl Pts',(29.1315478521803,0.806074678810529,30.3789179332106));
#69970=CARTESIAN_POINT('Ctrl Pts',(29.2421055811419,0.910792536064214,30.3684162008828));
#69971=CARTESIAN_POINT('Ctrl Pts',(29.5017160718709,1.07586594659562,30.3466216552675));
#69972=CARTESIAN_POINT('Ctrl Pts',(29.6495548172672,1.13268560353193,30.3355287526402));
#69973=CARTESIAN_POINT('Ctrl Pts',(29.9519945282947,1.1837871612187,30.3151448923318));
#69974=CARTESIAN_POINT('Ctrl Pts',(30.1031613914609,1.18026105601431,30.3063430973327));
#69975=CARTESIAN_POINT('Ctrl Pts',(30.3988201345177,1.11599305235349,30.2859088407808));
#69976=CARTESIAN_POINT('Ctrl Pts',(30.5402500629299,1.05480717912897,30.2750546900124));
#69977=CARTESIAN_POINT('Ctrl Pts',(30.7944347031296,0.879976451319597,30.2532473998958));
#69978=CARTESIAN_POINT('Ctrl Pts',(30.9040431118398,0.766951615348157,30.2425094496776));
#69979=CARTESIAN_POINT('Ctrl Pts',(31.0689753458081,0.510549117592882,30.223290918131));
#69980=CARTESIAN_POINT('Ctrl Pts',(31.1250271192607,0.371095429137332,30.2138134394961));
#69981=CARTESIAN_POINT('Ctrl Pts',(31.1830815580213,0.0732292938782705,
30.1926925042524));
#69982=CARTESIAN_POINT('Ctrl Pts',(31.1824563525586,-0.0827153416037653,
30.1816348640652));
#69983=CARTESIAN_POINT('Ctrl Pts',(31.1207993480439,-0.386085590380016,
30.1601236460354));
#69984=CARTESIAN_POINT('Ctrl Pts',(31.0601308144882,-0.530428613118422,
30.1504611573687));
#69985=CARTESIAN_POINT('Ctrl Pts',(30.8888193562276,-0.783487027384905,
30.1309694527541));
#69986=CARTESIAN_POINT('Ctrl Pts',(30.7812795445953,-0.890749011015136,
30.1205628449218));
#69987=CARTESIAN_POINT('Ctrl Pts',(30.5267682373962,-1.06214794901788,30.0988571647179));
#69988=CARTESIAN_POINT('Ctrl Pts',(30.3809100882996,-1.12274761000244,30.0877518706328));
#69989=CARTESIAN_POINT('Ctrl Pts',(30.1523604876879,-1.16783357423751,30.0721187053907));
#69990=CARTESIAN_POINT('Ctrl Pts',(30.0761915030069,-1.17524047358085,30.0671787429637));
#69991=CARTESIAN_POINT('Ctrl Pts',(30.,-1.17524047358085,30.0625));
#69992=CARTESIAN_POINT('Ctrl Pts',(29.9999999999996,-1.17524047358085,29.9999999999999));
#69993=CARTESIAN_POINT('Ctrl Pts',(30.1287289986958,-1.17524047358085,30.0079049483617));
#69994=CARTESIAN_POINT('Ctrl Pts',(30.2567455299606,-1.1540988796436,30.0165156942669));
#69995=CARTESIAN_POINT('Ctrl Pts',(30.5250941977629,-1.06268366593765,30.0362353726713));
#69996=CARTESIAN_POINT('Ctrl Pts',(30.659989580509,-0.984598569323181,30.0472873928126));
#69997=CARTESIAN_POINT('Ctrl Pts',(30.8878392789542,-0.78430373476697,30.0683803131598));
#69998=CARTESIAN_POINT('Ctrl Pts',(30.9799768519055,-0.665589512740196,
30.0778047289255));
#69999=CARTESIAN_POINT('Ctrl Pts',(31.1182025022512,-0.393869611947964,
30.0970717007283));
#70000=CARTESIAN_POINT('Ctrl Pts',(31.16052513775,-0.242215229337512,30.1078251299214));
#70001=CARTESIAN_POINT('Ctrl Pts',(31.183296750852,0.0653802899747305,30.1296359512119));
#70002=CARTESIAN_POINT('Ctrl Pts',(31.1648281646971,0.218291541355271,30.1404785017947));
#70003=CARTESIAN_POINT('Ctrl Pts',(31.0712608350547,0.506051914399227,30.1608828629668));
#70004=CARTESIAN_POINT('Ctrl Pts',(30.9980258995704,0.638460005209143,30.1696826775517));
#70005=CARTESIAN_POINT('Ctrl Pts',(30.8013405043472,0.873851821952036,30.1901061897083));
#70006=CARTESIAN_POINT('Ctrl Pts',(30.6777833777517,0.972810187954768,30.2012019893176));
#70007=CARTESIAN_POINT('Ctrl Pts',(30.4044625790663,1.11370354858798,30.222981179922));
#70008=CARTESIAN_POINT('Ctrl Pts',(30.2583590845709,1.15637148267232,30.2334657933678));
#70009=CARTESIAN_POINT('Ctrl Pts',(29.9547860481489,1.18442751029054,30.2531021983901));
#70010=CARTESIAN_POINT('Ctrl Pts',(29.8001302980418,1.16832333064129,30.2625187720286));
#70011=CARTESIAN_POINT('Ctrl Pts',(29.5050358022508,1.07710916045235,30.2838737217699));
#70012=CARTESIAN_POINT('Ctrl Pts',(29.3676216445827,1.00262104003874,30.2949528877718));
#70013=CARTESIAN_POINT('Ctrl Pts',(29.133885390368,0.808265735464436,30.3161967092816));
#70014=CARTESIAN_POINT('Ctrl Pts',(29.0384365029953,0.691955856048158,30.3259351581227));
#70015=CARTESIAN_POINT('Ctrl Pts',(28.8928615291795,0.423965303949737,30.3449376912299));
#70016=CARTESIAN_POINT('Ctrl Pts',(28.8464607134353,0.273539680594875,30.3556039922081));
#70017=CARTESIAN_POINT('Ctrl Pts',(28.8153257979048,-0.0336925494769084,
30.3773890535762));
#70018=CARTESIAN_POINT('Ctrl Pts',(28.8297608924994,-0.187447360914171,
30.3882914188718));
#70019=CARTESIAN_POINT('Ctrl Pts',(28.915763813331,-0.477469105343294,30.4088561281766));
#70020=CARTESIAN_POINT('Ctrl Pts',(28.9852090680907,-0.611342914279369,
30.4176917737044));
#70021=CARTESIAN_POINT('Ctrl Pts',(29.1753547758778,-0.851973319195576,
30.4378994263954));
#70022=CARTESIAN_POINT('Ctrl Pts',(29.296552814894,-0.954486386260336,30.4489763873607));
#70023=CARTESIAN_POINT('Ctrl Pts',(29.5667870728762,-1.10289061661543,30.4708323290802));
#70024=CARTESIAN_POINT('Ctrl Pts',(29.7121150852083,-1.14942616389095,30.4814064433112));
#70025=CARTESIAN_POINT('Ctrl Pts',(29.9080894843003,-1.17254804864973,30.4942605325068));
#70026=CARTESIAN_POINT('Ctrl Pts',(29.9540678655128,-1.17524047358085,30.497179414468));
#70027=CARTESIAN_POINT('Ctrl Pts',(29.9999999999996,-1.17524047358085,30.4999999999999));
#70028=CARTESIAN_POINT('Origin',(30.,-1.21864324187371E-14,15.78125));
#70029=CARTESIAN_POINT('',(30.8234078741651,-0.838564036615812,30.5625));
#70030=CARTESIAN_POINT('Ctrl Pts',(29.9999999999996,-1.17524047358085,30.4999999999999));
#70031=CARTESIAN_POINT('Ctrl Pts',(30.1063627165445,-1.17524047358085,30.506531487003));
#70032=CARTESIAN_POINT('Ctrl Pts',(30.2124142608556,-1.16080842479057,30.5135555357051));
#70033=CARTESIAN_POINT('Ctrl Pts',(30.4106617155444,-1.10559796456395,30.5276868678729));
#70034=CARTESIAN_POINT('Ctrl Pts',(30.5022820820407,-1.06709869288998,30.5346780045058));
#70035=CARTESIAN_POINT('Ctrl Pts',(30.673678737238,-0.968061456707972,30.5487143145253));
#70036=CARTESIAN_POINT('Ctrl Pts',(30.7527765496958,-0.90791877422844,30.555703810039));
#70037=CARTESIAN_POINT('Ctrl Pts',(30.823407874166,-0.83856403661491,30.5625000000001));
#70038=CARTESIAN_POINT('Origin',(30.,-1.56558793706907E-14,30.5625000000001));
#70039=CARTESIAN_POINT('Origin',(30.,-1.32966554433622E-14,16.));
#70040=CARTESIAN_POINT('Origin',(30.,-1.32966554433622E-14,16.));
#70041=CARTESIAN_POINT('',(31.2041934952953,-0.894381364904537,16.3247595264192));
#70042=CARTESIAN_POINT('Ctrl Pts',(29.1765921258349,-0.838564036615844,
16.));
#70043=CARTESIAN_POINT('Ctrl Pts',(29.2487520159976,-0.936812680701164,
16.0195455809545));
#70044=CARTESIAN_POINT('Ctrl Pts',(29.3353435467743,-1.0235639347367,16.039234228078));
#70045=CARTESIAN_POINT('Ctrl Pts',(29.5376779891223,-1.17276771461038,16.0788670880384));
#70046=CARTESIAN_POINT('Ctrl Pts',(29.6536089107031,-1.23245734148137,16.0985110228563));
#70047=CARTESIAN_POINT('Ctrl Pts',(29.9561347058367,-1.33132329595442,16.1436679915754));
#70048=CARTESIAN_POINT('Ctrl Pts',(30.1342881765676,-1.34356937043143,16.1651272257976));
#70049=CARTESIAN_POINT('Ctrl Pts',(30.4639364648848,-1.31596498262617,16.2103767681647));
#70050=CARTESIAN_POINT('Ctrl Pts',(30.6256204275016,-1.27296147517128,16.233574208582));
#70051=CARTESIAN_POINT('Ctrl Pts',(30.9367837613818,-1.12785658919505,16.2803666131763));
#70052=CARTESIAN_POINT('Ctrl Pts',(31.0819753809162,-1.0232586553723,16.3034869854933));
#70053=CARTESIAN_POINT('Ctrl Pts',(31.2041934952953,-0.894381364904556,
16.3247595264192));
#70054=CARTESIAN_POINT('',(30.2433378840047,-1.48013062741372,16.3247595264192));
#70055=CARTESIAN_POINT('Origin',(30.,-1.32966554433622E-14,16.3247595264192));
#70056=CARTESIAN_POINT('Ctrl Pts',(30.0000000000046,1.33373412263454,16.1584936490537));
#70057=CARTESIAN_POINT('Ctrl Pts',(29.9229566197526,1.33637706265986,16.161136589079));
#70058=CARTESIAN_POINT('Ctrl Pts',(29.8544450638259,1.33215454753135,16.163603109717));
#70059=CARTESIAN_POINT('Ctrl Pts',(29.6282514683273,1.30599264999734,16.1719556820851));
#70060=CARTESIAN_POINT('Ctrl Pts',(29.4645017898244,1.25493599443995,16.1785525854589));
#70061=CARTESIAN_POINT('Ctrl Pts',(29.1556314965168,1.0904442613039,16.1921322573206));
#70062=CARTESIAN_POINT('Ctrl Pts',(29.0151927695643,0.975180135374777,16.1989814826418));
#70063=CARTESIAN_POINT('Ctrl Pts',(28.7777605589636,0.68493937081347,16.2122079855113));
#70064=CARTESIAN_POINT('Ctrl Pts',(28.6970848553023,0.520026749838233,16.218047438772));
#70065=CARTESIAN_POINT('Ctrl Pts',(28.5955913245901,0.191124499754384,16.2305887595464));
#70066=CARTESIAN_POINT('Ctrl Pts',(28.5759298114947,0.010043627653028,16.2373963058958));
#70067=CARTESIAN_POINT('Ctrl Pts',(28.6063542045486,-0.355647637044131,
16.2509482038391));
#70068=CARTESIAN_POINT('Ctrl Pts',(28.6584675525716,-0.536586390481523,
16.2575508938686));
#70069=CARTESIAN_POINT('Ctrl Pts',(28.804769485922,-0.819110586341092,16.2677424893791));
#70070=CARTESIAN_POINT('Ctrl Pts',(28.9031317119719,-0.969713974958467,
16.273653025791));
#70071=CARTESIAN_POINT('Ctrl Pts',(29.199410976174,-1.23941646392093,16.2879449223019));
#70072=CARTESIAN_POINT('Ctrl Pts',(29.3637987944395,-1.33889148571261,16.2948596529243));
#70073=CARTESIAN_POINT('Ctrl Pts',(29.6508112528307,-1.44362228182862,16.3055460935814));
#70074=CARTESIAN_POINT('Ctrl Pts',(29.7632922636866,-1.47020844863719,16.3094443635539));
#70075=CARTESIAN_POINT('Ctrl Pts',(29.9994132050485,-1.49732183809384,16.3170683877131));
#70076=CARTESIAN_POINT('Ctrl Pts',(30.1229027402064,-1.49587628373705,16.3207589898335));
#70077=CARTESIAN_POINT('Ctrl Pts',(30.2433378840021,-1.48013062741405,16.3247595264191));
#70078=CARTESIAN_POINT('Origin',(30.,-1.32966554433622E-14,16.));
#70079=CARTESIAN_POINT('Ctrl Pts',(30.0000000000002,-1.50000000000001,16.8125));
#70080=CARTESIAN_POINT('Ctrl Pts',(29.8374309170617,-1.50000000000001,16.8046783913503));
#70081=CARTESIAN_POINT('Ctrl Pts',(29.6757197620765,-1.47357729444258,16.7961640957352));
#70082=CARTESIAN_POINT('Ctrl Pts',(29.3345753610171,-1.35867108066285,16.7765589388149));
#70083=CARTESIAN_POINT('Ctrl Pts',(29.1621497524653,-1.25967607222118,16.7655132465099));
#70084=CARTESIAN_POINT('Ctrl Pts',(28.8706191056789,-1.00528518925076,16.7444205583108));
#70085=CARTESIAN_POINT('Ctrl Pts',(28.7525289442937,-0.85433413605806,16.7349630075588));
#70086=CARTESIAN_POINT('Ctrl Pts',(28.5748830688675,-0.508513347476126,
16.7157507415264));
#70087=CARTESIAN_POINT('Ctrl Pts',(28.5201083225798,-0.315342861227666,
16.705019047846));
#70088=CARTESIAN_POINT('Ctrl Pts',(28.4893812381258,0.0768796360488758,
16.6832289091084));
#70089=CARTESIAN_POINT('Ctrl Pts',(28.5120877046559,0.272040866827356,16.6723866185096));
#70090=CARTESIAN_POINT('Ctrl Pts',(28.6297398561329,0.63947572665909,16.6519735707412));
#70091=CARTESIAN_POINT('Ctrl Pts',(28.7222788636186,0.808683440996407,16.6431776245867));
#70092=CARTESIAN_POINT('Ctrl Pts',(28.9715826684579,1.11011928821307,16.6228097717056));
#70093=CARTESIAN_POINT('Ctrl Pts',(29.1285972489479,1.2371944826493,16.6117255376675));
#70094=CARTESIAN_POINT('Ctrl Pts',(29.4764211128784,1.41875808710319,16.5899474207545));
#70095=CARTESIAN_POINT('Ctrl Pts',(29.6625283053455,1.47415762233606,16.5794544583034));
#70096=CARTESIAN_POINT('Ctrl Pts',(30.0492497355351,1.51196727264003,16.5597980467542));
#70097=CARTESIAN_POINT('Ctrl Pts',(30.2463054645629,1.49258742024928,16.5504437178179));
#70098=CARTESIAN_POINT('Ctrl Pts',(30.6231564270347,1.37865583779414,16.529147701253));
#70099=CARTESIAN_POINT('Ctrl Pts',(30.7990856424485,1.28470816478719,16.5180736453463));
#70100=CARTESIAN_POINT('Ctrl Pts',(31.0988336211311,1.03864170876325,16.4968168346638));
#70101=CARTESIAN_POINT('Ctrl Pts',(31.2215556301223,0.891049402060874,16.4870027445589));
#70102=CARTESIAN_POINT('Ctrl Pts',(31.4094506590971,0.550436181771672,16.4680797878762));
#70103=CARTESIAN_POINT('Ctrl Pts',(31.4699049158396,0.359005410515039,16.4574447450286));
#70104=CARTESIAN_POINT('Ctrl Pts',(31.5122933091642,-0.0326520383467692,
16.4356859978696));
#70105=CARTESIAN_POINT('Ctrl Pts',(31.4952196858866,-0.228959953862231,
16.4247800025632));
#70106=CARTESIAN_POINT('Ctrl Pts',(31.3881172406464,-0.599526626811694,
16.4041929651771));
#70107=CARTESIAN_POINT('Ctrl Pts',(31.300844426577,-0.770779121647004,16.3953430421646));
#70108=CARTESIAN_POINT('Ctrl Pts',(31.0690211851343,-1.06871793972269,16.3759133629805));
#70109=CARTESIAN_POINT('Ctrl Pts',(30.9276174608134,-1.1935139431374,16.3656435174717));
#70110=CARTESIAN_POINT('Ctrl Pts',(30.6058972740411,-1.3849221656676,16.3448478526983));
#70111=CARTESIAN_POINT('Ctrl Pts',(30.4282952255496,-1.44972308953241,16.3345029444933));
#70112=CARTESIAN_POINT('Ctrl Pts',(30.2433378840032,-1.48013062741398,16.3247595264191));
#70113=CARTESIAN_POINT('Ctrl Pts',(31.2041934952953,-0.894381364904531,
16.3247595264192));
#70114=CARTESIAN_POINT('Ctrl Pts',(31.2978308567217,-0.768308186313297,
16.33276668881));
#70115=CARTESIAN_POINT('Ctrl Pts',(31.3710758402094,-0.628345765505124,
16.3400919019164));
#70116=CARTESIAN_POINT('Ctrl Pts',(31.4735871865681,-0.324510524004584,
16.3569716375553));
#70117=CARTESIAN_POINT('Ctrl Pts',(31.5001727925959,-0.161986730686535,
16.3660007371841));
#70118=CARTESIAN_POINT('Ctrl Pts',(31.4997859079869,0.202485940247452,16.3862492189027));
#70119=CARTESIAN_POINT('Ctrl Pts',(31.4592164909323,0.401327421311596,16.3972959678507));
#70120=CARTESIAN_POINT('Ctrl Pts',(31.3063109849155,0.761415726638002,16.4173008737022));
#70121=CARTESIAN_POINT('Ctrl Pts',(31.1993149527403,0.920789441682028,16.4262087502572));
#70122=CARTESIAN_POINT('Ctrl Pts',(30.927737201713,1.19478997630558,16.4468861668575));
#70123=CARTESIAN_POINT('Ctrl Pts',(30.7642938567671,1.30539963746525,16.4578223290454));
#70124=CARTESIAN_POINT('Ctrl Pts',(30.4012071029328,1.45894804482998,16.4795565821721));
#70125=CARTESIAN_POINT('Ctrl Pts',(30.2045613271838,1.49922584611532,16.4901365342825));
#70126=CARTESIAN_POINT('Ctrl Pts',(29.8153532439137,1.50071981302521,16.5089038160006));
#70127=CARTESIAN_POINT('Ctrl Pts',(29.6264615866043,1.46518905889,16.5189388458803));
#70128=CARTESIAN_POINT('Ctrl Pts',(29.2652001883276,1.32257698188105,16.5402814895924));
#70129=CARTESIAN_POINT('Ctrl Pts',(29.0973517156097,1.21423683760981,16.5513665514533));
#70130=CARTESIAN_POINT('Ctrl Pts',(28.8152158635768,0.940440031832944,16.5725462857904));
#70131=CARTESIAN_POINT('Ctrl Pts',(28.7029935775965,0.778399491568193,16.5817555838018));
#70132=CARTESIAN_POINT('Ctrl Pts',(28.5479560175053,0.422736814401416,16.6015146214222));
#70133=CARTESIAN_POINT('Ctrl Pts',(28.5057189580682,0.232905312381588,16.6120608159788));
#70134=CARTESIAN_POINT('Ctrl Pts',(28.4951590610144,-0.159927799856357,
16.6338848777698));
#70135=CARTESIAN_POINT('Ctrl Pts',(28.5299387266544,-0.359247208886169,
16.6449581782715));
#70136=CARTESIAN_POINT('Ctrl Pts',(28.6722713443677,-0.723556115441905,
16.665197561969));
#70137=CARTESIAN_POINT('Ctrl Pts',(28.7749427214916,-0.886360478602884,
16.6740138619457));
#70138=CARTESIAN_POINT('Ctrl Pts',(29.0386829229376,-1.16785093047933,16.6945222475229));
#70139=CARTESIAN_POINT('Ctrl Pts',(29.1984334219549,-1.28276611305493,16.7054003353954));
#70140=CARTESIAN_POINT('Ctrl Pts',(29.5564186818177,-1.44663336596446,16.7271757773774));
#70141=CARTESIAN_POINT('Ctrl Pts',(29.7518446854206,-1.49263399091841,16.7378560104973));
#70142=CARTESIAN_POINT('Ctrl Pts',(29.9670564156215,-1.49972884223086,16.7484074688974));
#70143=CARTESIAN_POINT('Ctrl Pts',(29.9835330897433,-1.50000000000001,16.7492077354109));
#70144=CARTESIAN_POINT('Ctrl Pts',(30.,-1.50000000000001,16.75));
#70145=CARTESIAN_POINT('Origin',(27.4975425688509,1.03655180724329,15.7235432561772));
#70146=CARTESIAN_POINT('',(27.507537153458,1.0459948352816,31.5905494329235));
#70147=CARTESIAN_POINT('',(27.4979325782409,1.02280733953167,31.5905494329235));
#70148=CARTESIAN_POINT('Origin',(27.4975191258909,1.03656151763528,31.5962151370756));
#70149=CARTESIAN_POINT('',(27.4979325782409,1.02280733953167,33.8969505670765));
#70150=CARTESIAN_POINT('',(27.4979325782409,1.02280733953167,15.7235432561772));
#70151=CARTESIAN_POINT('',(27.507537153458,1.0459948352816,33.8969505670765));
#70152=CARTESIAN_POINT('Origin',(27.4975191258914,1.03656151763504,33.891284862925));
#70153=CARTESIAN_POINT('',(27.507537153458,1.0459948352816,15.7235432561772));
#70154=CARTESIAN_POINT('Origin',(27.4239298924869,0.837015916807854,15.7235432561772));
#70155=CARTESIAN_POINT('',(27.4331527756843,0.847214001212616,31.5905494329235));
#70156=CARTESIAN_POINT('',(27.4253970781159,0.823344418487269,31.5905494329235));
#70157=CARTESIAN_POINT('Origin',(27.4239057599253,0.837023757952457,31.5962151370753));
#70158=CARTESIAN_POINT('',(27.4253970781159,0.823344418487269,33.8969505670765));
#70159=CARTESIAN_POINT('',(27.4253970781159,0.823344418487269,15.7235432561772));
#70160=CARTESIAN_POINT('',(27.4331527756843,0.847214001212616,33.8969505670765));
#70161=CARTESIAN_POINT('Origin',(27.4239057599256,0.837023757952334,33.8912848629251));
#70162=CARTESIAN_POINT('',(27.4331527756843,0.847214001212616,15.7235432561772));
#70163=CARTESIAN_POINT('Origin',(27.3661995449658,0.632319544909263,15.7235432561772));
#70164=CARTESIAN_POINT('',(27.3745938646118,0.643209811098917,31.5905494329235));
#70165=CARTESIAN_POINT('',(27.3687348611468,0.618805305313091,31.5905494329235));
#70166=CARTESIAN_POINT('Origin',(27.3661748715877,0.632325468463276,31.5962151370755));
#70167=CARTESIAN_POINT('',(27.3687348611468,0.618805305313091,33.8969505670765));
#70168=CARTESIAN_POINT('',(27.3687348611468,0.618805305313091,15.7235432561772));
#70169=CARTESIAN_POINT('',(27.3745938646118,0.643209811098917,33.8969505670765));
#70170=CARTESIAN_POINT('Origin',(27.3661748715881,0.632325468463155,33.891284862925));
#70171=CARTESIAN_POINT('',(27.3745938646118,0.643209811098917,15.7235432561772));
#70172=CARTESIAN_POINT('Origin',(27.3247074530776,0.423724712748722,15.7235432561772));
#70173=CARTESIAN_POINT('',(27.3322214554001,0.435240018610828,31.5905494329235));
#70174=CARTESIAN_POINT('',(27.328295268743,0.410451051658016,31.5905494329235));
#70175=CARTESIAN_POINT('Origin',(27.3246823910025,0.423728682191457,31.5962151370754));
#70176=CARTESIAN_POINT('',(27.328295268743,0.410451051658016,33.8969505670765));
#70177=CARTESIAN_POINT('',(27.328295268743,0.410451051658016,15.7235432561772));
#70178=CARTESIAN_POINT('',(27.3322214554001,0.435240018610828,33.8969505670765));
#70179=CARTESIAN_POINT('Origin',(27.3246823910029,0.423728682191396,33.891284862925));
#70180=CARTESIAN_POINT('',(27.3322214554001,0.435240018610828,15.7235432561772));
#70181=CARTESIAN_POINT('Origin',(27.2997094293662,0.212517476831317,15.7235432561772));
#70182=CARTESIAN_POINT('',(27.3062967880422,0.224586826676008,31.5905494329235));
#70183=CARTESIAN_POINT('',(27.3043276244395,0.199566230780642,31.5905494329235));
#70184=CARTESIAN_POINT('Origin',(27.2996841331102,0.212519467689854,31.5962151370755));
#70185=CARTESIAN_POINT('',(27.3043276244395,0.199566230780642,33.8969505670765));
#70186=CARTESIAN_POINT('',(27.3043276244395,0.199566230780642,15.7235432561772));
#70187=CARTESIAN_POINT('',(27.3062967880422,0.224586826676008,33.8969505670765));
#70188=CARTESIAN_POINT('Origin',(27.2996841331108,0.212519467689809,33.8912848629251));
#70189=CARTESIAN_POINT('',(27.3062967880422,0.224586826676008,15.7235432561772));
#70190=CARTESIAN_POINT('Origin',(27.2913595949605,1.54398896472578E-14,
15.7235432561772));
#70191=CARTESIAN_POINT('',(27.2969796967333,0.0125489822720319,31.5905494329235));
#70192=CARTESIAN_POINT('',(27.2969796967333,-0.0125489822720016,31.5905494329235));
#70193=CARTESIAN_POINT('Origin',(27.2913342204835,1.66533453693773E-14,
31.5962151370755));
#70194=CARTESIAN_POINT('',(27.2969796967333,-0.0125489822720016,33.8969505670765));
#70195=CARTESIAN_POINT('',(27.2969796967333,-0.0125489822720016,15.7235432561772));
#70196=CARTESIAN_POINT('',(27.2969796967333,0.0125489822720319,33.8969505670765));
#70197=CARTESIAN_POINT('Origin',(27.2913342204839,1.44047100636424E-14,
33.891284862925));
#70198=CARTESIAN_POINT('',(27.2969796967333,0.0125489822720319,15.7235432561772));
#70199=CARTESIAN_POINT('Origin',(27.5865837274296,1.22969701109861,15.7235432561772));
#70200=CARTESIAN_POINT('',(27.5972883935087,1.23832676336248,31.5905494329235));
#70201=CARTESIAN_POINT('',(27.5858941560429,1.2159643132099,31.5905494329235));
#70202=CARTESIAN_POINT('Origin',(27.586561118605,1.22970853087013,31.5962151370754));
#70203=CARTESIAN_POINT('',(27.5858941560429,1.2159643132099,33.8969505670765));
#70204=CARTESIAN_POINT('',(27.5858941560429,1.2159643132099,15.7235432561772));
#70205=CARTESIAN_POINT('',(27.5972883935087,1.23832676336248,33.8969505670765));
#70206=CARTESIAN_POINT('Origin',(27.5865611186055,1.22970853086989,33.891284862925));
#70207=CARTESIAN_POINT('',(27.5972883935087,1.23832676336248,15.7235432561772));
#70208=CARTESIAN_POINT('Origin',(27.690504399871,1.41526072396476,15.7235432561772));
#70209=CARTESIAN_POINT('',(27.701853149596,1.42302399516181,31.5905494329235));
#70210=CARTESIAN_POINT('',(27.6887394991445,1.40162446254803,31.5905494329235));
#70211=CARTESIAN_POINT('Origin',(27.6904827645727,1.41527398209261,31.5962151370755));
#70212=CARTESIAN_POINT('',(27.6887394991445,1.40162446254803,33.8969505670765));
#70213=CARTESIAN_POINT('',(27.6887394991445,1.40162446254803,15.7235432561772));
#70214=CARTESIAN_POINT('',(27.701853149596,1.42302399516181,33.8969505670765));
#70215=CARTESIAN_POINT('Origin',(27.6904827645732,1.41527398209234,33.891284862925));
#70216=CARTESIAN_POINT('',(27.701853149596,1.42302399516181,15.7235432561772));
#70217=CARTESIAN_POINT('Origin',(27.8086638806724,1.59209888384573,15.7235432561772));
#70218=CARTESIAN_POINT('',(27.8205867452275,1.59894781082746,31.5905494329235));
#70219=CARTESIAN_POINT('',(27.805834531806,1.57864313098712,31.5905494329235));
#70220=CARTESIAN_POINT('Origin',(27.8086433522893,1.59211379858911,31.5962151370755));
#70221=CARTESIAN_POINT('',(27.805834531806,1.57864313098712,33.8969505670765));
#70222=CARTESIAN_POINT('',(27.805834531806,1.57864313098712,15.7235432561772));
#70223=CARTESIAN_POINT('',(27.8205867452275,1.59894781082746,33.8969505670765));
#70224=CARTESIAN_POINT('Origin',(27.8086433522896,1.59211379858882,33.8912848629251));
#70225=CARTESIAN_POINT('',(27.8205867452275,1.59894781082746,15.7235432561772));
#70226=CARTESIAN_POINT('Origin',(27.9403336773427,1.75912122468118,15.7235432561772));
#70227=CARTESIAN_POINT('',(27.9527571483031,1.76501358153527,31.5905494329235));
#70228=CARTESIAN_POINT('',(27.9364573242129,1.74592893957157,31.5905494329235));
#70229=CARTESIAN_POINT('Origin',(27.9403143824389,1.75913770408581,31.5962151370755));
#70230=CARTESIAN_POINT('',(27.9364573242129,1.74592893957157,33.8969505670765));
#70231=CARTESIAN_POINT('',(27.9364573242129,1.74592893957157,15.7235432561772));
#70232=CARTESIAN_POINT('',(27.9527571483031,1.76501358153527,33.8969505670765));
#70233=CARTESIAN_POINT('Origin',(27.9403143824393,1.75913770408551,33.891284862925));
#70234=CARTESIAN_POINT('',(27.9527571483031,1.76501358153527,15.7235432561772));
#70235=CARTESIAN_POINT('Origin',(28.0847020018007,1.9152979981993,15.7235432561772));
#70236=CARTESIAN_POINT('',(28.0975494843367,1.92019745658633,31.5905494329235));
#70237=CARTESIAN_POINT('',(28.0798025434137,1.90245051566326,31.5905494329235));
#70238=CARTESIAN_POINT('Origin',(28.0846840593359,1.9153159406641,31.5962151370755));
#70239=CARTESIAN_POINT('',(28.0798025434137,1.90245051566326,33.8969505670765));
#70240=CARTESIAN_POINT('',(28.0798025434137,1.90245051566326,15.7235432561772));
#70241=CARTESIAN_POINT('',(28.0975494843367,1.92019745658633,33.8969505670765));
#70242=CARTESIAN_POINT('Origin',(28.0846840593363,1.91531594066375,33.891284862925));
#70243=CARTESIAN_POINT('',(28.0975494843367,1.92019745658633,15.7235432561772));
#70244=CARTESIAN_POINT('Origin',(28.2408787753188,2.05966632265731,15.7235432561772));
#70245=CARTESIAN_POINT('',(28.2540710604285,2.06354267578708,31.5905494329235));
#70246=CARTESIAN_POINT('',(28.2349864184648,2.0472428516969,31.5905494329235));
#70247=CARTESIAN_POINT('Origin',(28.2408622959143,2.05968561756092,31.5962151370754));
#70248=CARTESIAN_POINT('',(28.2349864184648,2.0472428516969,33.8969505670765));
#70249=CARTESIAN_POINT('',(28.2349864184648,2.0472428516969,15.7235432561772));
#70250=CARTESIAN_POINT('',(28.2540710604285,2.06354267578708,33.8969505670765));
#70251=CARTESIAN_POINT('Origin',(28.2408622959145,2.05968561756065,33.891284862925));
#70252=CARTESIAN_POINT('',(28.2540710604285,2.06354267578708,15.7235432561772));
#70253=CARTESIAN_POINT('Origin',(28.4079011161543,2.19133611932758,15.7235432561772));
#70254=CARTESIAN_POINT('',(28.4213568690129,2.19416546819404,31.5905494329235));
#70255=CARTESIAN_POINT('',(28.4010521891726,2.1794132547725,31.5905494329235));
#70256=CARTESIAN_POINT('Origin',(28.407886201411,2.19135664771063,31.5962151370753));
#70257=CARTESIAN_POINT('',(28.4010521891726,2.1794132547725,33.8969505670765));
#70258=CARTESIAN_POINT('',(28.4010521891726,2.1794132547725,15.7235432561772));
#70259=CARTESIAN_POINT('',(28.4213568690129,2.19416546819404,33.8969505670765));
#70260=CARTESIAN_POINT('Origin',(28.4078862014112,2.19135664771024,33.8912848629252));
#70261=CARTESIAN_POINT('',(28.4213568690129,2.19416546819404,15.7235432561772));
#70262=CARTESIAN_POINT('Origin',(28.5847392760353,2.309495600129,15.7235432561772));
#70263=CARTESIAN_POINT('',(28.598375537452,2.31126050085552,31.5905494329235));
#70264=CARTESIAN_POINT('',(28.5769760048382,2.29814685040398,31.5905494329235));
#70265=CARTESIAN_POINT('Origin',(28.5847260179075,2.30951723542729,31.5962151370754));
#70266=CARTESIAN_POINT('',(28.5769760048382,2.29814685040398,33.8969505670765));
#70267=CARTESIAN_POINT('',(28.5769760048382,2.29814685040398,15.7235432561772));
#70268=CARTESIAN_POINT('',(28.598375537452,2.31126050085552,33.8969505670765));
#70269=CARTESIAN_POINT('Origin',(28.5847260179077,2.30951723542689,33.891284862925));
#70270=CARTESIAN_POINT('',(28.598375537452,2.31126050085552,15.7235432561772));
#70271=CARTESIAN_POINT('Origin',(28.7703029889014,2.4134162725704,15.7235432561772));
#70272=CARTESIAN_POINT('',(28.7840356867901,2.41410584395713,31.5905494329235));
#70273=CARTESIAN_POINT('',(28.7616732366375,2.40271160649133,31.5905494329235));
#70274=CARTESIAN_POINT('Origin',(28.7702914691299,2.41343888139489,31.5962151370753));
#70275=CARTESIAN_POINT('',(28.7616732366375,2.40271160649133,33.8969505670765));
#70276=CARTESIAN_POINT('',(28.7616732366375,2.40271160649133,15.7235432561772));
#70277=CARTESIAN_POINT('',(28.7840356867901,2.41410584395713,33.8969505670765));
#70278=CARTESIAN_POINT('Origin',(28.7702914691301,2.41343888139455,33.8912848629251));
#70279=CARTESIAN_POINT('',(28.7840356867901,2.41410584395713,15.7235432561772));
#70280=CARTESIAN_POINT('Origin',(30.,-1.32966554433622E-14,34.));
#70281=CARTESIAN_POINT('',(28.75,0.721687836487017,33.8917468245269));
#70282=CARTESIAN_POINT('',(28.75,-1.44824191072421E-14,33.6983711515529));
#70283=CARTESIAN_POINT('Ctrl Pts',(28.75,0.72168783648698,33.8917468245269));
#70284=CARTESIAN_POINT('Ctrl Pts',(28.75,0.334936490538873,33.6983711515529));
#70285=CARTESIAN_POINT('Ctrl Pts',(28.75,-1.55145598201422E-14,33.6983711515529));
#70286=CARTESIAN_POINT('',(30.,1.44337567297405,33.8917468245269));
#70287=CARTESIAN_POINT('Ctrl Pts',(30.,1.44337567297404,33.8917468245269));
#70288=CARTESIAN_POINT('Ctrl Pts',(29.375,1.08253175473053,33.5309029062834));
#70289=CARTESIAN_POINT('Ctrl Pts',(28.75,0.721687836487025,33.8917468245269));
#70290=CARTESIAN_POINT('',(31.25,0.721687836487017,33.891746824527));
#70291=CARTESIAN_POINT('Ctrl Pts',(31.25,0.721687836487027,33.8917468245269));
#70292=CARTESIAN_POINT('Ctrl Pts',(30.625,1.08253175473053,33.5309029062834));
#70293=CARTESIAN_POINT('Ctrl Pts',(30.,1.44337567297404,33.8917468245269));
#70294=CARTESIAN_POINT('',(31.25,-0.72168783648704,33.8917468245269));
#70295=CARTESIAN_POINT('Ctrl Pts',(31.25,-0.721687836487026,33.8917468245269));
#70296=CARTESIAN_POINT('Ctrl Pts',(31.25,-1.26287869051112E-14,33.5309029062834));
#70297=CARTESIAN_POINT('Ctrl Pts',(31.25,0.721687836487001,33.8917468245269));
#70298=CARTESIAN_POINT('',(30.,-1.44337567297407,33.8917468245269));
#70299=CARTESIAN_POINT('Ctrl Pts',(30.,-1.44337567297406,33.8917468245269));
#70300=CARTESIAN_POINT('Ctrl Pts',(30.625,-1.08253175473056,33.5309029062834));
#70301=CARTESIAN_POINT('Ctrl Pts',(31.25,-0.721687836487049,33.8917468245269));
#70302=CARTESIAN_POINT('',(28.75,-0.721687836487044,33.8917468245269));
#70303=CARTESIAN_POINT('Ctrl Pts',(28.75,-0.721687836487053,33.8917468245269));
#70304=CARTESIAN_POINT('Ctrl Pts',(29.375,-1.08253175473056,33.5309029062834));
#70305=CARTESIAN_POINT('Ctrl Pts',(30.,-1.44337567297406,33.8917468245269));
#70306=CARTESIAN_POINT('Ctrl Pts',(28.75,-1.55145598201422E-14,33.6983711515529));
#70307=CARTESIAN_POINT('Ctrl Pts',(28.75,-0.334936490538901,33.6983711515529));
#70308=CARTESIAN_POINT('Ctrl Pts',(28.75,-0.721687836487005,33.8917468245269));
#70309=CARTESIAN_POINT('',(28.4483711515529,-1.34873480853811E-14,34.));
#70310=CARTESIAN_POINT('',(28.4483711515529,-1.34873480853811E-14,34.));
#70311=CARTESIAN_POINT('Origin',(30.,-1.32966554433622E-14,34.));
#70312=CARTESIAN_POINT('Origin',(30.,-1.32966554433622E-14,33.953125));
#70313=CARTESIAN_POINT('',(30.,-2.6137293696319,33.9862706303681));
#70314=CARTESIAN_POINT('Origin',(30.,-1.32966554433622E-14,33.9862706303681));
#70315=CARTESIAN_POINT('',(30.,-2.58058373926378,34.));
#70316=CARTESIAN_POINT('Origin',(30.,-2.58058373926378,33.953125));
#70317=CARTESIAN_POINT('Origin',(30.,-1.32966554433622E-14,34.));
#70318=CARTESIAN_POINT('Origin',(30.,-1.32966554433622E-14,33.8637293696319));
#70319=CARTESIAN_POINT('',(30.012548982272,-2.70302030326669,33.8969505670765));
#70320=CARTESIAN_POINT('',(30.,-2.69489040503949,33.9051095949605));
#70321=CARTESIAN_POINT('Ctrl Pts',(30.012548982272,-2.70302030326672,33.8969505670765));
#70322=CARTESIAN_POINT('Ctrl Pts',(30.0117595027242,-2.70125749446881,33.8987170220581));
#70323=CARTESIAN_POINT('Ctrl Pts',(30.0105608813139,-2.69960157002983,33.9003782103613));
#70324=CARTESIAN_POINT('Ctrl Pts',(30.0079476416933,-2.69733049287042,33.9026580100842));
#70325=CARTESIAN_POINT('Ctrl Pts',(30.0065751610721,-2.69644647069985,33.9035459832655));
#70326=CARTESIAN_POINT('Ctrl Pts',(30.0034509360646,-2.69522714758869,33.9047710768107));
#70327=CARTESIAN_POINT('Ctrl Pts',(30.0017003028408,-2.69489040503949,33.9051095949605));
#70328=CARTESIAN_POINT('Ctrl Pts',(30.,-2.69489040503949,33.9051095949605));
#70329=CARTESIAN_POINT('',(30.027378900953,-2.73613365141358,33.8637293696319));
#70330=CARTESIAN_POINT('Ctrl Pts',(30.0273789009518,-2.73613365141079,33.8637293696347));
#70331=CARTESIAN_POINT('Ctrl Pts',(30.019918653996,-2.71947585577342,33.8804609779984));
#70332=CARTESIAN_POINT('Ctrl Pts',(30.0125489822686,-2.70302030325915,33.8969505670841));
#70333=CARTESIAN_POINT('',(30.1873800711417,-2.72984718831552,33.8637293696319));
#70334=CARTESIAN_POINT('Origin',(30.,-1.32966554433622E-14,33.8637293696319));
#70335=CARTESIAN_POINT('',(30.1995662307806,-2.69567237556051,33.8969505670765));
#70336=CARTESIAN_POINT('Ctrl Pts',(30.1995662307834,-2.69567237555272,33.8969505670841));
#70337=CARTESIAN_POINT('Ctrl Pts',(30.1935103650644,-2.71265541886991,33.8804609779983));
#70338=CARTESIAN_POINT('Ctrl Pts',(30.1873800711428,-2.72984718831265,33.8637293696347));
#70339=CARTESIAN_POINT('',(30.224586826676,-2.69370321195777,33.8969505670765));
#70340=CARTESIAN_POINT('Origin',(30.2125187883694,-2.70030745889015,33.8912937927563));
#70341=CARTESIAN_POINT('',(30.241969073019,-2.72555094069392,33.8637293696319));
#70342=CARTESIAN_POINT('Ctrl Pts',(30.2419690730176,-2.72555094069121,33.8637293696347));
#70343=CARTESIAN_POINT('Ctrl Pts',(30.233224867931,-2.70952981970859,33.8804609779984));
#70344=CARTESIAN_POINT('Ctrl Pts',(30.2245868266721,-2.69370321195052,33.8969505670841));
#70345=CARTESIAN_POINT('',(30.4009837827878,-2.70673030953518,33.8637293696319));
#70346=CARTESIAN_POINT('Origin',(30.,-1.32966554433622E-14,33.8637293696319));
#70347=CARTESIAN_POINT('',(30.410451051658,-2.67170473125697,33.8969505670765));
#70348=CARTESIAN_POINT('Ctrl Pts',(30.4104510516601,-2.67170473124899,33.8969505670841));
#70349=CARTESIAN_POINT('Ctrl Pts',(30.4057463283755,-2.68911055925959,33.8804609779983));
#70350=CARTESIAN_POINT('Ctrl Pts',(30.4009837827886,-2.70673030953223,33.8637293696347));
#70351=CARTESIAN_POINT('',(30.4352400186108,-2.66777854459992,33.8969505670765));
#70352=CARTESIAN_POINT('Origin',(30.4237273077484,-2.67530902338216,33.8912940899387));
#70353=CARTESIAN_POINT('',(30.455067425287,-2.69816430208722,33.8637293696319));
#70354=CARTESIAN_POINT('Ctrl Pts',(30.4550674252854,-2.69816430208464,33.8637293696347));
#70355=CARTESIAN_POINT('Ctrl Pts',(30.445093173,-2.68287863129519,33.8804609779983));
#70356=CARTESIAN_POINT('Ctrl Pts',(30.4352400186063,-2.667778544593,33.8969505670841));
#70357=CARTESIAN_POINT('',(30.6121152960723,-2.66692553831739,33.8637293696319));
#70358=CARTESIAN_POINT('Origin',(30.,-1.32966554433622E-14,33.8637293696319));
#70359=CARTESIAN_POINT('',(30.618805305313,-2.63126513885325,33.8969505670765));
#70360=CARTESIAN_POINT('Ctrl Pts',(30.6188053053145,-2.63126513884514,33.8969505670841));
#70361=CARTESIAN_POINT('Ctrl Pts',(30.6154807306477,-2.64898643883144,33.8804609779984));
#70362=CARTESIAN_POINT('Ctrl Pts',(30.6121152960728,-2.66692553831439,33.8637293696347));
#70363=CARTESIAN_POINT('',(30.6432098110989,-2.62540613538822,33.8969505670765));
#70364=CARTESIAN_POINT('Origin',(30.6323233823986,-2.63381649164655,33.8912943077151));
#70365=CARTESIAN_POINT('',(30.6653601355529,-2.65414258332748,33.8637293696319));
#70366=CARTESIAN_POINT('Ctrl Pts',(30.665360135551,-2.65414258332505,33.8637293696347));
#70367=CARTESIAN_POINT('Ctrl Pts',(30.6542173306489,-2.63968660397218,33.8804609779983));
#70368=CARTESIAN_POINT('Ctrl Pts',(30.6432098110939,-2.62540613538168,33.8969505670841));
#70369=CARTESIAN_POINT('',(30.8194729150075,-2.61067828431314,33.8637293696319));
#70370=CARTESIAN_POINT('Origin',(30.,-1.32966554433622E-14,33.8637293696319));
#70371=CARTESIAN_POINT('',(30.8233444184872,-2.57460292188405,33.8969505670765));
#70372=CARTESIAN_POINT('Ctrl Pts',(30.8233444184881,-2.57460292187584,33.8969505670841));
#70373=CARTESIAN_POINT('Ctrl Pts',(30.8214204895475,-2.59253043613051,33.8804609779984));
#70374=CARTESIAN_POINT('Ctrl Pts',(30.8194729150079,-2.61067828431011,33.8637293696347));
#70375=CARTESIAN_POINT('',(30.8472140012126,-2.56684722431573,33.8969505670765));
#70376=CARTESIAN_POINT('Origin',(30.837020957759,-2.57608565616367,33.891294472568));
#70377=CARTESIAN_POINT('',(30.8715506793283,-2.59375719294955,33.8637293696319));
#70378=CARTESIAN_POINT('Ctrl Pts',(30.8715506793263,-2.59375719294726,33.8637293696347));
#70379=CARTESIAN_POINT('Ctrl Pts',(30.8593080209051,-2.58022003095079,33.8804609779983));
#70380=CARTESIAN_POINT('Ctrl Pts',(30.8472140012071,-2.5668472243096,33.8969505670841));
#70381=CARTESIAN_POINT('',(31.0217782109194,-2.53833533054748,33.8637293696319));
#70382=CARTESIAN_POINT('Origin',(30.,-1.32966554433622E-14,33.8637293696319));
#70383=CARTESIAN_POINT('',(31.0228073395316,-2.5020674217591,33.8969505670765));
#70384=CARTESIAN_POINT('Ctrl Pts',(31.0228073395319,-2.50206742175084,33.8969505670841));
#70385=CARTESIAN_POINT('Ctrl Pts',(31.0222959179792,-2.52009062118698,33.8804609779983));
#70386=CARTESIAN_POINT('Ctrl Pts',(31.0217782109195,-2.53833533054442,33.8637293696347));
#70387=CARTESIAN_POINT('',(31.0459948352815,-2.49246284654201,33.8969505670765));
#70388=CARTESIAN_POINT('Origin',(31.0365580110689,-2.50247243285094,33.8912946002427));
#70389=CARTESIAN_POINT('',(31.0723678233457,-2.51738042696529,33.8637293696319));
#70390=CARTESIAN_POINT('Ctrl Pts',(31.0723678233435,-2.51738042696321,33.8637293696347));
#70391=CARTESIAN_POINT('Ctrl Pts',(31.0591007914634,-2.5048455434284,33.8804609779984));
#70392=CARTESIAN_POINT('Ctrl Pts',(31.0459948352755,-2.49246284653634,33.8969505670841));
#70393=CARTESIAN_POINT('',(31.2177839043851,-2.45034269538684,33.8637293696319));
#70394=CARTESIAN_POINT('Origin',(30.,-1.32966554433622E-14,33.8637293696319));
#70395=CARTESIAN_POINT('',(31.2159643132098,-2.41410584395714,33.8969505670765));
#70396=CARTESIAN_POINT('Ctrl Pts',(31.2159643132094,-2.4141058439489,33.8969505670841));
#70397=CARTESIAN_POINT('Ctrl Pts',(31.2168685521286,-2.43211360954869,33.8804609779984));
#70398=CARTESIAN_POINT('Ctrl Pts',(31.2177839043849,-2.4503426953838,33.8637293696347));
#70399=CARTESIAN_POINT('',(31.2383267633624,-2.40271160649135,33.8969505670765));
#70400=CARTESIAN_POINT('Origin',(31.2297043338602,-2.41343066267494,33.891294700665));
#70401=CARTESIAN_POINT('',(31.2665734631337,-2.42548317353486,33.8637293696319));
#70402=CARTESIAN_POINT('Ctrl Pts',(31.2665734631313,-2.42548317353296,33.8637293696347));
#70403=CARTESIAN_POINT('Ctrl Pts',(31.2523638534557,-2.41402785018508,33.8804609779983));
#70404=CARTESIAN_POINT('Ctrl Pts',(31.238326763356,-2.40271160648617,33.8969505670841));
#70405=CARTESIAN_POINT('',(31.4062815551261,-2.34724288268751,33.8637293696319));
#70406=CARTESIAN_POINT('Origin',(30.,-1.32966554433622E-14,33.8637293696319));
#70407=CARTESIAN_POINT('',(31.401624462548,-2.31126050085554,33.8969505670765));
#70408=CARTESIAN_POINT('Ctrl Pts',(31.4016244625469,-2.31126050084735,33.8969505670841));
#70409=CARTESIAN_POINT('Ctrl Pts',(31.4039387870044,-2.32914180874765,33.8804609779983));
#70410=CARTESIAN_POINT('Ctrl Pts',(31.4062815551258,-2.34724288268448,33.8637293696347));
#70411=CARTESIAN_POINT('',(31.4230239951618,-2.29814685040399,33.8969505670765));
#70412=CARTESIAN_POINT('Origin',(31.4152691174526,-2.30950931155476,33.8912947803757));
#70413=CARTESIAN_POINT('',(31.452970256343,-2.31863200978458,33.8637293696319));
#70414=CARTESIAN_POINT('Ctrl Pts',(31.4529702563405,-2.31863200978284,33.8637293696347));
#70415=CARTESIAN_POINT('Ctrl Pts',(31.4379056758382,-2.30832687249962,33.8804609779984));
#70416=CARTESIAN_POINT('Ctrl Pts',(31.423023995155,-2.29814685039932,33.8969505670841));
#70417=CARTESIAN_POINT('',(31.5861090124437,-2.22967153707895,33.8637293696319));
#70418=CARTESIAN_POINT('Origin',(30.,-1.32966554433622E-14,33.8637293696319));
#70419=CARTESIAN_POINT('',(31.5786431309871,-2.19416546819406,33.8969505670765));
#70420=CARTESIAN_POINT('Ctrl Pts',(31.5786431309854,-2.19416546818597,33.8969505670841));
#70421=CARTESIAN_POINT('Ctrl Pts',(31.5823532724012,-2.21181007417745,33.8804609779984));
#70422=CARTESIAN_POINT('Ctrl Pts',(31.5861090124431,-2.22967153707596,33.8637293696347));
#70423=CARTESIAN_POINT('',(31.5989478108274,-2.17941325477251,33.8969505670765));
#70424=CARTESIAN_POINT('Origin',(31.5921082951429,-2.19134908471607,33.891294843835));
#70425=CARTESIAN_POINT('',(31.6304090047603,-2.1974857086706,33.8637293696319));
#70426=CARTESIAN_POINT('Ctrl Pts',(31.6304090047577,-2.19748570866908,33.8637293696347));
#70427=CARTESIAN_POINT('Ctrl Pts',(31.6145823315769,-2.18839429204867,33.8804609779984));
#70428=CARTESIAN_POINT('Ctrl Pts',(31.5989478108202,-2.1794132547684,33.8969505670841));
#70429=CARTESIAN_POINT('',(31.7561575802648,-2.09835352500328,33.8637293696319));
#70430=CARTESIAN_POINT('Origin',(30.,-1.32966554433622E-14,33.8637293696319));
#70431=CARTESIAN_POINT('',(31.7459289395715,-2.0635426757871,33.8969505670765));
#70432=CARTESIAN_POINT('Ctrl Pts',(31.7459289395692,-2.06354267577917,33.8969505670841));
#70433=CARTESIAN_POINT('Ctrl Pts',(31.7510120236878,-2.08084179499847,33.8804609779983));
#70434=CARTESIAN_POINT('Ctrl Pts',(31.7561575802639,-2.09835352500035,33.8637293696347));
#70435=CARTESIAN_POINT('',(31.7650135815352,-2.04724285169692,33.8969505670765));
#70436=CARTESIAN_POINT('Origin',(31.7591315960217,-2.05967847590834,33.8912948941586));
#70437=CARTESIAN_POINT('',(31.7977957394973,-2.06279117742452,33.8637293696319));
#70438=CARTESIAN_POINT('Ctrl Pts',(31.7977957394945,-2.06279117742322,33.8637293696347));
#70439=CARTESIAN_POINT('Ctrl Pts',(31.7813045503384,-2.05496953307228,33.8804609779984));
#70440=CARTESIAN_POINT('Ctrl Pts',(31.7650135815277,-2.04724285169338,33.8969505670841));
#70441=CARTESIAN_POINT('',(31.9153788526219,-1.9540984656726,33.8637293696319));
#70442=CARTESIAN_POINT('Origin',(30.,-1.32966554433622E-14,33.8637293696319));
#70443=CARTESIAN_POINT('',(31.9024505156632,-1.92019745658634,33.8969505670765));
#70444=CARTESIAN_POINT('Ctrl Pts',(31.9024505156603,-1.92019745657863,33.8969505670841));
#70445=CARTESIAN_POINT('Ctrl Pts',(31.9088752035777,-1.93704443420321,33.8804609779984));
#70446=CARTESIAN_POINT('Ctrl Pts',(31.9153788526208,-1.95409846566976,33.8637293696347));
#70447=CARTESIAN_POINT('',(31.9201974565863,-1.90245051566327,33.8969505670765));
#70448=CARTESIAN_POINT('Origin',(31.9153092670123,-1.91530927561705,33.891294933562));
#70449=CARTESIAN_POINT('',(31.9540984656725,-1.91537885262194,33.8637293696319));
#70450=CARTESIAN_POINT('Ctrl Pts',(31.9540984656697,-1.91537885262084,33.8637293696347));
#70451=CARTESIAN_POINT('Ctrl Pts',(31.9370444342032,-1.90887520357777,33.8804609779984));
#70452=CARTESIAN_POINT('Ctrl Pts',(31.9201974565786,-1.90245051566033,33.8969505670841));
#70453=CARTESIAN_POINT('',(32.0627911774245,-1.79779573949737,33.8637293696319));
#70454=CARTESIAN_POINT('Origin',(30.,-1.32966554433622E-14,33.8637293696319));
#70455=CARTESIAN_POINT('',(32.0472428516969,-1.76501358153528,33.8969505670765));
#70456=CARTESIAN_POINT('Ctrl Pts',(32.0472428516934,-1.76501358152781,33.8969505670841));
#70457=CARTESIAN_POINT('Ctrl Pts',(32.0549695330723,-1.78130455033843,33.8804609779983));
#70458=CARTESIAN_POINT('Ctrl Pts',(32.0627911774232,-1.7977957394946,33.8637293696347));
#70459=CARTESIAN_POINT('',(32.063542675787,-1.74592893957158,33.8969505670765));
#70460=CARTESIAN_POINT('Origin',(32.0596784217459,-1.75913156587025,33.8912949636253));
#70461=CARTESIAN_POINT('',(32.0983535250032,-1.75615758026484,33.8637293696319));
#70462=CARTESIAN_POINT('Ctrl Pts',(32.0983535250003,-1.75615758026399,33.8637293696347));
#70463=CARTESIAN_POINT('Ctrl Pts',(32.0808417949984,-1.75101202368781,33.8804609779984));
#70464=CARTESIAN_POINT('Ctrl Pts',(32.0635426757791,-1.74592893956926,33.8969505670841));
#70465=CARTESIAN_POINT('',(32.1974857086705,-1.63040900476039,33.8637293696319));
#70466=CARTESIAN_POINT('Origin',(30.,-1.32966554433622E-14,33.8637293696319));
#70467=CARTESIAN_POINT('',(32.1794132547725,-1.59894781082747,33.8969505670765));
#70468=CARTESIAN_POINT('Ctrl Pts',(32.1794132547683,-1.59894781082035,33.8969505670841));
#70469=CARTESIAN_POINT('Ctrl Pts',(32.1883942920486,-1.61458233157699,33.8804609779984));
#70470=CARTESIAN_POINT('Ctrl Pts',(32.197485708669,-1.63040900475776,33.8637293696347));
#70471=CARTESIAN_POINT('',(32.194165468194,-1.57864313098713,33.8969505670765));
#70472=CARTESIAN_POINT('Origin',(32.1913489771416,-1.59210823242541,33.8912949854673));
#70473=CARTESIAN_POINT('',(32.2296715370789,-1.58610901244375,33.8637293696319));
#70474=CARTESIAN_POINT('Ctrl Pts',(32.2296715370759,-1.58610901244313,33.8637293696347));
#70475=CARTESIAN_POINT('Ctrl Pts',(32.2118100741774,-1.58235327240121,33.8804609779984));
#70476=CARTESIAN_POINT('Ctrl Pts',(32.1941654681859,-1.57864313098543,33.8969505670841));
#70477=CARTESIAN_POINT('',(32.3186320097845,-1.45297025634306,33.8637293696319));
#70478=CARTESIAN_POINT('Origin',(30.,-1.32966554433622E-14,33.8637293696319));
#70479=CARTESIAN_POINT('',(32.2981468504039,-1.42302399516182,33.8969505670765));
#70480=CARTESIAN_POINT('Ctrl Pts',(32.2981468503993,-1.42302399515499,33.8969505670841));
#70481=CARTESIAN_POINT('Ctrl Pts',(32.3083268724996,-1.4379056758382,33.8804609779984));
#70482=CARTESIAN_POINT('Ctrl Pts',(32.3186320097828,-1.45297025634053,33.8637293696347));
#70483=CARTESIAN_POINT('',(32.3112605008555,-1.40162446254804,33.8969505670765));
#70484=CARTESIAN_POINT('Origin',(32.3095091411127,-1.41526902814879,33.891294999854));
#70485=CARTESIAN_POINT('',(32.3472428826875,-1.40628155512619,33.8637293696319));
#70486=CARTESIAN_POINT('Ctrl Pts',(32.3472428826845,-1.4062815551258,33.8637293696347));
#70487=CARTESIAN_POINT('Ctrl Pts',(32.3291418087476,-1.4039387870044,33.8804609779983));
#70488=CARTESIAN_POINT('Ctrl Pts',(32.3112605008473,-1.40162446254698,33.8969505670841));
#70489=CARTESIAN_POINT('',(32.4254831735348,-1.26657346313373,33.8637293696319));
#70490=CARTESIAN_POINT('Origin',(30.,-1.32966554433622E-14,33.8637293696319));
#70491=CARTESIAN_POINT('',(32.4027116064913,-1.2383267633625,33.8969505670765));
#70492=CARTESIAN_POINT('Ctrl Pts',(32.4027116064861,-1.23832676335608,33.8969505670841));
#70493=CARTESIAN_POINT('Ctrl Pts',(32.414027850185,-1.25236385345577,33.8804609779983));
#70494=CARTESIAN_POINT('Ctrl Pts',(32.4254831735329,-1.26657346313137,33.8637293696347));
#70495=CARTESIAN_POINT('',(32.4141058439571,-1.21596431320991,33.8969505670765));
#70496=CARTESIAN_POINT('Origin',(32.4134304175703,-1.22970422416536,33.8912950072666));
#70497=CARTESIAN_POINT('',(32.4503426953868,-1.21778390438519,33.8637293696319));
#70498=CARTESIAN_POINT('Ctrl Pts',(32.4503426953838,-1.21778390438504,33.8637293696347));
#70499=CARTESIAN_POINT('Ctrl Pts',(32.4321136095486,-1.21686855212869,33.8804609779984));
#70500=CARTESIAN_POINT('Ctrl Pts',(32.4141058439489,-1.2159643132095,33.8969505670841));
#70501=CARTESIAN_POINT('',(32.5173804269652,-1.07236782334576,33.8637293696319));
#70502=CARTESIAN_POINT('Origin',(30.,-1.32966554433622E-14,33.8637293696319));
#70503=CARTESIAN_POINT('',(32.492462846542,-1.0459948352816,33.8969505670765));
#70504=CARTESIAN_POINT('Ctrl Pts',(32.4924628465363,-1.04599483527564,33.8969505670841));
#70505=CARTESIAN_POINT('Ctrl Pts',(32.5048455434283,-1.05910079146353,33.8804609779984));
#70506=CARTESIAN_POINT('Ctrl Pts',(32.5173804269631,-1.07236782334356,33.8637293696347));
#70507=CARTESIAN_POINT('',(32.5020674217591,-1.02280733953168,33.8969505670765));
#70508=CARTESIAN_POINT('Origin',(32.5024720978725,-1.03655788791108,33.8912950079413));
#70509=CARTESIAN_POINT('',(32.5383353305474,-1.02177821091943,33.8637293696319));
#70510=CARTESIAN_POINT('Ctrl Pts',(32.5383353305444,-1.02177821091952,33.8637293696347));
#70511=CARTESIAN_POINT('Ctrl Pts',(32.5200906211869,-1.02229591797926,33.8804609779983));
#70512=CARTESIAN_POINT('Ctrl Pts',(32.5020674217508,-1.02280733953191,33.8969505670841));
#70513=CARTESIAN_POINT('',(32.5937571929495,-0.871550679328387,33.8637293696319));
#70514=CARTESIAN_POINT('Origin',(30.,-1.32966554433622E-14,33.8637293696319));
#70515=CARTESIAN_POINT('',(32.5668472243157,-0.847214001212625,33.8969505670765));
#70516=CARTESIAN_POINT('Ctrl Pts',(32.5668472243096,-0.847214001207098,
33.8969505670841));
#70517=CARTESIAN_POINT('Ctrl Pts',(32.5802200309508,-0.859308020905142,
33.8804609779983));
#70518=CARTESIAN_POINT('Ctrl Pts',(32.5937571929472,-0.871550679326345,
33.8637293696347));
#70519=CARTESIAN_POINT('',(32.574602921884,-0.823344418487278,33.8969505670765));
#70520=CARTESIAN_POINT('Origin',(32.5760852110325,-0.837020829522246,33.8912950018862));
#70521=CARTESIAN_POINT('',(32.6106782843131,-0.819472915007605,33.8637293696319));
#70522=CARTESIAN_POINT('Ctrl Pts',(32.6106782843101,-0.819472915007929,
33.8637293696347));
#70523=CARTESIAN_POINT('Ctrl Pts',(32.5925304361305,-0.821420489547588,
33.8804609779984));
#70524=CARTESIAN_POINT('Ctrl Pts',(32.5746029218758,-0.823344418488157,
33.8969505670841));
#70525=CARTESIAN_POINT('',(32.6541425833274,-0.665360135552938,33.8637293696319));
#70526=CARTESIAN_POINT('Origin',(30.,-1.32966554433622E-14,33.8637293696319));
#70527=CARTESIAN_POINT('',(32.6254061353882,-0.643209811098926,33.8969505670765));
#70528=CARTESIAN_POINT('Ctrl Pts',(32.6254061353816,-0.643209811093906,
33.8969505670841));
#70529=CARTESIAN_POINT('Ctrl Pts',(32.6396866039721,-0.65421733064898,33.8804609779984));
#70530=CARTESIAN_POINT('Ctrl Pts',(32.654142583325,-0.665360135551083,33.8637293696347));
#70531=CARTESIAN_POINT('',(32.6312651388532,-0.6188053053131,33.8969505670765));
#70532=CARTESIAN_POINT('Origin',(32.633815908334,-0.632323260043048,33.8912949888765));
#70533=CARTESIAN_POINT('',(32.6669255383174,-0.612115296072366,33.8637293696319));
#70534=CARTESIAN_POINT('Ctrl Pts',(32.6669255383144,-0.612115296072921,
33.8637293696347));
#70535=CARTESIAN_POINT('Ctrl Pts',(32.6489864388314,-0.615480730647825,
33.8804609779983));
#70536=CARTESIAN_POINT('Ctrl Pts',(32.6312651388451,-0.618805305314621,
33.8969505670841));
#70537=CARTESIAN_POINT('',(32.6981643020872,-0.455067425287109,33.8637293696319));
#70538=CARTESIAN_POINT('Origin',(30.,-1.32966554433622E-14,33.8637293696319));
#70539=CARTESIAN_POINT('',(32.6677785445999,-0.435240018610835,33.8969505670765));
#70540=CARTESIAN_POINT('Ctrl Pts',(32.667778544593,-0.43524001860635,33.8969505670841));
#70541=CARTESIAN_POINT('Ctrl Pts',(32.6828786312952,-0.445093173000037,
33.8804609779984));
#70542=CARTESIAN_POINT('Ctrl Pts',(32.6981643020846,-0.45506742528547,33.8637293696347));
#70543=CARTESIAN_POINT('',(32.6717047312569,-0.410451051658023,33.8969505670765));
#70544=CARTESIAN_POINT('Origin',(32.6753082614924,-0.423727206709312,33.8912949684251));
#70545=CARTESIAN_POINT('',(32.7067303095351,-0.400983782787849,33.8637293696319));
#70546=CARTESIAN_POINT('Ctrl Pts',(32.7067303095322,-0.400983782788643,
33.8637293696347));
#70547=CARTESIAN_POINT('Ctrl Pts',(32.6891105592595,-0.405746328375509,
33.8804609779984));
#70548=CARTESIAN_POINT('Ctrl Pts',(32.6717047312489,-0.410451051660171,
33.8969505670841));
#70549=CARTESIAN_POINT('',(32.7255509406939,-0.241969073019109,33.8637293696319));
#70550=CARTESIAN_POINT('Origin',(30.,-1.32966554433622E-14,33.8637293696319));
#70551=CARTESIAN_POINT('',(32.6937032119577,-0.224586826676015,33.8969505670765));
#70552=CARTESIAN_POINT('Ctrl Pts',(32.6937032119505,-0.224586826672072,
33.8969505670841));
#70553=CARTESIAN_POINT('Ctrl Pts',(32.7095298197086,-0.233224867931026,
33.8804609779984));
#70554=CARTESIAN_POINT('Ctrl Pts',(32.7255509406912,-0.241969073017673,
33.8637293696347));
#70555=CARTESIAN_POINT('',(32.6956723755605,-0.199566230780649,33.8969505670765));
#70556=CARTESIAN_POINT('Origin',(32.7003064571198,-0.212518732061269,33.8912949397143));
#70557=CARTESIAN_POINT('',(32.7298471883155,-0.187380071141808,33.8637293696319));
#70558=CARTESIAN_POINT('Ctrl Pts',(32.7298471883126,-0.187380071142835,
33.8637293696347));
#70559=CARTESIAN_POINT('Ctrl Pts',(32.7126554188699,-0.19351036506442,33.8804609779983));
#70560=CARTESIAN_POINT('Ctrl Pts',(32.6956723755527,-0.199566230783424,
33.8969505670841));
#70561=CARTESIAN_POINT('',(32.7361336514135,-0.0273789009530657,33.8637293696319));
#70562=CARTESIAN_POINT('Origin',(30.,-1.32966554433622E-14,33.8637293696319));
#70563=CARTESIAN_POINT('',(32.7030203032667,-0.0125489822720396,33.8969505670765));
#70564=CARTESIAN_POINT('Ctrl Pts',(32.7030203032592,-0.0125489822686859,
33.8969505670841));
#70565=CARTESIAN_POINT('Ctrl Pts',(32.7194758557734,-0.0199186539960853,
33.8804609779984));
#70566=CARTESIAN_POINT('Ctrl Pts',(32.7361336514107,-0.0273789009518218,
33.8637293696347));
#70567=CARTESIAN_POINT('',(32.7030203032667,0.0125489822719939,33.8969505670765));
#70568=CARTESIAN_POINT('Origin',(32.7086563646857,-6.24428584025816E-9,
33.8912949140187));
#70569=CARTESIAN_POINT('',(32.7361336514135,0.0273789009530202,33.8637293696319));
#70570=CARTESIAN_POINT('Ctrl Pts',(32.7361336514108,0.027378900951751,33.8637293696347));
#70571=CARTESIAN_POINT('Ctrl Pts',(32.7194758557734,0.0199186539960142,
33.8804609779984));
#70572=CARTESIAN_POINT('Ctrl Pts',(32.7030203032592,0.0125489822686146,
33.8969505670841));
#70573=CARTESIAN_POINT('',(32.7298471883155,0.187380071141762,33.8637293696319));
#70574=CARTESIAN_POINT('Origin',(30.,-1.32966554433622E-14,33.8637293696319));
#70575=CARTESIAN_POINT('',(32.6956723755605,0.199566230780603,33.8969505670765));
#70576=CARTESIAN_POINT('Ctrl Pts',(32.6956723755527,0.199566230783364,33.8969505670841));
#70577=CARTESIAN_POINT('Ctrl Pts',(32.7126554188699,0.193510365064359,33.8804609779983));
#70578=CARTESIAN_POINT('Ctrl Pts',(32.7298471883126,0.187380071142775,33.8637293696347));
#70579=CARTESIAN_POINT('',(32.6937032119577,0.224586826675969,33.8969505670765));
#70580=CARTESIAN_POINT('Origin',(32.7003074588901,0.212518788369426,33.8912937927563));
#70581=CARTESIAN_POINT('',(32.7255509406939,0.241969073019064,33.8637293696319));
#70582=CARTESIAN_POINT('Ctrl Pts',(32.7255509406912,0.241969073017624,33.8637293696347));
#70583=CARTESIAN_POINT('Ctrl Pts',(32.7095298197086,0.233224867930978,33.8804609779984));
#70584=CARTESIAN_POINT('Ctrl Pts',(32.6937032119505,0.224586826672025,33.8969505670841));
#70585=CARTESIAN_POINT('',(32.7067303095351,0.400983782787804,33.8637293696319));
#70586=CARTESIAN_POINT('Origin',(30.,-1.32966554433622E-14,33.8637293696319));
#70587=CARTESIAN_POINT('',(32.6717047312569,0.410451051657977,33.8969505670765));
#70588=CARTESIAN_POINT('Ctrl Pts',(32.6717047312489,0.410451051660138,33.8969505670841));
#70589=CARTESIAN_POINT('Ctrl Pts',(32.6891105592595,0.405746328375475,33.8804609779984));
#70590=CARTESIAN_POINT('Ctrl Pts',(32.7067303095322,0.400983782788608,33.8637293696347));
#70591=CARTESIAN_POINT('',(32.6677785445999,0.435240018610789,33.8969505670765));
#70592=CARTESIAN_POINT('Origin',(32.6753090233822,0.423727307748461,33.8912940899386));
#70593=CARTESIAN_POINT('',(32.6981643020872,0.455067425287063,33.8637293696319));
#70594=CARTESIAN_POINT('Ctrl Pts',(32.6981643020846,0.455067425285395,33.8637293696347));
#70595=CARTESIAN_POINT('Ctrl Pts',(32.6828786312952,0.445093172999962,33.8804609779983));
#70596=CARTESIAN_POINT('Ctrl Pts',(32.667778544593,0.435240018606276,33.8969505670841));
#70597=CARTESIAN_POINT('',(32.6669255383174,0.61211529607232,33.8637293696319));
#70598=CARTESIAN_POINT('Origin',(30.,-1.32966554433622E-14,33.8637293696319));
#70599=CARTESIAN_POINT('',(32.6312651388532,0.618805305313054,33.8969505670765));
#70600=CARTESIAN_POINT('Ctrl Pts',(32.6312651388451,0.618805305314574,33.8969505670841));
#70601=CARTESIAN_POINT('Ctrl Pts',(32.6489864388314,0.615480730647778,33.8804609779983));
#70602=CARTESIAN_POINT('Ctrl Pts',(32.6669255383144,0.612115296072874,33.8637293696347));
#70603=CARTESIAN_POINT('',(32.6254061353882,0.64320981109888,33.8969505670765));
#70604=CARTESIAN_POINT('Origin',(32.6338164916465,0.632323382398585,33.8912943077151));
#70605=CARTESIAN_POINT('',(32.6541425833274,0.665360135552893,33.8637293696319));
#70606=CARTESIAN_POINT('Ctrl Pts',(32.654142583325,0.665360135551018,33.8637293696347));
#70607=CARTESIAN_POINT('Ctrl Pts',(32.6396866039721,0.654217330648915,33.8804609779984));
#70608=CARTESIAN_POINT('Ctrl Pts',(32.6254061353817,0.643209811093841,33.8969505670841));
#70609=CARTESIAN_POINT('',(32.6106782843131,0.81947291500756,33.8637293696319));
#70610=CARTESIAN_POINT('Origin',(30.,-1.32966554433622E-14,33.8637293696319));
#70611=CARTESIAN_POINT('',(32.574602921884,0.823344418487232,33.8969505670765));
#70612=CARTESIAN_POINT('Ctrl Pts',(32.5746029218758,0.823344418488117,33.8969505670841));
#70613=CARTESIAN_POINT('Ctrl Pts',(32.5925304361305,0.821420489547548,33.8804609779984));
#70614=CARTESIAN_POINT('Ctrl Pts',(32.6106782843101,0.819472915007888,33.8637293696347));
#70615=CARTESIAN_POINT('',(32.5668472243157,0.84721400121258,33.8969505670765));
#70616=CARTESIAN_POINT('Origin',(32.5760856561636,0.83702095775897,33.891294472568));
#70617=CARTESIAN_POINT('',(32.5937571929495,0.871550679328342,33.8637293696319));
#70618=CARTESIAN_POINT('Ctrl Pts',(32.5937571929473,0.871550679326287,33.8637293696347));
#70619=CARTESIAN_POINT('Ctrl Pts',(32.5802200309508,0.859308020905083,33.8804609779984));
#70620=CARTESIAN_POINT('Ctrl Pts',(32.5668472243096,0.847214001207037,33.8969505670841));
#70621=CARTESIAN_POINT('',(32.5383353305474,1.02177821091938,33.8637293696319));
#70622=CARTESIAN_POINT('Origin',(30.,-1.32966554433622E-14,33.8637293696319));
#70623=CARTESIAN_POINT('',(32.5020674217591,1.02280733953163,33.8969505670765));
#70624=CARTESIAN_POINT('Ctrl Pts',(32.5020674217508,1.02280733953187,33.8969505670841));
#70625=CARTESIAN_POINT('Ctrl Pts',(32.520090621187,1.02229591797922,33.8804609779984));
#70626=CARTESIAN_POINT('Ctrl Pts',(32.5383353305444,1.02177821091947,33.8637293696347));
#70627=CARTESIAN_POINT('',(32.492462846542,1.04599483528156,33.8969505670765));
#70628=CARTESIAN_POINT('Origin',(32.5024724328509,1.03655801106889,33.8912946002427));
#70629=CARTESIAN_POINT('',(32.5173804269653,1.07236782334572,33.8637293696319));
#70630=CARTESIAN_POINT('Ctrl Pts',(32.5173804269632,1.0723678233435,33.8637293696347));
#70631=CARTESIAN_POINT('Ctrl Pts',(32.5048455434284,1.05910079146346,33.8804609779983));
#70632=CARTESIAN_POINT('Ctrl Pts',(32.4924628465363,1.04599483527555,33.8969505670841));
#70633=CARTESIAN_POINT('',(32.4503426953868,1.21778390438515,33.8637293696319));
#70634=CARTESIAN_POINT('Origin',(30.,-1.32966554433622E-14,33.8637293696319));
#70635=CARTESIAN_POINT('',(32.4141058439571,1.21596431320987,33.8969505670765));
#70636=CARTESIAN_POINT('Ctrl Pts',(32.4141058439489,1.21596431320946,33.8969505670841));
#70637=CARTESIAN_POINT('Ctrl Pts',(32.4321136095487,1.21686855212866,33.8804609779984));
#70638=CARTESIAN_POINT('Ctrl Pts',(32.4503426953838,1.217783904385,33.8637293696347));
#70639=CARTESIAN_POINT('',(32.4027116064913,1.23832676336245,33.8969505670765));
#70640=CARTESIAN_POINT('Origin',(32.4134306626749,1.22970433386022,33.891294700665));
#70641=CARTESIAN_POINT('',(32.4254831735348,1.26657346313369,33.8637293696319));
#70642=CARTESIAN_POINT('Ctrl Pts',(32.4254831735329,1.26657346313132,33.8637293696347));
#70643=CARTESIAN_POINT('Ctrl Pts',(32.414027850185,1.25236385345572,33.8804609779984));
#70644=CARTESIAN_POINT('Ctrl Pts',(32.4027116064861,1.23832676335603,33.8969505670841));
#70645=CARTESIAN_POINT('',(32.3472428826875,1.40628155512614,33.8637293696319));
#70646=CARTESIAN_POINT('Origin',(30.,-1.32966554433622E-14,33.8637293696319));
#70647=CARTESIAN_POINT('',(32.3112605008555,1.401624462548,33.8969505670765));
#70648=CARTESIAN_POINT('Ctrl Pts',(32.3112605008473,1.40162446254694,33.8969505670841));
#70649=CARTESIAN_POINT('Ctrl Pts',(32.3291418087476,1.40393878700437,33.8804609779984));
#70650=CARTESIAN_POINT('Ctrl Pts',(32.3472428826845,1.40628155512576,33.8637293696347));
#70651=CARTESIAN_POINT('',(32.298146850404,1.42302399516178,33.8969505670765));
#70652=CARTESIAN_POINT('Origin',(32.3095093115547,1.41526911745259,33.8912947803757));
#70653=CARTESIAN_POINT('',(32.3186320097845,1.45297025634302,33.8637293696319));
#70654=CARTESIAN_POINT('Ctrl Pts',(32.3186320097828,1.45297025634046,33.8637293696347));
#70655=CARTESIAN_POINT('Ctrl Pts',(32.3083268724996,1.43790567583815,33.8804609779983));
#70656=CARTESIAN_POINT('Ctrl Pts',(32.2981468503993,1.42302399515495,33.8969505670841));
#70657=CARTESIAN_POINT('',(32.2296715370789,1.58610901244371,33.8637293696319));
#70658=CARTESIAN_POINT('Origin',(30.,-1.32966554433622E-14,33.8637293696319));
#70659=CARTESIAN_POINT('',(32.194165468194,1.57864313098709,33.8969505670765));
#70660=CARTESIAN_POINT('Ctrl Pts',(32.1941654681859,1.57864313098539,33.8969505670841));
#70661=CARTESIAN_POINT('Ctrl Pts',(32.2118100741774,1.58235327240116,33.8804609779984));
#70662=CARTESIAN_POINT('Ctrl Pts',(32.2296715370759,1.58610901244308,33.8637293696347));
#70663=CARTESIAN_POINT('',(32.1794132547725,1.59894781082743,33.8969505670765));
#70664=CARTESIAN_POINT('Origin',(32.191349084716,1.59210829514292,33.891294843835));
#70665=CARTESIAN_POINT('',(32.1974857086706,1.63040900476035,33.8637293696319));
#70666=CARTESIAN_POINT('Ctrl Pts',(32.1974857086691,1.6304090047577,33.8637293696347));
#70667=CARTESIAN_POINT('Ctrl Pts',(32.1883942920486,1.61458233157692,33.8804609779983));
#70668=CARTESIAN_POINT('Ctrl Pts',(32.1794132547684,1.59894781082026,33.8969505670841));
#70669=CARTESIAN_POINT('',(32.0983535250032,1.7561575802648,33.8637293696319));
#70670=CARTESIAN_POINT('Origin',(30.,-1.32966554433622E-14,33.8637293696319));
#70671=CARTESIAN_POINT('',(32.0635426757871,1.74592893957153,33.8969505670765));
#70672=CARTESIAN_POINT('Ctrl Pts',(32.0635426757792,1.74592893956921,33.8969505670841));
#70673=CARTESIAN_POINT('Ctrl Pts',(32.0808417949984,1.75101202368776,33.8804609779983));
#70674=CARTESIAN_POINT('Ctrl Pts',(32.0983535250003,1.75615758026393,33.8637293696347));
#70675=CARTESIAN_POINT('',(32.0472428516969,1.76501358153524,33.8969505670765));
#70676=CARTESIAN_POINT('Origin',(32.0596784759083,1.75913159602166,33.8912948941586));
#70677=CARTESIAN_POINT('',(32.0627911774245,1.79779573949733,33.8637293696319));
#70678=CARTESIAN_POINT('Ctrl Pts',(32.0627911774232,1.79779573949457,33.8637293696347));
#70679=CARTESIAN_POINT('Ctrl Pts',(32.0549695330723,1.78130455033839,33.8804609779984));
#70680=CARTESIAN_POINT('Ctrl Pts',(32.0472428516934,1.76501358152777,33.8969505670841));
#70681=CARTESIAN_POINT('',(31.9540984656726,1.9153788526219,33.8637293696319));
#70682=CARTESIAN_POINT('Origin',(30.,-1.32966554433622E-14,33.8637293696319));
#70683=CARTESIAN_POINT('',(31.9201974565863,1.90245051566323,33.8969505670765));
#70684=CARTESIAN_POINT('Ctrl Pts',(31.9201974565786,1.90245051566028,33.8969505670841));
#70685=CARTESIAN_POINT('Ctrl Pts',(31.9370444342032,1.90887520357773,33.8804609779983));
#70686=CARTESIAN_POINT('Ctrl Pts',(31.9540984656697,1.91537885262081,33.8637293696347));
#70687=CARTESIAN_POINT('',(31.9024505156632,1.9201974565863,33.8969505670765));
#70688=CARTESIAN_POINT('Origin',(31.915309275617,1.91530926701235,33.891294933562));
#70689=CARTESIAN_POINT('',(31.9153788526219,1.95409846567256,33.8637293696319));
#70690=CARTESIAN_POINT('Ctrl Pts',(31.9153788526208,1.95409846566973,33.8637293696347));
#70691=CARTESIAN_POINT('Ctrl Pts',(31.9088752035777,1.93704443420319,33.8804609779984));
#70692=CARTESIAN_POINT('Ctrl Pts',(31.9024505156603,1.9201974565786,33.8969505670841));
#70693=CARTESIAN_POINT('',(31.7977957394973,2.06279117742448,33.8637293696319));
#70694=CARTESIAN_POINT('Origin',(30.,-1.32966554433622E-14,33.8637293696319));
#70695=CARTESIAN_POINT('',(31.7650135815352,2.04724285169688,33.8969505670765));
#70696=CARTESIAN_POINT('Ctrl Pts',(31.7650135815278,2.04724285169333,33.8969505670841));
#70697=CARTESIAN_POINT('Ctrl Pts',(31.7813045503384,2.05496953307223,33.8804609779984));
#70698=CARTESIAN_POINT('Ctrl Pts',(31.7977957394946,2.06279117742316,33.8637293696347));
#70699=CARTESIAN_POINT('',(31.7459289395715,2.06354267578706,33.8969505670765));
#70700=CARTESIAN_POINT('Origin',(31.7591315658702,2.05967842174595,33.8912949636253));
#70701=CARTESIAN_POINT('',(31.7561575802648,2.09835352500324,33.8637293696319));
#70702=CARTESIAN_POINT('Ctrl Pts',(31.7561575802639,2.09835352500033,33.8637293696347));
#70703=CARTESIAN_POINT('Ctrl Pts',(31.7510120236877,2.08084179499845,33.8804609779984));
#70704=CARTESIAN_POINT('Ctrl Pts',(31.7459289395692,2.06354267577915,33.8969505670841));
#70705=CARTESIAN_POINT('',(31.6304090047604,2.19748570867057,33.8637293696319));
#70706=CARTESIAN_POINT('Origin',(30.,-1.32966554433622E-14,33.8637293696319));
#70707=CARTESIAN_POINT('',(31.5989478108274,2.17941325477248,33.8969505670765));
#70708=CARTESIAN_POINT('Ctrl Pts',(31.5989478108202,2.17941325476838,33.8969505670841));
#70709=CARTESIAN_POINT('Ctrl Pts',(31.6145823315769,2.18839429204865,33.8804609779983));
#70710=CARTESIAN_POINT('Ctrl Pts',(31.6304090047577,2.19748570866908,33.8637293696347));
#70711=CARTESIAN_POINT('',(31.5786431309871,2.19416546819402,33.8969505670765));
#70712=CARTESIAN_POINT('Origin',(31.5921082324254,2.19134897714166,33.8912949854673));
#70713=CARTESIAN_POINT('',(31.5861090124437,2.22967153707891,33.8637293696319));
#70714=CARTESIAN_POINT('Ctrl Pts',(31.5861090124431,2.22967153707593,33.8637293696347));
#70715=CARTESIAN_POINT('Ctrl Pts',(31.5823532724012,2.21181007417742,33.8804609779984));
#70716=CARTESIAN_POINT('Ctrl Pts',(31.5786431309854,2.19416546818594,33.8969505670841));
#70717=CARTESIAN_POINT('',(31.452970256343,2.31863200978455,33.8637293696319));
#70718=CARTESIAN_POINT('Origin',(30.,-1.32966554433622E-14,33.8637293696319));
#70719=CARTESIAN_POINT('',(31.4230239951618,2.29814685040396,33.8969505670765));
#70720=CARTESIAN_POINT('Ctrl Pts',(31.423023995155,2.29814685039929,33.8969505670841));
#70721=CARTESIAN_POINT('Ctrl Pts',(31.4379056758382,2.30832687249959,33.8804609779983));
#70722=CARTESIAN_POINT('Ctrl Pts',(31.4529702563405,2.31863200978281,33.8637293696347));
#70723=CARTESIAN_POINT('',(31.401624462548,2.3112605008555,33.8969505670765));
#70724=CARTESIAN_POINT('Origin',(31.4152690281487,2.30950914111275,33.891294999854));
#70725=CARTESIAN_POINT('',(31.4062815551261,2.34724288268748,33.8637293696319));
#70726=CARTESIAN_POINT('Ctrl Pts',(31.4062815551258,2.34724288268445,33.8637293696347));
#70727=CARTESIAN_POINT('Ctrl Pts',(31.4039387870044,2.32914180874762,33.8804609779983));
#70728=CARTESIAN_POINT('Ctrl Pts',(31.4016244625469,2.31126050084732,33.8969505670841));
#70729=CARTESIAN_POINT('',(31.2665734631337,2.42548317353483,33.8637293696319));
#70730=CARTESIAN_POINT('Origin',(30.,-1.32966554433622E-14,33.8637293696319));
#70731=CARTESIAN_POINT('',(31.2383267633625,2.40271160649132,33.8969505670765));
#70732=CARTESIAN_POINT('Ctrl Pts',(31.2383267633561,2.40271160648613,33.8969505670841));
#70733=CARTESIAN_POINT('Ctrl Pts',(31.2523638534557,2.41402785018503,33.8804609779983));
#70734=CARTESIAN_POINT('Ctrl Pts',(31.2665734631313,2.4254831735329,33.8637293696347));
#70735=CARTESIAN_POINT('',(31.2159643132099,2.41410584395711,33.8969505670765));
#70736=CARTESIAN_POINT('Origin',(31.2297042241653,2.41343041757031,33.8912950072666));
#70737=CARTESIAN_POINT('',(31.2177839043851,2.45034269538681,33.8637293696319));
#70738=CARTESIAN_POINT('Ctrl Pts',(31.217783904385,2.45034269538375,33.8637293696347));
#70739=CARTESIAN_POINT('Ctrl Pts',(31.2168685521287,2.43211360954864,33.8804609779984));
#70740=CARTESIAN_POINT('Ctrl Pts',(31.2159643132095,2.41410584394886,33.8969505670841));
#70741=CARTESIAN_POINT('',(31.0723678233457,2.51738042696526,33.8637293696319));
#70742=CARTESIAN_POINT('Origin',(30.,-1.32966554433622E-14,33.8637293696319));
#70743=CARTESIAN_POINT('',(31.0459948352816,2.49246284654197,33.8969505670765));
#70744=CARTESIAN_POINT('Ctrl Pts',(31.0459948352756,2.4924628465363,33.8969505670841));
#70745=CARTESIAN_POINT('Ctrl Pts',(31.0591007914635,2.50484554342835,33.8804609779983));
#70746=CARTESIAN_POINT('Ctrl Pts',(31.0723678233435,2.51738042696315,33.8637293696347));
#70747=CARTESIAN_POINT('',(31.0228073395316,2.50206742175906,33.8969505670765));
#70748=CARTESIAN_POINT('Origin',(31.036557887911,2.50247209787251,33.8912950079413));
#70749=CARTESIAN_POINT('',(31.0217782109194,2.53833533054745,33.8637293696319));
#70750=CARTESIAN_POINT('Ctrl Pts',(31.0217782109194,2.5383353305444,33.8637293696347));
#70751=CARTESIAN_POINT('Ctrl Pts',(31.0222959179792,2.52009062118696,33.8804609779984));
#70752=CARTESIAN_POINT('Ctrl Pts',(31.0228073395318,2.50206742175081,33.8969505670841));
#70753=CARTESIAN_POINT('',(30.8715506793283,2.59375719294951,33.8637293696319));
#70754=CARTESIAN_POINT('Origin',(30.,-1.32966554433622E-14,33.8637293696319));
#70755=CARTESIAN_POINT('',(30.8472140012126,2.5668472243157,33.8969505670765));
#70756=CARTESIAN_POINT('Ctrl Pts',(30.847214001207,2.56684722430959,33.8969505670841));
#70757=CARTESIAN_POINT('Ctrl Pts',(30.8593080209051,2.58022003095078,33.8804609779984));
#70758=CARTESIAN_POINT('Ctrl Pts',(30.8715506793263,2.59375719294725,33.8637293696347));
#70759=CARTESIAN_POINT('',(30.8233444184872,2.57460292188402,33.8969505670765));
#70760=CARTESIAN_POINT('Origin',(30.8370208295222,2.57608521103255,33.8912950018862));
#70761=CARTESIAN_POINT('',(30.8194729150076,2.61067828431311,33.8637293696319));
#70762=CARTESIAN_POINT('Ctrl Pts',(30.8194729150079,2.61067828431008,33.8637293696347));
#70763=CARTESIAN_POINT('Ctrl Pts',(30.8214204895475,2.59253043613048,33.8804609779984));
#70764=CARTESIAN_POINT('Ctrl Pts',(30.8233444184881,2.57460292187581,33.8969505670841));
#70765=CARTESIAN_POINT('',(30.6653601355529,2.65414258332745,33.8637293696319));
#70766=CARTESIAN_POINT('Origin',(30.,-1.32966554433622E-14,33.8637293696319));
#70767=CARTESIAN_POINT('',(30.6432098110989,2.62540613538819,33.8969505670765));
#70768=CARTESIAN_POINT('Ctrl Pts',(30.6432098110938,2.62540613538167,33.8969505670841));
#70769=CARTESIAN_POINT('Ctrl Pts',(30.6542173306489,2.63968660397217,33.8804609779983));
#70770=CARTESIAN_POINT('Ctrl Pts',(30.665360135551,2.65414258332504,33.8637293696347));
#70771=CARTESIAN_POINT('',(30.6188053053131,2.63126513885322,33.8969505670765));
#70772=CARTESIAN_POINT('Origin',(30.632323260043,2.633815908334,33.8912949888765));
#70773=CARTESIAN_POINT('',(30.6121152960723,2.66692553831736,33.8637293696319));
#70774=CARTESIAN_POINT('Ctrl Pts',(30.6121152960729,2.66692553831437,33.8637293696347));
#70775=CARTESIAN_POINT('Ctrl Pts',(30.6154807306478,2.6489864388314,33.8804609779983));
#70776=CARTESIAN_POINT('Ctrl Pts',(30.6188053053146,2.63126513884509,33.8969505670841));
#70777=CARTESIAN_POINT('',(30.4550674252871,2.69816430208719,33.8637293696319));
#70778=CARTESIAN_POINT('Origin',(30.,-1.32966554433622E-14,33.8637293696319));
#70779=CARTESIAN_POINT('',(30.4352400186108,2.66777854459989,33.8969505670765));
#70780=CARTESIAN_POINT('Ctrl Pts',(30.4352400186063,2.66777854459299,33.8969505670841));
#70781=CARTESIAN_POINT('Ctrl Pts',(30.4450931729999,2.68287863129519,33.8804609779983));
#70782=CARTESIAN_POINT('Ctrl Pts',(30.4550674252854,2.69816430208465,33.8637293696347));
#70783=CARTESIAN_POINT('',(30.410451051658,2.67170473125694,33.8969505670765));
#70784=CARTESIAN_POINT('Origin',(30.4237272067093,2.67530826149246,33.891294968425));
#70785=CARTESIAN_POINT('',(30.4009837827878,2.70673030953515,33.8637293696319));
#70786=CARTESIAN_POINT('Ctrl Pts',(30.4009837827886,2.7067303095322,33.8637293696347));
#70787=CARTESIAN_POINT('Ctrl Pts',(30.4057463283755,2.68911055925956,33.8804609779984));
#70788=CARTESIAN_POINT('Ctrl Pts',(30.4104510516602,2.67170473124897,33.8969505670841));
#70789=CARTESIAN_POINT('',(30.2419690730191,2.72555094069389,33.8637293696319));
#70790=CARTESIAN_POINT('Origin',(30.,-1.32966554433622E-14,33.8637293696319));
#70791=CARTESIAN_POINT('',(30.224586826676,2.69370321195774,33.8969505670765));
#70792=CARTESIAN_POINT('Ctrl Pts',(30.224586826672,2.6937032119505,33.8969505670841));
#70793=CARTESIAN_POINT('Ctrl Pts',(30.233224867931,2.70952981970859,33.8804609779983));
#70794=CARTESIAN_POINT('Ctrl Pts',(30.2419690730176,2.72555094069122,33.8637293696347));
#70795=CARTESIAN_POINT('',(30.1995662307806,2.69567237556048,33.8969505670765));
#70796=CARTESIAN_POINT('Origin',(30.2125187320612,2.70030645711979,33.8912949397143));
#70797=CARTESIAN_POINT('',(30.1873800711418,2.72984718831549,33.8637293696319));
#70798=CARTESIAN_POINT('Ctrl Pts',(30.1873800711428,2.7298471883126,33.8637293696347));
#70799=CARTESIAN_POINT('Ctrl Pts',(30.1935103650644,2.71265541886987,33.8804609779983));
#70800=CARTESIAN_POINT('Ctrl Pts',(30.1995662307834,2.6956723755527,33.8969505670841));
#70801=CARTESIAN_POINT('',(30.027378900953,2.73613365141356,33.8637293696319));
#70802=CARTESIAN_POINT('Origin',(30.,-1.32966554433622E-14,33.8637293696319));
#70803=CARTESIAN_POINT('',(30.012548982272,2.70302030326666,33.8969505670765));
#70804=CARTESIAN_POINT('Ctrl Pts',(30.0125489822686,2.70302030325912,33.8969505670841));
#70805=CARTESIAN_POINT('Ctrl Pts',(30.019918653996,2.71947585577339,33.8804609779983));
#70806=CARTESIAN_POINT('Ctrl Pts',(30.0273789009518,2.73613365141076,33.8637293696347));
#70807=CARTESIAN_POINT('',(29.987451017728,2.70302030326666,33.8969505670765));
#70808=CARTESIAN_POINT('Origin',(30.,2.70866577951602,33.891284862925));
#70809=CARTESIAN_POINT('',(29.9726210990469,2.73613365141356,33.8637293696319));
#70810=CARTESIAN_POINT('Ctrl Pts',(29.9726210990482,2.73613365141079,33.8637293696347));
#70811=CARTESIAN_POINT('Ctrl Pts',(29.980081346004,2.7194758557734,33.8804609779983));
#70812=CARTESIAN_POINT('Ctrl Pts',(29.9874510177314,2.70302030325912,33.8969505670841));
#70813=CARTESIAN_POINT('',(29.8126199288582,2.72984718831549,33.8637293696319));
#70814=CARTESIAN_POINT('Origin',(30.,-1.32966554433622E-14,33.8637293696319));
#70815=CARTESIAN_POINT('',(29.8004337692194,2.69567237556048,33.8969505670765));
#70816=CARTESIAN_POINT('Ctrl Pts',(29.8004337692166,2.6956723755527,33.8969505670841));
#70817=CARTESIAN_POINT('Ctrl Pts',(29.8064896349356,2.71265541886987,33.8804609779983));
#70818=CARTESIAN_POINT('Ctrl Pts',(29.8126199288572,2.7298471883126,33.8637293696347));
#70819=CARTESIAN_POINT('',(29.775413173324,2.69370321195775,33.8969505670765));
#70820=CARTESIAN_POINT('Origin',(29.7874812116306,2.70030745889017,33.8912937927563));
#70821=CARTESIAN_POINT('',(29.7580309269809,2.72555094069389,33.8637293696319));
#70822=CARTESIAN_POINT('Ctrl Pts',(29.7580309269824,2.72555094069121,33.8637293696347));
#70823=CARTESIAN_POINT('Ctrl Pts',(29.766775132069,2.70952981970858,33.8804609779983));
#70824=CARTESIAN_POINT('Ctrl Pts',(29.775413173328,2.69370321195049,33.8969505670841));
#70825=CARTESIAN_POINT('',(29.5990162172122,2.70673030953515,33.8637293696319));
#70826=CARTESIAN_POINT('Origin',(30.,-1.32966554433622E-14,33.8637293696319));
#70827=CARTESIAN_POINT('',(29.589548948342,2.67170473125694,33.8969505670765));
#70828=CARTESIAN_POINT('Ctrl Pts',(29.5895489483398,2.67170473124897,33.8969505670841));
#70829=CARTESIAN_POINT('Ctrl Pts',(29.5942536716245,2.68911055925956,33.8804609779983));
#70830=CARTESIAN_POINT('Ctrl Pts',(29.5990162172114,2.7067303095322,33.8637293696347));
#70831=CARTESIAN_POINT('',(29.5647599813892,2.6677785445999,33.8969505670765));
#70832=CARTESIAN_POINT('Origin',(29.5762726922515,2.67530902338217,33.8912940899386));
#70833=CARTESIAN_POINT('',(29.5449325747129,2.6981643020872,33.8637293696319));
#70834=CARTESIAN_POINT('Ctrl Pts',(29.5449325747146,2.69816430208465,33.8637293696347));
#70835=CARTESIAN_POINT('Ctrl Pts',(29.554906827,2.68287863129518,33.8804609779983));
#70836=CARTESIAN_POINT('Ctrl Pts',(29.5647599813937,2.66777854459298,33.8969505670841));
#70837=CARTESIAN_POINT('',(29.3878847039277,2.66692553831737,33.8637293696319));
#70838=CARTESIAN_POINT('Origin',(30.,-1.32966554433622E-14,33.8637293696319));
#70839=CARTESIAN_POINT('',(29.3811946946869,2.63126513885323,33.8969505670765));
#70840=CARTESIAN_POINT('Ctrl Pts',(29.3811946946854,2.6312651388451,33.8969505670841));
#70841=CARTESIAN_POINT('Ctrl Pts',(29.3845192693522,2.64898643883141,33.8804609779983));
#70842=CARTESIAN_POINT('Ctrl Pts',(29.3878847039271,2.66692553831437,33.8637293696347));
#70843=CARTESIAN_POINT('',(29.3567901889011,2.6254061353882,33.8969505670765));
#70844=CARTESIAN_POINT('Origin',(29.3676766176014,2.6338164916465,33.8912943077151));
#70845=CARTESIAN_POINT('',(29.3346398644471,2.65414258332745,33.8637293696319));
#70846=CARTESIAN_POINT('Ctrl Pts',(29.334639864449,2.65414258332502,33.8637293696347));
#70847=CARTESIAN_POINT('Ctrl Pts',(29.3457826693511,2.63968660397215,33.8804609779983));
#70848=CARTESIAN_POINT('Ctrl Pts',(29.3567901889061,2.62540613538165,33.8969505670841));
#70849=CARTESIAN_POINT('',(29.1805270849924,2.61067828431312,33.8637293696319));
#70850=CARTESIAN_POINT('Origin',(30.,-1.32966554433622E-14,33.8637293696319));
#70851=CARTESIAN_POINT('',(29.1766555815128,2.57460292188403,33.8969505670765));
#70852=CARTESIAN_POINT('Ctrl Pts',(29.1766555815118,2.57460292187581,33.8969505670841));
#70853=CARTESIAN_POINT('Ctrl Pts',(29.1785795104524,2.59253043613048,33.8804609779983));
#70854=CARTESIAN_POINT('Ctrl Pts',(29.1805270849921,2.61067828431008,33.8637293696347));
#70855=CARTESIAN_POINT('',(29.1527859987874,2.56684722431571,33.8969505670765));
#70856=CARTESIAN_POINT('Origin',(29.162979042241,2.57608565616365,33.891294472568));
#70857=CARTESIAN_POINT('',(29.1284493206716,2.59375719294953,33.8637293696319));
#70858=CARTESIAN_POINT('Ctrl Pts',(29.1284493206737,2.59375719294727,33.8637293696347));
#70859=CARTESIAN_POINT('Ctrl Pts',(29.1406919790949,2.58022003095078,33.8804609779983));
#70860=CARTESIAN_POINT('Ctrl Pts',(29.1527859987929,2.56684722430958,33.8969505670841));
#70861=CARTESIAN_POINT('',(28.9782217890806,2.53833533054746,33.8637293696319));
#70862=CARTESIAN_POINT('Origin',(30.,-1.32966554433622E-14,33.8637293696319));
#70863=CARTESIAN_POINT('',(28.9771926604684,2.50206742175908,33.8969505670765));
#70864=CARTESIAN_POINT('Ctrl Pts',(28.9771926604681,2.50206742175082,33.8969505670841));
#70865=CARTESIAN_POINT('Ctrl Pts',(28.9777040820208,2.52009062118696,33.8804609779983));
#70866=CARTESIAN_POINT('Ctrl Pts',(28.9782217890805,2.5383353305444,33.8637293696347));
#70867=CARTESIAN_POINT('',(28.9540051647184,2.49246284654199,33.8969505670765));
#70868=CARTESIAN_POINT('Origin',(28.9634419889311,2.50247243285091,33.8912946002427));
#70869=CARTESIAN_POINT('',(28.9276321766543,2.51738042696527,33.8637293696319));
#70870=CARTESIAN_POINT('Ctrl Pts',(28.9276321766565,2.51738042696315,33.8637293696347));
#70871=CARTESIAN_POINT('Ctrl Pts',(28.9408992085365,2.50484554342835,33.8804609779983));
#70872=CARTESIAN_POINT('Ctrl Pts',(28.9540051647244,2.49246284653631,33.8969505670841));
#70873=CARTESIAN_POINT('',(28.7822160956148,2.45034269538683,33.8637293696319));
#70874=CARTESIAN_POINT('Origin',(30.,-1.32966554433622E-14,33.8637293696319));
#70875=CARTESIAN_POINT('Ctrl Pts',(28.7840356867905,2.41410584394887,33.8969505670841));
#70876=CARTESIAN_POINT('Ctrl Pts',(28.7831314478713,2.43211360954865,33.8804609779983));
#70877=CARTESIAN_POINT('Ctrl Pts',(28.782216095615,2.45034269538377,33.8637293696347));
#70878=CARTESIAN_POINT('',(28.7334265368663,2.42548317353484,33.8637293696319));
#70879=CARTESIAN_POINT('Ctrl Pts',(28.7334265368687,2.42548317353291,33.8637293696347));
#70880=CARTESIAN_POINT('Ctrl Pts',(28.7476361465443,2.41402785018503,33.8804609779983));
#70881=CARTESIAN_POINT('Ctrl Pts',(28.7616732366439,2.40271160648614,33.8969505670841));
#70882=CARTESIAN_POINT('',(28.5937184448738,2.3472428826875,33.8637293696319));
#70883=CARTESIAN_POINT('Origin',(30.,-1.32966554433622E-14,33.8637293696319));
#70884=CARTESIAN_POINT('Ctrl Pts',(28.5983755374531,2.31126050084732,33.8969505670841));
#70885=CARTESIAN_POINT('Ctrl Pts',(28.5960612129956,2.32914180874763,33.8804609779983));
#70886=CARTESIAN_POINT('Ctrl Pts',(28.5937184448742,2.34724288268447,33.8637293696347));
#70887=CARTESIAN_POINT('',(28.547029743657,2.31863200978457,33.8637293696319));
#70888=CARTESIAN_POINT('Ctrl Pts',(28.5470297436595,2.31863200978283,33.8637293696347));
#70889=CARTESIAN_POINT('Ctrl Pts',(28.5620943241618,2.30832687249961,33.8804609779983));
#70890=CARTESIAN_POINT('Ctrl Pts',(28.576976004845,2.29814685039931,33.8969505670841));
#70891=CARTESIAN_POINT('',(28.4138909875563,2.22967153707894,33.8637293696319));
#70892=CARTESIAN_POINT('Origin',(30.,-1.32966554433622E-14,33.8637293696319));
#70893=CARTESIAN_POINT('Ctrl Pts',(28.4213568690146,2.19416546818595,33.8969505670841));
#70894=CARTESIAN_POINT('Ctrl Pts',(28.4176467275988,2.21181007417744,33.8804609779983));
#70895=CARTESIAN_POINT('Ctrl Pts',(28.4138909875569,2.22967153707594,33.8637293696347));
#70896=CARTESIAN_POINT('',(28.3695909952396,2.19748570867059,33.8637293696319));
#70897=CARTESIAN_POINT('Ctrl Pts',(28.3695909952423,2.19748570866909,33.8637293696347));
#70898=CARTESIAN_POINT('Ctrl Pts',(28.3854176684231,2.18839429204867,33.8804609779983));
#70899=CARTESIAN_POINT('Ctrl Pts',(28.4010521891798,2.17941325476839,33.8969505670841));
#70900=CARTESIAN_POINT('',(28.2438424197352,2.09835352500326,33.8637293696319));
#70901=CARTESIAN_POINT('Origin',(30.,-1.32966554433622E-14,33.8637293696319));
#70902=CARTESIAN_POINT('Ctrl Pts',(28.2540710604308,2.06354267577915,33.8969505670841));
#70903=CARTESIAN_POINT('Ctrl Pts',(28.2489879763122,2.08084179499845,33.8804609779983));
#70904=CARTESIAN_POINT('Ctrl Pts',(28.2438424197361,2.09835352500033,33.8637293696347));
#70905=CARTESIAN_POINT('',(28.2022042605027,2.0627911774245,33.8637293696319));
#70906=CARTESIAN_POINT('Ctrl Pts',(28.2022042605055,2.0627911774232,33.8637293696347));
#70907=CARTESIAN_POINT('Ctrl Pts',(28.2186954496616,2.05496953307227,33.8804609779984));
#70908=CARTESIAN_POINT('Ctrl Pts',(28.2349864184722,2.04724285169337,33.8969505670841));
#70909=CARTESIAN_POINT('',(28.0846211473781,1.95409846567259,33.8637293696319));
#70910=CARTESIAN_POINT('Origin',(30.,-1.32966554433622E-14,33.8637293696319));
#70911=CARTESIAN_POINT('Ctrl Pts',(28.0975494843397,1.92019745657863,33.8969505670841));
#70912=CARTESIAN_POINT('Ctrl Pts',(28.0911247964223,1.9370444342032,33.8804609779983));
#70913=CARTESIAN_POINT('Ctrl Pts',(28.0846211473792,1.95409846566974,33.8637293696347));
#70914=CARTESIAN_POINT('',(28.0459015343274,1.91537885262192,33.8637293696319));
#70915=CARTESIAN_POINT('Ctrl Pts',(28.0459015343303,1.91537885262084,33.8637293696347));
#70916=CARTESIAN_POINT('Ctrl Pts',(28.0629555657968,1.90887520357776,33.8804609779983));
#70917=CARTESIAN_POINT('Ctrl Pts',(28.0798025434214,1.90245051566032,33.8969505670841));
#70918=CARTESIAN_POINT('',(27.9372088225755,1.79779573949736,33.8637293696319));
#70919=CARTESIAN_POINT('Origin',(30.,-1.32966554433622E-14,33.8637293696319));
#70920=CARTESIAN_POINT('Ctrl Pts',(27.9527571483066,1.76501358152779,33.8969505670841));
#70921=CARTESIAN_POINT('Ctrl Pts',(27.9450304669277,1.78130455033841,33.8804609779983));
#70922=CARTESIAN_POINT('Ctrl Pts',(27.9372088225768,1.79779573949458,33.8637293696347));
#70923=CARTESIAN_POINT('',(27.9016464749967,1.75615758026483,33.8637293696319));
#70924=CARTESIAN_POINT('Ctrl Pts',(27.9016464749997,1.75615758026397,33.8637293696347));
#70925=CARTESIAN_POINT('Ctrl Pts',(27.9191582050016,1.75101202368779,33.8804609779983));
#70926=CARTESIAN_POINT('Ctrl Pts',(27.9364573242208,1.74592893956924,33.8969505670841));
#70927=CARTESIAN_POINT('',(27.8025142913294,1.63040900476038,33.8637293696319));
#70928=CARTESIAN_POINT('Origin',(30.,-1.32966554433622E-14,33.8637293696319));
#70929=CARTESIAN_POINT('Ctrl Pts',(27.8205867452316,1.59894781082027,33.8969505670841));
#70930=CARTESIAN_POINT('Ctrl Pts',(27.8116057079513,1.61458233157693,33.8804609779983));
#70931=CARTESIAN_POINT('Ctrl Pts',(27.8025142913309,1.63040900475771,33.8637293696347));
#70932=CARTESIAN_POINT('',(27.7703284629211,1.58610901244374,33.8637293696319));
#70933=CARTESIAN_POINT('Ctrl Pts',(27.7703284629241,1.58610901244311,33.8637293696347));
#70934=CARTESIAN_POINT('Ctrl Pts',(27.7881899258226,1.5823532724012,33.8804609779984));
#70935=CARTESIAN_POINT('Ctrl Pts',(27.8058345318141,1.57864313098542,33.8969505670841));
#70936=CARTESIAN_POINT('',(27.6813679902154,1.45297025634305,33.8637293696319));
#70937=CARTESIAN_POINT('Origin',(30.,-1.32966554433622E-14,33.8637293696319));
#70938=CARTESIAN_POINT('Ctrl Pts',(27.7018531496007,1.423023995155,33.8969505670841));
#70939=CARTESIAN_POINT('Ctrl Pts',(27.6916731275004,1.43790567583821,33.8804609779983));
#70940=CARTESIAN_POINT('Ctrl Pts',(27.6813679902172,1.45297025634054,33.8637293696347));
#70941=CARTESIAN_POINT('',(27.6527571173125,1.40628155512618,33.8637293696319));
#70942=CARTESIAN_POINT('Ctrl Pts',(27.6527571173155,1.40628155512578,33.8637293696347));
#70943=CARTESIAN_POINT('Ctrl Pts',(27.6708581912524,1.40393878700439,33.8804609779983));
#70944=CARTESIAN_POINT('Ctrl Pts',(27.6887394991527,1.40162446254697,33.8969505670841));
#70945=CARTESIAN_POINT('',(27.5745168264652,1.26657346313372,33.8637293696319));
#70946=CARTESIAN_POINT('Origin',(30.,-1.32966554433622E-14,33.8637293696319));
#70947=CARTESIAN_POINT('Ctrl Pts',(27.5972883935138,1.23832676335601,33.8969505670841));
#70948=CARTESIAN_POINT('Ctrl Pts',(27.5859721498149,1.2523638534557,33.8804609779984));
#70949=CARTESIAN_POINT('Ctrl Pts',(27.5745168264671,1.26657346313129,33.8637293696347));
#70950=CARTESIAN_POINT('',(27.5496573046132,1.21778390438518,33.8637293696319));
#70951=CARTESIAN_POINT('Ctrl Pts',(27.5496573046163,1.21778390438503,33.8637293696347));
#70952=CARTESIAN_POINT('Ctrl Pts',(27.5678863904514,1.21686855212868,33.8804609779984));
#70953=CARTESIAN_POINT('Ctrl Pts',(27.5858941560511,1.21596431320949,33.8969505670841));
#70954=CARTESIAN_POINT('',(27.4826195730347,1.07236782334576,33.8637293696319));
#70955=CARTESIAN_POINT('Origin',(30.,-1.32966554433622E-14,33.8637293696319));
#70956=CARTESIAN_POINT('Ctrl Pts',(27.5075371534637,1.04599483527557,33.8969505670841));
#70957=CARTESIAN_POINT('Ctrl Pts',(27.4951544565716,1.05910079146348,33.8804609779983));
#70958=CARTESIAN_POINT('Ctrl Pts',(27.4826195730368,1.07236782334352,33.8637293696347));
#70959=CARTESIAN_POINT('',(27.4616646694525,1.02177821091942,33.8637293696319));
#70960=CARTESIAN_POINT('Ctrl Pts',(27.4616646694556,1.0217782109195,33.8637293696347));
#70961=CARTESIAN_POINT('Ctrl Pts',(27.479909378813,1.02229591797925,33.8804609779983));
#70962=CARTESIAN_POINT('Ctrl Pts',(27.4979325782492,1.0228073395319,33.8969505670841));
#70963=CARTESIAN_POINT('',(27.4062428070505,0.871550679328378,33.8637293696319));
#70964=CARTESIAN_POINT('Origin',(30.,-1.32966554433622E-14,33.8637293696319));
#70965=CARTESIAN_POINT('Ctrl Pts',(27.4331527756904,0.847214001207086,33.8969505670841));
#70966=CARTESIAN_POINT('Ctrl Pts',(27.4197799690492,0.859308020905129,33.8804609779984));
#70967=CARTESIAN_POINT('Ctrl Pts',(27.4062428070528,0.871550679326332,33.8637293696347));
#70968=CARTESIAN_POINT('',(27.3893217156869,0.819472915007596,33.8637293696319));
#70969=CARTESIAN_POINT('Ctrl Pts',(27.3893217156899,0.819472915007932,33.8637293696347));
#70970=CARTESIAN_POINT('Ctrl Pts',(27.4074695638695,0.821420489547589,33.8804609779983));
#70971=CARTESIAN_POINT('Ctrl Pts',(27.4253970781241,0.823344418488154,33.8969505670841));
#70972=CARTESIAN_POINT('',(27.3458574166725,0.665360135552929,33.8637293696319));
#70973=CARTESIAN_POINT('Origin',(30.,-1.32966554433622E-14,33.8637293696319));
#70974=CARTESIAN_POINT('Ctrl Pts',(27.3745938646183,0.643209811093841,33.8969505670841));
#70975=CARTESIAN_POINT('Ctrl Pts',(27.3603133960278,0.654217330648928,33.8804609779983));
#70976=CARTESIAN_POINT('Ctrl Pts',(27.3458574166749,0.665360135551045,33.8637293696347));
#70977=CARTESIAN_POINT('',(27.3330744616826,0.612115296072357,33.8637293696319));
#70978=CARTESIAN_POINT('Ctrl Pts',(27.3330744616856,0.612115296072913,33.8637293696347));
#70979=CARTESIAN_POINT('Ctrl Pts',(27.3510135611686,0.615480730647817,33.8804609779983));
#70980=CARTESIAN_POINT('Ctrl Pts',(27.3687348611549,0.618805305314613,33.8969505670841));
#70981=CARTESIAN_POINT('',(27.3018356979128,0.455067425287102,33.8637293696319));
#70982=CARTESIAN_POINT('Origin',(30.,-1.32966554433622E-14,33.8637293696319));
#70983=CARTESIAN_POINT('Ctrl Pts',(27.332221455407,0.435240018606297,33.8969505670841));
#70984=CARTESIAN_POINT('Ctrl Pts',(27.3171213687048,0.445093172999983,33.8804609779983));
#70985=CARTESIAN_POINT('Ctrl Pts',(27.3018356979154,0.455067425285416,33.8637293696347));
#70986=CARTESIAN_POINT('',(27.2932696904648,0.400983782787843,33.8637293696319));
#70987=CARTESIAN_POINT('Ctrl Pts',(27.2932696904678,0.40098378278865,33.8637293696347));
#70988=CARTESIAN_POINT('Ctrl Pts',(27.3108894407404,0.405746328375518,33.8804609779983));
#70989=CARTESIAN_POINT('Ctrl Pts',(27.328295268751,0.410451051660182,33.8969505670841));
#70990=CARTESIAN_POINT('',(27.2744490593061,0.241969073019103,33.8637293696319));
#70991=CARTESIAN_POINT('Origin',(30.,-1.32966554433622E-14,33.8637293696319));
#70992=CARTESIAN_POINT('Ctrl Pts',(27.3062967880495,0.224586826672042,33.8969505670841));
#70993=CARTESIAN_POINT('Ctrl Pts',(27.2904701802914,0.233224867930985,33.8804609779983));
#70994=CARTESIAN_POINT('Ctrl Pts',(27.2744490593088,0.24196907301762,33.8637293696347));
#70995=CARTESIAN_POINT('',(27.2701528116845,0.1873800711418,33.8637293696319));
#70996=CARTESIAN_POINT('Ctrl Pts',(27.2701528116874,0.187380071142834,33.8637293696347));
#70997=CARTESIAN_POINT('Ctrl Pts',(27.2873445811301,0.193510365064418,33.8804609779983));
#70998=CARTESIAN_POINT('Ctrl Pts',(27.3043276244473,0.199566230783421,33.8969505670841));
#70999=CARTESIAN_POINT('',(27.2638663485864,0.0273789009530583,33.8637293696319));
#71000=CARTESIAN_POINT('Origin',(30.,-1.32966554433622E-14,33.8637293696319));
#71001=CARTESIAN_POINT('Ctrl Pts',(27.2969796967408,0.0125489822686371,
33.8969505670841));
#71002=CARTESIAN_POINT('Ctrl Pts',(27.2805241442266,0.0199186539960461,
33.8804609779983));
#71003=CARTESIAN_POINT('Ctrl Pts',(27.2638663485892,0.0273789009517924,
33.8637293696347));
#71004=CARTESIAN_POINT('',(27.2638663485864,-0.0273789009530277,33.8637293696319));
#71005=CARTESIAN_POINT('Ctrl Pts',(27.2638663485892,-0.0273789009517733,
33.8637293696347));
#71006=CARTESIAN_POINT('Ctrl Pts',(27.2805241442266,-0.0199186539960275,
33.8804609779983));
#71007=CARTESIAN_POINT('Ctrl Pts',(27.2969796967409,-0.012548982268619,
33.8969505670841));
#71008=CARTESIAN_POINT('',(27.2701528116845,-0.18738007114177,33.8637293696319));
#71009=CARTESIAN_POINT('Origin',(30.,-1.32966554433622E-14,33.8637293696319));
#71010=CARTESIAN_POINT('',(27.3043276244395,-0.199566230780611,33.8969505670765));
#71011=CARTESIAN_POINT('Ctrl Pts',(27.3043276244473,-0.199566230783401,
33.8969505670841));
#71012=CARTESIAN_POINT('Ctrl Pts',(27.2873445811301,-0.193510365064398,
33.8804609779983));
#71013=CARTESIAN_POINT('Ctrl Pts',(27.2701528116874,-0.187380071142813,
33.8637293696347));
#71014=CARTESIAN_POINT('',(27.3062967880422,-0.224586826675978,33.8969505670765));
#71015=CARTESIAN_POINT('Origin',(27.2996925411099,-0.212518788369432,33.8912937927564));
#71016=CARTESIAN_POINT('',(27.2744490593061,-0.241969073019072,33.8637293696319));
#71017=CARTESIAN_POINT('Ctrl Pts',(27.2744490593088,-0.241969073017592,
33.8637293696347));
#71018=CARTESIAN_POINT('Ctrl Pts',(27.2904701802914,-0.233224867930958,
33.8804609779983));
#71019=CARTESIAN_POINT('Ctrl Pts',(27.3062967880495,-0.224586826672017,
33.8969505670841));
#71020=CARTESIAN_POINT('',(27.2932696904648,-0.400983782787811,33.8637293696319));
#71021=CARTESIAN_POINT('Origin',(30.,-1.32966554433622E-14,33.8637293696319));
#71022=CARTESIAN_POINT('',(27.328295268743,-0.410451051657984,33.8969505670765));
#71023=CARTESIAN_POINT('Ctrl Pts',(27.328295268751,-0.410451051660133,33.8969505670841));
#71024=CARTESIAN_POINT('Ctrl Pts',(27.3108894407404,-0.40574632837547,33.8804609779983));
#71025=CARTESIAN_POINT('Ctrl Pts',(27.2932696904678,-0.400983782788603,
33.8637293696347));
#71026=CARTESIAN_POINT('',(27.3322214554001,-0.435240018610796,33.8969505670765));
#71027=CARTESIAN_POINT('Origin',(27.3246909766178,-0.423727307748468,33.8912940899386));
#71028=CARTESIAN_POINT('',(27.3018356979128,-0.45506742528707,33.8637293696319));
#71029=CARTESIAN_POINT('Ctrl Pts',(27.3018356979154,-0.455067425285398,
33.8637293696347));
#71030=CARTESIAN_POINT('Ctrl Pts',(27.3171213687048,-0.445093172999969,
33.8804609779984));
#71031=CARTESIAN_POINT('Ctrl Pts',(27.332221455407,-0.435240018606285,33.8969505670841));
#71032=CARTESIAN_POINT('',(27.3330744616826,-0.612115296072328,33.8637293696319));
#71033=CARTESIAN_POINT('Origin',(30.,-1.32966554433622E-14,33.8637293696319));
#71034=CARTESIAN_POINT('',(27.3687348611467,-0.618805305313063,33.8969505670765));
#71035=CARTESIAN_POINT('Ctrl Pts',(27.3687348611549,-0.618805305314591,
33.8969505670841));
#71036=CARTESIAN_POINT('Ctrl Pts',(27.3510135611686,-0.615480730647799,
33.8804609779983));
#71037=CARTESIAN_POINT('Ctrl Pts',(27.3330744616856,-0.6121152960729,33.8637293696347));
#71038=CARTESIAN_POINT('',(27.3745938646118,-0.643209811098888,33.8969505670765));
#71039=CARTESIAN_POINT('Origin',(27.3661835083535,-0.632323382398592,33.8912943077151));
#71040=CARTESIAN_POINT('',(27.3458574166725,-0.665360135552901,33.8637293696319));
#71041=CARTESIAN_POINT('Ctrl Pts',(27.345857416675,-0.665360135551053,33.8637293696347));
#71042=CARTESIAN_POINT('Ctrl Pts',(27.3603133960278,-0.654217330648938,
33.8804609779984));
#71043=CARTESIAN_POINT('Ctrl Pts',(27.3745938646183,-0.643209811093851,
33.8969505670841));
#71044=CARTESIAN_POINT('',(27.3893217156868,-0.819472915007569,33.8637293696319));
#71045=CARTESIAN_POINT('Origin',(30.,-1.32966554433622E-14,33.8637293696319));
#71046=CARTESIAN_POINT('',(27.4253970781159,-0.823344418487241,33.8969505670765));
#71047=CARTESIAN_POINT('Ctrl Pts',(27.4253970781241,-0.823344418488121,
33.8969505670841));
#71048=CARTESIAN_POINT('Ctrl Pts',(27.4074695638695,-0.821420489547552,
33.8804609779983));
#71049=CARTESIAN_POINT('Ctrl Pts',(27.3893217156899,-0.819472915007892,
33.8637293696347));
#71050=CARTESIAN_POINT('',(27.4331527756843,-0.847214001212589,33.8969505670765));
#71051=CARTESIAN_POINT('Origin',(27.4239143438363,-0.837020957758988,33.8912944725679));
#71052=CARTESIAN_POINT('',(27.4062428070504,-0.871550679328351,33.8637293696319));
#71053=CARTESIAN_POINT('Ctrl Pts',(27.4062428070527,-0.871550679326329,
33.8637293696347));
#71054=CARTESIAN_POINT('Ctrl Pts',(27.4197799690492,-0.859308020905111,
33.8804609779983));
#71055=CARTESIAN_POINT('Ctrl Pts',(27.4331527756904,-0.847214001207053,
33.8969505670841));
#71056=CARTESIAN_POINT('',(27.4616646694525,-1.02177821091939,33.8637293696319));
#71057=CARTESIAN_POINT('Origin',(30.,-1.32966554433622E-14,33.8637293696319));
#71058=CARTESIAN_POINT('',(27.4979325782409,-1.02280733953164,33.8969505670765));
#71059=CARTESIAN_POINT('Ctrl Pts',(27.4979325782492,-1.02280733953187,33.8969505670841));
#71060=CARTESIAN_POINT('Ctrl Pts',(27.479909378813,-1.02229591797922,33.8804609779983));
#71061=CARTESIAN_POINT('Ctrl Pts',(27.4616646694556,-1.02177821091947,33.8637293696347));
#71062=CARTESIAN_POINT('',(27.507537153458,-1.04599483528157,33.8969505670765));
#71063=CARTESIAN_POINT('Origin',(27.4975275671491,-1.03655801106889,33.8912946002427));
#71064=CARTESIAN_POINT('',(27.4826195730347,-1.07236782334573,33.8637293696319));
#71065=CARTESIAN_POINT('Ctrl Pts',(27.4826195730368,-1.07236782334351,33.8637293696347));
#71066=CARTESIAN_POINT('Ctrl Pts',(27.4951544565716,-1.05910079146347,33.8804609779983));
#71067=CARTESIAN_POINT('Ctrl Pts',(27.5075371534637,-1.04599483527557,33.8969505670841));
#71068=CARTESIAN_POINT('',(27.5496573046131,-1.21778390438516,33.8637293696319));
#71069=CARTESIAN_POINT('Origin',(30.,-1.32966554433622E-14,33.8637293696319));
#71070=CARTESIAN_POINT('',(27.5858941560428,-1.21596431320988,33.8969505670765));
#71071=CARTESIAN_POINT('Ctrl Pts',(27.5858941560511,-1.21596431320946,33.8969505670841));
#71072=CARTESIAN_POINT('Ctrl Pts',(27.5678863904513,-1.21686855212866,33.8804609779983));
#71073=CARTESIAN_POINT('Ctrl Pts',(27.5496573046162,-1.217783904385,33.8637293696347));
#71074=CARTESIAN_POINT('',(27.5972883935086,-1.23832676336246,33.8969505670765));
#71075=CARTESIAN_POINT('Origin',(27.5865693373251,-1.22970433386023,33.891294700665));
#71076=CARTESIAN_POINT('',(27.5745168264651,-1.2665734631337,33.8637293696319));
#71077=CARTESIAN_POINT('Ctrl Pts',(27.574516826467,-1.26657346313129,33.8637293696347));
#71078=CARTESIAN_POINT('Ctrl Pts',(27.5859721498149,-1.2523638534557,33.8804609779983));
#71079=CARTESIAN_POINT('Ctrl Pts',(27.5972883935138,-1.23832676335601,33.8969505670841));
#71080=CARTESIAN_POINT('',(27.6527571173125,-1.40628155512615,33.8637293696319));
#71081=CARTESIAN_POINT('Origin',(30.,-1.32966554433622E-14,33.8637293696319));
#71082=CARTESIAN_POINT('',(27.6887394991444,-1.40162446254801,33.8969505670765));
#71083=CARTESIAN_POINT('Ctrl Pts',(27.6887394991526,-1.40162446254695,33.8969505670841));
#71084=CARTESIAN_POINT('Ctrl Pts',(27.6708581912523,-1.40393878700437,33.8804609779983));
#71085=CARTESIAN_POINT('Ctrl Pts',(27.6527571173155,-1.40628155512576,33.8637293696347));
#71086=CARTESIAN_POINT('',(27.701853149596,-1.42302399516179,33.8969505670765));
#71087=CARTESIAN_POINT('Origin',(27.6904906884452,-1.4152691174526,33.8912947803756));
#71088=CARTESIAN_POINT('',(27.6813679902154,-1.45297025634303,33.8637293696319));
#71089=CARTESIAN_POINT('Ctrl Pts',(27.6813679902171,-1.4529702563405,33.8637293696347));
#71090=CARTESIAN_POINT('Ctrl Pts',(27.6916731275004,-1.43790567583818,33.8804609779983));
#71091=CARTESIAN_POINT('Ctrl Pts',(27.7018531496007,-1.42302399515497,33.8969505670841));
#71092=CARTESIAN_POINT('',(27.770328462921,-1.58610901244372,33.8637293696319));
#71093=CARTESIAN_POINT('Origin',(30.,-1.32966554433622E-14,33.8637293696319));
#71094=CARTESIAN_POINT('',(27.8058345318059,-1.5786431309871,33.8969505670765));
#71095=CARTESIAN_POINT('Ctrl Pts',(27.805834531814,-1.5786431309854,33.8969505670841));
#71096=CARTESIAN_POINT('Ctrl Pts',(27.7881899258225,-1.58235327240118,33.8804609779983));
#71097=CARTESIAN_POINT('Ctrl Pts',(27.770328462924,-1.5861090124431,33.8637293696347));
#71098=CARTESIAN_POINT('',(27.8205867452275,-1.59894781082744,33.8969505670765));
#71099=CARTESIAN_POINT('Origin',(27.8086509152839,-1.59210829514295,33.8912948438349));
#71100=CARTESIAN_POINT('',(27.8025142913294,-1.63040900476036,33.8637293696319));
#71101=CARTESIAN_POINT('Ctrl Pts',(27.8025142913309,-1.63040900475772,33.8637293696347));
#71102=CARTESIAN_POINT('Ctrl Pts',(27.8116057079513,-1.61458233157693,33.8804609779984));
#71103=CARTESIAN_POINT('Ctrl Pts',(27.8205867452316,-1.59894781082027,33.8969505670841));
#71104=CARTESIAN_POINT('',(27.9016464749967,-1.75615758026481,33.8637293696319));
#71105=CARTESIAN_POINT('Origin',(30.,-1.32966554433622E-14,33.8637293696319));
#71106=CARTESIAN_POINT('',(27.9364573242129,-1.74592893957155,33.8969505670765));
#71107=CARTESIAN_POINT('Ctrl Pts',(27.9364573242208,-1.74592893956922,33.8969505670841));
#71108=CARTESIAN_POINT('Ctrl Pts',(27.9191582050015,-1.75101202368778,33.8804609779983));
#71109=CARTESIAN_POINT('Ctrl Pts',(27.9016464749996,-1.75615758026396,33.8637293696347));
#71110=CARTESIAN_POINT('',(27.9527571483031,-1.76501358153525,33.8969505670765));
#71111=CARTESIAN_POINT('Origin',(27.9403215240917,-1.75913159602167,33.8912948941586));
#71112=CARTESIAN_POINT('',(27.9372088225755,-1.79779573949734,33.8637293696319));
#71113=CARTESIAN_POINT('Ctrl Pts',(27.9372088225768,-1.79779573949458,33.8637293696347));
#71114=CARTESIAN_POINT('Ctrl Pts',(27.9450304669278,-1.78130455033841,33.8804609779984));
#71115=CARTESIAN_POINT('Ctrl Pts',(27.9527571483066,-1.76501358152779,33.8969505670841));
#71116=CARTESIAN_POINT('',(28.0459015343274,-1.91537885262191,33.8637293696319));
#71117=CARTESIAN_POINT('Origin',(30.,-1.32966554433622E-14,33.8637293696319));
#71118=CARTESIAN_POINT('',(28.0798025434136,-1.90245051566325,33.8969505670765));
#71119=CARTESIAN_POINT('Ctrl Pts',(28.0798025434214,-1.90245051566032,33.8969505670841));
#71120=CARTESIAN_POINT('Ctrl Pts',(28.0629555657968,-1.90887520357775,33.8804609779983));
#71121=CARTESIAN_POINT('Ctrl Pts',(28.0459015343303,-1.91537885262082,33.8637293696347));
#71122=CARTESIAN_POINT('',(28.0975494843367,-1.92019745658631,33.8969505670765));
#71123=CARTESIAN_POINT('Origin',(28.0846907243829,-1.91530926701236,33.891294933562));
#71124=CARTESIAN_POINT('',(28.084621147378,-1.95409846567257,33.8637293696319));
#71125=CARTESIAN_POINT('Ctrl Pts',(28.0846211473791,-1.9540984656697,33.8637293696347));
#71126=CARTESIAN_POINT('Ctrl Pts',(28.0911247964222,-1.93704443420316,33.8804609779983));
#71127=CARTESIAN_POINT('Ctrl Pts',(28.0975494843396,-1.92019745657857,33.8969505670841));
#71128=CARTESIAN_POINT('',(28.2022042605026,-2.06279117742449,33.8637293696319));
#71129=CARTESIAN_POINT('Origin',(30.,-1.32966554433622E-14,33.8637293696319));
#71130=CARTESIAN_POINT('',(28.2349864184647,-2.04724285169689,33.8969505670765));
#71131=CARTESIAN_POINT('Ctrl Pts',(28.2349864184722,-2.04724285169334,33.8969505670841));
#71132=CARTESIAN_POINT('Ctrl Pts',(28.2186954496616,-2.05496953307223,33.8804609779983));
#71133=CARTESIAN_POINT('Ctrl Pts',(28.2022042605054,-2.06279117742317,33.8637293696347));
#71134=CARTESIAN_POINT('',(28.2540710604284,-2.06354267578707,33.8969505670765));
#71135=CARTESIAN_POINT('Origin',(28.2408684341297,-2.05967842174595,33.8912949636253));
#71136=CARTESIAN_POINT('',(28.2438424197351,-2.09835352500325,33.8637293696319));
#71137=CARTESIAN_POINT('Ctrl Pts',(28.243842419736,-2.09835352500031,33.8637293696347));
#71138=CARTESIAN_POINT('Ctrl Pts',(28.2489879763122,-2.08084179499844,33.8804609779983));
#71139=CARTESIAN_POINT('Ctrl Pts',(28.2540710604307,-2.06354267577914,33.8969505670841));
#71140=CARTESIAN_POINT('',(28.3695909952396,-2.19748570867058,33.8637293696319));
#71141=CARTESIAN_POINT('Origin',(30.,-1.32966554433622E-14,33.8637293696319));
#71142=CARTESIAN_POINT('',(28.4010521891725,-2.17941325477249,33.8969505670765));
#71143=CARTESIAN_POINT('Ctrl Pts',(28.4010521891797,-2.17941325476838,33.8969505670841));
#71144=CARTESIAN_POINT('Ctrl Pts',(28.385417668423,-2.18839429204864,33.8804609779983));
#71145=CARTESIAN_POINT('Ctrl Pts',(28.3695909952423,-2.19748570866905,33.8637293696347));
#71146=CARTESIAN_POINT('',(28.4213568690129,-2.19416546819403,33.8969505670765));
#71147=CARTESIAN_POINT('Origin',(28.4078917675746,-2.19134897714168,33.8912949854673));
#71148=CARTESIAN_POINT('',(28.4138909875562,-2.22967153707893,33.8637293696319));
#71149=CARTESIAN_POINT('Ctrl Pts',(28.4138909875569,-2.22967153707595,33.8637293696347));
#71150=CARTESIAN_POINT('Ctrl Pts',(28.4176467275988,-2.21181007417744,33.8804609779984));
#71151=CARTESIAN_POINT('Ctrl Pts',(28.4213568690146,-2.19416546818595,33.8969505670841));
#71152=CARTESIAN_POINT('',(28.5470297436569,-2.31863200978456,33.8637293696319));
#71153=CARTESIAN_POINT('Origin',(30.,-1.32966554433622E-14,33.8637293696319));
#71154=CARTESIAN_POINT('',(28.5769760048382,-2.29814685040397,33.8969505670765));
#71155=CARTESIAN_POINT('Ctrl Pts',(28.576976004845,-2.29814685039931,33.8969505670841));
#71156=CARTESIAN_POINT('Ctrl Pts',(28.5620943241618,-2.30832687249962,33.8804609779983));
#71157=CARTESIAN_POINT('Ctrl Pts',(28.5470297436595,-2.31863200978285,33.8637293696347));
#71158=CARTESIAN_POINT('',(28.5983755374519,-2.31126050085552,33.8969505670765));
#71159=CARTESIAN_POINT('Origin',(28.5847309718512,-2.30950914111276,33.891294999854));
#71160=CARTESIAN_POINT('',(28.5937184448738,-2.3472428826875,33.8637293696319));
#71161=CARTESIAN_POINT('Ctrl Pts',(28.5937184448742,-2.34724288268445,33.8637293696347));
#71162=CARTESIAN_POINT('Ctrl Pts',(28.5960612129955,-2.32914180874762,33.8804609779983));
#71163=CARTESIAN_POINT('Ctrl Pts',(28.598375537453,-2.31126050084731,33.8969505670841));
#71164=CARTESIAN_POINT('',(28.7334265368663,-2.42548317353484,33.8637293696319));
#71165=CARTESIAN_POINT('Origin',(30.,-1.32966554433622E-14,33.8637293696319));
#71166=CARTESIAN_POINT('',(28.7616732366375,-2.40271160649133,33.8969505670765));
#71167=CARTESIAN_POINT('Ctrl Pts',(28.761673236644,-2.40271160648615,33.8969505670841));
#71168=CARTESIAN_POINT('Ctrl Pts',(28.7476361465443,-2.41402785018505,33.8804609779983));
#71169=CARTESIAN_POINT('Ctrl Pts',(28.7334265368687,-2.42548317353292,33.8637293696347));
#71170=CARTESIAN_POINT('',(28.7840356867901,-2.41410584395713,33.8969505670765));
#71171=CARTESIAN_POINT('Origin',(28.7702957758346,-2.41343041757033,33.8912950072666));
#71172=CARTESIAN_POINT('',(28.7822160956148,-2.45034269538683,33.8637293696319));
#71173=CARTESIAN_POINT('Ctrl Pts',(28.782216095615,-2.45034269538378,33.8637293696347));
#71174=CARTESIAN_POINT('Ctrl Pts',(28.7831314478713,-2.43211360954867,33.8804609779983));
#71175=CARTESIAN_POINT('Ctrl Pts',(28.7840356867905,-2.41410584394888,33.8969505670841));
#71176=CARTESIAN_POINT('',(28.9276321766542,-2.51738042696528,33.8637293696319));
#71177=CARTESIAN_POINT('Origin',(30.,-1.32966554433622E-14,33.8637293696319));
#71178=CARTESIAN_POINT('',(28.9540051647184,-2.49246284654199,33.8969505670765));
#71179=CARTESIAN_POINT('Ctrl Pts',(28.9540051647244,-2.49246284653629,33.8969505670841));
#71180=CARTESIAN_POINT('Ctrl Pts',(28.9408992085365,-2.50484554342835,33.8804609779984));
#71181=CARTESIAN_POINT('Ctrl Pts',(28.9276321766564,-2.51738042696316,33.8637293696347));
#71182=CARTESIAN_POINT('',(28.9771926604683,-2.50206742175908,33.8969505670765));
#71183=CARTESIAN_POINT('Origin',(28.9634421120889,-2.50247209787259,33.8912950079413));
#71184=CARTESIAN_POINT('',(28.9782217890806,-2.53833533054747,33.8637293696319));
#71185=CARTESIAN_POINT('Ctrl Pts',(28.9782217890805,-2.53833533054441,33.8637293696347));
#71186=CARTESIAN_POINT('Ctrl Pts',(28.9777040820207,-2.52009062118697,33.8804609779983));
#71187=CARTESIAN_POINT('Ctrl Pts',(28.9771926604681,-2.50206742175082,33.8969505670841));
#71188=CARTESIAN_POINT('',(29.1284493206716,-2.59375719294953,33.8637293696319));
#71189=CARTESIAN_POINT('Origin',(30.,-1.32966554433622E-14,33.8637293696319));
#71190=CARTESIAN_POINT('',(29.1527859987874,-2.56684722431572,33.8969505670765));
#71191=CARTESIAN_POINT('Ctrl Pts',(29.1527859987929,-2.56684722430957,33.8969505670841));
#71192=CARTESIAN_POINT('Ctrl Pts',(29.1406919790949,-2.58022003095078,33.8804609779984));
#71193=CARTESIAN_POINT('Ctrl Pts',(29.1284493206736,-2.59375719294726,33.8637293696347));
#71194=CARTESIAN_POINT('',(29.1766555815127,-2.57460292188404,33.8969505670765));
#71195=CARTESIAN_POINT('Origin',(29.1629791704777,-2.57608521103258,33.8912950018861));
#71196=CARTESIAN_POINT('',(29.1805270849924,-2.61067828431313,33.8637293696319));
#71197=CARTESIAN_POINT('Ctrl Pts',(29.1805270849921,-2.61067828431009,33.8637293696347));
#71198=CARTESIAN_POINT('Ctrl Pts',(29.1785795104524,-2.59253043613049,33.8804609779983));
#71199=CARTESIAN_POINT('Ctrl Pts',(29.1766555815118,-2.57460292187582,33.8969505670841));
#71200=CARTESIAN_POINT('',(29.334639864447,-2.65414258332747,33.8637293696319));
#71201=CARTESIAN_POINT('Origin',(30.,-1.32966554433622E-14,33.8637293696319));
#71202=CARTESIAN_POINT('',(29.3567901889011,-2.62540613538822,33.8969505670765));
#71203=CARTESIAN_POINT('Ctrl Pts',(29.3567901889061,-2.62540613538166,33.8969505670841));
#71204=CARTESIAN_POINT('Ctrl Pts',(29.345782669351,-2.63968660397217,33.8804609779983));
#71205=CARTESIAN_POINT('Ctrl Pts',(29.3346398644489,-2.65414258332506,33.8637293696347));
#71206=CARTESIAN_POINT('',(29.3811946946869,-2.63126513885324,33.8969505670765));
#71207=CARTESIAN_POINT('Origin',(29.3676767399569,-2.63381590833404,33.8912949888765));
#71208=CARTESIAN_POINT('',(29.3878847039276,-2.66692553831738,33.8637293696319));
#71209=CARTESIAN_POINT('Ctrl Pts',(29.3878847039271,-2.66692553831437,33.8637293696347));
#71210=CARTESIAN_POINT('Ctrl Pts',(29.3845192693522,-2.64898643883142,33.8804609779983));
#71211=CARTESIAN_POINT('Ctrl Pts',(29.3811946946854,-2.63126513884512,33.8969505670841));
#71212=CARTESIAN_POINT('',(29.5449325747129,-2.69816430208721,33.8637293696319));
#71213=CARTESIAN_POINT('Origin',(30.,-1.32966554433622E-14,33.8637293696319));
#71214=CARTESIAN_POINT('',(29.5647599813891,-2.66777854459992,33.8969505670765));
#71215=CARTESIAN_POINT('Ctrl Pts',(29.5647599813936,-2.667778544593,33.8969505670841));
#71216=CARTESIAN_POINT('Ctrl Pts',(29.554906827,-2.68287863129519,33.8804609779983));
#71217=CARTESIAN_POINT('Ctrl Pts',(29.5449325747145,-2.69816430208464,33.8637293696347));
#71218=CARTESIAN_POINT('',(29.589548948342,-2.67170473125696,33.8969505670765));
#71219=CARTESIAN_POINT('Origin',(29.5762727932907,-2.67530826149246,33.8912949684251));
#71220=CARTESIAN_POINT('',(29.5990162172121,-2.70673030953517,33.8637293696319));
#71221=CARTESIAN_POINT('Ctrl Pts',(29.5990162172114,-2.70673030953221,33.8637293696347));
#71222=CARTESIAN_POINT('Ctrl Pts',(29.5942536716245,-2.68911055925957,33.8804609779984));
#71223=CARTESIAN_POINT('Ctrl Pts',(29.5895489483398,-2.67170473124899,33.8969505670841));
#71224=CARTESIAN_POINT('',(29.7580309269809,-2.72555094069392,33.8637293696319));
#71225=CARTESIAN_POINT('Origin',(30.,-1.32966554433622E-14,33.8637293696319));
#71226=CARTESIAN_POINT('',(29.775413173324,-2.69370321195777,33.8969505670765));
#71227=CARTESIAN_POINT('Ctrl Pts',(29.7754131733279,-2.6937032119505,33.8969505670841));
#71228=CARTESIAN_POINT('Ctrl Pts',(29.766775132069,-2.70952981970859,33.8804609779984));
#71229=CARTESIAN_POINT('Ctrl Pts',(29.7580309269823,-2.72555094069122,33.8637293696347));
#71230=CARTESIAN_POINT('',(29.8004337692193,-2.6956723755605,33.8969505670765));
#71231=CARTESIAN_POINT('Origin',(29.7874812679387,-2.70030645711978,33.8912949397144));
#71232=CARTESIAN_POINT('',(29.8126199288582,-2.72984718831551,33.8637293696319));
#71233=CARTESIAN_POINT('Ctrl Pts',(29.8126199288571,-2.72984718831264,33.8637293696347));
#71234=CARTESIAN_POINT('Ctrl Pts',(29.8064896349355,-2.7126554188699,33.8804609779983));
#71235=CARTESIAN_POINT('Ctrl Pts',(29.8004337692165,-2.69567237555272,33.8969505670841));
#71236=CARTESIAN_POINT('',(29.9726210990469,-2.73613365141358,33.8637293696319));
#71237=CARTESIAN_POINT('Origin',(30.,-1.32966554433622E-14,33.8637293696319));
#71238=CARTESIAN_POINT('',(29.987451017728,-2.70302030326669,33.8969505670765));
#71239=CARTESIAN_POINT('Ctrl Pts',(29.9874510177314,-2.70302030325915,33.8969505670841));
#71240=CARTESIAN_POINT('Ctrl Pts',(29.980081346004,-2.71947585577343,33.8804609779983));
#71241=CARTESIAN_POINT('Ctrl Pts',(29.9726210990482,-2.73613365141081,33.8637293696347));
#71242=CARTESIAN_POINT('Ctrl Pts',(30.,-2.69489040503949,33.9051095949605));
#71243=CARTESIAN_POINT('Ctrl Pts',(29.9982996971592,-2.69489040503949,33.9051095949605));
#71244=CARTESIAN_POINT('Ctrl Pts',(29.9965490639354,-2.69522714758869,33.9047710768107));
#71245=CARTESIAN_POINT('Ctrl Pts',(29.9934248389279,-2.69644647069985,33.9035459832655));
#71246=CARTESIAN_POINT('Ctrl Pts',(29.9920523583067,-2.69733049287042,33.9026580100842));
#71247=CARTESIAN_POINT('Ctrl Pts',(29.9894391186861,-2.69960157002983,33.9003782103613));
#71248=CARTESIAN_POINT('Ctrl Pts',(29.9882404972758,-2.7012574944688,33.8987170220582));
#71249=CARTESIAN_POINT('Ctrl Pts',(29.987451017728,-2.7030203032667,33.8969505670765));
#71250=CARTESIAN_POINT('',(30.,-2.73627063036813,33.8637293696319));
#71251=CARTESIAN_POINT('Origin',(30.,-1.32966554433622E-14,31.5762293696319));
#71252=CARTESIAN_POINT('',(30.012548982272,2.70302030326666,31.5905494329235));
#71253=CARTESIAN_POINT('',(30.,2.69489040503946,31.5823904050395));
#71254=CARTESIAN_POINT('Ctrl Pts',(30.012548982272,2.70302030326668,31.5905494329235));
#71255=CARTESIAN_POINT('Ctrl Pts',(30.0117595027242,2.70125749446877,31.5887829779419));
#71256=CARTESIAN_POINT('Ctrl Pts',(30.0105608813139,2.6996015700298,31.5871217896387));
#71257=CARTESIAN_POINT('Ctrl Pts',(30.0079476416933,2.69733049287039,31.5848419899159));
#71258=CARTESIAN_POINT('Ctrl Pts',(30.0065751610721,2.69644647069982,31.5839540167345));
#71259=CARTESIAN_POINT('Ctrl Pts',(30.0034509360646,2.69522714758867,31.5827289231894));
#71260=CARTESIAN_POINT('Ctrl Pts',(30.0017003028408,2.69489040503946,31.5823904050395));
#71261=CARTESIAN_POINT('Ctrl Pts',(30.,2.69489040503946,31.5823904050395));
#71262=CARTESIAN_POINT('',(30.0273789009535,2.73613365141461,31.6237706303691));
#71263=CARTESIAN_POINT('Ctrl Pts',(30.0273789009505,2.73613365140797,31.6237706303625));
#71264=CARTESIAN_POINT('Ctrl Pts',(30.0199186539932,2.71947585576695,31.6070390219952));
#71265=CARTESIAN_POINT('Ctrl Pts',(30.0125489822642,2.70302030324912,31.5905494329059));
#71266=CARTESIAN_POINT('',(30.1873800711414,2.72984718831658,31.6237706303691));
#71267=CARTESIAN_POINT('Origin',(30.,-1.32966554433622E-14,31.6237706303681));
#71268=CARTESIAN_POINT('',(30.1995662307806,2.69567237556048,31.5905494329235));
#71269=CARTESIAN_POINT('Ctrl Pts',(30.1995662307774,2.69567237556935,31.5905494329321));
#71270=CARTESIAN_POINT('Ctrl Pts',(30.1935103650619,2.71265541887687,31.6070390220085));
#71271=CARTESIAN_POINT('Ctrl Pts',(30.1873800711438,2.72984718830972,31.6237706303625));
#71272=CARTESIAN_POINT('',(30.224586826676,2.69370321195774,31.5905494329235));
#71273=CARTESIAN_POINT('Origin',(30.2125187883694,2.70030745889013,31.5962062072437));
#71274=CARTESIAN_POINT('',(30.2419690730196,2.72555094069491,31.6237706303691));
#71275=CARTESIAN_POINT('Ctrl Pts',(30.2419690730161,2.72555094068852,31.6237706303625));
#71276=CARTESIAN_POINT('Ctrl Pts',(30.2332248679276,2.70952981970239,31.6070390219952));
#71277=CARTESIAN_POINT('Ctrl Pts',(30.2245868266668,2.69370321194088,31.5905494329059));
#71278=CARTESIAN_POINT('',(30.4009837827875,2.70673030953627,31.6237706303691));
#71279=CARTESIAN_POINT('Origin',(30.,-1.32966554433622E-14,31.6237706303681));
#71280=CARTESIAN_POINT('',(30.410451051658,2.67170473125694,31.5905494329235));
#71281=CARTESIAN_POINT('Ctrl Pts',(30.4104510516555,2.67170473126603,31.5905494329321));
#71282=CARTESIAN_POINT('Ctrl Pts',(30.4057463283736,2.68911055926674,31.6070390220085));
#71283=CARTESIAN_POINT('Ctrl Pts',(30.4009837827894,2.70673030952925,31.6237706303625));
#71284=CARTESIAN_POINT('',(30.4352400186108,2.66777854459989,31.5905494329235));
#71285=CARTESIAN_POINT('Origin',(30.4237273077485,2.6753090233822,31.5962059100614));
#71286=CARTESIAN_POINT('',(30.4550674252877,2.69816430208816,31.6237706303691));
#71287=CARTESIAN_POINT('Ctrl Pts',(30.4550674252837,2.69816430208208,31.6237706303625));
#71288=CARTESIAN_POINT('Ctrl Pts',(30.4450931729961,2.68287863128927,31.6070390219952));
#71289=CARTESIAN_POINT('Ctrl Pts',(30.4352400186003,2.66777854458381,31.5905494329059));
#71290=CARTESIAN_POINT('',(30.6121152960721,2.6669255383185,31.6237706303691));
#71291=CARTESIAN_POINT('Origin',(30.,-1.32966554433622E-14,31.6237706303681));
#71292=CARTESIAN_POINT('',(30.6188053053131,2.63126513885322,31.5905494329235));
#71293=CARTESIAN_POINT('Ctrl Pts',(30.6188053053114,2.63126513886247,31.5905494329321));
#71294=CARTESIAN_POINT('Ctrl Pts',(30.6154807306465,2.64898643883871,31.6070390220085));
#71295=CARTESIAN_POINT('Ctrl Pts',(30.6121152960735,2.66692553831135,31.6237706303626));
#71296=CARTESIAN_POINT('',(30.6432098110989,2.62540613538819,31.5905494329235));
#71297=CARTESIAN_POINT('Origin',(30.6323233823986,2.63381649164648,31.5962056922849));
#71298=CARTESIAN_POINT('',(30.6653601355536,2.65414258332836,31.6237706303691));
#71299=CARTESIAN_POINT('Ctrl Pts',(30.6653601355491,2.65414258332261,31.6237706303625));
#71300=CARTESIAN_POINT('Ctrl Pts',(30.6542173306446,2.63968660396658,31.6070390219952));
#71301=CARTESIAN_POINT('Ctrl Pts',(30.6432098110871,2.62540613537299,31.5905494329059));
#71302=CARTESIAN_POINT('',(30.8194729150074,2.61067828431427,31.6237706303691));
#71303=CARTESIAN_POINT('Origin',(30.,-1.32966554433622E-14,31.6237706303681));
#71304=CARTESIAN_POINT('',(30.8233444184872,2.57460292188402,31.5905494329235));
#71305=CARTESIAN_POINT('Ctrl Pts',(30.8233444184862,2.57460292189339,31.5905494329321));
#71306=CARTESIAN_POINT('Ctrl Pts',(30.8214204895467,2.59253043613788,31.6070390220085));
#71307=CARTESIAN_POINT('Ctrl Pts',(30.8194729150082,2.61067828430704,31.6237706303625));
#71308=CARTESIAN_POINT('',(30.8472140012126,2.5668472243157,31.5905494329235));
#71309=CARTESIAN_POINT('Origin',(30.837020957759,2.57608565616362,31.596205527432));
#71310=CARTESIAN_POINT('',(30.8715506793291,2.59375719295037,31.6237706303691));
#71311=CARTESIAN_POINT('Ctrl Pts',(30.8715506793242,2.59375719294498,31.6237706303625));
#71312=CARTESIAN_POINT('Ctrl Pts',(30.8593080209003,2.58022003094555,31.6070390219952));
#71313=CARTESIAN_POINT('Ctrl Pts',(30.8472140011997,2.56684722430147,31.5905494329059));
#71314=CARTESIAN_POINT('',(31.0217782109193,2.53833533054861,31.6237706303691));
#71315=CARTESIAN_POINT('Origin',(30.,-1.32966554433622E-14,31.6237706303681));
#71316=CARTESIAN_POINT('',(31.0228073395316,2.50206742175906,31.5905494329235));
#71317=CARTESIAN_POINT('Ctrl Pts',(31.0228073395313,2.50206742176848,31.5905494329321));
#71318=CARTESIAN_POINT('Ctrl Pts',(31.022295917979,2.52009062119439,31.6070390220085));
#71319=CARTESIAN_POINT('Ctrl Pts',(31.0217782109195,2.53833533054134,31.6237706303625));
#71320=CARTESIAN_POINT('',(31.0459948352816,2.49246284654197,31.5905494329235));
#71321=CARTESIAN_POINT('Origin',(31.0365580110689,2.5024724328509,31.5962053997573));
#71322=CARTESIAN_POINT('',(31.0723678233466,2.51738042696606,31.6237706303691));
#71323=CARTESIAN_POINT('Ctrl Pts',(31.0723678233413,2.51738042696106,31.6237706303625));
#71324=CARTESIAN_POINT('Ctrl Pts',(31.0591007914584,2.50484554342351,31.6070390219952));
#71325=CARTESIAN_POINT('Ctrl Pts',(31.0459948352676,2.49246284652878,31.5905494329059));
#71326=CARTESIAN_POINT('',(31.2177839043852,2.45034269538797,31.6237706303691));
#71327=CARTESIAN_POINT('Origin',(30.,-1.32966554433622E-14,31.6237706303681));
#71328=CARTESIAN_POINT('',(31.2159643132099,2.41410584395711,31.5905494329235));
#71329=CARTESIAN_POINT('Ctrl Pts',(31.2159643132104,2.41410584396651,31.5905494329321));
#71330=CARTESIAN_POINT('Ctrl Pts',(31.216868552129,2.43211360955606,31.6070390220085));
#71331=CARTESIAN_POINT('Ctrl Pts',(31.2177839043849,2.4503426953807,31.6237706303625));
#71332=CARTESIAN_POINT('',(31.2383267633625,2.40271160649132,31.5905494329235));
#71333=CARTESIAN_POINT('Origin',(31.2297043338602,2.41343066267493,31.5962052993351));
#71334=CARTESIAN_POINT('',(31.2665734631346,2.42548317353555,31.6237706303691));
#71335=CARTESIAN_POINT('Ctrl Pts',(31.266573463129,2.42548317353098,31.6237706303625));
#71336=CARTESIAN_POINT('Ctrl Pts',(31.2523638534503,2.4140278501806,31.6070390219952));
#71337=CARTESIAN_POINT('Ctrl Pts',(31.2383267633475,2.40271160647926,31.5905494329059));
#71338=CARTESIAN_POINT('',(31.4062815551263,2.34724288268863,31.6237706303691));
#71339=CARTESIAN_POINT('Origin',(30.,-1.32966554433622E-14,31.6237706303681));
#71340=CARTESIAN_POINT('',(31.401624462548,2.3112605008555,31.5905494329235));
#71341=CARTESIAN_POINT('Ctrl Pts',(31.4016244625492,2.31126050086484,31.5905494329321));
#71342=CARTESIAN_POINT('Ctrl Pts',(31.4039387870053,2.32914180875499,31.6070390220085));
#71343=CARTESIAN_POINT('Ctrl Pts',(31.4062815551254,2.34724288268141,31.6237706303625));
#71344=CARTESIAN_POINT('',(31.4230239951618,2.29814685040396,31.5905494329235));
#71345=CARTESIAN_POINT('Origin',(31.4152691174526,2.30950931155475,31.5962052196244));
#71346=CARTESIAN_POINT('',(31.452970256344,2.3186320097852,31.6237706303691));
#71347=CARTESIAN_POINT('Ctrl Pts',(31.452970256338,2.31863200978109,31.6237706303625));
#71348=CARTESIAN_POINT('Ctrl Pts',(31.4379056758324,2.30832687249561,31.6070390219952));
#71349=CARTESIAN_POINT('Ctrl Pts',(31.4230239951459,2.2981468503931,31.5905494329059));
#71350=CARTESIAN_POINT('',(31.5861090124439,2.22967153708005,31.6237706303691));
#71351=CARTESIAN_POINT('Origin',(30.,-1.32966554433622E-14,31.6237706303681));
#71352=CARTESIAN_POINT('',(31.5786431309871,2.19416546819402,31.5905494329235));
#71353=CARTESIAN_POINT('Ctrl Pts',(31.578643130989,2.19416546820324,31.5905494329321));
#71354=CARTESIAN_POINT('Ctrl Pts',(31.5823532724027,2.21181007418469,31.6070390220085));
#71355=CARTESIAN_POINT('Ctrl Pts',(31.5861090124425,2.22967153707293,31.6237706303625));
#71356=CARTESIAN_POINT('',(31.5989478108274,2.17941325477248,31.5905494329235));
#71357=CARTESIAN_POINT('Origin',(31.5921082951429,2.19134908471604,31.596205156165));
#71358=CARTESIAN_POINT('',(31.6304090047614,2.19748570867114,31.6237706303691));
#71359=CARTESIAN_POINT('Ctrl Pts',(31.6304090047551,2.19748570866755,31.6237706303626));
#71360=CARTESIAN_POINT('Ctrl Pts',(31.6145823315708,2.18839429204514,31.6070390219952));
#71361=CARTESIAN_POINT('Ctrl Pts',(31.5989478108108,2.17941325476293,31.5905494329059));
#71362=CARTESIAN_POINT('',(31.7561575802651,2.09835352500435,31.6237706303691));
#71363=CARTESIAN_POINT('Origin',(30.,-1.32966554433622E-14,31.6237706303681));
#71364=CARTESIAN_POINT('',(31.7459289395715,2.06354267578706,31.5905494329235));
#71365=CARTESIAN_POINT('Ctrl Pts',(31.7459289395742,2.06354267579611,31.5905494329321));
#71366=CARTESIAN_POINT('Ctrl Pts',(31.7510120236898,2.08084179500558,31.6070390220085));
#71367=CARTESIAN_POINT('Ctrl Pts',(31.7561575802631,2.09835352499738,31.6237706303625));
#71368=CARTESIAN_POINT('',(31.7650135815352,2.04724285169688,31.5905494329235));
#71369=CARTESIAN_POINT('Origin',(31.7591315960216,2.05967847590828,31.5962051058414));
#71370=CARTESIAN_POINT('',(31.7977957394984,2.06279117742498,31.6237706303691));
#71371=CARTESIAN_POINT('Ctrl Pts',(31.7977957394918,2.06279117742187,31.6237706303625));
#71372=CARTESIAN_POINT('Ctrl Pts',(31.781304550332,2.05496953306921,31.6070390219952));
#71373=CARTESIAN_POINT('Ctrl Pts',(31.7650135815179,2.04724285168864,31.5905494329059));
#71374=CARTESIAN_POINT('',(31.9153788526223,1.95409846567364,31.6237706303691));
#71375=CARTESIAN_POINT('Origin',(30.,-1.32966554433622E-14,31.6237706303681));
#71376=CARTESIAN_POINT('',(31.9024505156632,1.9201974565863,31.5905494329235));
#71377=CARTESIAN_POINT('Ctrl Pts',(31.9024505156666,1.92019745659511,31.5905494329321));
#71378=CARTESIAN_POINT('Ctrl Pts',(31.9088752035804,1.93704443421013,31.6070390220085));
#71379=CARTESIAN_POINT('Ctrl Pts',(31.9153788526197,1.95409846566686,31.6237706303625));
#71380=CARTESIAN_POINT('',(31.9201974565863,1.90245051566323,31.5905494329235));
#71381=CARTESIAN_POINT('Origin',(31.9153092670123,1.91530927561703,31.596205066438));
#71382=CARTESIAN_POINT('',(31.9540984656736,1.91537885262231,31.6237706303691));
#71383=CARTESIAN_POINT('Ctrl Pts',(31.9540984656668,1.9153788526197,31.6237706303625));
#71384=CARTESIAN_POINT('Ctrl Pts',(31.9370444341966,1.90887520357521,31.6070390219952));
#71385=CARTESIAN_POINT('Ctrl Pts',(31.9201974565683,1.90245051565638,31.5905494329059));
#71386=CARTESIAN_POINT('',(32.062791177425,1.79779573949838,31.6237706303691));
#71387=CARTESIAN_POINT('Origin',(30.,-1.32966554433622E-14,31.6237706303681));
#71388=CARTESIAN_POINT('',(32.0472428516969,1.76501358153524,31.5905494329235));
#71389=CARTESIAN_POINT('Ctrl Pts',(32.0472428517009,1.76501358154374,31.5905494329321));
#71390=CARTESIAN_POINT('Ctrl Pts',(32.0549695330754,1.78130455034511,31.6070390220085));
#71391=CARTESIAN_POINT('Ctrl Pts',(32.0627911774219,1.7977957394918,31.6237706303625));
#71392=CARTESIAN_POINT('',(32.0635426757871,1.74592893957153,31.5905494329235));
#71393=CARTESIAN_POINT('Origin',(32.059678421746,1.75913156587022,31.5962050363748));
#71394=CARTESIAN_POINT('',(32.0983535250043,1.75615758026513,31.6237706303691));
#71395=CARTESIAN_POINT('Ctrl Pts',(32.0983535249974,1.75615758026307,31.6237706303625));
#71396=CARTESIAN_POINT('Ctrl Pts',(32.0808417949917,1.75101202368577,31.6070390219952));
#71397=CARTESIAN_POINT('Ctrl Pts',(32.0635426757687,1.74592893956612,31.5905494329059));
#71398=CARTESIAN_POINT('',(32.1974857086711,1.63040900476136,31.6237706303691));
#71399=CARTESIAN_POINT('Origin',(30.,-1.32966554433622E-14,31.6237706303681));
#71400=CARTESIAN_POINT('',(32.1794132547725,1.59894781082743,31.5905494329235));
#71401=CARTESIAN_POINT('Ctrl Pts',(32.1794132547772,1.59894781083559,31.5905494329321));
#71402=CARTESIAN_POINT('Ctrl Pts',(32.1883942920524,1.61458233158336,31.6070390220085));
#71403=CARTESIAN_POINT('Ctrl Pts',(32.1974857086675,1.63040900475503,31.6237706303625));
#71404=CARTESIAN_POINT('',(32.194165468194,1.57864313098709,31.5905494329235));
#71405=CARTESIAN_POINT('Origin',(32.1913489771416,1.59210823242537,31.5962050145327));
#71406=CARTESIAN_POINT('',(32.22967153708,1.58610901244395,31.6237706303691));
#71407=CARTESIAN_POINT('Ctrl Pts',(32.2296715370729,1.58610901244245,31.6237706303625));
#71408=CARTESIAN_POINT('Ctrl Pts',(32.2118100741705,1.58235327239971,31.6070390219952));
#71409=CARTESIAN_POINT('Ctrl Pts',(32.1941654681752,1.57864313098313,31.5905494329059));
#71410=CARTESIAN_POINT('',(32.3186320097852,1.45297025634397,31.6237706303691));
#71411=CARTESIAN_POINT('Origin',(30.,-1.32966554433622E-14,31.6237706303681));
#71412=CARTESIAN_POINT('',(32.298146850404,1.42302399516178,31.5905494329235));
#71413=CARTESIAN_POINT('Ctrl Pts',(32.2981468504093,1.42302399516954,31.5905494329321));
#71414=CARTESIAN_POINT('Ctrl Pts',(32.3083268725038,1.43790567584429,31.6070390220085));
#71415=CARTESIAN_POINT('Ctrl Pts',(32.3186320097811,1.45297025633794,31.6237706303625));
#71416=CARTESIAN_POINT('',(32.3112605008555,1.401624462548,31.5905494329235));
#71417=CARTESIAN_POINT('Origin',(32.3095091411128,1.41526902814876,31.596205000146));
#71418=CARTESIAN_POINT('',(32.3472428826886,1.40628155512629,31.6237706303691));
#71419=CARTESIAN_POINT('Ctrl Pts',(32.3472428826814,1.40628155512536,31.6237706303625));
#71420=CARTESIAN_POINT('Ctrl Pts',(32.3291418087406,1.40393878700346,31.6070390219952));
#71421=CARTESIAN_POINT('Ctrl Pts',(32.3112605008365,1.40162446254554,31.5905494329059));
#71422=CARTESIAN_POINT('',(32.4254831735355,1.26657346313459,31.6237706303691));
#71423=CARTESIAN_POINT('Origin',(30.,-1.32966554433622E-14,31.6237706303681));
#71424=CARTESIAN_POINT('',(32.4027116064913,1.23832676336245,31.5905494329235));
#71425=CARTESIAN_POINT('Ctrl Pts',(32.4027116064972,1.23832676336979,31.5905494329321));
#71426=CARTESIAN_POINT('Ctrl Pts',(32.4140278501897,1.2523638534615,31.6070390220085));
#71427=CARTESIAN_POINT('Ctrl Pts',(32.425483173531,1.26657346312893,31.6237706303625));
#71428=CARTESIAN_POINT('',(32.4141058439571,1.21596431320987,31.5905494329235));
#71429=CARTESIAN_POINT('Origin',(32.4134304175703,1.22970422416531,31.5962049927334));
#71430=CARTESIAN_POINT('',(32.450342695388,1.21778390438521,31.6237706303691));
#71431=CARTESIAN_POINT('Ctrl Pts',(32.4503426953807,1.21778390438485,31.6237706303625));
#71432=CARTESIAN_POINT('Ctrl Pts',(32.4321136095416,1.2168685521283,31.6070390219952));
#71433=CARTESIAN_POINT('Ctrl Pts',(32.4141058439379,1.21596431320891,31.5905494329059));
#71434=CARTESIAN_POINT('',(32.517380426966,1.07236782334656,31.6237706303691));
#71435=CARTESIAN_POINT('Origin',(30.,-1.32966554433622E-14,31.6237706303681));
#71436=CARTESIAN_POINT('',(32.492462846542,1.04599483528156,31.5905494329235));
#71437=CARTESIAN_POINT('Ctrl Pts',(32.4924628465485,1.04599483528841,31.5905494329321));
#71438=CARTESIAN_POINT('Ctrl Pts',(32.5048455434335,1.05910079146886,31.6070390220085));
#71439=CARTESIAN_POINT('Ctrl Pts',(32.5173804269611,1.07236782334125,31.6237706303625));
#71440=CARTESIAN_POINT('',(32.5020674217591,1.02280733953163,31.5905494329235));
#71441=CARTESIAN_POINT('Origin',(32.5024720978725,1.03655788791103,31.5962049920587));
#71442=CARTESIAN_POINT('',(32.5383353305486,1.02177821091935,31.6237706303691));
#71443=CARTESIAN_POINT('Ctrl Pts',(32.5383353305413,1.02177821091956,31.6237706303625));
#71444=CARTESIAN_POINT('Ctrl Pts',(32.5200906211799,1.02229591797942,31.6070390219952));
#71445=CARTESIAN_POINT('Ctrl Pts',(32.5020674217399,1.02280733953218,31.5905494329059));
#71446=CARTESIAN_POINT('',(32.5937571929504,0.87155067932912,31.6237706303691));
#71447=CARTESIAN_POINT('Origin',(30.,-1.32966554433622E-14,31.6237706303681));
#71448=CARTESIAN_POINT('',(32.5668472243157,0.84721400121258,31.5905494329235));
#71449=CARTESIAN_POINT('Ctrl Pts',(32.5668472243227,0.847214001218895,31.5905494329321));
#71450=CARTESIAN_POINT('Ctrl Pts',(32.5802200309563,0.859308020910075,31.6070390220085));
#71451=CARTESIAN_POINT('Ctrl Pts',(32.593757192945,0.871550679324244,31.6237706303625));
#71452=CARTESIAN_POINT('',(32.574602921884,0.823344418487232,31.5905494329235));
#71453=CARTESIAN_POINT('Origin',(32.5760852110325,0.837020829522203,31.5962049981138));
#71454=CARTESIAN_POINT('',(32.6106782843143,0.819472915007436,31.6237706303691));
#71455=CARTESIAN_POINT('Ctrl Pts',(32.6106782843071,0.819472915008212,31.6237706303625));
#71456=CARTESIAN_POINT('Ctrl Pts',(32.5925304361235,0.8214204895483,31.6070390219952));
#71457=CARTESIAN_POINT('Ctrl Pts',(32.5746029218649,0.823344418489286,31.5905494329059));
#71458=CARTESIAN_POINT('',(32.6541425833284,0.665360135553601,31.6237706303691));
#71459=CARTESIAN_POINT('Origin',(30.,-1.32966554433622E-14,31.6237706303681));
#71460=CARTESIAN_POINT('',(32.6254061353882,0.64320981109888,31.5905494329235));
#71461=CARTESIAN_POINT('Ctrl Pts',(32.6254061353957,0.643209811104633,31.5905494329321));
#71462=CARTESIAN_POINT('Ctrl Pts',(32.639686603978,0.654217330653466,31.6070390220085));
#71463=CARTESIAN_POINT('Ctrl Pts',(32.6541425833226,0.665360135549173,31.6237706303625));
#71464=CARTESIAN_POINT('',(32.6312651388532,0.618805305313054,31.5905494329235));
#71465=CARTESIAN_POINT('Origin',(32.633815908334,0.632323260043002,31.5962050111235));
#71466=CARTESIAN_POINT('',(32.6669255383185,0.612115296072106,31.6237706303691));
#71467=CARTESIAN_POINT('Ctrl Pts',(32.6669255383114,0.61211529607344,31.6237706303625));
#71468=CARTESIAN_POINT('Ctrl Pts',(32.6489864388245,0.61548073064908,31.6070390219952));
#71469=CARTESIAN_POINT('Ctrl Pts',(32.6312651388343,0.618805305316593,31.5905494329059));
#71470=CARTESIAN_POINT('',(32.6981643020882,0.455067425287697,31.6237706303691));
#71471=CARTESIAN_POINT('Origin',(30.,-1.32966554433622E-14,31.6237706303681));
#71472=CARTESIAN_POINT('',(32.6677785445999,0.435240018610789,31.5905494329235));
#71473=CARTESIAN_POINT('Ctrl Pts',(32.6677785446078,0.435240018615936,31.5905494329321));
#71474=CARTESIAN_POINT('Ctrl Pts',(32.6828786313014,0.44509317300403,31.6070390220085));
#71475=CARTESIAN_POINT('Ctrl Pts',(32.6981643020821,0.455067425283731,31.6237706303625));
#71476=CARTESIAN_POINT('',(32.6717047312569,0.410451051657977,31.5905494329235));
#71477=CARTESIAN_POINT('Origin',(32.6753082614925,0.423727206709275,31.596205031575));
#71478=CARTESIAN_POINT('',(32.7067303095363,0.400983782787501,31.6237706303691));
#71479=CARTESIAN_POINT('Ctrl Pts',(32.7067303095293,0.400983782789396,31.6237706303625));
#71480=CARTESIAN_POINT('Ctrl Pts',(32.6891105592528,0.405746328377311,31.6070390219952));
#71481=CARTESIAN_POINT('Ctrl Pts',(32.6717047312384,0.410451051662997,31.5905494329059));
#71482=CARTESIAN_POINT('',(32.7255509406949,0.24196907301962,31.6237706303691));
#71483=CARTESIAN_POINT('Origin',(30.,-1.32966554433622E-14,31.6237706303681));
#71484=CARTESIAN_POINT('',(32.6937032119577,0.224586826675969,31.5905494329235));
#71485=CARTESIAN_POINT('Ctrl Pts',(32.693703211966,0.224586826680493,31.5905494329321));
#71486=CARTESIAN_POINT('Ctrl Pts',(32.7095298197151,0.233224867934539,31.6070390220085));
#71487=CARTESIAN_POINT('Ctrl Pts',(32.7255509406885,0.241969073016156,31.6237706303625));
#71488=CARTESIAN_POINT('',(32.6956723755605,0.199566230780603,31.5905494329235));
#71489=CARTESIAN_POINT('Origin',(32.7003064571198,0.212518732061222,31.5962050602857));
#71490=CARTESIAN_POINT('',(32.7298471883166,0.187380071141372,31.6237706303691));
#71491=CARTESIAN_POINT('Ctrl Pts',(32.7298471883097,0.187380071143799,31.6237706303625));
#71492=CARTESIAN_POINT('Ctrl Pts',(32.7126554188632,0.193510365066728,31.6070390219952));
#71493=CARTESIAN_POINT('Ctrl Pts',(32.6956723755424,0.199566230787043,31.5905494329059));
#71494=CARTESIAN_POINT('',(32.7361336514146,0.0273789009534945,31.6237706303691));
#71495=CARTESIAN_POINT('Origin',(30.,-1.32966554433622E-14,31.6237706303681));
#71496=CARTESIAN_POINT('',(32.7030203032667,0.0125489822719939,31.5905494329235));
#71497=CARTESIAN_POINT('Ctrl Pts',(32.7030203032753,0.0125489822758371,
31.5905494329321));
#71498=CARTESIAN_POINT('Ctrl Pts',(32.7194758557802,0.0199186539990537,
31.6070390220085));
#71499=CARTESIAN_POINT('Ctrl Pts',(32.736133651408,0.0273789009505039,31.6237706303625));
#71500=CARTESIAN_POINT('',(32.7030203032667,-0.0125489822720396,31.5905494329235));
#71501=CARTESIAN_POINT('Origin',(32.7086563646858,6.24424376688964E-9,31.5962050859813));
#71502=CARTESIAN_POINT('',(32.7361336514146,-0.02737890095354,31.6237706303691));
#71503=CARTESIAN_POINT('Ctrl Pts',(32.736133651408,-0.0273789009505768,
31.6237706303625));
#71504=CARTESIAN_POINT('Ctrl Pts',(32.719475855767,-0.0199186539932038,
31.6070390219952));
#71505=CARTESIAN_POINT('Ctrl Pts',(32.7030203032491,-0.0125489822642076,
31.5905494329059));
#71506=CARTESIAN_POINT('',(32.7298471883166,-0.187380071141418,31.6237706303691));
#71507=CARTESIAN_POINT('Origin',(30.,-1.32966554433622E-14,31.6237706303681));
#71508=CARTESIAN_POINT('',(32.6956723755605,-0.199566230780649,31.5905494329235));
#71509=CARTESIAN_POINT('Ctrl Pts',(32.6956723755694,-0.199566230777489,
31.5905494329321));
#71510=CARTESIAN_POINT('Ctrl Pts',(32.7126554188769,-0.193510365061924,
31.6070390220085));
#71511=CARTESIAN_POINT('Ctrl Pts',(32.7298471883097,-0.187380071143864,
31.6237706303625));
#71512=CARTESIAN_POINT('',(32.6937032119577,-0.224586826676015,31.5905494329235));
#71513=CARTESIAN_POINT('Origin',(32.7003074588902,-0.212518788369472,31.5962062072437));
#71514=CARTESIAN_POINT('',(32.7255509406949,-0.241969073019665,31.6237706303691));
#71515=CARTESIAN_POINT('Ctrl Pts',(32.7255509406885,-0.241969073016199,
31.6237706303625));
#71516=CARTESIAN_POINT('Ctrl Pts',(32.7095298197024,-0.23322486792764,31.6070390219952));
#71517=CARTESIAN_POINT('Ctrl Pts',(32.6937032119408,-0.22458682666682,31.5905494329059));
#71518=CARTESIAN_POINT('',(32.7067303095363,-0.400983782787547,31.6237706303691));
#71519=CARTESIAN_POINT('Origin',(30.,-1.32966554433622E-14,31.6237706303681));
#71520=CARTESIAN_POINT('',(32.6717047312569,-0.410451051658023,31.5905494329235));
#71521=CARTESIAN_POINT('Ctrl Pts',(32.671704731266,-0.41045105165556,31.5905494329321));
#71522=CARTESIAN_POINT('Ctrl Pts',(32.6891105592667,-0.405746328373564,
31.6070390220085));
#71523=CARTESIAN_POINT('Ctrl Pts',(32.7067303095293,-0.40098378278943,31.6237706303625));
#71524=CARTESIAN_POINT('',(32.6677785445999,-0.435240018610835,31.5905494329235));
#71525=CARTESIAN_POINT('Origin',(32.6753090233822,-0.42372730774851,31.5962059100614));
#71526=CARTESIAN_POINT('',(32.6981643020882,-0.455067425287743,31.6237706303691));
#71527=CARTESIAN_POINT('Ctrl Pts',(32.6981643020821,-0.455067425283808,
31.6237706303625));
#71528=CARTESIAN_POINT('Ctrl Pts',(32.6828786312893,-0.445093172996188,
31.6070390219952));
#71529=CARTESIAN_POINT('Ctrl Pts',(32.6677785445838,-0.435240018600367,
31.5905494329059));
#71530=CARTESIAN_POINT('',(32.6669255383185,-0.612115296072152,31.6237706303691));
#71531=CARTESIAN_POINT('Origin',(30.,-1.32966554433622E-14,31.6237706303681));
#71532=CARTESIAN_POINT('',(32.6312651388532,-0.6188053053131,31.5905494329235));
#71533=CARTESIAN_POINT('Ctrl Pts',(32.6312651388625,-0.618805305311361,
31.5905494329321));
#71534=CARTESIAN_POINT('Ctrl Pts',(32.6489864388387,-0.615480730646455,
31.6070390220085));
#71535=CARTESIAN_POINT('Ctrl Pts',(32.6669255383114,-0.612115296073488,
31.6237706303625));
#71536=CARTESIAN_POINT('',(32.6254061353882,-0.643209811098926,31.5905494329235));
#71537=CARTESIAN_POINT('Origin',(32.6338164916465,-0.632323382398633,31.5962056922849));
#71538=CARTESIAN_POINT('',(32.6541425833284,-0.665360135553646,31.6237706303691));
#71539=CARTESIAN_POINT('Ctrl Pts',(32.6541425833226,-0.665360135549238,
31.6237706303625));
#71540=CARTESIAN_POINT('Ctrl Pts',(32.6396866039666,-0.654217330644686,
31.6070390219952));
#71541=CARTESIAN_POINT('Ctrl Pts',(32.625406135373,-0.643209811087222,31.5905494329059));
#71542=CARTESIAN_POINT('',(32.6106782843143,-0.819472915007481,31.6237706303691));
#71543=CARTESIAN_POINT('Origin',(30.,-1.32966554433622E-14,31.6237706303681));
#71544=CARTESIAN_POINT('',(32.574602921884,-0.823344418487278,31.5905494329235));
#71545=CARTESIAN_POINT('Ctrl Pts',(32.5746029218934,-0.823344418486272,
31.5905494329321));
#71546=CARTESIAN_POINT('Ctrl Pts',(32.5925304361379,-0.821420489546795,
31.6070390220085));
#71547=CARTESIAN_POINT('Ctrl Pts',(32.610678284307,-0.819472915008254,31.6237706303626));
#71548=CARTESIAN_POINT('',(32.5668472243157,-0.847214001212625,31.5905494329235));
#71549=CARTESIAN_POINT('Origin',(32.5760856561636,-0.837020957759021,31.596205527432));
#71550=CARTESIAN_POINT('',(32.5937571929504,-0.871550679329165,31.6237706303691));
#71551=CARTESIAN_POINT('Ctrl Pts',(32.593757192945,-0.871550679324299,31.6237706303625));
#71552=CARTESIAN_POINT('Ctrl Pts',(32.5802200309455,-0.859308020900409,
31.6070390219952));
#71553=CARTESIAN_POINT('Ctrl Pts',(32.5668472243014,-0.847214001199744,
31.5905494329059));
#71554=CARTESIAN_POINT('',(32.5383353305486,-1.02177821091939,31.6237706303691));
#71555=CARTESIAN_POINT('Origin',(30.,-1.32966554433622E-14,31.6237706303681));
#71556=CARTESIAN_POINT('',(32.5020674217591,-1.02280733953168,31.5905494329235));
#71557=CARTESIAN_POINT('Ctrl Pts',(32.5020674217685,-1.02280733953141,31.5905494329321));
#71558=CARTESIAN_POINT('Ctrl Pts',(32.5200906211944,-1.02229591797905,31.6070390220085));
#71559=CARTESIAN_POINT('Ctrl Pts',(32.5383353305413,-1.0217782109196,31.6237706303625));
#71560=CARTESIAN_POINT('',(32.492462846542,-1.0459948352816,31.5905494329235));
#71561=CARTESIAN_POINT('Origin',(32.5024724328509,-1.03655801106895,31.5962053997573));
#71562=CARTESIAN_POINT('',(32.517380426966,-1.07236782334661,31.6237706303691));
#71563=CARTESIAN_POINT('Ctrl Pts',(32.517380426961,-1.07236782334134,31.6237706303625));
#71564=CARTESIAN_POINT('Ctrl Pts',(32.5048455434235,-1.0591007914584,31.6070390219952));
#71565=CARTESIAN_POINT('Ctrl Pts',(32.4924628465288,-1.04599483526767,31.5905494329059));
#71566=CARTESIAN_POINT('',(32.450342695388,-1.21778390438525,31.6237706303691));
#71567=CARTESIAN_POINT('Origin',(30.,-1.32966554433622E-14,31.6237706303681));
#71568=CARTESIAN_POINT('',(32.4141058439571,-1.21596431320991,31.5905494329235));
#71569=CARTESIAN_POINT('Ctrl Pts',(32.4141058439665,-1.21596431321038,31.5905494329321));
#71570=CARTESIAN_POINT('Ctrl Pts',(32.4321136095561,-1.21686855212907,31.6070390220085));
#71571=CARTESIAN_POINT('Ctrl Pts',(32.4503426953807,-1.21778390438489,31.6237706303625));
#71572=CARTESIAN_POINT('',(32.4027116064913,-1.2383267633625,31.5905494329235));
#71573=CARTESIAN_POINT('Origin',(32.4134306626749,-1.2297043338603,31.5962052993351));
#71574=CARTESIAN_POINT('',(32.4254831735355,-1.26657346313463,31.6237706303691));
#71575=CARTESIAN_POINT('Ctrl Pts',(32.425483173531,-1.26657346312898,31.6237706303625));
#71576=CARTESIAN_POINT('Ctrl Pts',(32.4140278501806,-1.25236385345028,31.6070390219952));
#71577=CARTESIAN_POINT('Ctrl Pts',(32.4027116064792,-1.23832676334755,31.5905494329059));
#71578=CARTESIAN_POINT('',(32.3472428826886,-1.40628155512633,31.6237706303691));
#71579=CARTESIAN_POINT('Origin',(30.,-1.32966554433622E-14,31.6237706303681));
#71580=CARTESIAN_POINT('',(32.3112605008555,-1.40162446254804,31.5905494329235));
#71581=CARTESIAN_POINT('Ctrl Pts',(32.3112605008648,-1.40162446254925,31.5905494329321));
#71582=CARTESIAN_POINT('Ctrl Pts',(32.329141808755,-1.40393878700536,31.6070390220085));
#71583=CARTESIAN_POINT('Ctrl Pts',(32.3472428826814,-1.4062815551254,31.6237706303625));
#71584=CARTESIAN_POINT('',(32.2981468504039,-1.42302399516182,31.5905494329235));
#71585=CARTESIAN_POINT('Origin',(32.3095093115547,-1.41526911745265,31.5962052196244));
#71586=CARTESIAN_POINT('',(32.3186320097852,-1.45297025634402,31.6237706303691));
#71587=CARTESIAN_POINT('Ctrl Pts',(32.3186320097811,-1.45297025633802,31.6237706303625));
#71588=CARTESIAN_POINT('Ctrl Pts',(32.3083268724956,-1.43790567583238,31.6070390219952));
#71589=CARTESIAN_POINT('Ctrl Pts',(32.2981468503931,-1.42302399514595,31.5905494329059));
#71590=CARTESIAN_POINT('',(32.22967153708,-1.58610901244399,31.6237706303691));
#71591=CARTESIAN_POINT('Origin',(30.,-1.32966554433622E-14,31.6237706303681));
#71592=CARTESIAN_POINT('',(32.194165468194,-1.57864313098713,31.5905494329235));
#71593=CARTESIAN_POINT('Ctrl Pts',(32.1941654682032,-1.57864313098907,31.5905494329321));
#71594=CARTESIAN_POINT('Ctrl Pts',(32.2118100741847,-1.58235327240274,31.6070390220085));
#71595=CARTESIAN_POINT('Ctrl Pts',(32.2296715370729,-1.58610901244249,31.6237706303625));
#71596=CARTESIAN_POINT('',(32.1794132547725,-1.59894781082747,31.5905494329235));
#71597=CARTESIAN_POINT('Origin',(32.191349084716,-1.59210829514296,31.596205156165));
#71598=CARTESIAN_POINT('',(32.1974857086711,-1.6304090047614,31.6237706303691));
#71599=CARTESIAN_POINT('Ctrl Pts',(32.1974857086675,-1.63040900475512,31.6237706303625));
#71600=CARTESIAN_POINT('Ctrl Pts',(32.1883942920451,-1.61458233157088,31.6070390219952));
#71601=CARTESIAN_POINT('Ctrl Pts',(32.1794132547629,-1.59894781081085,31.5905494329059));
#71602=CARTESIAN_POINT('',(32.0983535250043,-1.75615758026517,31.6237706303691));
#71603=CARTESIAN_POINT('Origin',(30.,-1.32966554433622E-14,31.6237706303681));
#71604=CARTESIAN_POINT('',(32.063542675787,-1.74592893957158,31.5905494329235));
#71605=CARTESIAN_POINT('Ctrl Pts',(32.0635426757961,-1.74592893957424,31.5905494329321));
#71606=CARTESIAN_POINT('Ctrl Pts',(32.0808417950055,-1.75101202368991,31.6070390220085));
#71607=CARTESIAN_POINT('Ctrl Pts',(32.0983535249973,-1.75615758026313,31.6237706303625));
#71608=CARTESIAN_POINT('',(32.0472428516969,-1.76501358153528,31.5905494329235));
#71609=CARTESIAN_POINT('Origin',(32.0596784759083,-1.75913159602171,31.5962051058414));
#71610=CARTESIAN_POINT('',(32.062791177425,-1.79779573949842,31.6237706303691));
#71611=CARTESIAN_POINT('Ctrl Pts',(32.0627911774219,-1.79779573949184,31.6237706303625));
#71612=CARTESIAN_POINT('Ctrl Pts',(32.0549695330692,-1.78130455033205,31.6070390219952));
#71613=CARTESIAN_POINT('Ctrl Pts',(32.0472428516887,-1.76501358151791,31.5905494329059));
#71614=CARTESIAN_POINT('',(31.9540984656736,-1.91537885262235,31.6237706303691));
#71615=CARTESIAN_POINT('Origin',(30.,-1.32966554433622E-14,31.6237706303681));
#71616=CARTESIAN_POINT('',(31.9201974565863,-1.90245051566327,31.5905494329235));
#71617=CARTESIAN_POINT('Ctrl Pts',(31.9201974565951,-1.90245051566663,31.5905494329321));
#71618=CARTESIAN_POINT('Ctrl Pts',(31.9370444342101,-1.90887520358042,31.6070390220085));
#71619=CARTESIAN_POINT('Ctrl Pts',(31.9540984656668,-1.91537885261975,31.6237706303625));
#71620=CARTESIAN_POINT('',(31.9024505156632,-1.92019745658634,31.5905494329235));
#71621=CARTESIAN_POINT('Origin',(31.915309275617,-1.91530926701241,31.5962050664381));
#71622=CARTESIAN_POINT('',(31.9153788526223,-1.95409846567368,31.6237706303691));
#71623=CARTESIAN_POINT('Ctrl Pts',(31.9153788526197,-1.9540984656669,31.6237706303625));
#71624=CARTESIAN_POINT('Ctrl Pts',(31.9088752035752,-1.93704443419662,31.6070390219952));
#71625=CARTESIAN_POINT('Ctrl Pts',(31.9024505156564,-1.92019745656839,31.5905494329059));
#71626=CARTESIAN_POINT('',(31.7977957394984,-2.06279117742501,31.6237706303691));
#71627=CARTESIAN_POINT('Origin',(30.,-1.32966554433622E-14,31.6237706303681));
#71628=CARTESIAN_POINT('',(31.7650135815352,-2.04724285169692,31.5905494329235));
#71629=CARTESIAN_POINT('Ctrl Pts',(31.7650135815437,-2.04724285170096,31.5905494329321));
#71630=CARTESIAN_POINT('Ctrl Pts',(31.7813045503451,-2.05496953307547,31.6070390220085));
#71631=CARTESIAN_POINT('Ctrl Pts',(31.7977957394918,-2.06279117742192,31.6237706303625));
#71632=CARTESIAN_POINT('',(31.7459289395715,-2.0635426757871,31.5905494329235));
#71633=CARTESIAN_POINT('Origin',(31.7591315658702,-2.05967842174604,31.5962050363748));
#71634=CARTESIAN_POINT('',(31.7561575802651,-2.09835352500439,31.6237706303691));
#71635=CARTESIAN_POINT('Ctrl Pts',(31.7561575802631,-2.09835352499741,31.6237706303625));
#71636=CARTESIAN_POINT('Ctrl Pts',(31.7510120236858,-2.08084179499169,31.6070390219952));
#71637=CARTESIAN_POINT('Ctrl Pts',(31.7459289395661,-2.06354267576866,31.5905494329059));
#71638=CARTESIAN_POINT('',(31.6304090047613,-2.19748570867118,31.6237706303691));
#71639=CARTESIAN_POINT('Origin',(30.,-1.32966554433622E-14,31.6237706303681));
#71640=CARTESIAN_POINT('',(31.5989478108274,-2.17941325477251,31.5905494329235));
#71641=CARTESIAN_POINT('Ctrl Pts',(31.5989478108356,-2.17941325477721,31.5905494329321));
#71642=CARTESIAN_POINT('Ctrl Pts',(31.6145823315833,-2.18839429205237,31.6070390220085));
#71643=CARTESIAN_POINT('Ctrl Pts',(31.630409004755,-2.19748570866756,31.6237706303625));
#71644=CARTESIAN_POINT('',(31.5786431309871,-2.19416546819406,31.5905494329235));
#71645=CARTESIAN_POINT('Origin',(31.5921082324253,-2.19134897714169,31.5962050145327));
#71646=CARTESIAN_POINT('',(31.5861090124439,-2.22967153708009,31.6237706303691));
#71647=CARTESIAN_POINT('Ctrl Pts',(31.5861090124425,-2.22967153707296,31.6237706303625));
#71648=CARTESIAN_POINT('Ctrl Pts',(31.5823532723997,-2.21181007417054,31.6070390219952));
#71649=CARTESIAN_POINT('Ctrl Pts',(31.5786431309832,-2.19416546817524,31.5905494329059));
#71650=CARTESIAN_POINT('',(31.452970256344,-2.31863200978524,31.6237706303691));
#71651=CARTESIAN_POINT('Origin',(30.,-1.32966554433622E-14,31.6237706303681));
#71652=CARTESIAN_POINT('',(31.4230239951618,-2.29814685040399,31.5905494329235));
#71653=CARTESIAN_POINT('Ctrl Pts',(31.4230239951696,-2.2981468504093,31.5905494329321));
#71654=CARTESIAN_POINT('Ctrl Pts',(31.4379056758443,-2.30832687250383,31.6070390220085));
#71655=CARTESIAN_POINT('Ctrl Pts',(31.452970256338,-2.31863200978113,31.6237706303625));
#71656=CARTESIAN_POINT('',(31.401624462548,-2.31126050085554,31.5905494329235));
#71657=CARTESIAN_POINT('Origin',(31.4152690281487,-2.30950914111279,31.596205000146));
#71658=CARTESIAN_POINT('',(31.4062815551263,-2.34724288268866,31.6237706303691));
#71659=CARTESIAN_POINT('Ctrl Pts',(31.4062815551254,-2.34724288268144,31.6237706303625));
#71660=CARTESIAN_POINT('Ctrl Pts',(31.4039387870035,-2.32914180874065,31.6070390219952));
#71661=CARTESIAN_POINT('Ctrl Pts',(31.4016244625455,-2.31126050083648,31.5905494329059));
#71662=CARTESIAN_POINT('',(31.2665734631346,-2.42548317353559,31.6237706303691));
#71663=CARTESIAN_POINT('Origin',(30.,-1.32966554433622E-14,31.6237706303681));
#71664=CARTESIAN_POINT('',(31.2383267633624,-2.40271160649135,31.5905494329235));
#71665=CARTESIAN_POINT('Ctrl Pts',(31.2383267633697,-2.40271160649727,31.5905494329321));
#71666=CARTESIAN_POINT('Ctrl Pts',(31.2523638534615,-2.41402785018975,31.6070390220085));
#71667=CARTESIAN_POINT('Ctrl Pts',(31.2665734631289,-2.42548317353104,31.6237706303625));
#71668=CARTESIAN_POINT('',(31.2159643132098,-2.41410584395714,31.5905494329235));
#71669=CARTESIAN_POINT('Origin',(31.2297042241653,-2.41343041757036,31.5962049927334));
#71670=CARTESIAN_POINT('',(31.2177839043852,-2.450342695388,31.6237706303691));
#71671=CARTESIAN_POINT('Ctrl Pts',(31.2177839043848,-2.45034269538075,31.6237706303625));
#71672=CARTESIAN_POINT('Ctrl Pts',(31.2168685521282,-2.43211360954164,31.6070390219952));
#71673=CARTESIAN_POINT('Ctrl Pts',(31.2159643132088,-2.41410584393796,31.5905494329059));
#71674=CARTESIAN_POINT('',(31.0723678233465,-2.51738042696609,31.6237706303691));
#71675=CARTESIAN_POINT('Origin',(30.,-1.32966554433622E-14,31.6237706303681));
#71676=CARTESIAN_POINT('',(31.0459948352815,-2.49246284654201,31.5905494329235));
#71677=CARTESIAN_POINT('Ctrl Pts',(31.0459948352884,-2.49246284654849,31.5905494329321));
#71678=CARTESIAN_POINT('Ctrl Pts',(31.0591007914688,-2.5048455434335,31.6070390220085));
#71679=CARTESIAN_POINT('Ctrl Pts',(31.0723678233412,-2.51738042696111,31.6237706303625));
#71680=CARTESIAN_POINT('',(31.0228073395316,-2.5020674217591,31.5905494329235));
#71681=CARTESIAN_POINT('Origin',(31.036557887911,-2.50247209787259,31.5962049920587));
#71682=CARTESIAN_POINT('',(31.0217782109193,-2.53833533054864,31.6237706303691));
#71683=CARTESIAN_POINT('Ctrl Pts',(31.0217782109196,-2.53833533054137,31.6237706303625));
#71684=CARTESIAN_POINT('Ctrl Pts',(31.0222959179794,-2.52009062117993,31.6070390219952));
#71685=CARTESIAN_POINT('Ctrl Pts',(31.0228073395322,-2.50206742173989,31.5905494329059));
#71686=CARTESIAN_POINT('',(30.8715506793291,-2.59375719295041,31.6237706303691));
#71687=CARTESIAN_POINT('Origin',(30.,-1.32966554433622E-14,31.6237706303681));
#71688=CARTESIAN_POINT('',(30.8472140012126,-2.56684722431573,31.5905494329235));
#71689=CARTESIAN_POINT('Ctrl Pts',(30.8472140012189,-2.56684722432271,31.5905494329321));
#71690=CARTESIAN_POINT('Ctrl Pts',(30.8593080209101,-2.58022003095631,31.6070390220085));
#71691=CARTESIAN_POINT('Ctrl Pts',(30.8715506793242,-2.593757192945,31.6237706303625));
#71692=CARTESIAN_POINT('',(30.8233444184872,-2.57460292188405,31.5905494329235));
#71693=CARTESIAN_POINT('Origin',(30.8370208295222,-2.5760852110326,31.5962049981139));
#71694=CARTESIAN_POINT('',(30.8194729150074,-2.6106782843143,31.6237706303691));
#71695=CARTESIAN_POINT('Ctrl Pts',(30.8194729150082,-2.61067828430707,31.6237706303625));
#71696=CARTESIAN_POINT('Ctrl Pts',(30.8214204895483,-2.5925304361235,31.6070390219952));
#71697=CARTESIAN_POINT('Ctrl Pts',(30.8233444184892,-2.57460292186495,31.5905494329059));
#71698=CARTESIAN_POINT('',(30.6653601355536,-2.65414258332839,31.6237706303691));
#71699=CARTESIAN_POINT('Origin',(30.,-1.32966554433622E-14,31.6237706303681));
#71700=CARTESIAN_POINT('',(30.6432098110989,-2.62540613538822,31.5905494329235));
#71701=CARTESIAN_POINT('Ctrl Pts',(30.6432098111046,-2.62540613539568,31.5905494329321));
#71702=CARTESIAN_POINT('Ctrl Pts',(30.6542173306535,-2.63968660397806,31.6070390220085));
#71703=CARTESIAN_POINT('Ctrl Pts',(30.6653601355492,-2.65414258332262,31.6237706303625));
#71704=CARTESIAN_POINT('',(30.618805305313,-2.63126513885325,31.5905494329235));
#71705=CARTESIAN_POINT('Origin',(30.632323260043,-2.63381590833404,31.5962050111235));
#71706=CARTESIAN_POINT('',(30.6121152960721,-2.66692553831853,31.6237706303691));
#71707=CARTESIAN_POINT('Ctrl Pts',(30.6121152960734,-2.66692553831138,31.6237706303625));
#71708=CARTESIAN_POINT('Ctrl Pts',(30.615480730649,-2.6489864388245,31.6070390219952));
#71709=CARTESIAN_POINT('Ctrl Pts',(30.6188053053166,-2.63126513883437,31.5905494329059));
#71710=CARTESIAN_POINT('',(30.4550674252877,-2.69816430208819,31.6237706303691));
#71711=CARTESIAN_POINT('Origin',(30.,-1.32966554433622E-14,31.6237706303681));
#71712=CARTESIAN_POINT('',(30.4352400186108,-2.66777854459992,31.5905494329235));
#71713=CARTESIAN_POINT('Ctrl Pts',(30.435240018616,-2.6677785446078,31.5905494329321));
#71714=CARTESIAN_POINT('Ctrl Pts',(30.445093173004,-2.68287863130142,31.6070390220085));
#71715=CARTESIAN_POINT('Ctrl Pts',(30.4550674252837,-2.69816430208209,31.6237706303625));
#71716=CARTESIAN_POINT('',(30.410451051658,-2.67170473125697,31.5905494329235));
#71717=CARTESIAN_POINT('Origin',(30.4237272067093,-2.67530826149246,31.5962050315749));
#71718=CARTESIAN_POINT('',(30.4009837827875,-2.7067303095363,31.6237706303691));
#71719=CARTESIAN_POINT('Ctrl Pts',(30.4009837827894,-2.70673030952928,31.6237706303625));
#71720=CARTESIAN_POINT('Ctrl Pts',(30.4057463283773,-2.68911055925278,31.6070390219952));
#71721=CARTESIAN_POINT('Ctrl Pts',(30.410451051663,-2.67170473123841,31.5905494329059));
#71722=CARTESIAN_POINT('',(30.2419690730196,-2.72555094069494,31.6237706303691));
#71723=CARTESIAN_POINT('Origin',(30.,-1.32966554433622E-14,31.6237706303681));
#71724=CARTESIAN_POINT('',(30.224586826676,-2.69370321195777,31.5905494329235));
#71725=CARTESIAN_POINT('Ctrl Pts',(30.2245868266805,-2.69370321196604,31.5905494329321));
#71726=CARTESIAN_POINT('Ctrl Pts',(30.2332248679346,-2.70952981971513,31.6070390220085));
#71727=CARTESIAN_POINT('Ctrl Pts',(30.2419690730162,-2.72555094068854,31.6237706303625));
#71728=CARTESIAN_POINT('',(30.1995662307806,-2.69567237556051,31.5905494329235));
#71729=CARTESIAN_POINT('Origin',(30.2125187320612,-2.70030645711985,31.5962050602857));
#71730=CARTESIAN_POINT('',(30.1873800711414,-2.72984718831661,31.6237706303691));
#71731=CARTESIAN_POINT('Ctrl Pts',(30.1873800711438,-2.72984718830975,31.6237706303625));
#71732=CARTESIAN_POINT('Ctrl Pts',(30.1935103650667,-2.71265541886325,31.6070390219952));
#71733=CARTESIAN_POINT('Ctrl Pts',(30.199566230787,-2.6956723755424,31.5905494329059));
#71734=CARTESIAN_POINT('',(30.0273789009535,-2.73613365141464,31.6237706303691));
#71735=CARTESIAN_POINT('Origin',(30.,-1.32966554433622E-14,31.6237706303681));
#71736=CARTESIAN_POINT('',(30.012548982272,-2.70302030326669,31.5905494329235));
#71737=CARTESIAN_POINT('Ctrl Pts',(30.0125489822759,-2.70302030327528,31.5905494329321));
#71738=CARTESIAN_POINT('Ctrl Pts',(30.0199186539991,-2.7194758557802,31.6070390220085));
#71739=CARTESIAN_POINT('Ctrl Pts',(30.0273789009505,-2.736133651408,31.6237706303625));
#71740=CARTESIAN_POINT('',(29.987451017728,-2.70302030326669,31.5905494329235));
#71741=CARTESIAN_POINT('Origin',(30.,-2.7086657795165,31.5962151370754));
#71742=CARTESIAN_POINT('',(29.9726210990465,-2.73613365141464,31.6237706303691));
#71743=CARTESIAN_POINT('Ctrl Pts',(29.9726210990495,-2.73613365140799,31.6237706303625));
#71744=CARTESIAN_POINT('Ctrl Pts',(29.9800813460068,-2.71947585576697,31.6070390219952));
#71745=CARTESIAN_POINT('Ctrl Pts',(29.9874510177359,-2.70302030324915,31.5905494329059));
#71746=CARTESIAN_POINT('',(29.8126199288586,-2.72984718831661,31.6237706303691));
#71747=CARTESIAN_POINT('Origin',(30.,-1.32966554433622E-14,31.6237706303681));
#71748=CARTESIAN_POINT('',(29.8004337692193,-2.6956723755605,31.5905494329235));
#71749=CARTESIAN_POINT('Ctrl Pts',(29.8004337692225,-2.69567237556937,31.5905494329321));
#71750=CARTESIAN_POINT('Ctrl Pts',(29.806489634938,-2.71265541887691,31.6070390220085));
#71751=CARTESIAN_POINT('Ctrl Pts',(29.8126199288561,-2.72984718830976,31.6237706303625));
#71752=CARTESIAN_POINT('',(29.775413173324,-2.69370321195777,31.5905494329235));
#71753=CARTESIAN_POINT('Origin',(29.7874812116305,-2.70030745889015,31.5962062072437));
#71754=CARTESIAN_POINT('',(29.7580309269803,-2.72555094069494,31.6237706303691));
#71755=CARTESIAN_POINT('Ctrl Pts',(29.7580309269838,-2.72555094068855,31.6237706303625));
#71756=CARTESIAN_POINT('Ctrl Pts',(29.7667751320723,-2.7095298197024,31.6070390219952));
#71757=CARTESIAN_POINT('Ctrl Pts',(29.7754131733332,-2.69370321194088,31.5905494329059));
#71758=CARTESIAN_POINT('',(29.5990162172124,-2.70673030953629,31.6237706303691));
#71759=CARTESIAN_POINT('Origin',(30.,-1.32966554433622E-14,31.6237706303681));
#71760=CARTESIAN_POINT('',(29.589548948342,-2.67170473125696,31.5905494329235));
#71761=CARTESIAN_POINT('Ctrl Pts',(29.5895489483445,-2.67170473126605,31.5905494329321));
#71762=CARTESIAN_POINT('Ctrl Pts',(29.5942536716264,-2.68911055926676,31.6070390220085));
#71763=CARTESIAN_POINT('Ctrl Pts',(29.5990162172106,-2.70673030952926,31.6237706303625));
#71764=CARTESIAN_POINT('',(29.5647599813891,-2.66777854459992,31.5905494329235));
#71765=CARTESIAN_POINT('Origin',(29.5762726922515,-2.67530902338218,31.5962059100614));
#71766=CARTESIAN_POINT('',(29.5449325747122,-2.69816430208819,31.6237706303691));
#71767=CARTESIAN_POINT('Ctrl Pts',(29.5449325747162,-2.6981643020821,31.6237706303625));
#71768=CARTESIAN_POINT('Ctrl Pts',(29.5549068270038,-2.68287863128929,31.6070390219952));
#71769=CARTESIAN_POINT('Ctrl Pts',(29.5647599813996,-2.66777854458383,31.5905494329059));
#71770=CARTESIAN_POINT('',(29.3878847039278,-2.66692553831852,31.6237706303691));
#71771=CARTESIAN_POINT('Origin',(30.,-1.32966554433622E-14,31.6237706303681));
#71772=CARTESIAN_POINT('',(29.3811946946869,-2.63126513885324,31.5905494329235));
#71773=CARTESIAN_POINT('Ctrl Pts',(29.3811946946886,-2.63126513886249,31.5905494329321));
#71774=CARTESIAN_POINT('Ctrl Pts',(29.3845192693535,-2.64898643883873,31.6070390220085));
#71775=CARTESIAN_POINT('Ctrl Pts',(29.3878847039265,-2.66692553831137,31.6237706303625));
#71776=CARTESIAN_POINT('',(29.3567901889011,-2.62540613538822,31.5905494329235));
#71777=CARTESIAN_POINT('Origin',(29.3676766176013,-2.63381649164654,31.5962056922849));
#71778=CARTESIAN_POINT('',(29.3346398644463,-2.65414258332839,31.6237706303691));
#71779=CARTESIAN_POINT('Ctrl Pts',(29.3346398644508,-2.65414258332263,31.6237706303626));
#71780=CARTESIAN_POINT('Ctrl Pts',(29.3457826693553,-2.63968660396658,31.6070390219952));
#71781=CARTESIAN_POINT('Ctrl Pts',(29.3567901889128,-2.62540613537299,31.5905494329059));
#71782=CARTESIAN_POINT('',(29.1805270849925,-2.61067828431429,31.6237706303691));
#71783=CARTESIAN_POINT('Origin',(30.,-1.32966554433622E-14,31.6237706303681));
#71784=CARTESIAN_POINT('',(29.1766555815127,-2.57460292188404,31.5905494329235));
#71785=CARTESIAN_POINT('Ctrl Pts',(29.1766555815137,-2.5746029218934,31.5905494329321));
#71786=CARTESIAN_POINT('Ctrl Pts',(29.1785795104532,-2.59253043613788,31.6070390220085));
#71787=CARTESIAN_POINT('Ctrl Pts',(29.1805270849917,-2.61067828430705,31.6237706303625));
#71788=CARTESIAN_POINT('',(29.1527859987874,-2.56684722431572,31.5905494329235));
#71789=CARTESIAN_POINT('Origin',(29.162979042241,-2.57608565616368,31.5962055274321));
#71790=CARTESIAN_POINT('',(29.1284493206708,-2.59375719295039,31.6237706303691));
#71791=CARTESIAN_POINT('Ctrl Pts',(29.1284493206757,-2.593757192945,31.6237706303625));
#71792=CARTESIAN_POINT('Ctrl Pts',(29.1406919790996,-2.58022003094555,31.6070390219952));
#71793=CARTESIAN_POINT('Ctrl Pts',(29.1527859988003,-2.56684722430145,31.5905494329059));
#71794=CARTESIAN_POINT('',(28.9782217890806,-2.53833533054863,31.6237706303691));
#71795=CARTESIAN_POINT('Origin',(30.,-1.32966554433622E-14,31.6237706303681));
#71796=CARTESIAN_POINT('',(28.9771926604683,-2.50206742175908,31.5905494329235));
#71797=CARTESIAN_POINT('Ctrl Pts',(28.9771926604686,-2.50206742176849,31.5905494329321));
#71798=CARTESIAN_POINT('Ctrl Pts',(28.9777040820209,-2.5200906211944,31.6070390220085));
#71799=CARTESIAN_POINT('Ctrl Pts',(28.9782217890804,-2.53833533054136,31.6237706303625));
#71800=CARTESIAN_POINT('',(28.9540051647184,-2.49246284654199,31.5905494329235));
#71801=CARTESIAN_POINT('Origin',(28.963441988931,-2.50247243285095,31.5962053997573));
#71802=CARTESIAN_POINT('',(28.9276321766534,-2.51738042696608,31.6237706303691));
#71803=CARTESIAN_POINT('Ctrl Pts',(28.9276321766587,-2.51738042696105,31.6237706303625));
#71804=CARTESIAN_POINT('Ctrl Pts',(28.9408992085416,-2.5048455434235,31.6070390219952));
#71805=CARTESIAN_POINT('Ctrl Pts',(28.9540051647323,-2.49246284652876,31.5905494329059));
#71806=CARTESIAN_POINT('',(28.7822160956147,-2.45034269538798,31.6237706303691));
#71807=CARTESIAN_POINT('Origin',(30.,-1.32966554433622E-14,31.6237706303681));
#71808=CARTESIAN_POINT('',(28.7840356867901,-2.41410584395713,31.5905494329235));
#71809=CARTESIAN_POINT('Ctrl Pts',(28.7840356867896,-2.41410584396654,31.5905494329321));
#71810=CARTESIAN_POINT('Ctrl Pts',(28.783131447871,-2.43211360955609,31.6070390220085));
#71811=CARTESIAN_POINT('Ctrl Pts',(28.7822160956151,-2.45034269538072,31.6237706303625));
#71812=CARTESIAN_POINT('',(28.7616732366375,-2.40271160649133,31.5905494329235));
#71813=CARTESIAN_POINT('Origin',(28.7702956661397,-2.41343066267495,31.5962052993351));
#71814=CARTESIAN_POINT('',(28.7334265368654,-2.42548317353557,31.6237706303691));
#71815=CARTESIAN_POINT('Ctrl Pts',(28.7334265368711,-2.425483173531,31.6237706303625));
#71816=CARTESIAN_POINT('Ctrl Pts',(28.7476361465498,-2.41402785018062,31.6070390219952));
#71817=CARTESIAN_POINT('Ctrl Pts',(28.7616732366525,-2.40271160647928,31.5905494329059));
#71818=CARTESIAN_POINT('',(28.5937184448736,-2.34724288268865,31.6237706303691));
#71819=CARTESIAN_POINT('Origin',(30.,-1.32966554433622E-14,31.6237706303681));
#71820=CARTESIAN_POINT('',(28.5983755374519,-2.31126050085552,31.5905494329235));
#71821=CARTESIAN_POINT('Ctrl Pts',(28.5983755374507,-2.31126050086484,31.5905494329321));
#71822=CARTESIAN_POINT('Ctrl Pts',(28.5960612129946,-2.32914180875499,31.6070390220085));
#71823=CARTESIAN_POINT('Ctrl Pts',(28.5937184448745,-2.34724288268142,31.6237706303625));
#71824=CARTESIAN_POINT('',(28.5769760048382,-2.29814685040397,31.5905494329235));
#71825=CARTESIAN_POINT('Origin',(28.5847308825473,-2.30950931155478,31.5962052196244));
#71826=CARTESIAN_POINT('',(28.547029743656,-2.31863200978522,31.6237706303691));
#71827=CARTESIAN_POINT('Ctrl Pts',(28.547029743662,-2.31863200978111,31.6237706303625));
#71828=CARTESIAN_POINT('Ctrl Pts',(28.5620943241676,-2.30832687249563,31.6070390219952));
#71829=CARTESIAN_POINT('Ctrl Pts',(28.5769760048541,-2.29814685039312,31.5905494329059));
#71830=CARTESIAN_POINT('',(28.413890987556,-2.22967153708007,31.6237706303691));
#71831=CARTESIAN_POINT('Origin',(30.,-1.32966554433622E-14,31.6237706303681));
#71832=CARTESIAN_POINT('',(28.4213568690129,-2.19416546819403,31.5905494329235));
#71833=CARTESIAN_POINT('Ctrl Pts',(28.421356869011,-2.19416546820326,31.5905494329321));
#71834=CARTESIAN_POINT('Ctrl Pts',(28.4176467275973,-2.21181007418472,31.6070390220085));
#71835=CARTESIAN_POINT('Ctrl Pts',(28.4138909875575,-2.22967153707296,31.6237706303625));
#71836=CARTESIAN_POINT('',(28.4010521891725,-2.17941325477249,31.5905494329235));
#71837=CARTESIAN_POINT('Origin',(28.407891704857,-2.19134908471608,31.596205156165));
#71838=CARTESIAN_POINT('',(28.3695909952386,-2.19748570867116,31.6237706303691));
#71839=CARTESIAN_POINT('Ctrl Pts',(28.3695909952449,-2.19748570866753,31.6237706303625));
#71840=CARTESIAN_POINT('Ctrl Pts',(28.3854176684292,-2.18839429204513,31.6070390219952));
#71841=CARTESIAN_POINT('Ctrl Pts',(28.4010521891892,-2.17941325476292,31.5905494329059));
#71842=CARTESIAN_POINT('',(28.2438424197348,-2.09835352500436,31.6237706303691));
#71843=CARTESIAN_POINT('Origin',(30.,-1.32966554433622E-14,31.6237706303681));
#71844=CARTESIAN_POINT('',(28.2540710604284,-2.06354267578707,31.5905494329235));
#71845=CARTESIAN_POINT('Ctrl Pts',(28.2540710604258,-2.0635426757961,31.5905494329321));
#71846=CARTESIAN_POINT('Ctrl Pts',(28.2489879763101,-2.08084179500557,31.6070390220085));
#71847=CARTESIAN_POINT('Ctrl Pts',(28.2438424197369,-2.09835352499738,31.6237706303625));
#71848=CARTESIAN_POINT('',(28.2349864184647,-2.04724285169689,31.5905494329235));
#71849=CARTESIAN_POINT('Origin',(28.2408684039783,-2.05967847590829,31.5962051058414));
#71850=CARTESIAN_POINT('',(28.2022042605016,-2.06279117742499,31.6237706303691));
#71851=CARTESIAN_POINT('Ctrl Pts',(28.2022042605082,-2.06279117742185,31.6237706303625));
#71852=CARTESIAN_POINT('Ctrl Pts',(28.2186954496679,-2.0549695330692,31.6070390219952));
#71853=CARTESIAN_POINT('Ctrl Pts',(28.2349864184821,-2.04724285168864,31.5905494329059));
#71854=CARTESIAN_POINT('',(28.0846211473776,-1.95409846567366,31.6237706303691));
#71855=CARTESIAN_POINT('Origin',(30.,-1.32966554433622E-14,31.6237706303681));
#71856=CARTESIAN_POINT('',(28.0975494843367,-1.92019745658631,31.5905494329235));
#71857=CARTESIAN_POINT('Ctrl Pts',(28.0975494843333,-1.92019745659509,31.5905494329321));
#71858=CARTESIAN_POINT('Ctrl Pts',(28.0911247964195,-1.93704443421011,31.6070390220085));
#71859=CARTESIAN_POINT('Ctrl Pts',(28.0846211473802,-1.95409846566685,31.6237706303626));
#71860=CARTESIAN_POINT('',(28.0798025434136,-1.90245051566325,31.5905494329235));
#71861=CARTESIAN_POINT('Origin',(28.0846907329876,-1.91530927561707,31.5962050664381));
#71862=CARTESIAN_POINT('',(28.0459015343263,-1.91537885262232,31.6237706303691));
#71863=CARTESIAN_POINT('Ctrl Pts',(28.0459015343331,-1.91537885261973,31.6237706303625));
#71864=CARTESIAN_POINT('Ctrl Pts',(28.0629555658034,-1.90887520357524,31.6070390219952));
#71865=CARTESIAN_POINT('Ctrl Pts',(28.0798025434316,-1.90245051565641,31.5905494329059));
#71866=CARTESIAN_POINT('',(27.937208822575,-1.79779573949839,31.6237706303691));
#71867=CARTESIAN_POINT('Origin',(30.,-1.32966554433622E-14,31.6237706303681));
#71868=CARTESIAN_POINT('',(27.9527571483031,-1.76501358153525,31.5905494329235));
#71869=CARTESIAN_POINT('Ctrl Pts',(27.9527571482991,-1.76501358154376,31.5905494329321));
#71870=CARTESIAN_POINT('Ctrl Pts',(27.9450304669246,-1.78130455034514,31.6070390220085));
#71871=CARTESIAN_POINT('Ctrl Pts',(27.9372088225781,-1.79779573949183,31.6237706303625));
#71872=CARTESIAN_POINT('',(27.9364573242129,-1.74592893957155,31.5905494329235));
#71873=CARTESIAN_POINT('Origin',(27.940321578254,-1.75913156587022,31.5962050363747));
#71874=CARTESIAN_POINT('',(27.9016464749956,-1.75615758026514,31.6237706303691));
#71875=CARTESIAN_POINT('Ctrl Pts',(27.9016464750026,-1.75615758026309,31.6237706303625));
#71876=CARTESIAN_POINT('Ctrl Pts',(27.9191582050083,-1.75101202368579,31.6070390219952));
#71877=CARTESIAN_POINT('Ctrl Pts',(27.9364573242313,-1.74592893956614,31.5905494329059));
#71878=CARTESIAN_POINT('',(27.8025142913288,-1.63040900476137,31.6237706303691));
#71879=CARTESIAN_POINT('Origin',(30.,-1.32966554433622E-14,31.6237706303681));
#71880=CARTESIAN_POINT('',(27.8205867452275,-1.59894781082744,31.5905494329235));
#71881=CARTESIAN_POINT('Ctrl Pts',(27.8205867452228,-1.59894781083561,31.5905494329321));
#71882=CARTESIAN_POINT('Ctrl Pts',(27.8116057079476,-1.61458233158338,31.6070390220085));
#71883=CARTESIAN_POINT('Ctrl Pts',(27.8025142913325,-1.63040900475507,31.6237706303625));
#71884=CARTESIAN_POINT('',(27.8058345318059,-1.5786431309871,31.5905494329235));
#71885=CARTESIAN_POINT('Origin',(27.8086510228583,-1.5921082324254,31.5962050145327));
#71886=CARTESIAN_POINT('',(27.7703284629199,-1.58610901244396,31.6237706303691));
#71887=CARTESIAN_POINT('Ctrl Pts',(27.770328462927,-1.58610901244246,31.6237706303625));
#71888=CARTESIAN_POINT('Ctrl Pts',(27.7881899258294,-1.58235327239973,31.6070390219952));
#71889=CARTESIAN_POINT('Ctrl Pts',(27.8058345318247,-1.57864313098315,31.5905494329059));
#71890=CARTESIAN_POINT('',(27.6813679902147,-1.45297025634398,31.6237706303691));
#71891=CARTESIAN_POINT('Origin',(30.,-1.32966554433622E-14,31.6237706303681));
#71892=CARTESIAN_POINT('',(27.701853149596,-1.42302399516179,31.5905494329235));
#71893=CARTESIAN_POINT('Ctrl Pts',(27.7018531495907,-1.42302399516956,31.5905494329321));
#71894=CARTESIAN_POINT('Ctrl Pts',(27.6916731274962,-1.43790567584432,31.6070390220085));
#71895=CARTESIAN_POINT('Ctrl Pts',(27.6813679902189,-1.45297025633799,31.6237706303626));
#71896=CARTESIAN_POINT('',(27.6887394991444,-1.40162446254801,31.5905494329235));
#71897=CARTESIAN_POINT('Origin',(27.6904908588872,-1.41526902814876,31.596205000146));
#71898=CARTESIAN_POINT('',(27.6527571173113,-1.4062815551263,31.6237706303691));
#71899=CARTESIAN_POINT('Ctrl Pts',(27.6527571173185,-1.40628155512537,31.6237706303626));
#71900=CARTESIAN_POINT('Ctrl Pts',(27.6708581912593,-1.40393878700346,31.6070390219953));
#71901=CARTESIAN_POINT('Ctrl Pts',(27.6887394991635,-1.40162446254554,31.5905494329059));
#71902=CARTESIAN_POINT('',(27.5745168264644,-1.2665734631346,31.6237706303691));
#71903=CARTESIAN_POINT('Origin',(30.,-1.32966554433622E-14,31.6237706303681));
#71904=CARTESIAN_POINT('',(27.5972883935086,-1.23832676336246,31.5905494329235));
#71905=CARTESIAN_POINT('Ctrl Pts',(27.5972883935027,-1.23832676336977,31.5905494329321));
#71906=CARTESIAN_POINT('Ctrl Pts',(27.5859721498102,-1.25236385346148,31.6070390220085));
#71907=CARTESIAN_POINT('Ctrl Pts',(27.574516826469,-1.2665734631289,31.6237706303626));
#71908=CARTESIAN_POINT('',(27.5858941560428,-1.21596431320988,31.5905494329235));
#71909=CARTESIAN_POINT('Origin',(27.5865695824296,-1.22970422416533,31.5962049927334));
#71910=CARTESIAN_POINT('',(27.549657304612,-1.21778390438522,31.6237706303691));
#71911=CARTESIAN_POINT('Ctrl Pts',(27.5496573046193,-1.21778390438485,31.6237706303625));
#71912=CARTESIAN_POINT('Ctrl Pts',(27.5678863904584,-1.2168685521283,31.6070390219952));
#71913=CARTESIAN_POINT('Ctrl Pts',(27.585894156062,-1.21596431320891,31.5905494329059));
#71914=CARTESIAN_POINT('',(27.4826195730339,-1.07236782334657,31.6237706303691));
#71915=CARTESIAN_POINT('Origin',(30.,-1.32966554433622E-14,31.6237706303681));
#71916=CARTESIAN_POINT('',(27.507537153458,-1.04599483528157,31.5905494329235));
#71917=CARTESIAN_POINT('Ctrl Pts',(27.5075371534515,-1.04599483528841,31.5905494329321));
#71918=CARTESIAN_POINT('Ctrl Pts',(27.4951544565665,-1.05910079146888,31.6070390220085));
#71919=CARTESIAN_POINT('Ctrl Pts',(27.4826195730389,-1.07236782334129,31.6237706303626));
#71920=CARTESIAN_POINT('',(27.4979325782409,-1.02280733953164,31.5905494329235));
#71921=CARTESIAN_POINT('Origin',(27.4975279021274,-1.03655788791105,31.5962049920587));
#71922=CARTESIAN_POINT('',(27.4616646694513,-1.02177821091936,31.6237706303691));
#71923=CARTESIAN_POINT('Ctrl Pts',(27.4616646694586,-1.02177821091956,31.6237706303626));
#71924=CARTESIAN_POINT('Ctrl Pts',(27.4799093788201,-1.02229591797942,31.6070390219952));
#71925=CARTESIAN_POINT('Ctrl Pts',(27.4979325782601,-1.02280733953218,31.5905494329059));
#71926=CARTESIAN_POINT('',(27.4062428070496,-0.871550679329129,31.6237706303691));
#71927=CARTESIAN_POINT('Origin',(30.,-1.32966554433622E-14,31.6237706303681));
#71928=CARTESIAN_POINT('',(27.4331527756843,-0.847214001212589,31.5905494329235));
#71929=CARTESIAN_POINT('Ctrl Pts',(27.4331527756773,-0.847214001218912,
31.5905494329321));
#71930=CARTESIAN_POINT('Ctrl Pts',(27.4197799690437,-0.859308020910092,
31.6070390220085));
#71931=CARTESIAN_POINT('Ctrl Pts',(27.406242807055,-0.871550679324261,31.6237706303625));
#71932=CARTESIAN_POINT('',(27.4253970781159,-0.823344418487241,31.5905494329235));
#71933=CARTESIAN_POINT('Origin',(27.4239147889674,-0.837020829522197,31.5962049981138));
#71934=CARTESIAN_POINT('',(27.3893217156857,-0.819472915007445,31.6237706303691));
#71935=CARTESIAN_POINT('Ctrl Pts',(27.3893217156929,-0.819472915008222,
31.6237706303625));
#71936=CARTESIAN_POINT('Ctrl Pts',(27.4074695638765,-0.821420489548307,
31.6070390219952));
#71937=CARTESIAN_POINT('Ctrl Pts',(27.425397078135,-0.823344418489291,31.590549432906));
#71938=CARTESIAN_POINT('',(27.3458574166716,-0.665360135553609,31.6237706303691));
#71939=CARTESIAN_POINT('Origin',(30.,-1.32966554433622E-14,31.6237706303681));
#71940=CARTESIAN_POINT('',(27.3745938646118,-0.643209811098888,31.5905494329235));
#71941=CARTESIAN_POINT('Ctrl Pts',(27.3745938646043,-0.643209811104637,
31.5905494329321));
#71942=CARTESIAN_POINT('Ctrl Pts',(27.3603133960219,-0.65421733065347,31.6070390220085));
#71943=CARTESIAN_POINT('Ctrl Pts',(27.3458574166774,-0.665360135549176,
31.6237706303625));
#71944=CARTESIAN_POINT('',(27.3687348611467,-0.618805305313063,31.5905494329235));
#71945=CARTESIAN_POINT('Origin',(27.3661840916659,-0.632323260043008,31.5962050111235));
#71946=CARTESIAN_POINT('',(27.3330744616815,-0.612115296072114,31.6237706303691));
#71947=CARTESIAN_POINT('Ctrl Pts',(27.3330744616886,-0.612115296073467,
31.6237706303625));
#71948=CARTESIAN_POINT('Ctrl Pts',(27.3510135611755,-0.615480730649101,
31.6070390219952));
#71949=CARTESIAN_POINT('Ctrl Pts',(27.3687348611656,-0.61880530531661,31.590549432906));
#71950=CARTESIAN_POINT('',(27.3018356979118,-0.455067425287704,31.6237706303691));
#71951=CARTESIAN_POINT('Origin',(30.,-1.32966554433622E-14,31.6237706303681));
#71952=CARTESIAN_POINT('',(27.3322214554001,-0.435240018610796,31.5905494329235));
#71953=CARTESIAN_POINT('Ctrl Pts',(27.3322214553922,-0.435240018615941,
31.5905494329321));
#71954=CARTESIAN_POINT('Ctrl Pts',(27.3171213686986,-0.445093173004034,
31.6070390220085));
#71955=CARTESIAN_POINT('Ctrl Pts',(27.3018356979179,-0.455067425283735,
31.6237706303625));
#71956=CARTESIAN_POINT('',(27.328295268743,-0.410451051657984,31.5905494329235));
#71957=CARTESIAN_POINT('Origin',(27.3246917385075,-0.423727206709274,31.5962050315749));
#71958=CARTESIAN_POINT('',(27.2932696904637,-0.400983782787508,31.6237706303691));
#71959=CARTESIAN_POINT('Ctrl Pts',(27.2932696904707,-0.400983782789399,
31.6237706303625));
#71960=CARTESIAN_POINT('Ctrl Pts',(27.3108894407472,-0.405746328377308,
31.6070390219952));
#71961=CARTESIAN_POINT('Ctrl Pts',(27.3282952687616,-0.410451051662988,
31.5905494329059));
#71962=CARTESIAN_POINT('',(27.274449059305,-0.241969073019628,31.6237706303691));
#71963=CARTESIAN_POINT('Origin',(30.,-1.32966554433622E-14,31.6237706303681));
#71964=CARTESIAN_POINT('',(27.3062967880422,-0.224586826675978,31.5905494329235));
#71965=CARTESIAN_POINT('Ctrl Pts',(27.306296788034,-0.224586826680481,31.5905494329321));
#71966=CARTESIAN_POINT('Ctrl Pts',(27.2904701802848,-0.233224867934527,
31.6070390220085));
#71967=CARTESIAN_POINT('Ctrl Pts',(27.2744490593114,-0.241969073016143,
31.6237706303626));
#71968=CARTESIAN_POINT('',(27.3043276244395,-0.199566230780611,31.5905494329235));
#71969=CARTESIAN_POINT('Origin',(27.2996935428802,-0.212518732061225,31.5962050602856));
#71970=CARTESIAN_POINT('',(27.2701528116834,-0.18738007114138,31.6237706303691));
#71971=CARTESIAN_POINT('Ctrl Pts',(27.2701528116903,-0.187380071143839,
31.6237706303625));
#71972=CARTESIAN_POINT('Ctrl Pts',(27.2873445811368,-0.193510365066767,
31.6070390219952));
#71973=CARTESIAN_POINT('Ctrl Pts',(27.3043276244576,-0.199566230787083,
31.5905494329059));
#71974=CARTESIAN_POINT('',(27.2638663485853,-0.027378900953502,31.6237706303691));
#71975=CARTESIAN_POINT('Origin',(30.,-1.32966554433622E-14,31.6237706303681));
#71976=CARTESIAN_POINT('Ctrl Pts',(27.2969796967247,-0.0125489822758455,
31.5905494329321));
#71977=CARTESIAN_POINT('Ctrl Pts',(27.2805241442198,-0.0199186539990725,
31.6070390220085));
#71978=CARTESIAN_POINT('Ctrl Pts',(27.263866348592,-0.0273789009505331,
31.6237706303626));
#71979=CARTESIAN_POINT('',(27.2638663485853,0.0273789009535324,31.6237706303691));
#71980=CARTESIAN_POINT('Ctrl Pts',(27.263866348592,0.0273789009505529,31.6237706303626));
#71981=CARTESIAN_POINT('Ctrl Pts',(27.280524144233,0.0199186539931685,31.6070390219952));
#71982=CARTESIAN_POINT('Ctrl Pts',(27.2969796967508,0.012548982264161,31.5905494329059));
#71983=CARTESIAN_POINT('',(27.2701528116834,0.187380071141411,31.6237706303691));
#71984=CARTESIAN_POINT('Origin',(30.,-1.32966554433622E-14,31.6237706303681));
#71985=CARTESIAN_POINT('Ctrl Pts',(27.3043276244306,0.199566230777481,31.5905494329321));
#71986=CARTESIAN_POINT('Ctrl Pts',(27.2873445811231,0.193510365061917,31.6070390220085));
#71987=CARTESIAN_POINT('Ctrl Pts',(27.2701528116902,0.187380071143857,31.6237706303625));
#71988=CARTESIAN_POINT('',(27.2744490593051,0.241969073019658,31.6237706303691));
#71989=CARTESIAN_POINT('Ctrl Pts',(27.2744490593115,0.241969073016152,31.6237706303625));
#71990=CARTESIAN_POINT('Ctrl Pts',(27.2904701802976,0.233224867927605,31.6070390219952));
#71991=CARTESIAN_POINT('Ctrl Pts',(27.3062967880591,0.224586826666795,31.5905494329059));
#71992=CARTESIAN_POINT('',(27.2932696904637,0.40098378278754,31.6237706303691));
#71993=CARTESIAN_POINT('Origin',(30.,-1.32966554433622E-14,31.6237706303681));
#71994=CARTESIAN_POINT('Ctrl Pts',(27.3282952687339,0.410451051655568,31.5905494329321));
#71995=CARTESIAN_POINT('Ctrl Pts',(27.3108894407332,0.405746328373579,31.6070390220085));
#71996=CARTESIAN_POINT('Ctrl Pts',(27.2932696904707,0.400983782789452,31.6237706303626));
#71997=CARTESIAN_POINT('',(27.3018356979118,0.455067425287736,31.6237706303691));
#71998=CARTESIAN_POINT('Ctrl Pts',(27.3018356979179,0.455067425283746,31.6237706303626));
#71999=CARTESIAN_POINT('Ctrl Pts',(27.3171213687107,0.445093172996126,31.6070390219952));
#72000=CARTESIAN_POINT('Ctrl Pts',(27.3322214554162,0.435240018600305,31.5905494329059));
#72001=CARTESIAN_POINT('',(27.3330744616815,0.612115296072143,31.6237706303691));
#72002=CARTESIAN_POINT('Origin',(30.,-1.32966554433622E-14,31.6237706303681));
#72003=CARTESIAN_POINT('Ctrl Pts',(27.3687348611375,0.618805305311351,31.5905494329321));
#72004=CARTESIAN_POINT('Ctrl Pts',(27.3510135611613,0.615480730646445,31.6070390220085));
#72005=CARTESIAN_POINT('Ctrl Pts',(27.3330744616886,0.612115296073478,31.6237706303625));
#72006=CARTESIAN_POINT('',(27.3458574166716,0.665360135553637,31.6237706303691));
#72007=CARTESIAN_POINT('Ctrl Pts',(27.3458574166774,0.665360135549173,31.6237706303626));
#72008=CARTESIAN_POINT('Ctrl Pts',(27.3603133960334,0.65421733064462,31.6070390219952));
#72009=CARTESIAN_POINT('Ctrl Pts',(27.374593864627,0.643209811087154,31.5905494329059));
#72010=CARTESIAN_POINT('',(27.3893217156857,0.819472915007473,31.6237706303691));
#72011=CARTESIAN_POINT('Origin',(30.,-1.32966554433622E-14,31.6237706303681));
#72012=CARTESIAN_POINT('Ctrl Pts',(27.4253970781066,0.823344418486268,31.5905494329322));
#72013=CARTESIAN_POINT('Ctrl Pts',(27.4074695638621,0.821420489546793,31.6070390220085));
#72014=CARTESIAN_POINT('Ctrl Pts',(27.3893217156929,0.819472915008255,31.6237706303625));
#72015=CARTESIAN_POINT('',(27.4062428070496,0.871550679329156,31.6237706303691));
#72016=CARTESIAN_POINT('Ctrl Pts',(27.406242807055,0.87155067932429,31.6237706303625));
#72017=CARTESIAN_POINT('Ctrl Pts',(27.4197799690545,0.8593080209004,31.6070390219952));
#72018=CARTESIAN_POINT('Ctrl Pts',(27.4331527756986,0.847214001199735,31.5905494329059));
#72019=CARTESIAN_POINT('',(27.4616646694514,1.02177821091938,31.6237706303691));
#72020=CARTESIAN_POINT('Origin',(30.,-1.32966554433622E-14,31.6237706303681));
#72021=CARTESIAN_POINT('Ctrl Pts',(27.4979325782315,1.0228073395314,31.5905494329321));
#72022=CARTESIAN_POINT('Ctrl Pts',(27.4799093788056,1.02229591797904,31.6070390220085));
#72023=CARTESIAN_POINT('Ctrl Pts',(27.4616646694587,1.02177821091959,31.6237706303625));
#72024=CARTESIAN_POINT('',(27.4826195730339,1.0723678233466,31.6237706303691));
#72025=CARTESIAN_POINT('Ctrl Pts',(27.4826195730389,1.0723678233413,31.6237706303626));
#72026=CARTESIAN_POINT('Ctrl Pts',(27.4951544565765,1.05910079145835,31.6070390219952));
#72027=CARTESIAN_POINT('Ctrl Pts',(27.5075371534712,1.04599483526761,31.5905494329059));
#72028=CARTESIAN_POINT('',(27.549657304612,1.21778390438524,31.6237706303691));
#72029=CARTESIAN_POINT('Origin',(30.,-1.32966554433622E-14,31.6237706303681));
#72030=CARTESIAN_POINT('Ctrl Pts',(27.5858941560335,1.21596431321037,31.5905494329321));
#72031=CARTESIAN_POINT('Ctrl Pts',(27.5678863904439,1.21686855212906,31.6070390220085));
#72032=CARTESIAN_POINT('Ctrl Pts',(27.5496573046193,1.21778390438488,31.6237706303626));
#72033=CARTESIAN_POINT('',(27.5745168264644,1.26657346313462,31.6237706303691));
#72034=CARTESIAN_POINT('Ctrl Pts',(27.574516826469,1.26657346312892,31.6237706303626));
#72035=CARTESIAN_POINT('Ctrl Pts',(27.5859721498194,1.25236385345021,31.6070390219952));
#72036=CARTESIAN_POINT('Ctrl Pts',(27.5972883935207,1.23832676334747,31.5905494329059));
#72037=CARTESIAN_POINT('',(27.6527571173114,1.40628155512632,31.6237706303691));
#72038=CARTESIAN_POINT('Origin',(30.,-1.32966554433622E-14,31.6237706303681));
#72039=CARTESIAN_POINT('Ctrl Pts',(27.6887394991352,1.40162446254924,31.5905494329321));
#72040=CARTESIAN_POINT('Ctrl Pts',(27.670858191245,1.40393878700535,31.6070390220085));
#72041=CARTESIAN_POINT('Ctrl Pts',(27.6527571173186,1.40628155512539,31.6237706303625));
#72042=CARTESIAN_POINT('',(27.6813679902148,1.45297025634401,31.6237706303691));
#72043=CARTESIAN_POINT('Ctrl Pts',(27.6813679902189,1.452970256338,31.6237706303625));
#72044=CARTESIAN_POINT('Ctrl Pts',(27.6916731275044,1.43790567583238,31.6070390219952));
#72045=CARTESIAN_POINT('Ctrl Pts',(27.7018531496069,1.42302399514596,31.5905494329059));
#72046=CARTESIAN_POINT('',(27.7703284629199,1.58610901244398,31.6237706303691));
#72047=CARTESIAN_POINT('Origin',(30.,-1.32966554433622E-14,31.6237706303681));
#72048=CARTESIAN_POINT('Ctrl Pts',(27.8058345317968,1.57864313098906,31.5905494329321));
#72049=CARTESIAN_POINT('Ctrl Pts',(27.7881899258153,1.58235327240273,31.6070390220085));
#72050=CARTESIAN_POINT('Ctrl Pts',(27.770328462927,1.58610901244249,31.6237706303626));
#72051=CARTESIAN_POINT('',(27.8025142913288,1.63040900476139,31.6237706303691));
#72052=CARTESIAN_POINT('Ctrl Pts',(27.8025142913324,1.63040900475507,31.6237706303626));
#72053=CARTESIAN_POINT('Ctrl Pts',(27.8116057079549,1.61458233157081,31.6070390219952));
#72054=CARTESIAN_POINT('Ctrl Pts',(27.8205867452371,1.59894781081078,31.5905494329059));
#72055=CARTESIAN_POINT('',(27.9016464749956,1.75615758026516,31.6237706303691));
#72056=CARTESIAN_POINT('Origin',(30.,-1.32966554433622E-14,31.6237706303681));
#72057=CARTESIAN_POINT('Ctrl Pts',(27.9364573242039,1.74592893957422,31.5905494329321));
#72058=CARTESIAN_POINT('Ctrl Pts',(27.9191582049944,1.75101202368989,31.6070390220085));
#72059=CARTESIAN_POINT('Ctrl Pts',(27.9016464750026,1.7561575802631,31.6237706303626));
#72060=CARTESIAN_POINT('',(27.937208822575,1.79779573949841,31.6237706303691));
#72061=CARTESIAN_POINT('Ctrl Pts',(27.9372088225781,1.79779573949182,31.6237706303625));
#72062=CARTESIAN_POINT('Ctrl Pts',(27.9450304669308,1.78130455033204,31.6070390219952));
#72063=CARTESIAN_POINT('Ctrl Pts',(27.9527571483113,1.76501358151789,31.5905494329059));
#72064=CARTESIAN_POINT('',(28.0459015343263,1.91537885262234,31.6237706303691));
#72065=CARTESIAN_POINT('Origin',(30.,-1.32966554433622E-14,31.6237706303681));
#72066=CARTESIAN_POINT('Ctrl Pts',(28.0798025434049,1.90245051566662,31.5905494329321));
#72067=CARTESIAN_POINT('Ctrl Pts',(28.0629555657899,1.90887520358041,31.6070390220085));
#72068=CARTESIAN_POINT('Ctrl Pts',(28.0459015343331,1.91537885261975,31.6237706303626));
#72069=CARTESIAN_POINT('',(28.0846211473777,1.95409846567367,31.6237706303691));
#72070=CARTESIAN_POINT('Ctrl Pts',(28.0846211473803,1.95409846566688,31.6237706303625));
#72071=CARTESIAN_POINT('Ctrl Pts',(28.0911247964248,1.93704443419661,31.6070390219952));
#72072=CARTESIAN_POINT('Ctrl Pts',(28.0975494843436,1.9201974565684,31.5905494329059));
#72073=CARTESIAN_POINT('',(28.2022042605016,2.062791177425,31.6237706303691));
#72074=CARTESIAN_POINT('Origin',(30.,-1.32966554433622E-14,31.6237706303681));
#72075=CARTESIAN_POINT('Ctrl Pts',(28.2349864184563,2.04724285170094,31.5905494329321));
#72076=CARTESIAN_POINT('Ctrl Pts',(28.2186954496549,2.05496953307545,31.6070390220085));
#72077=CARTESIAN_POINT('Ctrl Pts',(28.2022042605082,2.0627911774219,31.6237706303626));
#72078=CARTESIAN_POINT('',(28.2438424197349,2.09835352500437,31.6237706303691));
#72079=CARTESIAN_POINT('Ctrl Pts',(28.2438424197369,2.09835352499738,31.6237706303625));
#72080=CARTESIAN_POINT('Ctrl Pts',(28.2489879763142,2.08084179499167,31.6070390219952));
#72081=CARTESIAN_POINT('Ctrl Pts',(28.2540710604339,2.06354267576863,31.5905494329059));
#72082=CARTESIAN_POINT('',(28.3695909952386,2.19748570867117,31.6237706303691));
#72083=CARTESIAN_POINT('Origin',(30.,-1.32966554433622E-14,31.6237706303681));
#72084=CARTESIAN_POINT('Ctrl Pts',(28.4010521891644,2.17941325477719,31.5905494329321));
#72085=CARTESIAN_POINT('Ctrl Pts',(28.3854176684167,2.18839429205237,31.6070390220085));
#72086=CARTESIAN_POINT('Ctrl Pts',(28.369590995245,2.19748570866756,31.6237706303626));
#72087=CARTESIAN_POINT('',(28.413890987556,2.22967153708007,31.6237706303691));
#72088=CARTESIAN_POINT('Ctrl Pts',(28.4138909875575,2.22967153707294,31.6237706303625));
#72089=CARTESIAN_POINT('Ctrl Pts',(28.4176467276003,2.21181007417053,31.6070390219952));
#72090=CARTESIAN_POINT('Ctrl Pts',(28.4213568690169,2.19416546817523,31.5905494329059));
#72091=CARTESIAN_POINT('',(28.547029743656,2.31863200978522,31.6237706303691));
#72092=CARTESIAN_POINT('Origin',(30.,-1.32966554433622E-14,31.6237706303681));
#72093=CARTESIAN_POINT('Ctrl Pts',(28.5769760048304,2.29814685040929,31.5905494329321));
#72094=CARTESIAN_POINT('Ctrl Pts',(28.5620943241557,2.30832687250382,31.6070390220085));
#72095=CARTESIAN_POINT('Ctrl Pts',(28.547029743662,2.31863200978111,31.6237706303625));
#72096=CARTESIAN_POINT('',(28.5937184448737,2.34724288268865,31.6237706303691));
#72097=CARTESIAN_POINT('Ctrl Pts',(28.5937184448746,2.34724288268143,31.6237706303626));
#72098=CARTESIAN_POINT('Ctrl Pts',(28.5960612129965,2.32914180874063,31.6070390219952));
#72099=CARTESIAN_POINT('Ctrl Pts',(28.5983755374545,2.31126050083645,31.5905494329059));
#72100=CARTESIAN_POINT('',(28.7334265368654,2.42548317353557,31.6237706303691));
#72101=CARTESIAN_POINT('Origin',(30.,-1.32966554433622E-14,31.6237706303681));
#72102=CARTESIAN_POINT('Ctrl Pts',(28.7616732366302,2.40271160649724,31.5905494329321));
#72103=CARTESIAN_POINT('Ctrl Pts',(28.7476361465385,2.4140278501897,31.6070390220085));
#72104=CARTESIAN_POINT('Ctrl Pts',(28.7334265368711,2.42548317353099,31.6237706303625));
#72105=CARTESIAN_POINT('',(28.7822160956148,2.45034269538798,31.6237706303691));
#72106=CARTESIAN_POINT('Ctrl Pts',(28.7822160956151,2.45034269538071,31.6237706303626));
#72107=CARTESIAN_POINT('Ctrl Pts',(28.7831314478717,2.4321136095416,31.6070390219952));
#72108=CARTESIAN_POINT('Ctrl Pts',(28.7840356867911,2.41410584393792,31.5905494329059));
#72109=CARTESIAN_POINT('',(28.9276321766534,2.51738042696607,31.6237706303691));
#72110=CARTESIAN_POINT('Origin',(30.,-1.32966554433622E-14,31.6237706303681));
#72111=CARTESIAN_POINT('',(28.9540051647184,2.49246284654199,31.5905494329235));
#72112=CARTESIAN_POINT('Ctrl Pts',(28.9540051647116,2.49246284654845,31.5905494329321));
#72113=CARTESIAN_POINT('Ctrl Pts',(28.9408992085311,2.50484554343346,31.6070390220085));
#72114=CARTESIAN_POINT('Ctrl Pts',(28.9276321766587,2.51738042696107,31.6237706303625));
#72115=CARTESIAN_POINT('',(28.9771926604684,2.50206742175908,31.5905494329235));
#72116=CARTESIAN_POINT('Origin',(28.9634421120889,2.50247209787257,31.5962049920587));
#72117=CARTESIAN_POINT('',(28.9782217890806,2.53833533054862,31.6237706303691));
#72118=CARTESIAN_POINT('Ctrl Pts',(28.9782217890804,2.53833533054134,31.6237706303625));
#72119=CARTESIAN_POINT('Ctrl Pts',(28.9777040820206,2.52009062117991,31.6070390219952));
#72120=CARTESIAN_POINT('Ctrl Pts',(28.9771926604678,2.50206742173986,31.5905494329059));
#72121=CARTESIAN_POINT('',(29.1284493206709,2.59375719295039,31.6237706303691));
#72122=CARTESIAN_POINT('Origin',(30.,-1.32966554433622E-14,31.6237706303681));
#72123=CARTESIAN_POINT('',(29.1527859987874,2.56684722431571,31.5905494329235));
#72124=CARTESIAN_POINT('Ctrl Pts',(29.1527859987811,2.56684722432269,31.5905494329321));
#72125=CARTESIAN_POINT('Ctrl Pts',(29.1406919790899,2.58022003095629,31.6070390220085));
#72126=CARTESIAN_POINT('Ctrl Pts',(29.1284493206758,2.59375719294498,31.6237706303625));
#72127=CARTESIAN_POINT('',(29.1766555815128,2.57460292188403,31.5905494329235));
#72128=CARTESIAN_POINT('Origin',(29.1629791704778,2.57608521103256,31.5962049981139));
#72129=CARTESIAN_POINT('',(29.1805270849926,2.61067828431428,31.6237706303691));
#72130=CARTESIAN_POINT('Ctrl Pts',(29.1805270849917,2.61067828430704,31.6237706303626));
#72131=CARTESIAN_POINT('Ctrl Pts',(29.1785795104516,2.59253043612347,31.6070390219952));
#72132=CARTESIAN_POINT('Ctrl Pts',(29.1766555815107,2.57460292186492,31.5905494329059));
#72133=CARTESIAN_POINT('',(29.3346398644464,2.65414258332837,31.6237706303691));
#72134=CARTESIAN_POINT('Origin',(30.,-1.32966554433622E-14,31.6237706303681));
#72135=CARTESIAN_POINT('',(29.3567901889011,2.6254061353882,31.5905494329235));
#72136=CARTESIAN_POINT('Ctrl Pts',(29.3567901888954,2.62540613539565,31.5905494329321));
#72137=CARTESIAN_POINT('Ctrl Pts',(29.3457826693465,2.63968660397804,31.6070390220085));
#72138=CARTESIAN_POINT('Ctrl Pts',(29.3346398644508,2.6541425833226,31.6237706303625));
#72139=CARTESIAN_POINT('',(29.3811946946869,2.63126513885323,31.5905494329235));
#72140=CARTESIAN_POINT('Origin',(29.367676739957,2.63381590833401,31.5962050111235));
#72141=CARTESIAN_POINT('',(29.3878847039279,2.66692553831851,31.6237706303691));
#72142=CARTESIAN_POINT('Ctrl Pts',(29.3878847039265,2.66692553831136,31.6237706303626));
#72143=CARTESIAN_POINT('Ctrl Pts',(29.3845192693509,2.64898643882447,31.6070390219952));
#72144=CARTESIAN_POINT('Ctrl Pts',(29.3811946946833,2.63126513883434,31.5905494329059));
#72145=CARTESIAN_POINT('',(29.5449325747123,2.69816430208817,31.6237706303691));
#72146=CARTESIAN_POINT('Origin',(30.,-1.32966554433622E-14,31.6237706303681));
#72147=CARTESIAN_POINT('',(29.5647599813892,2.6677785445999,31.5905494329235));
#72148=CARTESIAN_POINT('Ctrl Pts',(29.5647599813841,2.66777854460778,31.5905494329321));
#72149=CARTESIAN_POINT('Ctrl Pts',(29.554906826996,2.6828786313014,31.6070390220085));
#72150=CARTESIAN_POINT('Ctrl Pts',(29.5449325747163,2.69816430208207,31.6237706303625));
#72151=CARTESIAN_POINT('',(29.589548948342,2.67170473125694,31.5905494329235));
#72152=CARTESIAN_POINT('Origin',(29.5762727932907,2.67530826149244,31.5962050315749));
#72153=CARTESIAN_POINT('',(29.5990162172125,2.70673030953627,31.6237706303691));
#72154=CARTESIAN_POINT('Ctrl Pts',(29.5990162172106,2.70673030952925,31.6237706303625));
#72155=CARTESIAN_POINT('Ctrl Pts',(29.5942536716227,2.68911055925274,31.6070390219952));
#72156=CARTESIAN_POINT('Ctrl Pts',(29.589548948337,2.67170473123838,31.5905494329059));
#72157=CARTESIAN_POINT('',(29.7580309269804,2.72555094069491,31.6237706303691));
#72158=CARTESIAN_POINT('Origin',(30.,-1.32966554433622E-14,31.6237706303681));
#72159=CARTESIAN_POINT('',(29.775413173324,2.69370321195775,31.5905494329235));
#72160=CARTESIAN_POINT('Ctrl Pts',(29.7754131733195,2.69370321196601,31.5905494329321));
#72161=CARTESIAN_POINT('Ctrl Pts',(29.7667751320655,2.7095298197151,31.6070390220085));
#72162=CARTESIAN_POINT('Ctrl Pts',(29.7580309269838,2.72555094068851,31.6237706303625));
#72163=CARTESIAN_POINT('',(29.8004337692194,2.69567237556048,31.5905494329235));
#72164=CARTESIAN_POINT('Origin',(29.7874812679388,2.70030645711977,31.5962050602857));
#72165=CARTESIAN_POINT('',(29.8126199288586,2.72984718831658,31.6237706303691));
#72166=CARTESIAN_POINT('Ctrl Pts',(29.8126199288562,2.72984718830972,31.6237706303625));
#72167=CARTESIAN_POINT('Ctrl Pts',(29.8064896349333,2.71265541886322,31.6070390219952));
#72168=CARTESIAN_POINT('Ctrl Pts',(29.800433769213,2.69567237554238,31.5905494329059));
#72169=CARTESIAN_POINT('',(29.9726210990465,2.73613365141461,31.6237706303691));
#72170=CARTESIAN_POINT('Origin',(30.,-1.32966554433622E-14,31.6237706303681));
#72171=CARTESIAN_POINT('',(29.987451017728,2.70302030326666,31.5905494329235));
#72172=CARTESIAN_POINT('Ctrl Pts',(29.9874510177241,2.70302030327525,31.5905494329321));
#72173=CARTESIAN_POINT('Ctrl Pts',(29.9800813460009,2.71947585578017,31.6070390220085));
#72174=CARTESIAN_POINT('Ctrl Pts',(29.9726210990495,2.73613365140797,31.6237706303625));
#72175=CARTESIAN_POINT('Ctrl Pts',(30.,2.69489040503946,31.5823904050395));
#72176=CARTESIAN_POINT('Ctrl Pts',(29.9982996971592,2.69489040503946,31.5823904050395));
#72177=CARTESIAN_POINT('Ctrl Pts',(29.9965490639354,2.69522714758866,31.5827289231894));
#72178=CARTESIAN_POINT('Ctrl Pts',(29.9934248389279,2.69644647069982,31.5839540167345));
#72179=CARTESIAN_POINT('Ctrl Pts',(29.9920523583067,2.69733049287039,31.5848419899159));
#72180=CARTESIAN_POINT('Ctrl Pts',(29.9894391186861,2.6996015700298,31.5871217896387));
#72181=CARTESIAN_POINT('Ctrl Pts',(29.9882404972758,2.70125749446876,31.5887829779419));
#72182=CARTESIAN_POINT('Ctrl Pts',(29.987451017728,2.70302030326666,31.5905494329235));
#72183=CARTESIAN_POINT('',(30.,2.68872936963187,31.5762293696319));
#72184=CARTESIAN_POINT('',(30.,2.68872936963187,31.5762293696319));
#72185=CARTESIAN_POINT('',(30.,-2.68872936963189,31.5762293696319));
#72186=CARTESIAN_POINT('Origin',(30.,-1.32966554433622E-14,31.5762293696319));
#72187=CARTESIAN_POINT('Origin',(30.,-1.32966554433622E-14,31.5762293696319));
#72188=CARTESIAN_POINT('Origin',(30.,-1.32966554433622E-14,31.5430837392638));
#72189=CARTESIAN_POINT('',(30.,-2.67500000000001,31.5430837392638));
#72190=CARTESIAN_POINT('Origin',(30.,-1.32966554433622E-14,31.5430837392638));
#72191=CARTESIAN_POINT('Origin',(30.,-2.72187500000001,31.5430837392638));
#72192=CARTESIAN_POINT('Origin',(30.,-1.32966554433622E-14,16.));
#72193=CARTESIAN_POINT('',(30.,-2.67500000000001,31.06875));
#72194=CARTESIAN_POINT('Origin',(30.,-1.32966554433622E-14,31.06875));
#72195=CARTESIAN_POINT('',(30.,-2.67500000000001,16.));
#72196=CARTESIAN_POINT('Origin',(30.,-1.32966554433622E-14,31.06875));
#72197=CARTESIAN_POINT('',(30.,-2.60625000000001,31.));
#72198=CARTESIAN_POINT('Origin',(30.,-1.32966554433622E-14,31.));
#72199=CARTESIAN_POINT('Origin',(30.,-2.60625000000001,31.06875));
#72200=CARTESIAN_POINT('Origin',(30.,-1.32966554433622E-14,30.85));
#72201=CARTESIAN_POINT('',(30.,-1.65000000000002,31.));
#72202=CARTESIAN_POINT('Origin',(30.,-1.65000000000001,30.85));
#72203=CARTESIAN_POINT('Origin',(30.,-1.32966554433622E-14,31.));
#72204=CARTESIAN_POINT('Origin',(30.,-1.32966554433622E-14,31.6569162607362));
#72205=CARTESIAN_POINT('',(27.4723387620945,1.08324912480478,31.6569162607362));
#72206=CARTESIAN_POINT('Origin',(27.5075595450194,1.04598613791953,31.6570432561871));
#72207=CARTESIAN_POINT('',(27.5347062454699,1.21853465435945,31.6569162607362));
#72208=CARTESIAN_POINT('Origin',(30.,-1.32966554433622E-14,31.6569162607362));
#72209=CARTESIAN_POINT('Origin',(27.5859112932463,1.21595145595199,31.6570220656254));
#72210=CARTESIAN_POINT('Origin',(30.,-1.32966554433622E-14,31.6569162607362));
#72211=CARTESIAN_POINT('',(27.4467007962708,1.0213536000015,31.6569162607362));
#72212=CARTESIAN_POINT('Origin',(27.4979506713832,1.02279586647784,31.6570220656247));
#72213=CARTESIAN_POINT('',(27.3951399513465,0.881591814236737,31.6569162607362));
#72214=CARTESIAN_POINT('Origin',(27.4331757806072,0.847207087483285,31.6570432561871));
#72215=CARTESIAN_POINT('Origin',(30.,-1.32966554433622E-14,31.6569162607362));
#72216=CARTESIAN_POINT('Origin',(30.,-1.32966554433622E-14,31.6569162607362));
#72217=CARTESIAN_POINT('',(27.3744372857209,0.817875561065013,31.6569162607362));
#72218=CARTESIAN_POINT('Origin',(27.4254160156494,0.82333440037271,31.6570220656251));
#72219=CARTESIAN_POINT('',(27.3340009690024,0.674499196974899,31.6569162607362));
#72220=CARTESIAN_POINT('Origin',(27.3746173410621,0.643204723628532,31.6570432561866));
#72221=CARTESIAN_POINT('Origin',(30.,-1.32966554433622E-14,31.6569162607362));
#72222=CARTESIAN_POINT('Origin',(30.,-1.32966554433622E-14,31.6569162607362));
#72223=CARTESIAN_POINT('',(27.3183612423927,0.609355047323335,31.6569162607362));
#72224=CARTESIAN_POINT('Origin',(27.3687545263143,0.61879680390278,31.6570220656251));
#72225=CARTESIAN_POINT('',(27.2892987572189,0.463248067869971,31.6569162607362));
#72226=CARTESIAN_POINT('Origin',(27.3322452586394,0.435236788764015,31.6570432561869));
#72227=CARTESIAN_POINT('Origin',(30.,-1.32966554433622E-14,31.6569162607362));
#72228=CARTESIAN_POINT('Origin',(30.,-1.32966554433622E-14,31.6569162607362));
#72229=CARTESIAN_POINT('',(27.2788183937405,0.397077657083795,31.6569162607362));
#72230=CARTESIAN_POINT('Origin',(27.3283155403022,0.41044411936593,31.6570220656249));
#72231=CARTESIAN_POINT('',(27.2613089199969,0.249140860381007,31.6569162607362));
#72232=CARTESIAN_POINT('Origin',(27.3063207713152,0.224585474366194,31.6570432561871));
#72233=CARTESIAN_POINT('Origin',(30.,-1.32966554433622E-14,31.6569162607362));
#72234=CARTESIAN_POINT('Origin',(30.,-1.32966554433622E-14,31.6569162607362));
#72235=CARTESIAN_POINT('',(27.2560525345756,0.182352151046611,31.6569162607362));
#72236=CARTESIAN_POINT('Origin',(27.3043483774102,0.199560910346922,31.6570220656251));
#72237=CARTESIAN_POINT('',(27.2502040239902,0.0334976166400503,31.6569162607362));
#72238=CARTESIAN_POINT('Origin',(27.2970037121761,0.0125495158363338,31.6570432561875));
#72239=CARTESIAN_POINT('Origin',(30.,-1.32966554433622E-14,31.6569162607362));
#72240=CARTESIAN_POINT('Origin',(30.,-1.32966554433622E-14,31.6569162607362));
#72241=CARTESIAN_POINT('',(27.2502040239902,-0.0334976166400194,31.6569162607362));
#72242=CARTESIAN_POINT('Origin',(27.297000803166,-0.0125526580452972,31.6570220656252));
#72243=CARTESIAN_POINT('',(27.2560525345756,-0.18235215104658,31.6569162607362));
#72244=CARTESIAN_POINT('Origin',(27.3043515239857,-0.199563814630509,31.6570432561868));
#72245=CARTESIAN_POINT('Origin',(30.,-1.32966554433622E-14,31.6569162607362));
#72246=CARTESIAN_POINT('Origin',(30.,-1.32966554433622E-14,31.6569162607362));
#72247=CARTESIAN_POINT('',(27.2613089199969,-0.249140860380976,31.6569162607362));
#72248=CARTESIAN_POINT('Origin',(27.3063181178117,-0.22458883512474,31.6570220656265));
#72249=CARTESIAN_POINT('',(27.2788183937405,-0.397077657083763,31.6569162607362));
#72250=CARTESIAN_POINT('Origin',(27.3283189050458,-0.410446767819208,31.6570432561867));
#72251=CARTESIAN_POINT('Origin',(30.,-1.32966554433622E-14,31.6569162607362));
#72252=CARTESIAN_POINT('Origin',(30.,-1.32966554433622E-14,31.6569162607362));
#72253=CARTESIAN_POINT('',(27.2892987572189,-0.463248067869938,31.6569162607362));
#72254=CARTESIAN_POINT('Origin',(27.3322428769935,-0.4352403473568,31.6570220656245));
#72255=CARTESIAN_POINT('',(27.3183612423927,-0.609355047323306,31.6569162607362));
#72256=CARTESIAN_POINT('Origin',(27.3687580884808,-0.618799180197033,31.6570432561867));
#72257=CARTESIAN_POINT('Origin',(30.,-1.32966554433622E-14,31.6569162607362));
#72258=CARTESIAN_POINT('Origin',(30.,-1.32966554433622E-14,31.6569162607362));
#72259=CARTESIAN_POINT('',(27.3340009690024,-0.674499196974871,31.6569162607362));
#72260=CARTESIAN_POINT('Origin',(27.3746152459701,-0.643208458106799,31.6570220656281));
#72261=CARTESIAN_POINT('',(27.3744372857209,-0.817875561064986,31.6569162607362));
#72262=CARTESIAN_POINT('Origin',(27.4254197532793,-0.823336489857566,31.6570432561877));
#72263=CARTESIAN_POINT('Origin',(30.,-1.32966554433622E-14,31.6569162607362));
#72264=CARTESIAN_POINT('Origin',(30.,-1.32966554433622E-14,31.6569162607362));
#72265=CARTESIAN_POINT('',(27.3951399513465,-0.88159181423671,31.6569162607362));
#72266=CARTESIAN_POINT('Origin',(27.4331739849698,-0.847210974835381,31.6570220656246));
#72267=CARTESIAN_POINT('',(27.4467007962708,-1.02135360000148,31.6569162607362));
#72268=CARTESIAN_POINT('Origin',(27.4979545614299,-1.02279765627042,31.6570432561873));
#72269=CARTESIAN_POINT('Origin',(30.,-1.32966554433622E-14,31.6569162607362));
#72270=CARTESIAN_POINT('Origin',(30.,-1.32966554433622E-14,31.6569162607362));
#72271=CARTESIAN_POINT('',(27.4723387620945,-1.08324912480475,31.6569162607362));
#72272=CARTESIAN_POINT('Origin',(27.5075580599161,-1.04599015417175,31.657022065625));
#72273=CARTESIAN_POINT('',(27.5347062454699,-1.21853465435942,31.6569162607362));
#72274=CARTESIAN_POINT('Origin',(27.5859153117243,-1.21595293501783,31.6570432561869));
#72275=CARTESIAN_POINT('Origin',(30.,-1.32966554433622E-14,31.6569162607362));
#72276=CARTESIAN_POINT('Origin',(30.,-1.32966554433622E-14,31.6569162607362));
#72277=CARTESIAN_POINT('',(27.5651214449068,-1.27822784430149,31.6569162607362));
#72278=CARTESIAN_POINT('Origin',(27.5973088682438,-1.23832045638074,31.6570220656251));
#72279=CARTESIAN_POINT('',(27.637911050459,-1.40820303736935,31.6569162607362));
#72280=CARTESIAN_POINT('Origin',(27.6887596968882,-1.40161145957539,31.6570432561872));
#72281=CARTESIAN_POINT('Origin',(30.,-1.32966554433622E-14,31.6569162607362));
#72282=CARTESIAN_POINT('Origin',(30.,-1.32966554433622E-14,31.6569162607362));
#72283=CARTESIAN_POINT('',(27.6729159636906,-1.46532586408421,31.6569162607362));
#72284=CARTESIAN_POINT('Origin',(27.7018730663766,-1.42301610118967,31.6570220656267));
#72285=CARTESIAN_POINT('',(27.7556789192963,-1.58918938037887,31.6569162607362));
#72286=CARTESIAN_POINT('Origin',(27.8058536470839,-1.57862858340189,31.6570432561867));
#72287=CARTESIAN_POINT('Origin',(30.,-1.32966554433622E-14,31.6569162607362));
#72288=CARTESIAN_POINT('Origin',(30.,-1.32966554433622E-14,31.6569162607362));
#72289=CARTESIAN_POINT('',(27.7950577293922,-1.64338966264456,31.6569162607362));
#72290=CARTESIAN_POINT('Origin',(27.8206059812726,-1.59893837851,31.6570220656387));
#72291=CARTESIAN_POINT('',(27.8872837739086,-1.76037784239926,31.6569162607362));
#72292=CARTESIAN_POINT('Origin',(27.9364752391763,-1.7459129370637,31.6570432561874));
#72293=CARTESIAN_POINT('Origin',(30.,-1.32966554433622E-14,31.6569162607362));
#72294=CARTESIAN_POINT('Origin',(30.,-1.32966554433622E-14,31.6569162607362));
#72295=CARTESIAN_POINT('',(27.9307936974098,-1.81132141745219,31.6569162607362));
#72296=CARTESIAN_POINT('Origin',(27.9527755849842,-1.76500266908356,31.6570220656253));
#72297=CARTESIAN_POINT('',(28.0319142266042,-1.92071298963622,31.6569162607362));
#72298=CARTESIAN_POINT('Origin',(28.0798191476078,-1.90243315689441,31.657043256187));
#72299=CARTESIAN_POINT('Origin',(30.,-1.32966554433622E-14,31.6569162607362));
#72300=CARTESIAN_POINT('Origin',(30.,-1.32966554433622E-14,31.6569162607362));
#72301=CARTESIAN_POINT('',(28.0792870103637,-1.96808577339573,31.6569162607362));
#72302=CARTESIAN_POINT('Origin',(28.097567008002,-1.92018513125043,31.6570220656245));
#72303=CARTESIAN_POINT('',(28.1886785825478,-2.06920630259019,31.6569162607362));
#72304=CARTESIAN_POINT('Origin',(28.2350016095212,-2.0472242436889,31.6570432561873));
#72305=CARTESIAN_POINT('Origin',(30.,-1.32966554433622E-14,31.6569162607362));
#72306=CARTESIAN_POINT('Origin',(30.,-1.32966554433622E-14,31.6569162607362));
#72307=CARTESIAN_POINT('',(28.2396221576007,-2.11271622609136,31.6569162607362));
#72308=CARTESIAN_POINT('Origin',(28.2540875630401,-2.06352901355267,31.6570220656256));
#72309=CARTESIAN_POINT('',(28.3566103373554,-2.20494227060778,31.6569162607362));
#72310=CARTESIAN_POINT('Origin',(28.4010658734316,-2.17939351225073,31.6570432561869));
#72311=CARTESIAN_POINT('Origin',(30.,-1.32966554433622E-14,31.6569162607362));
#72312=CARTESIAN_POINT('Origin',(30.,-1.32966554433622E-14,31.6569162607362));
#72313=CARTESIAN_POINT('',(28.4108106196211,-2.2443210807037,31.6569162607362));
#72314=CARTESIAN_POINT('Origin',(28.4213722488256,-2.19415055329735,31.6570220656249));
#72315=CARTESIAN_POINT('',(28.5346741359157,-2.32708403630936,31.6569162607362));
#72316=CARTESIAN_POINT('Origin',(28.5769880979323,-2.29812609508764,31.6570432561867));
#72317=CARTESIAN_POINT('Origin',(30.,-1.32966554433622E-14,31.6569162607362));
#72318=CARTESIAN_POINT('Origin',(30.,-1.32966554433622E-14,31.6569162607362));
#72319=CARTESIAN_POINT('',(28.5917969626306,-2.362088949541,31.6569162607362));
#72320=CARTESIAN_POINT('Origin',(28.5983896996446,-2.31124442525031,31.6570220656249));
#72321=CARTESIAN_POINT('',(28.7217721556985,-2.43487855509312,31.6569162607362));
#72322=CARTESIAN_POINT('Origin',(28.7616836640096,-2.40268996634326,31.6570432561868));
#72323=CARTESIAN_POINT('Origin',(30.,-1.32966554433622E-14,31.6569162607362));
#72324=CARTESIAN_POINT('Origin',(30.,-1.32966554433622E-14,31.6569162607362));
#72325=CARTESIAN_POINT('',(28.7814653456405,-2.46529375453011,31.6569162607362));
#72326=CARTESIAN_POINT('Origin',(28.784048544048,-2.41408870675338,31.6570220656255));
#72327=CARTESIAN_POINT('',(28.9167508751952,-2.52766123790546,31.6569162607362));
#72328=CARTESIAN_POINT('Origin',(28.9540138620808,-2.49244045498024,31.6570432561872));
#72329=CARTESIAN_POINT('Origin',(30.,-1.32966554433622E-14,31.6569162607362));
#72330=CARTESIAN_POINT('Origin',(30.,-1.32966554433622E-14,31.6569162607362));
#72331=CARTESIAN_POINT('',(28.9786463999985,-2.55329920372917,31.6569162607362));
#72332=CARTESIAN_POINT('Origin',(28.9772041335221,-2.50204932861609,31.657022065625));
#72333=CARTESIAN_POINT('',(29.1184081857632,-2.60486004865345,31.6569162607362));
#72334=CARTESIAN_POINT('Origin',(29.1527929125168,-2.56682421939275,31.6570432561872));
#72335=CARTESIAN_POINT('Origin',(30.,-1.32966554433622E-14,31.6569162607362));
#72336=CARTESIAN_POINT('Origin',(30.,-1.32966554433622E-14,31.6569162607362));
#72337=CARTESIAN_POINT('',(29.182124438935,-2.6255627142791,31.6569162607362));
#72338=CARTESIAN_POINT('Origin',(29.1766655996274,-2.57458398435135,31.6570220656246));
#72339=CARTESIAN_POINT('',(29.3255008030251,-2.66599903099763,31.6569162607362));
#72340=CARTESIAN_POINT('Origin',(29.3567952763715,-2.62538265893786,31.6570432561866));
#72341=CARTESIAN_POINT('Origin',(30.,-1.32966554433622E-14,31.6569162607362));
#72342=CARTESIAN_POINT('Origin',(30.,-1.32966554433622E-14,31.6569162607362));
#72343=CARTESIAN_POINT('',(29.3906449526766,-2.6816387576073,31.6569162607362));
#72344=CARTESIAN_POINT('Origin',(29.3812031960972,-2.63124547368565,31.6570220656251));
#72345=CARTESIAN_POINT('',(29.53675193213,-2.71070124278106,31.6569162607362));
#72346=CARTESIAN_POINT('Origin',(29.5647632112362,-2.66775474136028,31.6570432561871));
#72347=CARTESIAN_POINT('Origin',(30.,-1.32966554433622E-14,31.6569162607362));
#72348=CARTESIAN_POINT('Origin',(30.,-1.32966554433622E-14,31.6569162607362));
#72349=CARTESIAN_POINT('',(29.6029223429162,-2.72118160625948,31.6569162607362));
#72350=CARTESIAN_POINT('Origin',(29.5895558806344,-2.67168445969898,31.6570220656245));
#72351=CARTESIAN_POINT('',(29.750859139619,-2.73869108000313,31.6569162607362));
#72352=CARTESIAN_POINT('Origin',(29.7754145256345,-2.69367922868347,31.6570432561876));
#72353=CARTESIAN_POINT('Origin',(30.,-1.32966554433622E-14,31.6569162607362));
#72354=CARTESIAN_POINT('Origin',(30.,-1.32966554433622E-14,31.6569162607362));
#72355=CARTESIAN_POINT('',(29.8176478489534,-2.74394746542436,31.6569162607362));
#72356=CARTESIAN_POINT('Origin',(29.800439089653,-2.69565162258972,31.6570220656252));
#72357=CARTESIAN_POINT('',(29.9665023833599,-2.74979597600977,31.6569162607362));
#72358=CARTESIAN_POINT('Origin',(29.9874504841626,-2.70299628782621,31.6570432561866));
#72359=CARTESIAN_POINT('Origin',(30.,-1.32966554433622E-14,31.6569162607362));
#72360=CARTESIAN_POINT('Origin',(30.,-1.32966554433622E-14,31.6569162607362));
#72361=CARTESIAN_POINT('',(30.03349761664,-2.74979597600977,31.6569162607362));
#72362=CARTESIAN_POINT('Origin',(30.0125526580435,-2.70299919683014,31.6570220656269));
#72363=CARTESIAN_POINT('',(30.1823521510466,-2.74394746542436,31.6569162607362));
#72364=CARTESIAN_POINT('Origin',(30.1995638146306,-2.69564847601399,31.6570432561868));
#72365=CARTESIAN_POINT('Origin',(30.,-1.32966554433622E-14,31.6569162607362));
#72366=CARTESIAN_POINT('Origin',(30.,-1.32966554433622E-14,31.6569162607362));
#72367=CARTESIAN_POINT('',(30.2491408603809,-2.73869108000313,31.6569162607362));
#72368=CARTESIAN_POINT('Origin',(30.2245888351274,-2.69368188219317,31.6570220656245));
#72369=CARTESIAN_POINT('',(30.3970776570837,-2.72118160625948,31.6569162607362));
#72370=CARTESIAN_POINT('Origin',(30.4104467678196,-2.67168109495285,31.6570432561872));
#72371=CARTESIAN_POINT('Origin',(30.,-1.32966554433622E-14,31.6569162607362));
#72372=CARTESIAN_POINT('Origin',(30.,-1.32966554433622E-14,31.6569162607362));
#72373=CARTESIAN_POINT('',(30.4632480678699,-2.71070124278107,31.6569162607362));
#72374=CARTESIAN_POINT('Origin',(30.4352403473562,-2.66775712300563,31.6570220656249));
#72375=CARTESIAN_POINT('',(30.6093550473233,-2.68163875760731,31.6569162607362));
#72376=CARTESIAN_POINT('Origin',(30.6187991801974,-2.63124191151731,31.6570432561874));
#72377=CARTESIAN_POINT('Origin',(30.,-1.32966554433622E-14,31.6569162607362));
#72378=CARTESIAN_POINT('Origin',(30.,-1.32966554433622E-14,31.6569162607362));
#72379=CARTESIAN_POINT('',(30.6744991969748,-2.66599903099764,31.6569162607362));
#72380=CARTESIAN_POINT('Origin',(30.6432084581108,-2.62538475403506,31.6570220656255));
#72381=CARTESIAN_POINT('',(30.817875561065,-2.62556271427912,31.6569162607362));
#72382=CARTESIAN_POINT('Origin',(30.8233364898573,-2.57458024672293,31.6570432561868));
#72383=CARTESIAN_POINT('Origin',(30.,-1.32966554433622E-14,31.6569162607362));
#72384=CARTESIAN_POINT('Origin',(30.,-1.32966554433622E-14,31.6569162607362));
#72385=CARTESIAN_POINT('',(30.8815918142367,-2.60486004865346,31.6569162607362));
#72386=CARTESIAN_POINT('Origin',(30.8472109748348,-2.56682601502956,31.6570220656249));
#72387=CARTESIAN_POINT('',(31.0213536000014,-2.55329920372919,31.6569162607362));
#72388=CARTESIAN_POINT('Origin',(31.0227976562703,-2.50204543857134,31.6570432561867));
#72389=CARTESIAN_POINT('Origin',(30.,-1.32966554433622E-14,31.6569162607362));
#72390=CARTESIAN_POINT('Origin',(30.,-1.32966554433622E-14,31.6569162607362));
#72391=CARTESIAN_POINT('',(31.0832491248047,-2.52766123790547,31.6569162607362));
#72392=CARTESIAN_POINT('Origin',(31.0459901541642,-2.49244194007693,31.6570220656289));
#72393=CARTESIAN_POINT('',(31.2185346543594,-2.46529375453013,31.6569162607362));
#72394=CARTESIAN_POINT('Origin',(31.2159529350178,-2.41408468827489,31.6570432561872));
#72395=CARTESIAN_POINT('Origin',(30.,-1.32966554433622E-14,31.6569162607362));
#72396=CARTESIAN_POINT('Origin',(30.,-1.32966554433622E-14,31.6569162607362));
#72397=CARTESIAN_POINT('',(31.2782278443015,-2.43487855509314,31.6569162607362));
#72398=CARTESIAN_POINT('Origin',(31.238320456382,-2.40269113175716,31.6570220656245));
#72399=CARTESIAN_POINT('',(31.4082030373693,-2.36208894954102,31.6569162607362));
#72400=CARTESIAN_POINT('Origin',(31.4016114595753,-2.31124030311134,31.6570432561875));
#72401=CARTESIAN_POINT('Origin',(30.,-1.32966554433622E-14,31.6569162607362));
#72402=CARTESIAN_POINT('Origin',(30.,-1.32966554433622E-14,31.6569162607362));
#72403=CARTESIAN_POINT('',(31.4653258640842,-2.32708403630938,31.6569162607362));
#72404=CARTESIAN_POINT('Origin',(31.4230161011935,-2.29812693362589,31.657022065625));
#72405=CARTESIAN_POINT('',(31.5891893803788,-2.24432108070372,31.6569162607362));
#72406=CARTESIAN_POINT('Origin',(31.5786285834021,-2.1941463529175,31.6570432561862));
#72407=CARTESIAN_POINT('Origin',(30.,-1.32966554433622E-14,31.6569162607362));
#72408=CARTESIAN_POINT('Origin',(30.,-1.32966554433622E-14,31.6569162607362));
#72409=CARTESIAN_POINT('',(31.6433896626445,-2.2049422706078,31.6569162607362));
#72410=CARTESIAN_POINT('Origin',(31.5989383785409,-2.17939401874466,31.6570220656252));
#72411=CARTESIAN_POINT('',(31.7603778423992,-2.11271622609138,31.6569162607362));
#72412=CARTESIAN_POINT('Origin',(31.7459129370641,-2.0635247608251,31.6570432561869));
#72413=CARTESIAN_POINT('Origin',(30.,-1.32966554433622E-14,31.6569162607362));
#72414=CARTESIAN_POINT('Origin',(30.,-1.32966554433622E-14,31.6569162607362));
#72415=CARTESIAN_POINT('',(31.8113214174522,-2.06920630259022,31.6569162607362));
#72416=CARTESIAN_POINT('Origin',(31.7650026690826,-2.04722441501533,31.6570220656257));
#72417=CARTESIAN_POINT('',(31.9207129896362,-1.96808577339576,31.6569162607362));
#72418=CARTESIAN_POINT('Origin',(31.9024331568943,-1.92018085239205,31.657043256187));
#72419=CARTESIAN_POINT('Origin',(30.,-1.32966554433622E-14,31.6569162607362));
#72420=CARTESIAN_POINT('Origin',(30.,-1.32966554433622E-14,31.6569162607362));
#72421=CARTESIAN_POINT('',(31.9680857733957,-1.92071298963625,31.6569162607362));
#72422=CARTESIAN_POINT('Origin',(31.9201851312437,-1.90243299199549,31.6570220656273));
#72423=CARTESIAN_POINT('',(32.0692063025902,-1.81132141745222,31.6569162607362));
#72424=CARTESIAN_POINT('Origin',(32.0472242436891,-1.76499839047944,31.6570432561871));
#72425=CARTESIAN_POINT('Origin',(30.,-1.32966554433622E-14,31.6569162607362));
#72426=CARTESIAN_POINT('Origin',(30.,-1.32966554433622E-14,31.6569162607362));
#72427=CARTESIAN_POINT('',(32.1127162260913,-1.76037784239929,31.6569162607362));
#72428=CARTESIAN_POINT('Origin',(32.0635290135546,-1.74591243696045,31.6570220656248));
#72429=CARTESIAN_POINT('',(32.2049422706077,-1.64338966264459,31.6569162607362));
#72430=CARTESIAN_POINT('Origin',(32.1793935122505,-1.59893412656801,31.6570432561871));
#72431=CARTESIAN_POINT('Origin',(30.,-1.32966554433622E-14,31.6569162607362));
#72432=CARTESIAN_POINT('Origin',(30.,-1.32966554433622E-14,31.6569162607362));
#72433=CARTESIAN_POINT('',(32.2443210807037,-1.5891893803789,31.6569162607362));
#72434=CARTESIAN_POINT('Origin',(32.1941505532956,-1.57862775117404,31.6570220656256));
#72435=CARTESIAN_POINT('',(32.3270840363093,-1.46532586408424,31.6569162607362));
#72436=CARTESIAN_POINT('Origin',(32.2981260950875,-1.42301190206755,31.6570432561867));
#72437=CARTESIAN_POINT('Origin',(30.,-1.32966554433622E-14,31.6569162607362));
#72438=CARTESIAN_POINT('Origin',(30.,-1.32966554433622E-14,31.6569162607362));
#72439=CARTESIAN_POINT('',(32.362088949541,-1.40820303736938,31.6569162607362));
#72440=CARTESIAN_POINT('Origin',(32.3112444252322,-1.40161030035328,31.657022065632));
#72441=CARTESIAN_POINT('',(32.4348785550931,-1.27822784430152,31.6569162607362));
#72442=CARTESIAN_POINT('Origin',(32.4026899663432,-1.23831633599041,31.6570432561868));
#72443=CARTESIAN_POINT('Origin',(30.,-1.32966554433622E-14,31.6569162607362));
#72444=CARTESIAN_POINT('Origin',(30.,-1.32966554433622E-14,31.6569162607362));
#72445=CARTESIAN_POINT('',(32.4652937545301,-1.21853465435946,31.6569162607362));
#72446=CARTESIAN_POINT('Origin',(32.414088706754,-1.21595145595202,31.6570220656252));
#72447=CARTESIAN_POINT('',(32.5276612379054,-1.08324912480479,31.6569162607362));
#72448=CARTESIAN_POINT('Origin',(32.4924404549811,-1.04598613792014,31.6570432561868));
#72449=CARTESIAN_POINT('Origin',(30.,-1.32966554433622E-14,31.6569162607362));
#72450=CARTESIAN_POINT('Origin',(30.,-1.32966554433622E-14,31.6569162607362));
#72451=CARTESIAN_POINT('',(32.5532992037291,-1.02135360000151,31.6569162607362));
#72452=CARTESIAN_POINT('Origin',(32.5020493286151,-1.0227958664779,31.6570220656254));
#72453=CARTESIAN_POINT('',(32.6048600486534,-0.881591814236746,31.6569162607362));
#72454=CARTESIAN_POINT('Origin',(32.5668242193914,-0.847207087482045,31.6570432561878));
#72455=CARTESIAN_POINT('Origin',(30.,-1.32966554433622E-14,31.6569162607362));
#72456=CARTESIAN_POINT('Origin',(30.,-1.32966554433622E-14,31.6569162607362));
#72457=CARTESIAN_POINT('',(32.6255627142791,-0.817875561065022,31.6569162607362));
#72458=CARTESIAN_POINT('Origin',(32.5745839843496,-0.82333440037284,31.6570220656255));
#72459=CARTESIAN_POINT('',(32.6659990309976,-0.674499196974908,31.6569162607362));
#72460=CARTESIAN_POINT('Origin',(32.6253826589374,-0.643204723628158,31.6570432561868));
#72461=CARTESIAN_POINT('Origin',(30.,-1.32966554433622E-14,31.6569162607362));
#72462=CARTESIAN_POINT('Origin',(30.,-1.32966554433622E-14,31.6569162607362));
#72463=CARTESIAN_POINT('',(32.6816387576073,-0.609355047323343,31.6569162607362));
#72464=CARTESIAN_POINT('Origin',(32.6312454736857,-0.618796803902764,31.657022065625));
#72465=CARTESIAN_POINT('',(32.710701242781,-0.463248067869977,31.6569162607362));
#72466=CARTESIAN_POINT('Origin',(32.6677547413593,-0.435236788763208,31.6570432561875));
#72467=CARTESIAN_POINT('Origin',(30.,-1.32966554433622E-14,31.6569162607362));
#72468=CARTESIAN_POINT('Origin',(30.,-1.32966554433622E-14,31.6569162607362));
#72469=CARTESIAN_POINT('',(32.7211816062594,-0.397077657083801,31.6569162607362));
#72470=CARTESIAN_POINT('Origin',(32.6716844596186,-0.410444119388296,31.6570220656567));
#72471=CARTESIAN_POINT('',(32.7386910800031,-0.249140860381013,31.6569162607362));
#72472=CARTESIAN_POINT('Origin',(32.6936792286845,-0.224585474366052,31.6570432561872));
#72473=CARTESIAN_POINT('Origin',(30.,-1.32966554433622E-14,31.6569162607362));
#72474=CARTESIAN_POINT('Origin',(30.,-1.32966554433622E-14,31.6569162607362));
#72475=CARTESIAN_POINT('',(32.7439474654243,-0.182352151046618,31.6569162607362));
#72476=CARTESIAN_POINT('Origin',(32.695651622591,-0.19956091034649,31.6570220656247));
#72477=CARTESIAN_POINT('',(32.7497959760097,-0.0334976166400576,31.6569162607362));
#72478=CARTESIAN_POINT('Origin',(32.702996287825,-0.0125495158368562,31.657043256187));
#72479=CARTESIAN_POINT('Origin',(30.,-1.32966554433622E-14,31.6569162607362));
#72480=CARTESIAN_POINT('Origin',(30.,-1.32966554433622E-14,31.6569162607362));
#72481=CARTESIAN_POINT('',(32.7497959760097,0.0334976166400122,31.6569162607362));
#72482=CARTESIAN_POINT('Origin',(32.7029991968315,0.0125526580441019,31.6570220656263));
#72483=CARTESIAN_POINT('',(32.7439474654243,0.182352151046572,31.6569162607362));
#72484=CARTESIAN_POINT('Origin',(32.695648476013,0.199563814630937,31.6570432561873));
#72485=CARTESIAN_POINT('Origin',(30.,-1.32966554433622E-14,31.6569162607362));
#72486=CARTESIAN_POINT('Origin',(30.,-1.32966554433622E-14,31.6569162607362));
#72487=CARTESIAN_POINT('',(32.7386910800031,0.249140860380968,31.6569162607362));
#72488=CARTESIAN_POINT('Origin',(32.6936818821912,0.224588835126342,31.6570220656253));
#72489=CARTESIAN_POINT('',(32.7211816062594,0.397077657083756,31.6569162607362));
#72490=CARTESIAN_POINT('Origin',(32.6716810949533,0.410446767819417,31.657043256187));
#72491=CARTESIAN_POINT('Origin',(30.,-1.32966554433622E-14,31.6569162607362));
#72492=CARTESIAN_POINT('Origin',(30.,-1.32966554433622E-14,31.6569162607362));
#72493=CARTESIAN_POINT('',(32.710701242781,0.463248067869931,31.6569162607362));
#72494=CARTESIAN_POINT('Origin',(32.6677571230054,0.435240347356078,31.6570220656249));
#72495=CARTESIAN_POINT('',(32.6816387576073,0.609355047323298,31.6569162607362));
#72496=CARTESIAN_POINT('Origin',(32.6312419115184,0.618799180197174,31.657043256187));
#72497=CARTESIAN_POINT('Origin',(30.,-1.32966554433622E-14,31.6569162607362));
#72498=CARTESIAN_POINT('Origin',(30.,-1.32966554433622E-14,31.6569162607362));
#72499=CARTESIAN_POINT('',(32.6659990309976,0.674499196974863,31.6569162607362));
#72500=CARTESIAN_POINT('Origin',(32.6253847539863,0.643208458072405,31.6570220656495));
#72501=CARTESIAN_POINT('',(32.6255627142791,0.817875561064977,31.6569162607362));
#72502=CARTESIAN_POINT('Origin',(32.574580246722,0.823336489857403,31.6570432561872));
#72503=CARTESIAN_POINT('Origin',(30.,-1.32966554433622E-14,31.6569162607362));
#72504=CARTESIAN_POINT('Origin',(30.,-1.32966554433622E-14,31.6569162607362));
#72505=CARTESIAN_POINT('',(32.6048600486534,0.881591814236701,31.6569162607362));
#72506=CARTESIAN_POINT('Origin',(32.5668260150295,0.847210974834854,31.6570220656249));
#72507=CARTESIAN_POINT('',(32.5532992037291,1.02135360000147,31.6569162607362));
#72508=CARTESIAN_POINT('Origin',(32.5020454385711,1.02279765627039,31.6570432561869));
#72509=CARTESIAN_POINT('Origin',(30.,-1.32966554433622E-14,31.6569162607362));
#72510=CARTESIAN_POINT('Origin',(30.,-1.32966554433622E-14,31.6569162607362));
#72511=CARTESIAN_POINT('',(32.5276612379054,1.08324912480474,31.6569162607362));
#72512=CARTESIAN_POINT('Origin',(32.4924419400839,1.04599015417185,31.6570220656248));
#72513=CARTESIAN_POINT('',(32.4652937545301,1.21853465435941,31.6569162607362));
#72514=CARTESIAN_POINT('Origin',(32.4140846882753,1.2159529350178,31.657043256187));
#72515=CARTESIAN_POINT('Origin',(30.,-1.32966554433622E-14,31.6569162607362));
#72516=CARTESIAN_POINT('Origin',(30.,-1.32966554433622E-14,31.6569162607362));
#72517=CARTESIAN_POINT('',(32.4348785550931,1.27822784430148,31.6569162607362));
#72518=CARTESIAN_POINT('Origin',(32.4026911317566,1.23832045638126,31.6570220656248));
#72519=CARTESIAN_POINT('',(32.362088949541,1.40820303736934,31.6569162607362));
#72520=CARTESIAN_POINT('Origin',(32.3112403031114,1.40161145957535,31.6570432561874));
#72521=CARTESIAN_POINT('Origin',(30.,-1.32966554433622E-14,31.6569162607362));
#72522=CARTESIAN_POINT('Origin',(30.,-1.32966554433622E-14,31.6569162607362));
#72523=CARTESIAN_POINT('',(32.3270840363093,1.4653258640842,31.6569162607362));
#72524=CARTESIAN_POINT('Origin',(32.2981269336259,1.42301610119356,31.657022065625));
#72525=CARTESIAN_POINT('',(32.2443210807037,1.58918938037886,31.6569162607362));
#72526=CARTESIAN_POINT('Origin',(32.1941463529162,1.57862858340189,31.6570432561866));
#72527=CARTESIAN_POINT('Origin',(30.,-1.32966554433622E-14,31.6569162607362));
#72528=CARTESIAN_POINT('Origin',(30.,-1.32966554433622E-14,31.6569162607362));
#72529=CARTESIAN_POINT('',(32.2049422706078,1.64338966264455,31.6569162607362));
#72530=CARTESIAN_POINT('Origin',(32.1793940187453,1.59893837854221,31.6570220656245));
#72531=CARTESIAN_POINT('',(32.1127162260913,1.76037784239925,31.6569162607362));
#72532=CARTESIAN_POINT('Origin',(32.0635247608241,1.74591293706383,31.6570432561872));
#72533=CARTESIAN_POINT('Origin',(30.,-1.32966554433622E-14,31.6569162607362));
#72534=CARTESIAN_POINT('Origin',(30.,-1.32966554433622E-14,31.6569162607362));
#72535=CARTESIAN_POINT('',(32.0692063025902,1.81132141745218,31.6569162607362));
#72536=CARTESIAN_POINT('Origin',(32.0472244150162,1.76500266908448,31.6570220656248));
#72537=CARTESIAN_POINT('',(31.9680857733957,1.92071298963621,31.6569162607362));
#72538=CARTESIAN_POINT('Origin',(31.9201808523931,1.90243315689474,31.6570432561866));
#72539=CARTESIAN_POINT('Origin',(30.,-1.32966554433622E-14,31.6569162607362));
#72540=CARTESIAN_POINT('Origin',(30.,-1.32966554433622E-14,31.6569162607362));
#72541=CARTESIAN_POINT('',(31.9207129896362,1.96808577339572,31.6569162607362));
#72542=CARTESIAN_POINT('Origin',(31.9024329919958,1.92018513124459,31.657022065627));
#72543=CARTESIAN_POINT('',(31.8113214174522,2.06920630259018,31.6569162607362));
#72544=CARTESIAN_POINT('Origin',(31.7649983904793,2.04722424368911,31.6570432561871));
#72545=CARTESIAN_POINT('Origin',(30.,-1.32966554433622E-14,31.6569162607362));
#72546=CARTESIAN_POINT('Origin',(30.,-1.32966554433622E-14,31.6569162607362));
#72547=CARTESIAN_POINT('',(31.7603778423992,2.11271622609134,31.6569162607362));
#72548=CARTESIAN_POINT('Origin',(31.7459124369604,2.06352901355459,31.6570220656248));
#72549=CARTESIAN_POINT('',(31.6433896626445,2.20494227060776,31.6569162607362));
#72550=CARTESIAN_POINT('Origin',(31.5989341265682,2.17939351225069,31.657043256187));
#72551=CARTESIAN_POINT('Origin',(30.,-1.32966554433622E-14,31.6569162607362));
#72552=CARTESIAN_POINT('Origin',(30.,-1.32966554433622E-14,31.6569162607362));
#72553=CARTESIAN_POINT('',(31.5891893803789,2.24432108070368,31.6569162607362));
#72554=CARTESIAN_POINT('Origin',(31.5786277511742,2.19415055329685,31.6570220656251));
#72555=CARTESIAN_POINT('',(31.4653258640842,2.32708403630934,31.6569162607362));
#72556=CARTESIAN_POINT('Origin',(31.4230119020666,2.29812609508688,31.6570432561872));
#72557=CARTESIAN_POINT('Origin',(30.,-1.32966554433622E-14,31.6569162607362));
#72558=CARTESIAN_POINT('Origin',(30.,-1.32966554433622E-14,31.6569162607362));
#72559=CARTESIAN_POINT('',(31.4082030373693,2.36208894954099,31.6569162607362));
#72560=CARTESIAN_POINT('Origin',(31.4016103003533,2.31124442523252,31.6570220656319));
#72561=CARTESIAN_POINT('',(31.2782278443015,2.4348785550931,31.6569162607362));
#72562=CARTESIAN_POINT('Origin',(31.2383163359906,2.4026899663434,31.6570432561867));
#72563=CARTESIAN_POINT('Origin',(30.,-1.32966554433622E-14,31.6569162607362));
#72564=CARTESIAN_POINT('Origin',(30.,-1.32966554433622E-14,31.6569162607362));
#72565=CARTESIAN_POINT('',(31.2185346543594,2.46529375453009,31.6569162607362));
#72566=CARTESIAN_POINT('Origin',(31.215951455952,2.4140887067551,31.6570220656248));
#72567=CARTESIAN_POINT('',(31.0832491248047,2.52766123790544,31.6569162607362));
#72568=CARTESIAN_POINT('Origin',(31.045986137919,2.49244045498011,31.6570432561873));
#72569=CARTESIAN_POINT('Origin',(30.,-1.32966554433622E-14,31.6569162607362));
#72570=CARTESIAN_POINT('Origin',(30.,-1.32966554433622E-14,31.6569162607362));
#72571=CARTESIAN_POINT('',(31.0213536000015,2.55329920372915,31.6569162607362));
#72572=CARTESIAN_POINT('Origin',(31.0227958664779,2.50204932861496,31.6570220656254));
#72573=CARTESIAN_POINT('',(30.8815918142367,2.60486004865343,31.6569162607362));
#72574=CARTESIAN_POINT('Origin',(30.8472070874836,2.56682421939316,31.6570432561869));
#72575=CARTESIAN_POINT('Origin',(30.,-1.32966554433622E-14,31.6569162607362));
#72576=CARTESIAN_POINT('Origin',(30.,-1.32966554433622E-14,31.6569162607362));
#72577=CARTESIAN_POINT('',(30.817875561065,2.62556271427908,31.6569162607362));
#72578=CARTESIAN_POINT('Origin',(30.8233344003728,2.5745839843498,31.6570220656254));
#72579=CARTESIAN_POINT('',(30.6744991969749,2.6659990309976,31.6569162607362));
#72580=CARTESIAN_POINT('Origin',(30.6432047236281,2.62538265893739,31.6570432561868));
#72581=CARTESIAN_POINT('Origin',(30.,-1.32966554433622E-14,31.6569162607362));
#72582=CARTESIAN_POINT('Origin',(30.,-1.32966554433622E-14,31.6569162607362));
#72583=CARTESIAN_POINT('',(30.6093550473233,2.68163875760728,31.6569162607362));
#72584=CARTESIAN_POINT('Origin',(30.6187968039028,2.63124547368537,31.6570220656252));
#72585=CARTESIAN_POINT('',(30.4632480678699,2.71070124278104,31.6569162607362));
#72586=CARTESIAN_POINT('Origin',(30.4352367887645,2.66775474136143,31.6570432561865));
#72587=CARTESIAN_POINT('Origin',(30.,-1.32966554433622E-14,31.6569162607362));
#72588=CARTESIAN_POINT('Origin',(30.,-1.32966554433622E-14,31.6569162607362));
#72589=CARTESIAN_POINT('',(27.5651214449069,1.27822784430151,31.6569162607362));
#72590=CARTESIAN_POINT('Origin',(27.5973100336575,1.23831633598946,31.6570432561873));
#72591=CARTESIAN_POINT('',(27.637911050459,1.40820303736937,31.6569162607362));
#72592=CARTESIAN_POINT('Origin',(30.,-1.32966554433622E-14,31.6569162607362));
#72593=CARTESIAN_POINT('Origin',(27.6887555747495,1.40161030035545,31.6570220656248));
#72594=CARTESIAN_POINT('Origin',(30.,-1.32966554433622E-14,31.6569162607362));
#72595=CARTESIAN_POINT('',(27.6729159636906,1.46532586408423,31.6569162607362));
#72596=CARTESIAN_POINT('Origin',(27.7018739049127,1.42301190206727,31.6570432561868));
#72597=CARTESIAN_POINT('',(27.7556789192963,1.58918938037889,31.6569162607362));
#72598=CARTESIAN_POINT('Origin',(30.,-1.32966554433622E-14,31.6569162607362));
#72599=CARTESIAN_POINT('Origin',(27.805849446702,1.5786277511745,31.6570220656247));
#72600=CARTESIAN_POINT('Origin',(30.,-1.32966554433622E-14,31.6569162607362));
#72601=CARTESIAN_POINT('',(27.7950577293922,1.64338966264458,31.6569162607362));
#72602=CARTESIAN_POINT('Origin',(27.8206064877494,1.59893412656804,31.6570432561871));
#72603=CARTESIAN_POINT('',(27.8872837739086,1.76037784239928,31.6569162607362));
#72604=CARTESIAN_POINT('Origin',(30.,-1.32966554433622E-14,31.6569162607362));
#72605=CARTESIAN_POINT('Origin',(27.936470986445,1.74591243696058,31.6570220656246));
#72606=CARTESIAN_POINT('Origin',(30.,-1.32966554433622E-14,31.6569162607362));
#72607=CARTESIAN_POINT('',(27.9307936974098,1.81132141745221,31.6569162607362));
#72608=CARTESIAN_POINT('Origin',(27.9527757563104,1.76499839048029,31.6570432561867));
#72609=CARTESIAN_POINT('',(28.0319142266043,1.92071298963623,31.6569162607362));
#72610=CARTESIAN_POINT('Origin',(30.,-1.32966554433622E-14,31.6569162607362));
#72611=CARTESIAN_POINT('Origin',(28.0798148687497,1.90243299199796,31.6570220656246));
#72612=CARTESIAN_POINT('Origin',(30.,-1.32966554433622E-14,31.6569162607362));
#72613=CARTESIAN_POINT('',(28.0792870103638,1.96808577339574,31.6569162607362));
#72614=CARTESIAN_POINT('Origin',(28.0975668431059,1.92018085239124,31.6570432561874));
#72615=CARTESIAN_POINT('',(28.1886785825478,2.0692063025902,31.6569162607362));
#72616=CARTESIAN_POINT('Origin',(30.,-1.32966554433622E-14,31.6569162607362));
#72617=CARTESIAN_POINT('Origin',(28.2349973309159,2.04722441501599,31.657022065625));
#72618=CARTESIAN_POINT('Origin',(30.,-1.32966554433622E-14,31.6569162607362));
#72619=CARTESIAN_POINT('',(28.2396221576007,2.11271622609137,31.6569162607362));
#72620=CARTESIAN_POINT('Origin',(28.2540870629359,2.06352476082518,31.6570432561869));
#72621=CARTESIAN_POINT('',(28.3566103373554,2.20494227060779,31.6569162607362));
#72622=CARTESIAN_POINT('Origin',(30.,-1.32966554433622E-14,31.6569162607362));
#72623=CARTESIAN_POINT('Origin',(28.4010616214895,2.17939401872761,31.6570220656385));
#72624=CARTESIAN_POINT('Origin',(30.,-1.32966554433622E-14,31.6569162607362));
#72625=CARTESIAN_POINT('',(28.4108106196211,2.2443210807037,31.6569162607362));
#72626=CARTESIAN_POINT('Origin',(28.4213714165984,2.19414635291463,31.6570432561873));
#72627=CARTESIAN_POINT('',(28.5346741359158,2.32708403630936,31.6569162607362));
#72628=CARTESIAN_POINT('Origin',(30.,-1.32966554433622E-14,31.6569162607362));
#72629=CARTESIAN_POINT('Origin',(28.5769838988101,2.29812693362349,31.6570220656266));
#72630=CARTESIAN_POINT('Origin',(30.,-1.32966554433622E-14,31.6569162607362));
#72631=CARTESIAN_POINT('',(28.5917969626306,2.36208894954101,31.6569162607362));
#72632=CARTESIAN_POINT('Origin',(28.5983885404246,2.31124030311217,31.6570432561871));
#72633=CARTESIAN_POINT('',(28.7217721556985,2.43487855509312,31.6569162607362));
#72634=CARTESIAN_POINT('Origin',(30.,-1.32966554433622E-14,31.6569162607362));
#72635=CARTESIAN_POINT('Origin',(28.7616795436181,2.40269113175706,31.6570220656245));
#72636=CARTESIAN_POINT('Origin',(30.,-1.32966554433622E-14,31.6569162607362));
#72637=CARTESIAN_POINT('',(28.7814653456406,2.46529375453011,31.6569162607362));
#72638=CARTESIAN_POINT('Origin',(28.7840470649822,2.41408468827519,31.6570432561871));
#72639=CARTESIAN_POINT('',(28.9167508751953,2.52766123790545,31.6569162607362));
#72640=CARTESIAN_POINT('Origin',(30.,-1.32966554433622E-14,31.6569162607362));
#72641=CARTESIAN_POINT('Origin',(28.9540098458282,2.49244194008388,31.6570220656249));
#72642=CARTESIAN_POINT('Origin',(30.,-1.32966554433622E-14,31.6569162607362));
#72643=CARTESIAN_POINT('',(28.9786463999985,2.55329920372917,31.6569162607362));
#72644=CARTESIAN_POINT('Origin',(28.9772023437296,2.50204543857058,31.657043256187));
#72645=CARTESIAN_POINT('',(29.1184081857633,2.60486004865344,31.6569162607362));
#72646=CARTESIAN_POINT('Origin',(30.,-1.32966554433622E-14,31.6569162607362));
#72647=CARTESIAN_POINT('Origin',(29.1527890251647,2.56682601503002,31.6570220656247));
#72648=CARTESIAN_POINT('Origin',(30.,-1.32966554433622E-14,31.6569162607362));
#72649=CARTESIAN_POINT('',(29.182124438935,2.62556271427909,31.6569162607362));
#72650=CARTESIAN_POINT('Origin',(29.1766635101426,2.57458024672254,31.657043256187));
#72651=CARTESIAN_POINT('',(29.3255008030251,2.66599903099761,31.6569162607362));
#72652=CARTESIAN_POINT('Origin',(30.,-1.32966554433622E-14,31.6569162607362));
#72653=CARTESIAN_POINT('Origin',(29.356791541893,2.62538475403008,31.657022065628));
#72654=CARTESIAN_POINT('Origin',(30.,-1.32966554433622E-14,31.6569162607362));
#72655=CARTESIAN_POINT('',(29.3906449526767,2.68163875760729,31.6569162607362));
#72656=CARTESIAN_POINT('Origin',(29.3812008198028,2.6312419115181,31.6570432561872));
#72657=CARTESIAN_POINT('',(29.5367519321301,2.71070124278105,31.6569162607362));
#72658=CARTESIAN_POINT('Origin',(30.,-1.32966554433622E-14,31.6569162607362));
#72659=CARTESIAN_POINT('Origin',(29.5647596526443,2.66775712300484,31.6570220656252));
#72660=CARTESIAN_POINT('Origin',(30.,-1.32966554433622E-14,31.6569162607362));
#72661=CARTESIAN_POINT('',(29.6029223429162,2.72118160625946,31.6569162607362));
#72662=CARTESIAN_POINT('Origin',(29.5895532321803,2.67168109495224,31.6570432561874));
#72663=CARTESIAN_POINT('',(29.750859139619,2.7386910800031,31.6569162607362));
#72664=CARTESIAN_POINT('Origin',(30.,-1.32966554433622E-14,31.6569162607362));
#72665=CARTESIAN_POINT('Origin',(29.7754111648735,2.69368188219135,31.6570220656252));
#72666=CARTESIAN_POINT('Origin',(30.,-1.32966554433622E-14,31.6569162607362));
#72667=CARTESIAN_POINT('',(29.8176478489534,2.74394746542433,31.6569162607362));
#72668=CARTESIAN_POINT('Origin',(29.8004361853695,2.6956484760142,31.6570432561868));
#72669=CARTESIAN_POINT('',(29.9665023833599,2.74979597600974,31.6569162607362));
#72670=CARTESIAN_POINT('Origin',(30.,-1.32966554433622E-14,31.6569162607362));
#72671=CARTESIAN_POINT('Origin',(29.9874473419551,2.70299919683309,31.6570220656256));
#72672=CARTESIAN_POINT('Origin',(30.,-1.32966554433622E-14,31.6569162607362));
#72673=CARTESIAN_POINT('',(30.3970776570838,2.72118160625945,31.6569162607362));
#72674=CARTESIAN_POINT('Origin',(30.4104441193885,2.67168445961759,31.6570220656571));
#72675=CARTESIAN_POINT('',(30.249140860381,2.7386910800031,31.6569162607362));
#72676=CARTESIAN_POINT('Origin',(30.2245854743662,2.69367922868485,31.657043256187));
#72677=CARTESIAN_POINT('Origin',(30.,-1.32966554433622E-14,31.6569162607362));
#72678=CARTESIAN_POINT('Origin',(30.,-1.32966554433622E-14,16.));
#72679=CARTESIAN_POINT('',(27.4723387620945,1.08324912480478,33.8305837392638));
#72680=CARTESIAN_POINT('',(27.4723387620945,1.08324912480478,16.));
#72681=CARTESIAN_POINT('',(27.5347062454699,1.21853465435945,33.8305837392638));
#72682=CARTESIAN_POINT('Origin',(30.,-1.32966554433622E-14,33.8305837392638));
#72683=CARTESIAN_POINT('',(27.5347062454699,1.21853465435945,16.));
#72684=CARTESIAN_POINT('Origin',(30.,-1.32966554433622E-14,16.));
#72685=CARTESIAN_POINT('',(27.4467007962708,1.0213536000015,33.8305837392638));
#72686=CARTESIAN_POINT('',(27.4467007962708,1.0213536000015,16.));
#72687=CARTESIAN_POINT('',(27.3951399513465,0.881591814236741,33.8305837392638));
#72688=CARTESIAN_POINT('',(27.3951399513465,0.881591814236737,16.));
#72689=CARTESIAN_POINT('Origin',(30.,-1.32966554433622E-14,33.8305837392638));
#72690=CARTESIAN_POINT('Origin',(30.,-1.32966554433622E-14,16.));
#72691=CARTESIAN_POINT('',(27.3744372857209,0.817875561065013,33.8305837392638));
#72692=CARTESIAN_POINT('',(27.3744372857209,0.817875561065013,16.));
#72693=CARTESIAN_POINT('',(27.3340009690024,0.674499196974903,33.8305837392638));
#72694=CARTESIAN_POINT('',(27.3340009690024,0.674499196974899,16.));
#72695=CARTESIAN_POINT('Origin',(30.,-1.32966554433622E-14,33.8305837392638));
#72696=CARTESIAN_POINT('Origin',(30.,-1.32966554433622E-14,16.));
#72697=CARTESIAN_POINT('',(27.3183612423927,0.609355047323334,33.8305837392638));
#72698=CARTESIAN_POINT('',(27.3183612423927,0.609355047323335,16.));
#72699=CARTESIAN_POINT('',(27.2892987572189,0.463248067869974,33.8305837392638));
#72700=CARTESIAN_POINT('',(27.2892987572189,0.463248067869971,16.));
#72701=CARTESIAN_POINT('Origin',(30.,-1.32966554433622E-14,33.8305837392638));
#72702=CARTESIAN_POINT('Origin',(30.,-1.32966554433622E-14,16.));
#72703=CARTESIAN_POINT('',(27.2788183937405,0.397077657083793,33.8305837392638));
#72704=CARTESIAN_POINT('',(27.2788183937405,0.397077657083795,16.));
#72705=CARTESIAN_POINT('',(27.2613089199969,0.24914086038101,33.8305837392638));
#72706=CARTESIAN_POINT('',(27.2613089199969,0.249140860381007,16.));
#72707=CARTESIAN_POINT('Origin',(30.,-1.32966554433622E-14,33.8305837392638));
#72708=CARTESIAN_POINT('Origin',(30.,-1.32966554433622E-14,16.));
#72709=CARTESIAN_POINT('',(27.2560525345756,0.182352151046609,33.8305837392638));
#72710=CARTESIAN_POINT('',(27.2560525345756,0.182352151046611,16.));
#72711=CARTESIAN_POINT('',(27.2502040239902,0.0334976166400525,33.8305837392638));
#72712=CARTESIAN_POINT('',(27.2502040239902,0.0334976166400503,16.));
#72713=CARTESIAN_POINT('Origin',(30.,-1.32966554433622E-14,33.8305837392638));
#72714=CARTESIAN_POINT('Origin',(30.,-1.32966554433622E-14,16.));
#72715=CARTESIAN_POINT('',(27.2502040239902,-0.0334976166400219,33.8305837392638));
#72716=CARTESIAN_POINT('',(27.2502040239902,-0.0334976166400194,16.));
#72717=CARTESIAN_POINT('',(27.2560525345756,-0.182352151046578,33.8305837392638));
#72718=CARTESIAN_POINT('',(27.2560525345756,-0.18235215104658,16.));
#72719=CARTESIAN_POINT('Origin',(30.,-1.32966554433622E-14,33.8305837392638));
#72720=CARTESIAN_POINT('Origin',(30.,-1.32966554433622E-14,16.));
#72721=CARTESIAN_POINT('',(27.2613089199969,-0.249140860380979,33.8305837392638));
#72722=CARTESIAN_POINT('',(27.2613089199969,-0.249140860380976,16.));
#72723=CARTESIAN_POINT('',(27.2788183937405,-0.397077657083761,33.8305837392638));
#72724=CARTESIAN_POINT('',(27.2788183937405,-0.397077657083763,16.));
#72725=CARTESIAN_POINT('Origin',(30.,-1.32966554433622E-14,33.8305837392638));
#72726=CARTESIAN_POINT('Origin',(30.,-1.32966554433622E-14,16.));
#72727=CARTESIAN_POINT('',(27.2892987572189,-0.463248067869942,33.8305837392638));
#72728=CARTESIAN_POINT('',(27.2892987572189,-0.463248067869938,16.));
#72729=CARTESIAN_POINT('',(27.3183612423927,-0.609355047323305,33.8305837392638));
#72730=CARTESIAN_POINT('',(27.3183612423927,-0.609355047323306,16.));
#72731=CARTESIAN_POINT('Origin',(30.,-1.32966554433622E-14,33.8305837392638));
#72732=CARTESIAN_POINT('Origin',(30.,-1.32966554433622E-14,16.));
#72733=CARTESIAN_POINT('',(27.3340009690023,-0.674499196974875,33.8305837392638));
#72734=CARTESIAN_POINT('',(27.3340009690024,-0.674499196974871,16.));
#72735=CARTESIAN_POINT('',(27.3744372857209,-0.817875561064985,33.8305837392638));
#72736=CARTESIAN_POINT('',(27.3744372857209,-0.817875561064986,16.));
#72737=CARTESIAN_POINT('Origin',(30.,-1.32966554433622E-14,33.8305837392638));
#72738=CARTESIAN_POINT('Origin',(30.,-1.32966554433622E-14,16.));
#72739=CARTESIAN_POINT('',(27.3951399513465,-0.881591814236714,33.8305837392638));
#72740=CARTESIAN_POINT('',(27.3951399513465,-0.88159181423671,16.));
#72741=CARTESIAN_POINT('',(27.4467007962708,-1.02135360000148,33.8305837392638));
#72742=CARTESIAN_POINT('',(27.4467007962708,-1.02135360000148,16.));
#72743=CARTESIAN_POINT('Origin',(30.,-1.32966554433622E-14,33.8305837392638));
#72744=CARTESIAN_POINT('Origin',(30.,-1.32966554433622E-14,16.));
#72745=CARTESIAN_POINT('',(27.4723387620945,-1.08324912480476,33.8305837392638));
#72746=CARTESIAN_POINT('',(27.4723387620945,-1.08324912480475,16.));
#72747=CARTESIAN_POINT('',(27.5347062454699,-1.21853465435942,33.8305837392638));
#72748=CARTESIAN_POINT('',(27.5347062454699,-1.21853465435942,16.));
#72749=CARTESIAN_POINT('Origin',(30.,-1.32966554433622E-14,33.8305837392638));
#72750=CARTESIAN_POINT('Origin',(30.,-1.32966554433622E-14,16.));
#72751=CARTESIAN_POINT('',(27.5651214449068,-1.27822784430149,33.8305837392638));
#72752=CARTESIAN_POINT('',(27.5651214449068,-1.27822784430149,16.));
#72753=CARTESIAN_POINT('',(27.637911050459,-1.40820303736935,33.8305837392638));
#72754=CARTESIAN_POINT('',(27.637911050459,-1.40820303736935,16.));
#72755=CARTESIAN_POINT('Origin',(30.,-1.32966554433622E-14,33.8305837392638));
#72756=CARTESIAN_POINT('Origin',(30.,-1.32966554433622E-14,16.));
#72757=CARTESIAN_POINT('',(27.6729159636906,-1.46532586408422,33.8305837392638));
#72758=CARTESIAN_POINT('',(27.6729159636906,-1.46532586408421,16.));
#72759=CARTESIAN_POINT('',(27.7556789192963,-1.58918938037887,33.8305837392638));
#72760=CARTESIAN_POINT('',(27.7556789192963,-1.58918938037887,16.));
#72761=CARTESIAN_POINT('Origin',(30.,-1.32966554433622E-14,33.8305837392638));
#72762=CARTESIAN_POINT('Origin',(30.,-1.32966554433622E-14,16.));
#72763=CARTESIAN_POINT('',(27.7950577293922,-1.64338966264456,33.8305837392638));
#72764=CARTESIAN_POINT('',(27.7950577293922,-1.64338966264456,16.));
#72765=CARTESIAN_POINT('',(27.8872837739086,-1.76037784239926,33.8305837392638));
#72766=CARTESIAN_POINT('',(27.8872837739086,-1.76037784239926,16.));
#72767=CARTESIAN_POINT('Origin',(30.,-1.32966554433622E-14,33.8305837392638));
#72768=CARTESIAN_POINT('Origin',(30.,-1.32966554433622E-14,16.));
#72769=CARTESIAN_POINT('',(27.9307936974098,-1.81132141745219,33.8305837392638));
#72770=CARTESIAN_POINT('',(27.9307936974098,-1.81132141745219,16.));
#72771=CARTESIAN_POINT('',(28.0319142266042,-1.92071298963622,33.8305837392638));
#72772=CARTESIAN_POINT('',(28.0319142266042,-1.92071298963622,16.));
#72773=CARTESIAN_POINT('Origin',(30.,-1.32966554433622E-14,33.8305837392638));
#72774=CARTESIAN_POINT('Origin',(30.,-1.32966554433622E-14,16.));
#72775=CARTESIAN_POINT('',(28.0792870103637,-1.96808577339574,33.8305837392638));
#72776=CARTESIAN_POINT('',(28.0792870103637,-1.96808577339573,16.));
#72777=CARTESIAN_POINT('',(28.1886785825478,-2.06920630259019,33.8305837392638));
#72778=CARTESIAN_POINT('',(28.1886785825478,-2.06920630259019,16.));
#72779=CARTESIAN_POINT('Origin',(30.,-1.32966554433622E-14,33.8305837392638));
#72780=CARTESIAN_POINT('Origin',(30.,-1.32966554433622E-14,16.));
#72781=CARTESIAN_POINT('',(28.2396221576007,-2.11271622609136,33.8305837392638));
#72782=CARTESIAN_POINT('',(28.2396221576007,-2.11271622609136,16.));
#72783=CARTESIAN_POINT('',(28.3566103373554,-2.20494227060778,33.8305837392638));
#72784=CARTESIAN_POINT('',(28.3566103373554,-2.20494227060778,16.));
#72785=CARTESIAN_POINT('Origin',(30.,-1.32966554433622E-14,33.8305837392638));
#72786=CARTESIAN_POINT('Origin',(30.,-1.32966554433622E-14,16.));
#72787=CARTESIAN_POINT('',(28.4108106196211,-2.2443210807037,33.8305837392638));
#72788=CARTESIAN_POINT('',(28.4108106196211,-2.2443210807037,16.));
#72789=CARTESIAN_POINT('',(28.5346741359157,-2.32708403630936,33.8305837392638));
#72790=CARTESIAN_POINT('',(28.5346741359157,-2.32708403630936,16.));
#72791=CARTESIAN_POINT('Origin',(30.,-1.32966554433622E-14,33.8305837392638));
#72792=CARTESIAN_POINT('Origin',(30.,-1.32966554433622E-14,16.));
#72793=CARTESIAN_POINT('',(28.5917969626306,-2.36208894954101,33.8305837392638));
#72794=CARTESIAN_POINT('',(28.5917969626306,-2.362088949541,16.));
#72795=CARTESIAN_POINT('',(28.7217721556985,-2.43487855509313,33.8305837392638));
#72796=CARTESIAN_POINT('',(28.7217721556985,-2.43487855509312,16.));
#72797=CARTESIAN_POINT('Origin',(30.,-1.32966554433622E-14,33.8305837392638));
#72798=CARTESIAN_POINT('Origin',(30.,-1.32966554433622E-14,16.));
#72799=CARTESIAN_POINT('',(28.7814653456405,-2.46529375453011,33.8305837392638));
#72800=CARTESIAN_POINT('',(28.7814653456405,-2.46529375453011,16.));
#72801=CARTESIAN_POINT('',(28.9167508751952,-2.52766123790546,33.8305837392638));
#72802=CARTESIAN_POINT('',(28.9167508751952,-2.52766123790546,16.));
#72803=CARTESIAN_POINT('Origin',(30.,-1.32966554433622E-14,33.8305837392638));
#72804=CARTESIAN_POINT('Origin',(30.,-1.32966554433622E-14,16.));
#72805=CARTESIAN_POINT('',(28.9786463999985,-2.55329920372918,33.8305837392638));
#72806=CARTESIAN_POINT('',(28.9786463999985,-2.55329920372917,16.));
#72807=CARTESIAN_POINT('',(29.1184081857632,-2.60486004865345,33.8305837392638));
#72808=CARTESIAN_POINT('',(29.1184081857632,-2.60486004865345,16.));
#72809=CARTESIAN_POINT('Origin',(30.,-1.32966554433622E-14,33.8305837392638));
#72810=CARTESIAN_POINT('Origin',(30.,-1.32966554433622E-14,16.));
#72811=CARTESIAN_POINT('',(29.182124438935,-2.62556271427911,33.8305837392638));
#72812=CARTESIAN_POINT('',(29.182124438935,-2.6255627142791,16.));
#72813=CARTESIAN_POINT('',(29.3255008030251,-2.66599903099763,33.8305837392638));
#72814=CARTESIAN_POINT('',(29.3255008030251,-2.66599903099763,16.));
#72815=CARTESIAN_POINT('Origin',(30.,-1.32966554433622E-14,33.8305837392638));
#72816=CARTESIAN_POINT('Origin',(30.,-1.32966554433622E-14,16.));
#72817=CARTESIAN_POINT('',(29.3906449526766,-2.68163875760731,33.8305837392638));
#72818=CARTESIAN_POINT('',(29.3906449526766,-2.6816387576073,16.));
#72819=CARTESIAN_POINT('',(29.53675193213,-2.71070124278107,33.8305837392638));
#72820=CARTESIAN_POINT('',(29.53675193213,-2.71070124278106,16.));
#72821=CARTESIAN_POINT('Origin',(30.,-1.32966554433622E-14,33.8305837392638));
#72822=CARTESIAN_POINT('Origin',(30.,-1.32966554433622E-14,16.));
#72823=CARTESIAN_POINT('',(29.6029223429162,-2.72118160625948,33.8305837392638));
#72824=CARTESIAN_POINT('',(29.6029223429162,-2.72118160625948,16.));
#72825=CARTESIAN_POINT('',(29.750859139619,-2.73869108000313,33.8305837392638));
#72826=CARTESIAN_POINT('',(29.750859139619,-2.73869108000313,16.));
#72827=CARTESIAN_POINT('Origin',(30.,-1.32966554433622E-14,33.8305837392638));
#72828=CARTESIAN_POINT('Origin',(30.,-1.32966554433622E-14,16.));
#72829=CARTESIAN_POINT('',(29.8176478489534,-2.74394746542436,33.8305837392638));
#72830=CARTESIAN_POINT('',(29.8176478489534,-2.74394746542436,16.));
#72831=CARTESIAN_POINT('',(29.9665023833599,-2.74979597600977,33.8305837392638));
#72832=CARTESIAN_POINT('',(29.9665023833599,-2.74979597600977,16.));
#72833=CARTESIAN_POINT('Origin',(30.,-1.32966554433622E-14,33.8305837392638));
#72834=CARTESIAN_POINT('Origin',(30.,-1.32966554433622E-14,16.));
#72835=CARTESIAN_POINT('',(30.03349761664,-2.74979597600977,33.8305837392638));
#72836=CARTESIAN_POINT('',(30.03349761664,-2.74979597600977,16.));
#72837=CARTESIAN_POINT('',(30.1823521510466,-2.74394746542436,33.8305837392638));
#72838=CARTESIAN_POINT('',(30.1823521510466,-2.74394746542436,16.));
#72839=CARTESIAN_POINT('Origin',(30.,-1.32966554433622E-14,33.8305837392638));
#72840=CARTESIAN_POINT('Origin',(30.,-1.32966554433622E-14,16.));
#72841=CARTESIAN_POINT('',(30.249140860381,-2.73869108000313,33.8305837392638));
#72842=CARTESIAN_POINT('',(30.2491408603809,-2.73869108000313,16.));
#72843=CARTESIAN_POINT('',(30.3970776570837,-2.72118160625949,33.8305837392638));
#72844=CARTESIAN_POINT('',(30.3970776570837,-2.72118160625948,16.));
#72845=CARTESIAN_POINT('Origin',(30.,-1.32966554433622E-14,33.8305837392638));
#72846=CARTESIAN_POINT('Origin',(30.,-1.32966554433622E-14,16.));
#72847=CARTESIAN_POINT('',(30.4632480678699,-2.71070124278108,33.8305837392638));
#72848=CARTESIAN_POINT('',(30.4632480678699,-2.71070124278107,16.));
#72849=CARTESIAN_POINT('',(30.6093550473233,-2.68163875760732,33.8305837392638));
#72850=CARTESIAN_POINT('',(30.6093550473233,-2.68163875760731,16.));
#72851=CARTESIAN_POINT('Origin',(30.,-1.32966554433622E-14,33.8305837392638));
#72852=CARTESIAN_POINT('Origin',(30.,-1.32966554433622E-14,16.));
#72853=CARTESIAN_POINT('',(30.6744991969748,-2.66599903099764,33.8305837392638));
#72854=CARTESIAN_POINT('',(30.6744991969748,-2.66599903099764,16.));
#72855=CARTESIAN_POINT('',(30.817875561065,-2.62556271427912,33.8305837392638));
#72856=CARTESIAN_POINT('',(30.817875561065,-2.62556271427912,16.));
#72857=CARTESIAN_POINT('Origin',(30.,-1.32966554433622E-14,33.8305837392638));
#72858=CARTESIAN_POINT('Origin',(30.,-1.32966554433622E-14,16.));
#72859=CARTESIAN_POINT('',(30.8815918142367,-2.60486004865346,33.8305837392638));
#72860=CARTESIAN_POINT('',(30.8815918142367,-2.60486004865346,16.));
#72861=CARTESIAN_POINT('',(31.0213536000014,-2.55329920372919,33.8305837392638));
#72862=CARTESIAN_POINT('',(31.0213536000014,-2.55329920372919,16.));
#72863=CARTESIAN_POINT('Origin',(30.,-1.32966554433622E-14,33.8305837392638));
#72864=CARTESIAN_POINT('Origin',(30.,-1.32966554433622E-14,16.));
#72865=CARTESIAN_POINT('',(31.0832491248047,-2.52766123790547,33.8305837392638));
#72866=CARTESIAN_POINT('',(31.0832491248047,-2.52766123790547,16.));
#72867=CARTESIAN_POINT('',(31.2185346543594,-2.46529375453013,33.8305837392638));
#72868=CARTESIAN_POINT('',(31.2185346543594,-2.46529375453013,16.));
#72869=CARTESIAN_POINT('Origin',(30.,-1.32966554433622E-14,33.8305837392638));
#72870=CARTESIAN_POINT('Origin',(30.,-1.32966554433622E-14,16.));
#72871=CARTESIAN_POINT('',(31.2782278443015,-2.43487855509314,33.8305837392638));
#72872=CARTESIAN_POINT('',(31.2782278443015,-2.43487855509314,16.));
#72873=CARTESIAN_POINT('',(31.4082030373693,-2.36208894954103,33.8305837392638));
#72874=CARTESIAN_POINT('',(31.4082030373693,-2.36208894954102,16.));
#72875=CARTESIAN_POINT('Origin',(30.,-1.32966554433622E-14,33.8305837392638));
#72876=CARTESIAN_POINT('Origin',(30.,-1.32966554433622E-14,16.));
#72877=CARTESIAN_POINT('',(31.4653258640842,-2.32708403630938,33.8305837392638));
#72878=CARTESIAN_POINT('',(31.4653258640842,-2.32708403630938,16.));
#72879=CARTESIAN_POINT('',(31.5891893803788,-2.24432108070372,33.8305837392638));
#72880=CARTESIAN_POINT('',(31.5891893803788,-2.24432108070372,16.));
#72881=CARTESIAN_POINT('Origin',(30.,-1.32966554433622E-14,33.8305837392638));
#72882=CARTESIAN_POINT('Origin',(30.,-1.32966554433622E-14,16.));
#72883=CARTESIAN_POINT('',(31.6433896626445,-2.2049422706078,33.8305837392638));
#72884=CARTESIAN_POINT('',(31.6433896626445,-2.2049422706078,16.));
#72885=CARTESIAN_POINT('',(31.7603778423992,-2.11271622609139,33.8305837392638));
#72886=CARTESIAN_POINT('',(31.7603778423992,-2.11271622609138,16.));
#72887=CARTESIAN_POINT('Origin',(30.,-1.32966554433622E-14,33.8305837392638));
#72888=CARTESIAN_POINT('Origin',(30.,-1.32966554433622E-14,16.));
#72889=CARTESIAN_POINT('',(31.8113214174522,-2.06920630259022,33.8305837392638));
#72890=CARTESIAN_POINT('',(31.8113214174522,-2.06920630259022,16.));
#72891=CARTESIAN_POINT('',(31.9207129896362,-1.96808577339576,33.8305837392638));
#72892=CARTESIAN_POINT('',(31.9207129896362,-1.96808577339576,16.));
#72893=CARTESIAN_POINT('Origin',(30.,-1.32966554433622E-14,33.8305837392638));
#72894=CARTESIAN_POINT('Origin',(30.,-1.32966554433622E-14,16.));
#72895=CARTESIAN_POINT('',(31.9680857733957,-1.92071298963625,33.8305837392638));
#72896=CARTESIAN_POINT('',(31.9680857733957,-1.92071298963625,16.));
#72897=CARTESIAN_POINT('',(32.0692063025902,-1.81132141745222,33.8305837392638));
#72898=CARTESIAN_POINT('',(32.0692063025902,-1.81132141745222,16.));
#72899=CARTESIAN_POINT('Origin',(30.,-1.32966554433622E-14,33.8305837392638));
#72900=CARTESIAN_POINT('Origin',(30.,-1.32966554433622E-14,16.));
#72901=CARTESIAN_POINT('',(32.1127162260913,-1.76037784239929,33.8305837392638));
#72902=CARTESIAN_POINT('',(32.1127162260913,-1.76037784239929,16.));
#72903=CARTESIAN_POINT('',(32.2049422706078,-1.6433896626446,33.8305837392638));
#72904=CARTESIAN_POINT('',(32.2049422706077,-1.64338966264459,16.));
#72905=CARTESIAN_POINT('Origin',(30.,-1.32966554433622E-14,33.8305837392638));
#72906=CARTESIAN_POINT('Origin',(30.,-1.32966554433622E-14,16.));
#72907=CARTESIAN_POINT('',(32.2443210807037,-1.5891893803789,33.8305837392638));
#72908=CARTESIAN_POINT('',(32.2443210807037,-1.5891893803789,16.));
#72909=CARTESIAN_POINT('',(32.3270840363093,-1.46532586408425,33.8305837392638));
#72910=CARTESIAN_POINT('',(32.3270840363093,-1.46532586408424,16.));
#72911=CARTESIAN_POINT('Origin',(30.,-1.32966554433622E-14,33.8305837392638));
#72912=CARTESIAN_POINT('Origin',(30.,-1.32966554433622E-14,16.));
#72913=CARTESIAN_POINT('',(32.362088949541,-1.40820303736938,33.8305837392638));
#72914=CARTESIAN_POINT('',(32.362088949541,-1.40820303736938,16.));
#72915=CARTESIAN_POINT('',(32.4348785550931,-1.27822784430152,33.8305837392638));
#72916=CARTESIAN_POINT('',(32.4348785550931,-1.27822784430152,16.));
#72917=CARTESIAN_POINT('Origin',(30.,-1.32966554433622E-14,33.8305837392638));
#72918=CARTESIAN_POINT('Origin',(30.,-1.32966554433622E-14,16.));
#72919=CARTESIAN_POINT('',(32.4652937545301,-1.21853465435946,33.8305837392638));
#72920=CARTESIAN_POINT('',(32.4652937545301,-1.21853465435946,16.));
#72921=CARTESIAN_POINT('',(32.5276612379054,-1.08324912480479,33.8305837392638));
#72922=CARTESIAN_POINT('',(32.5276612379054,-1.08324912480479,16.));
#72923=CARTESIAN_POINT('Origin',(30.,-1.32966554433622E-14,33.8305837392638));
#72924=CARTESIAN_POINT('Origin',(30.,-1.32966554433622E-14,16.));
#72925=CARTESIAN_POINT('',(32.5532992037291,-1.02135360000151,33.8305837392638));
#72926=CARTESIAN_POINT('',(32.5532992037291,-1.02135360000151,16.));
#72927=CARTESIAN_POINT('',(32.6048600486534,-0.88159181423675,33.8305837392638));
#72928=CARTESIAN_POINT('',(32.6048600486534,-0.881591814236746,16.));
#72929=CARTESIAN_POINT('Origin',(30.,-1.32966554433622E-14,33.8305837392638));
#72930=CARTESIAN_POINT('Origin',(30.,-1.32966554433622E-14,16.));
#72931=CARTESIAN_POINT('',(32.6255627142791,-0.817875561065022,33.8305837392638));
#72932=CARTESIAN_POINT('',(32.6255627142791,-0.817875561065022,16.));
#72933=CARTESIAN_POINT('',(32.6659990309976,-0.674499196974912,33.8305837392638));
#72934=CARTESIAN_POINT('',(32.6659990309976,-0.674499196974908,16.));
#72935=CARTESIAN_POINT('Origin',(30.,-1.32966554433622E-14,33.8305837392638));
#72936=CARTESIAN_POINT('Origin',(30.,-1.32966554433622E-14,16.));
#72937=CARTESIAN_POINT('',(32.6816387576073,-0.609355047323342,33.8305837392638));
#72938=CARTESIAN_POINT('',(32.6816387576073,-0.609355047323343,16.));
#72939=CARTESIAN_POINT('',(32.710701242781,-0.463248067869981,33.8305837392638));
#72940=CARTESIAN_POINT('',(32.710701242781,-0.463248067869977,16.));
#72941=CARTESIAN_POINT('Origin',(30.,-1.32966554433622E-14,33.8305837392638));
#72942=CARTESIAN_POINT('Origin',(30.,-1.32966554433622E-14,16.));
#72943=CARTESIAN_POINT('',(32.7211816062594,-0.3970776570838,33.8305837392638));
#72944=CARTESIAN_POINT('',(32.7211816062594,-0.397077657083801,16.));
#72945=CARTESIAN_POINT('',(32.7386910800031,-0.249140860381016,33.8305837392638));
#72946=CARTESIAN_POINT('',(32.7386910800031,-0.249140860381013,16.));
#72947=CARTESIAN_POINT('Origin',(30.,-1.32966554433622E-14,33.8305837392638));
#72948=CARTESIAN_POINT('Origin',(30.,-1.32966554433622E-14,16.));
#72949=CARTESIAN_POINT('',(32.7439474654243,-0.182352151046616,33.8305837392638));
#72950=CARTESIAN_POINT('',(32.7439474654243,-0.182352151046618,16.));
#72951=CARTESIAN_POINT('',(32.7497959760097,-0.03349761664006,33.8305837392638));
#72952=CARTESIAN_POINT('',(32.7497959760097,-0.0334976166400576,16.));
#72953=CARTESIAN_POINT('Origin',(30.,-1.32966554433622E-14,33.8305837392638));
#72954=CARTESIAN_POINT('Origin',(30.,-1.32966554433622E-14,16.));
#72955=CARTESIAN_POINT('',(32.7497959760097,0.0334976166400146,33.8305837392638));
#72956=CARTESIAN_POINT('',(32.7497959760097,0.0334976166400122,16.));
#72957=CARTESIAN_POINT('',(32.7439474654243,0.18235215104657,33.8305837392638));
#72958=CARTESIAN_POINT('',(32.7439474654243,0.182352151046572,16.));
#72959=CARTESIAN_POINT('Origin',(30.,-1.32966554433622E-14,33.8305837392638));
#72960=CARTESIAN_POINT('Origin',(30.,-1.32966554433622E-14,16.));
#72961=CARTESIAN_POINT('',(32.7386910800031,0.249140860380971,33.8305837392638));
#72962=CARTESIAN_POINT('',(32.7386910800031,0.249140860380968,16.));
#72963=CARTESIAN_POINT('',(32.7211816062594,0.397077657083754,33.8305837392638));
#72964=CARTESIAN_POINT('',(32.7211816062594,0.397077657083756,16.));
#72965=CARTESIAN_POINT('Origin',(30.,-1.32966554433622E-14,33.8305837392638));
#72966=CARTESIAN_POINT('Origin',(30.,-1.32966554433622E-14,16.));
#72967=CARTESIAN_POINT('',(32.710701242781,0.463248067869934,33.8305837392638));
#72968=CARTESIAN_POINT('',(32.710701242781,0.463248067869931,16.));
#72969=CARTESIAN_POINT('',(32.6816387576073,0.609355047323297,33.8305837392638));
#72970=CARTESIAN_POINT('',(32.6816387576073,0.609355047323298,16.));
#72971=CARTESIAN_POINT('Origin',(30.,-1.32966554433622E-14,33.8305837392638));
#72972=CARTESIAN_POINT('Origin',(30.,-1.32966554433622E-14,16.));
#72973=CARTESIAN_POINT('',(32.6659990309976,0.674499196974867,33.8305837392638));
#72974=CARTESIAN_POINT('',(32.6659990309976,0.674499196974863,16.));
#72975=CARTESIAN_POINT('',(32.6255627142791,0.817875561064977,33.8305837392638));
#72976=CARTESIAN_POINT('',(32.6255627142791,0.817875561064977,16.));
#72977=CARTESIAN_POINT('Origin',(30.,-1.32966554433622E-14,33.8305837392638));
#72978=CARTESIAN_POINT('Origin',(30.,-1.32966554433622E-14,16.));
#72979=CARTESIAN_POINT('',(32.6048600486534,0.881591814236705,33.8305837392638));
#72980=CARTESIAN_POINT('',(32.6048600486534,0.881591814236701,16.));
#72981=CARTESIAN_POINT('',(32.5532992037292,1.02135360000147,33.8305837392638));
#72982=CARTESIAN_POINT('',(32.5532992037291,1.02135360000147,16.));
#72983=CARTESIAN_POINT('Origin',(30.,-1.32966554433622E-14,33.8305837392638));
#72984=CARTESIAN_POINT('Origin',(30.,-1.32966554433622E-14,16.));
#72985=CARTESIAN_POINT('',(32.5276612379054,1.08324912480475,33.8305837392638));
#72986=CARTESIAN_POINT('',(32.5276612379054,1.08324912480474,16.));
#72987=CARTESIAN_POINT('',(32.4652937545301,1.21853465435941,33.8305837392638));
#72988=CARTESIAN_POINT('',(32.4652937545301,1.21853465435941,16.));
#72989=CARTESIAN_POINT('Origin',(30.,-1.32966554433622E-14,33.8305837392638));
#72990=CARTESIAN_POINT('Origin',(30.,-1.32966554433622E-14,16.));
#72991=CARTESIAN_POINT('',(32.4348785550931,1.27822784430148,33.8305837392638));
#72992=CARTESIAN_POINT('',(32.4348785550931,1.27822784430148,16.));
#72993=CARTESIAN_POINT('',(32.362088949541,1.40820303736934,33.8305837392638));
#72994=CARTESIAN_POINT('',(32.362088949541,1.40820303736934,16.));
#72995=CARTESIAN_POINT('Origin',(30.,-1.32966554433622E-14,33.8305837392638));
#72996=CARTESIAN_POINT('Origin',(30.,-1.32966554433622E-14,16.));
#72997=CARTESIAN_POINT('',(32.3270840363093,1.4653258640842,33.8305837392638));
#72998=CARTESIAN_POINT('',(32.3270840363093,1.4653258640842,16.));
#72999=CARTESIAN_POINT('',(32.2443210807037,1.58918938037886,33.8305837392638));
#73000=CARTESIAN_POINT('',(32.2443210807037,1.58918938037886,16.));
#73001=CARTESIAN_POINT('Origin',(30.,-1.32966554433622E-14,33.8305837392638));
#73002=CARTESIAN_POINT('Origin',(30.,-1.32966554433622E-14,16.));
#73003=CARTESIAN_POINT('',(32.2049422706078,1.64338966264455,33.8305837392638));
#73004=CARTESIAN_POINT('',(32.2049422706078,1.64338966264455,16.));
#73005=CARTESIAN_POINT('',(32.1127162260914,1.76037784239925,33.8305837392638));
#73006=CARTESIAN_POINT('',(32.1127162260913,1.76037784239925,16.));
#73007=CARTESIAN_POINT('Origin',(30.,-1.32966554433622E-14,33.8305837392638));
#73008=CARTESIAN_POINT('Origin',(30.,-1.32966554433622E-14,16.));
#73009=CARTESIAN_POINT('',(32.0692063025902,1.81132141745218,33.8305837392638));
#73010=CARTESIAN_POINT('',(32.0692063025902,1.81132141745218,16.));
#73011=CARTESIAN_POINT('',(31.9680857733957,1.92071298963621,33.8305837392638));
#73012=CARTESIAN_POINT('',(31.9680857733957,1.92071298963621,16.));
#73013=CARTESIAN_POINT('Origin',(30.,-1.32966554433622E-14,33.8305837392638));
#73014=CARTESIAN_POINT('Origin',(30.,-1.32966554433622E-14,16.));
#73015=CARTESIAN_POINT('',(31.9207129896362,1.96808577339572,33.8305837392638));
#73016=CARTESIAN_POINT('',(31.9207129896362,1.96808577339572,16.));
#73017=CARTESIAN_POINT('',(31.8113214174522,2.06920630259018,33.8305837392638));
#73018=CARTESIAN_POINT('',(31.8113214174522,2.06920630259018,16.));
#73019=CARTESIAN_POINT('Origin',(30.,-1.32966554433622E-14,33.8305837392638));
#73020=CARTESIAN_POINT('Origin',(30.,-1.32966554433622E-14,16.));
#73021=CARTESIAN_POINT('',(31.7603778423992,2.11271622609135,33.8305837392638));
#73022=CARTESIAN_POINT('',(31.7603778423992,2.11271622609134,16.));
#73023=CARTESIAN_POINT('',(31.6433896626446,2.20494227060777,33.8305837392638));
#73024=CARTESIAN_POINT('',(31.6433896626445,2.20494227060776,16.));
#73025=CARTESIAN_POINT('Origin',(30.,-1.32966554433622E-14,33.8305837392638));
#73026=CARTESIAN_POINT('Origin',(30.,-1.32966554433622E-14,16.));
#73027=CARTESIAN_POINT('',(31.5891893803789,2.24432108070369,33.8305837392638));
#73028=CARTESIAN_POINT('',(31.5891893803789,2.24432108070368,16.));
#73029=CARTESIAN_POINT('',(31.4653258640842,2.32708403630934,33.8305837392638));
#73030=CARTESIAN_POINT('',(31.4653258640842,2.32708403630934,16.));
#73031=CARTESIAN_POINT('Origin',(30.,-1.32966554433622E-14,33.8305837392638));
#73032=CARTESIAN_POINT('Origin',(30.,-1.32966554433622E-14,16.));
#73033=CARTESIAN_POINT('',(31.4082030373693,2.36208894954099,33.8305837392638));
#73034=CARTESIAN_POINT('',(31.4082030373693,2.36208894954099,16.));
#73035=CARTESIAN_POINT('',(31.2782278443015,2.43487855509311,33.8305837392638));
#73036=CARTESIAN_POINT('',(31.2782278443015,2.4348785550931,16.));
#73037=CARTESIAN_POINT('Origin',(30.,-1.32966554433622E-14,33.8305837392638));
#73038=CARTESIAN_POINT('Origin',(30.,-1.32966554433622E-14,16.));
#73039=CARTESIAN_POINT('',(31.2185346543594,2.4652937545301,33.8305837392638));
#73040=CARTESIAN_POINT('',(31.2185346543594,2.46529375453009,16.));
#73041=CARTESIAN_POINT('',(31.0832491248047,2.52766123790544,33.8305837392638));
#73042=CARTESIAN_POINT('',(31.0832491248047,2.52766123790544,16.));
#73043=CARTESIAN_POINT('Origin',(30.,-1.32966554433622E-14,33.8305837392638));
#73044=CARTESIAN_POINT('Origin',(30.,-1.32966554433622E-14,16.));
#73045=CARTESIAN_POINT('',(31.0213536000015,2.55329920372916,33.8305837392638));
#73046=CARTESIAN_POINT('',(31.0213536000015,2.55329920372915,16.));
#73047=CARTESIAN_POINT('',(30.8815918142367,2.60486004865343,33.8305837392638));
#73048=CARTESIAN_POINT('',(30.8815918142367,2.60486004865343,16.));
#73049=CARTESIAN_POINT('Origin',(30.,-1.32966554433622E-14,33.8305837392638));
#73050=CARTESIAN_POINT('Origin',(30.,-1.32966554433622E-14,16.));
#73051=CARTESIAN_POINT('',(30.817875561065,2.62556271427909,33.8305837392638));
#73052=CARTESIAN_POINT('',(30.817875561065,2.62556271427908,16.));
#73053=CARTESIAN_POINT('',(30.6744991969749,2.66599903099761,33.8305837392638));
#73054=CARTESIAN_POINT('',(30.6744991969749,2.6659990309976,16.));
#73055=CARTESIAN_POINT('Origin',(30.,-1.32966554433622E-14,33.8305837392638));
#73056=CARTESIAN_POINT('Origin',(30.,-1.32966554433622E-14,16.));
#73057=CARTESIAN_POINT('',(30.6093550473233,2.68163875760729,33.8305837392638));
#73058=CARTESIAN_POINT('',(30.6093550473233,2.68163875760728,16.));
#73059=CARTESIAN_POINT('',(30.4632480678699,2.71070124278105,33.8305837392638));
#73060=CARTESIAN_POINT('',(30.4632480678699,2.71070124278104,16.));
#73061=CARTESIAN_POINT('Origin',(30.,-1.32966554433622E-14,33.8305837392638));
#73062=CARTESIAN_POINT('Origin',(30.,-1.32966554433622E-14,16.));
#73063=CARTESIAN_POINT('',(27.5651214449069,1.27822784430151,33.8305837392638));
#73064=CARTESIAN_POINT('',(27.5651214449069,1.27822784430151,16.));
#73065=CARTESIAN_POINT('',(27.637911050459,1.40820303736937,33.8305837392638));
#73066=CARTESIAN_POINT('Origin',(30.,-1.32966554433622E-14,33.8305837392638));
#73067=CARTESIAN_POINT('',(27.637911050459,1.40820303736937,16.));
#73068=CARTESIAN_POINT('Origin',(30.,-1.32966554433622E-14,16.));
#73069=CARTESIAN_POINT('',(27.6729159636906,1.46532586408424,33.8305837392638));
#73070=CARTESIAN_POINT('',(27.6729159636906,1.46532586408423,16.));
#73071=CARTESIAN_POINT('',(27.7556789192963,1.58918938037889,33.8305837392638));
#73072=CARTESIAN_POINT('Origin',(30.,-1.32966554433622E-14,33.8305837392638));
#73073=CARTESIAN_POINT('',(27.7556789192963,1.58918938037889,16.));
#73074=CARTESIAN_POINT('Origin',(30.,-1.32966554433622E-14,16.));
#73075=CARTESIAN_POINT('',(27.7950577293922,1.64338966264458,33.8305837392638));
#73076=CARTESIAN_POINT('',(27.7950577293922,1.64338966264458,16.));
#73077=CARTESIAN_POINT('',(27.8872837739086,1.76037784239928,33.8305837392638));
#73078=CARTESIAN_POINT('Origin',(30.,-1.32966554433622E-14,33.8305837392638));
#73079=CARTESIAN_POINT('',(27.8872837739086,1.76037784239928,16.));
#73080=CARTESIAN_POINT('Origin',(30.,-1.32966554433622E-14,16.));
#73081=CARTESIAN_POINT('',(27.9307936974098,1.81132141745221,33.8305837392638));
#73082=CARTESIAN_POINT('',(27.9307936974098,1.81132141745221,16.));
#73083=CARTESIAN_POINT('',(28.0319142266043,1.92071298963624,33.8305837392638));
#73084=CARTESIAN_POINT('Origin',(30.,-1.32966554433622E-14,33.8305837392638));
#73085=CARTESIAN_POINT('',(28.0319142266043,1.92071298963623,16.));
#73086=CARTESIAN_POINT('Origin',(30.,-1.32966554433622E-14,16.));
#73087=CARTESIAN_POINT('',(28.0792870103638,1.96808577339575,33.8305837392638));
#73088=CARTESIAN_POINT('',(28.0792870103638,1.96808577339574,16.));
#73089=CARTESIAN_POINT('',(28.1886785825478,2.06920630259021,33.8305837392638));
#73090=CARTESIAN_POINT('Origin',(30.,-1.32966554433622E-14,33.8305837392638));
#73091=CARTESIAN_POINT('',(28.1886785825478,2.0692063025902,16.));
#73092=CARTESIAN_POINT('Origin',(30.,-1.32966554433622E-14,16.));
#73093=CARTESIAN_POINT('',(28.2396221576007,2.11271622609138,33.8305837392638));
#73094=CARTESIAN_POINT('',(28.2396221576007,2.11271622609137,16.));
#73095=CARTESIAN_POINT('',(28.3566103373554,2.20494227060779,33.8305837392638));
#73096=CARTESIAN_POINT('Origin',(30.,-1.32966554433622E-14,33.8305837392638));
#73097=CARTESIAN_POINT('',(28.3566103373554,2.20494227060779,16.));
#73098=CARTESIAN_POINT('Origin',(30.,-1.32966554433622E-14,16.));
#73099=CARTESIAN_POINT('',(28.4108106196211,2.24432108070371,33.8305837392638));
#73100=CARTESIAN_POINT('',(28.4108106196211,2.2443210807037,16.));
#73101=CARTESIAN_POINT('',(28.5346741359158,2.32708403630936,33.8305837392638));
#73102=CARTESIAN_POINT('Origin',(30.,-1.32966554433622E-14,33.8305837392638));
#73103=CARTESIAN_POINT('',(28.5346741359158,2.32708403630936,16.));
#73104=CARTESIAN_POINT('Origin',(30.,-1.32966554433622E-14,16.));
#73105=CARTESIAN_POINT('',(28.5917969626306,2.36208894954101,33.8305837392638));
#73106=CARTESIAN_POINT('',(28.5917969626306,2.36208894954101,16.));
#73107=CARTESIAN_POINT('',(28.7217721556985,2.43487855509313,33.8305837392638));
#73108=CARTESIAN_POINT('Origin',(30.,-1.32966554433622E-14,33.8305837392638));
#73109=CARTESIAN_POINT('',(28.7217721556985,2.43487855509312,16.));
#73110=CARTESIAN_POINT('Origin',(30.,-1.32966554433622E-14,16.));
#73111=CARTESIAN_POINT('',(28.7814653456406,2.46529375453011,33.8305837392638));
#73112=CARTESIAN_POINT('',(28.7814653456406,2.46529375453011,16.));
#73113=CARTESIAN_POINT('',(28.9167508751952,2.52766123790546,33.8305837392638));
#73114=CARTESIAN_POINT('Origin',(30.,-1.32966554433622E-14,33.8305837392638));
#73115=CARTESIAN_POINT('',(28.9167508751953,2.52766123790545,16.));
#73116=CARTESIAN_POINT('Origin',(30.,-1.32966554433622E-14,16.));
#73117=CARTESIAN_POINT('',(28.9786463999985,2.55329920372917,33.8305837392638));
#73118=CARTESIAN_POINT('',(28.9786463999985,2.55329920372917,16.));
#73119=CARTESIAN_POINT('',(29.1184081857633,2.60486004865344,33.8305837392638));
#73120=CARTESIAN_POINT('Origin',(30.,-1.32966554433622E-14,33.8305837392638));
#73121=CARTESIAN_POINT('',(29.1184081857633,2.60486004865344,16.));
#73122=CARTESIAN_POINT('Origin',(30.,-1.32966554433622E-14,16.));
#73123=CARTESIAN_POINT('',(29.182124438935,2.6255627142791,33.8305837392638));
#73124=CARTESIAN_POINT('',(29.182124438935,2.62556271427909,16.));
#73125=CARTESIAN_POINT('',(29.3255008030251,2.66599903099762,33.8305837392638));
#73126=CARTESIAN_POINT('Origin',(30.,-1.32966554433622E-14,33.8305837392638));
#73127=CARTESIAN_POINT('',(29.3255008030251,2.66599903099761,16.));
#73128=CARTESIAN_POINT('Origin',(30.,-1.32966554433622E-14,16.));
#73129=CARTESIAN_POINT('',(29.3906449526767,2.6816387576073,33.8305837392638));
#73130=CARTESIAN_POINT('',(29.3906449526767,2.68163875760729,16.));
#73131=CARTESIAN_POINT('',(29.5367519321301,2.71070124278105,33.8305837392638));
#73132=CARTESIAN_POINT('Origin',(30.,-1.32966554433622E-14,33.8305837392638));
#73133=CARTESIAN_POINT('',(29.5367519321301,2.71070124278105,16.));
#73134=CARTESIAN_POINT('Origin',(30.,-1.32966554433622E-14,16.));
#73135=CARTESIAN_POINT('',(29.6029223429162,2.72118160625947,33.8305837392638));
#73136=CARTESIAN_POINT('',(29.6029223429162,2.72118160625946,16.));
#73137=CARTESIAN_POINT('',(29.750859139619,2.73869108000311,33.8305837392638));
#73138=CARTESIAN_POINT('Origin',(30.,-1.32966554433622E-14,33.8305837392638));
#73139=CARTESIAN_POINT('',(29.750859139619,2.7386910800031,16.));
#73140=CARTESIAN_POINT('Origin',(30.,-1.32966554433622E-14,16.));
#73141=CARTESIAN_POINT('',(29.8176478489534,2.74394746542434,33.8305837392638));
#73142=CARTESIAN_POINT('',(29.8176478489534,2.74394746542433,16.));
#73143=CARTESIAN_POINT('',(29.9665023833599,2.74979597600975,33.8305837392638));
#73144=CARTESIAN_POINT('Origin',(30.,-1.32966554433622E-14,33.8305837392638));
#73145=CARTESIAN_POINT('',(29.9665023833599,2.74979597600974,16.));
#73146=CARTESIAN_POINT('Origin',(30.,-1.32966554433622E-14,16.));
#73147=CARTESIAN_POINT('',(30.3970776570838,2.72118160625946,33.8305837392638));
#73148=CARTESIAN_POINT('',(30.3970776570838,2.72118160625945,16.));
#73149=CARTESIAN_POINT('',(30.249140860381,2.73869108000311,33.8305837392638));
#73150=CARTESIAN_POINT('',(30.249140860381,2.7386910800031,16.));
#73151=CARTESIAN_POINT('Origin',(30.,-1.32966554433622E-14,33.8305837392638));
#73152=CARTESIAN_POINT('Origin',(30.,-1.32966554433622E-14,33.8305837392638));
#73153=CARTESIAN_POINT('Origin',(27.5075580599235,1.0459901541636,33.8304779343707));
#73154=CARTESIAN_POINT('Origin',(27.5859153117241,1.21595293501799,33.830456743813));
#73155=CARTESIAN_POINT('Origin',(30.,-1.32966554433622E-14,33.8305837392638));
#73156=CARTESIAN_POINT('Origin',(27.4979545614264,1.02279765627048,33.8304567438139));
#73157=CARTESIAN_POINT('Origin',(27.4331739849704,0.847210974834779,33.830477934375));
#73158=CARTESIAN_POINT('Origin',(30.,-1.32966554433622E-14,33.8305837392638));
#73159=CARTESIAN_POINT('Origin',(27.4254197532764,0.823336489857381,33.8304567438132));
#73160=CARTESIAN_POINT('Origin',(27.3746152459633,0.643208458112014,33.8304779343751));
#73161=CARTESIAN_POINT('Origin',(30.,-1.32966554433622E-14,33.8305837392638));
#73162=CARTESIAN_POINT('Origin',(27.368758088479,0.618799180196873,33.8304567438137));
#73163=CARTESIAN_POINT('Origin',(27.3322428769935,0.435240347356666,33.8304779343754));
#73164=CARTESIAN_POINT('Origin',(30.,-1.32966554433622E-14,33.8305837392638));
#73165=CARTESIAN_POINT('Origin',(27.3283189050469,0.410446767819665,33.8304567438127));
#73166=CARTESIAN_POINT('Origin',(27.3063181178076,0.224588835126915,33.8304779343751));
#73167=CARTESIAN_POINT('Origin',(30.,-1.32966554433622E-14,33.8305837392638));
#73168=CARTESIAN_POINT('Origin',(27.3043515239852,0.199563814630461,33.8304567438133));
#73169=CARTESIAN_POINT('Origin',(27.2970008031678,0.0125526580442922,33.8304779343738));
#73170=CARTESIAN_POINT('Origin',(30.,-1.32966554433622E-14,33.8305837392638));
#73171=CARTESIAN_POINT('Origin',(27.2970037121732,-0.012549515837469,33.8304567438135));
#73172=CARTESIAN_POINT('Origin',(27.3043483774083,-0.199560910346332,33.8304779343754));
#73173=CARTESIAN_POINT('Origin',(30.,-1.32966554433622E-14,33.8305837392638));
#73174=CARTESIAN_POINT('Origin',(27.3063207713147,-0.224585474366301,33.8304567438129));
#73175=CARTESIAN_POINT('Origin',(27.3283155403039,-0.410444119366497,33.8304779343742));
#73176=CARTESIAN_POINT('Origin',(30.,-1.32966554433622E-14,33.8305837392638));
#73177=CARTESIAN_POINT('Origin',(27.3322452586388,-0.435236788764194,33.8304567438132));
#73178=CARTESIAN_POINT('Origin',(27.3687545263134,-0.618796803902706,33.8304779343752));
#73179=CARTESIAN_POINT('Origin',(30.,-1.32966554433622E-14,33.8305837392638));
#73180=CARTESIAN_POINT('Origin',(27.3746173410614,-0.643204723628853,33.8304567438136));
#73181=CARTESIAN_POINT('Origin',(27.4254160156486,-0.823334400372707,33.8304779343751));
#73182=CARTESIAN_POINT('Origin',(30.,-1.32966554433622E-14,33.8305837392638));
#73183=CARTESIAN_POINT('Origin',(27.433175780606,-0.847207087484101,33.8304567438133));
#73184=CARTESIAN_POINT('Origin',(27.4979506713824,-1.02279586647791,33.8304779343754));
#73185=CARTESIAN_POINT('Origin',(30.,-1.32966554433622E-14,33.8305837392638));
#73186=CARTESIAN_POINT('Origin',(27.5075595450189,-1.04598613791989,33.830456743813));
#73187=CARTESIAN_POINT('Origin',(27.5859112932449,-1.21595145595217,33.830477934375));
#73188=CARTESIAN_POINT('Origin',(30.,-1.32966554433622E-14,33.8305837392638));
#73189=CARTESIAN_POINT('Origin',(27.5973100336554,-1.23831633599182,33.8304567438138));
#73190=CARTESIAN_POINT('Origin',(27.6887555747498,-1.40161030035549,33.8304779343749));
#73191=CARTESIAN_POINT('Origin',(30.,-1.32966554433622E-14,33.8305837392638));
#73192=CARTESIAN_POINT('Origin',(27.7018739049122,-1.42301190206769,33.8304567438132));
#73193=CARTESIAN_POINT('Origin',(27.8058494467036,-1.57862775117429,33.8304779343746));
#73194=CARTESIAN_POINT('Origin',(30.,-1.32966554433622E-14,33.8305837392638));
#73195=CARTESIAN_POINT('Origin',(27.8206064877493,-1.59893412656796,33.8304567438128));
#73196=CARTESIAN_POINT('Origin',(27.9364709864456,-1.74591243696051,33.830477934375));
#73197=CARTESIAN_POINT('Origin',(30.,-1.32966554433622E-14,33.8305837392638));
#73198=CARTESIAN_POINT('Origin',(27.9527757563098,-1.76499839048126,33.8304567438135));
#73199=CARTESIAN_POINT('Origin',(28.0798148687495,-1.90243299199812,33.8304779343753));
#73200=CARTESIAN_POINT('Origin',(30.,-1.32966554433622E-14,33.8305837392638));
#73201=CARTESIAN_POINT('Origin',(28.0975668431045,-1.92018085239454,33.8304567438138));
#73202=CARTESIAN_POINT('Origin',(28.234997330915,-2.04722441501659,33.8304779343752));
#73203=CARTESIAN_POINT('Origin',(30.,-1.32966554433622E-14,33.8305837392638));
#73204=CARTESIAN_POINT('Origin',(28.2540870629355,-2.06352476082575,33.8304567438132));
#73205=CARTESIAN_POINT('Origin',(28.4010616214883,-2.1793940187284,33.8304779343619));
#73206=CARTESIAN_POINT('Origin',(30.,-1.32966554433622E-14,33.8305837392638));
#73207=CARTESIAN_POINT('Origin',(28.4213714165976,-2.19414635291788,33.8304567438138));
#73208=CARTESIAN_POINT('Origin',(28.5769838988107,-2.29812693362319,33.8304779343729));
#73209=CARTESIAN_POINT('Origin',(30.,-1.32966554433622E-14,33.8305837392638));
#73210=CARTESIAN_POINT('Origin',(28.5983885404242,-2.31124030311337,33.8304567438133));
#73211=CARTESIAN_POINT('Origin',(28.7616795436178,-2.40269113175742,33.8304779343754));
#73212=CARTESIAN_POINT('Origin',(30.,-1.32966554433622E-14,33.8305837392638));
#73213=CARTESIAN_POINT('Origin',(28.7840470649819,-2.41408468827727,33.8304567438135));
#73214=CARTESIAN_POINT('Origin',(28.9540098458287,-2.49244194008352,33.8304779343747));
#73215=CARTESIAN_POINT('Origin',(30.,-1.32966554433622E-14,33.8305837392638));
#73216=CARTESIAN_POINT('Origin',(28.9772023437295,-2.50204543857419,33.8304567438141));
#73217=CARTESIAN_POINT('Origin',(29.1527890251654,-2.5668260150294,33.8304779343748));
#73218=CARTESIAN_POINT('Origin',(30.,-1.32966554433622E-14,33.8305837392638));
#73219=CARTESIAN_POINT('Origin',(29.1766635101425,-2.57458024672298,33.8304567438129));
#73220=CARTESIAN_POINT('Origin',(29.3567915418921,-2.62538475403142,33.8304779343725));
#73221=CARTESIAN_POINT('Origin',(30.,-1.32966554433622E-14,33.8305837392638));
#73222=CARTESIAN_POINT('Origin',(29.3812008198029,-2.63124191151983,33.8304567438133));
#73223=CARTESIAN_POINT('Origin',(29.5647596526443,-2.66775712300496,33.8304779343746));
#73224=CARTESIAN_POINT('Origin',(30.,-1.32966554433622E-14,33.8305837392638));
#73225=CARTESIAN_POINT('Origin',(29.589553232181,-2.67168109495555,33.8304567438136));
#73226=CARTESIAN_POINT('Origin',(29.7754111648755,-2.69368188218804,33.8304779343731));
#73227=CARTESIAN_POINT('Origin',(30.,-1.32966554433622E-14,33.8305837392638));
#73228=CARTESIAN_POINT('Origin',(29.8004361853699,-2.69564847601571,33.8304567438137));
#73229=CARTESIAN_POINT('Origin',(29.9874473419542,-2.70299919683539,33.8304779343752));
#73230=CARTESIAN_POINT('Origin',(30.,-1.32966554433622E-14,33.8305837392638));
#73231=CARTESIAN_POINT('Origin',(30.0125495158367,-2.70299628782517,33.8304567438128));
#73232=CARTESIAN_POINT('Origin',(30.199560910346,-2.6956516225925,33.8304779343757));
#73233=CARTESIAN_POINT('Origin',(30.,-1.32966554433622E-14,33.8305837392638));
#73234=CARTESIAN_POINT('Origin',(30.2245854743665,-2.69367922868563,33.8304567438131));
#73235=CARTESIAN_POINT('Origin',(30.4104441193657,-2.67168445969903,33.8304779343754));
#73236=CARTESIAN_POINT('Origin',(30.,-1.32966554433622E-14,33.8305837392638));
#73237=CARTESIAN_POINT('Origin',(30.4352367887642,-2.66775474136125,33.8304567438132));
#73238=CARTESIAN_POINT('Origin',(30.6187968039027,-2.63124547368644,33.8304779343751));
#73239=CARTESIAN_POINT('Origin',(30.,-1.32966554433622E-14,33.8305837392638));
#73240=CARTESIAN_POINT('Origin',(30.6432047236274,-2.6253826589367,33.8304567438126));
#73241=CARTESIAN_POINT('Origin',(30.8233344003726,-2.57458398435223,33.8304779343755));
#73242=CARTESIAN_POINT('Origin',(30.,-1.32966554433622E-14,33.8305837392638));
#73243=CARTESIAN_POINT('Origin',(30.8472070874839,-2.5668242193938,33.8304567438132));
#73244=CARTESIAN_POINT('Origin',(31.0227958664778,-2.50204932861793,33.8304779343756));
#73245=CARTESIAN_POINT('Origin',(30.,-1.32966554433622E-14,33.8305837392638));
#73246=CARTESIAN_POINT('Origin',(31.0459861379201,-2.49244045498134,33.8304567438131));
#73247=CARTESIAN_POINT('Origin',(31.2159514559521,-2.41408870675381,33.8304779343746));
#73248=CARTESIAN_POINT('Origin',(30.,-1.32966554433622E-14,33.8305837392638));
#73249=CARTESIAN_POINT('Origin',(31.2383163359911,-2.402689966344,33.8304567438135));
#73250=CARTESIAN_POINT('Origin',(31.4016103003557,-2.3112444252517,33.8304779343755));
#73251=CARTESIAN_POINT('Origin',(30.,-1.32966554433622E-14,33.8305837392638));
#73252=CARTESIAN_POINT('Origin',(31.4230119020685,-2.29812609508837,33.8304567438136));
#73253=CARTESIAN_POINT('Origin',(31.5786277511746,-2.19415055329817,33.8304779343753));
#73254=CARTESIAN_POINT('Origin',(30.,-1.32966554433622E-14,33.8305837392638));
#73255=CARTESIAN_POINT('Origin',(31.5989341265715,-2.17939351225268,33.8304567438143));
#73256=CARTESIAN_POINT('Origin',(31.7459124369605,-2.06352901355452,33.8304779343751));
#73257=CARTESIAN_POINT('Origin',(30.,-1.32966554433622E-14,33.8305837392638));
#73258=CARTESIAN_POINT('Origin',(31.764998390482,-2.04722424369058,33.8304567438139));
#73259=CARTESIAN_POINT('Origin',(31.9024329919978,-1.92018513124985,33.8304779343751));
#73260=CARTESIAN_POINT('Origin',(30.,-1.32966554433622E-14,33.8305837392638));
#73261=CARTESIAN_POINT('Origin',(31.9201808523926,-1.90243315689474,33.8304567438131));
#73262=CARTESIAN_POINT('Origin',(32.0472244150163,-1.76500266908446,33.830477934375));
#73263=CARTESIAN_POINT('Origin',(30.,-1.32966554433622E-14,33.8305837392638));
#73264=CARTESIAN_POINT('Origin',(32.0635247608254,-1.74591293706441,33.8304567438131));
#73265=CARTESIAN_POINT('Origin',(32.1793940187282,-1.59893837851134,33.8304779343617));
#73266=CARTESIAN_POINT('Origin',(30.,-1.32966554433622E-14,33.8305837392638));
#73267=CARTESIAN_POINT('Origin',(32.1941463529172,-1.57862858340229,33.8304567438136));
#73268=CARTESIAN_POINT('Origin',(32.2981269336233,-1.42301610118952,33.830477934373));
#73269=CARTESIAN_POINT('Origin',(30.,-1.32966554433622E-14,33.8305837392638));
#73270=CARTESIAN_POINT('Origin',(32.311240303114,-1.40161145957583,33.8304567438134));
#73271=CARTESIAN_POINT('Origin',(32.4026911317571,-1.23832045638176,33.8304779343753));
#73272=CARTESIAN_POINT('Origin',(30.,-1.32966554433622E-14,33.8305837392638));
#73273=CARTESIAN_POINT('Origin',(32.4140846882749,-1.21595293501797,33.8304567438127));
#73274=CARTESIAN_POINT('Origin',(32.4924419400838,-1.04599015417152,33.8304779343749));
#73275=CARTESIAN_POINT('Origin',(30.,-1.32966554433622E-14,33.8305837392638));
#73276=CARTESIAN_POINT('Origin',(32.5020454385714,-1.02279765627054,33.8304567438132));
#73277=CARTESIAN_POINT('Origin',(32.56682601503,-0.847210974835106,33.8304779343751));
#73278=CARTESIAN_POINT('Origin',(30.,-1.32966554433622E-14,33.8305837392638));
#73279=CARTESIAN_POINT('Origin',(32.5745802467237,-0.823336489857386,33.8304567438133));
#73280=CARTESIAN_POINT('Origin',(32.6253847540299,-0.643208458106727,33.8304779343718));
#73281=CARTESIAN_POINT('Origin',(30.,-1.32966554433622E-14,33.8305837392638));
#73282=CARTESIAN_POINT('Origin',(32.6312419115182,-0.618799180197391,33.8304567438127));
#73283=CARTESIAN_POINT('Origin',(32.6677571230055,-0.435240347356057,33.830477934375));
#73284=CARTESIAN_POINT('Origin',(30.,-1.32966554433622E-14,33.8305837392638));
#73285=CARTESIAN_POINT('Origin',(32.6716810949544,-0.410446767819313,33.8304567438133));
#73286=CARTESIAN_POINT('Origin',(32.6936818821919,-0.224588835126652,33.8304779343749));
#73287=CARTESIAN_POINT('Origin',(30.,-1.32966554433622E-14,33.8305837392638));
#73288=CARTESIAN_POINT('Origin',(32.6956484760151,-0.199563814630355,33.8304567438134));
#73289=CARTESIAN_POINT('Origin',(32.7029991968333,-0.0125526580448477,33.8304779343743));
#73290=CARTESIAN_POINT('Origin',(30.,-1.32966554433622E-14,33.8305837392638));
#73291=CARTESIAN_POINT('Origin',(32.7029962878262,0.0125495158371826,33.8304567438133));
#73292=CARTESIAN_POINT('Origin',(32.6956516225903,0.19956091034681,33.8304779343749));
#73293=CARTESIAN_POINT('Origin',(30.,-1.32966554433622E-14,33.8305837392638));
#73294=CARTESIAN_POINT('Origin',(32.6936792286859,0.22458547436666,33.8304567438133));
#73295=CARTESIAN_POINT('Origin',(32.6716844596177,0.410444119388619,33.8304779343428));
#73296=CARTESIAN_POINT('Origin',(30.,-1.32966554433622E-14,33.8305837392638));
#73297=CARTESIAN_POINT('Origin',(32.6677547413622,0.435236788764869,33.8304567438136));
#73298=CARTESIAN_POINT('Origin',(32.6312454736863,0.618796803902747,33.8304779343751));
#73299=CARTESIAN_POINT('Origin',(30.,-1.32966554433622E-14,33.8305837392638));
#73300=CARTESIAN_POINT('Origin',(32.625382658939,0.643204723629168,33.8304567438138));
#73301=CARTESIAN_POINT('Origin',(32.5745839843506,0.823334400372804,33.8304779343749));
#73302=CARTESIAN_POINT('Origin',(30.,-1.32966554433622E-14,33.8305837392638));
#73303=CARTESIAN_POINT('Origin',(32.5668242193939,0.847207087484111,33.8304567438133));
#73304=CARTESIAN_POINT('Origin',(32.5020493286164,1.02279586647793,33.830477934375));
#73305=CARTESIAN_POINT('Origin',(30.,-1.32966554433622E-14,33.8305837392638));
#73306=CARTESIAN_POINT('Origin',(32.4924404549818,1.04598613792066,33.8304567438134));
#73307=CARTESIAN_POINT('Origin',(32.4140887067556,1.21595145595219,33.8304779343752));
#73308=CARTESIAN_POINT('Origin',(30.,-1.32966554433622E-14,33.8305837392638));
#73309=CARTESIAN_POINT('Origin',(32.4026899663445,1.2383163359917,33.8304567438137));
#73310=CARTESIAN_POINT('Origin',(32.3112444252326,1.40161030035344,33.830477934368));
#73311=CARTESIAN_POINT('Origin',(30.,-1.32966554433622E-14,33.8305837392638));
#73312=CARTESIAN_POINT('Origin',(32.2981260950878,1.42301190206775,33.8304567438133));
#73313=CARTESIAN_POINT('Origin',(32.1941505532983,1.57862775117468,33.8304779343753));
#73314=CARTESIAN_POINT('Origin',(30.,-1.32966554433622E-14,33.8305837392638));
#73315=CARTESIAN_POINT('Origin',(32.1793935122518,1.59893412656992,33.8304567438136));
#73316=CARTESIAN_POINT('Origin',(32.0635290135536,1.74591243696026,33.8304779343747));
#73317=CARTESIAN_POINT('Origin',(30.,-1.32966554433622E-14,33.8305837392638));
#73318=CARTESIAN_POINT('Origin',(32.04722424369,1.76499839048088,33.8304567438134));
#73319=CARTESIAN_POINT('Origin',(31.9201851312459,1.90243299199643,33.8304779343734));
#73320=CARTESIAN_POINT('Origin',(30.,-1.32966554433622E-14,33.8305837392638));
#73321=CARTESIAN_POINT('Origin',(31.9024331568948,1.92018085239292,33.8304567438132));
#73322=CARTESIAN_POINT('Origin',(31.7650026690842,2.0472244150162,33.8304779343749));
#73323=CARTESIAN_POINT('Origin',(30.,-1.32966554433622E-14,33.8305837392638));
#73324=CARTESIAN_POINT('Origin',(31.7459129370645,2.06352476082576,33.8304567438132));
#73325=CARTESIAN_POINT('Origin',(31.5989383785419,2.17939401874533,33.8304779343753));
#73326=CARTESIAN_POINT('Origin',(30.,-1.32966554433622E-14,33.8305837392638));
#73327=CARTESIAN_POINT('Origin',(31.5786285834019,2.1941463529156,33.830456743813));
#73328=CARTESIAN_POINT('Origin',(31.4230161011941,2.29812693362645,33.8304779343752));
#73329=CARTESIAN_POINT('Origin',(30.,-1.32966554433622E-14,33.8305837392638));
#73330=CARTESIAN_POINT('Origin',(31.4016114595758,2.31124030311394,33.8304567438134));
#73331=CARTESIAN_POINT('Origin',(31.2383204563814,2.40269113175683,33.8304779343751));
#73332=CARTESIAN_POINT('Origin',(30.,-1.32966554433622E-14,33.8305837392638));
#73333=CARTESIAN_POINT('Origin',(31.215952935018,2.41408468827632,33.8304567438131));
#73334=CARTESIAN_POINT('Origin',(31.0459901541714,2.49244194008366,33.8304779343748));
#73335=CARTESIAN_POINT('Origin',(30.,-1.32966554433622E-14,33.8305837392638));
#73336=CARTESIAN_POINT('Origin',(31.0227976562705,2.50204543857161,33.8304567438132));
#73337=CARTESIAN_POINT('Origin',(30.8472109748356,2.56682601503055,33.8304779343754));
#73338=CARTESIAN_POINT('Origin',(30.,-1.32966554433622E-14,33.8305837392638));
#73339=CARTESIAN_POINT('Origin',(30.8233364898573,2.574580246724,33.8304567438134));
#73340=CARTESIAN_POINT('Origin',(30.6432084580721,2.62538475398616,33.8304779343503));
#73341=CARTESIAN_POINT('Origin',(30.,-1.32966554433622E-14,33.8305837392638));
#73342=CARTESIAN_POINT('Origin',(30.6187991801972,2.63124191151918,33.8304567438131));
#73343=CARTESIAN_POINT('Origin',(30.4352403473569,2.66775712300684,33.8304779343755));
#73344=CARTESIAN_POINT('Origin',(30.,-1.32966554433622E-14,33.8305837392638));
#73345=CARTESIAN_POINT('Origin',(27.5973088682432,1.23832045638137,33.8304779343751));
#73346=CARTESIAN_POINT('Origin',(27.6887596968862,1.40161145957579,33.8304567438134));
#73347=CARTESIAN_POINT('Origin',(30.,-1.32966554433622E-14,33.8305837392638));
#73348=CARTESIAN_POINT('Origin',(27.7018730663741,1.4230161011934,33.8304779343749));
#73349=CARTESIAN_POINT('Origin',(27.8058536470835,1.57862858340213,33.8304567438133));
#73350=CARTESIAN_POINT('Origin',(30.,-1.32966554433622E-14,33.8305837392638));
#73351=CARTESIAN_POINT('Origin',(27.8206059812548,1.59893837854177,33.8304779343751));
#73352=CARTESIAN_POINT('Origin',(27.9364752391745,1.7459129370644,33.8304567438132));
#73353=CARTESIAN_POINT('Origin',(30.,-1.32966554433622E-14,33.8305837392638));
#73354=CARTESIAN_POINT('Origin',(27.952775584984,1.76500266908388,33.8304779343747));
#73355=CARTESIAN_POINT('Origin',(28.0798191476065,1.90243315689505,33.8304567438134));
#73356=CARTESIAN_POINT('Origin',(30.,-1.32966554433622E-14,33.8305837392638));
#73357=CARTESIAN_POINT('Origin',(28.0975670080041,1.92018513124447,33.8304779343728));
#73358=CARTESIAN_POINT('Origin',(28.23500160952,2.04722424368963,33.830456743813));
#73359=CARTESIAN_POINT('Origin',(30.,-1.32966554433622E-14,33.8305837392638));
#73360=CARTESIAN_POINT('Origin',(28.2540875630398,2.06352901355343,33.8304779343746));
#73361=CARTESIAN_POINT('Origin',(28.4010658734306,2.17939351225149,33.8304567438134));
#73362=CARTESIAN_POINT('Origin',(30.,-1.32966554433622E-14,33.8305837392638));
#73363=CARTESIAN_POINT('Origin',(28.4213722488255,2.19415055329726,33.8304779343749));
#73364=CARTESIAN_POINT('Origin',(28.5769880979325,2.29812609508769,33.8304567438131));
#73365=CARTESIAN_POINT('Origin',(30.,-1.32966554433622E-14,33.8305837392638));
#73366=CARTESIAN_POINT('Origin',(28.5983896996467,2.31124442523142,33.8304779343677));
#73367=CARTESIAN_POINT('Origin',(28.7616836640084,2.40268996634441,33.8304567438137));
#73368=CARTESIAN_POINT('Origin',(30.,-1.32966554433622E-14,33.8305837392638));
#73369=CARTESIAN_POINT('Origin',(28.7840485440478,2.41408870675589,33.8304779343753));
#73370=CARTESIAN_POINT('Origin',(28.9540138620795,2.49244045498167,33.8304567438133));
#73371=CARTESIAN_POINT('Origin',(30.,-1.32966554433622E-14,33.8305837392638));
#73372=CARTESIAN_POINT('Origin',(28.9772041335221,2.50204932861683,33.8304779343752));
#73373=CARTESIAN_POINT('Origin',(29.1527929125161,2.56682421939371,33.8304567438132));
#73374=CARTESIAN_POINT('Origin',(30.,-1.32966554433622E-14,33.8305837392638));
#73375=CARTESIAN_POINT('Origin',(29.1766655996273,2.57458398435145,33.8304779343752));
#73376=CARTESIAN_POINT('Origin',(29.3567952763716,2.62538265893797,33.8304567438133));
#73377=CARTESIAN_POINT('Origin',(30.,-1.32966554433622E-14,33.8305837392638));
#73378=CARTESIAN_POINT('Origin',(29.3812031960975,2.63124547368767,33.8304779343756));
#73379=CARTESIAN_POINT('Origin',(29.5647632112354,2.66775474136179,33.8304567438135));
#73380=CARTESIAN_POINT('Origin',(30.,-1.32966554433622E-14,33.8305837392638));
#73381=CARTESIAN_POINT('Origin',(29.5895558806117,2.67168445961877,33.8304779343432));
#73382=CARTESIAN_POINT('Origin',(29.775414525633,2.69367922868643,33.8304567438135));
#73383=CARTESIAN_POINT('Origin',(30.,-1.32966554433622E-14,33.8305837392638));
#73384=CARTESIAN_POINT('Origin',(29.8004390896529,2.69565162258947,33.8304779343745));
#73385=CARTESIAN_POINT('Origin',(29.9874504841622,2.70299628782743,33.8304567438137));
#73386=CARTESIAN_POINT('Origin',(30.,-1.32966554433622E-14,33.8305837392638));
#73387=CARTESIAN_POINT('Origin',(30.4104467678198,2.67168109495229,33.8304567438124));
#73388=CARTESIAN_POINT('Origin',(30.2245888351268,2.69368188219228,33.830477934375));
#73389=CARTESIAN_POINT('Origin',(30.,1.17524047358083,16.));
#73390=CARTESIAN_POINT('Origin',(30.,2.60624999999999,31.));
#73391=CARTESIAN_POINT('Origin',(30.,-1.32966554433622E-14,31.6569162607362));
#73392=CARTESIAN_POINT('',(30.1823521510466,2.74394746542433,31.6569162607362));
#73393=CARTESIAN_POINT('Origin',(30.1995609103462,2.69565162259179,31.6570220656244));
#73394=CARTESIAN_POINT('',(30.03349761664,2.74979597600974,31.6569162607362));
#73395=CARTESIAN_POINT('Origin',(30.0125495158372,2.70299628782596,31.6570432561867));
#73396=CARTESIAN_POINT('Origin',(30.,-1.32966554433622E-14,31.6569162607362));
#73397=CARTESIAN_POINT('Origin',(30.,-1.32966554433622E-14,16.));
#73398=CARTESIAN_POINT('',(30.1823521510466,2.74394746542434,33.8305837392638));
#73399=CARTESIAN_POINT('',(30.1823521510466,2.74394746542433,16.));
#73400=CARTESIAN_POINT('',(30.03349761664,2.74979597600975,33.8305837392638));
#73401=CARTESIAN_POINT('',(30.03349761664,2.74979597600974,16.));
#73402=CARTESIAN_POINT('Origin',(30.,-1.32966554433622E-14,33.8305837392638));
#73403=CARTESIAN_POINT('Origin',(30.,-1.32966554433622E-14,33.8305837392638));
#73404=CARTESIAN_POINT('Origin',(30.1995638146302,2.69564847601544,33.8304567438135));
#73405=CARTESIAN_POINT('Origin',(30.0125526580447,2.70299919683307,33.8304779343742));
#73406=CARTESIAN_POINT('Origin',(30.,-1.32966554433622E-14,34.));
#73407=CARTESIAN_POINT('Origin',(30.,-1.32966554433622E-14,32.5));
#73408=CARTESIAN_POINT('',(30.,-1.44337567297407,32.5));
#73409=CARTESIAN_POINT('',(31.25,-0.72168783648704,32.5));
#73410=CARTESIAN_POINT('',(30.,-1.44337567297407,32.5));
#73411=CARTESIAN_POINT('',(31.25,0.721687836487017,32.5));
#73412=CARTESIAN_POINT('',(31.25,-0.72168783648704,32.5));
#73413=CARTESIAN_POINT('',(30.,1.44337567297405,32.5));
#73414=CARTESIAN_POINT('',(31.25,0.721687836487017,32.5));
#73415=CARTESIAN_POINT('',(28.75,0.721687836487017,32.5));
#73416=CARTESIAN_POINT('',(30.,1.44337567297405,32.5));
#73417=CARTESIAN_POINT('',(28.75,-0.721687836487044,32.5));
#73418=CARTESIAN_POINT('',(28.75,0.721687836487017,32.5));
#73419=CARTESIAN_POINT('',(28.75,-0.721687836487044,32.5));
#73420=CARTESIAN_POINT('Origin',(31.25,-0.72168783648704,32.5));
#73421=CARTESIAN_POINT('',(31.25,-0.72168783648704,32.5));
#73422=CARTESIAN_POINT('',(31.25,0.721687836487017,32.5));
#73423=CARTESIAN_POINT('Origin',(31.25,0.721687836487017,32.5));
#73424=CARTESIAN_POINT('',(30.,1.44337567297405,32.5));
#73425=CARTESIAN_POINT('Origin',(30.,1.44337567297405,32.5));
#73426=CARTESIAN_POINT('',(28.75,0.721687836487017,32.5));
#73427=CARTESIAN_POINT('Origin',(28.75,0.721687836487017,32.5));
#73428=CARTESIAN_POINT('',(28.75,-0.721687836487044,32.5));
#73429=CARTESIAN_POINT('Origin',(28.75,-0.721687836487044,32.5));
#73430=CARTESIAN_POINT('',(30.,-1.44337567297407,32.5));
#73431=CARTESIAN_POINT('Origin',(30.,-1.44337567297407,32.5));
#73432=CARTESIAN_POINT('Ctrl Pts',(30.,1.17523237272422,15.7500046770317));
#73433=CARTESIAN_POINT('Ctrl Pts',(29.3214792732473,1.17523237272422,15.7916713436984));
#73434=CARTESIAN_POINT('Ctrl Pts',(28.9822189098709,0.587616186362105,15.8333380103651));
#73435=CARTESIAN_POINT('Ctrl Pts',(28.6429585464946,-1.32141491426617E-14,
15.8750046770317));
#73436=CARTESIAN_POINT('Ctrl Pts',(28.9822189098709,-0.587616186362132,
15.9166713436984));
#73437=CARTESIAN_POINT('Ctrl Pts',(29.3214792732473,-1.17523237272425,15.9583380103651));
#73438=CARTESIAN_POINT('Ctrl Pts',(30.,-1.17523237272425,16.0000046770317));
#73439=CARTESIAN_POINT('Ctrl Pts',(30.6785207267527,-1.17523237272425,16.0416713436984));
#73440=CARTESIAN_POINT('Ctrl Pts',(31.017781090129,-0.587616186362132,16.0833380103651));
#73441=CARTESIAN_POINT('Ctrl Pts',(31.3570414535054,-1.35453513912972E-14,
16.1250046770317));
#73442=CARTESIAN_POINT('Ctrl Pts',(31.017781090129,0.587616186362104,16.1666713436984));
#73443=CARTESIAN_POINT('Ctrl Pts',(30.6785207267527,1.17523237272422,16.2083380103651));
#73444=CARTESIAN_POINT('Ctrl Pts',(30.,1.17523237272422,16.2500046770317));
#73445=CARTESIAN_POINT('Ctrl Pts',(29.3214792732473,1.17523237272422,16.2916713436984));
#73446=CARTESIAN_POINT('Ctrl Pts',(28.9822189098709,0.587616186362105,16.3333380103651));
#73447=CARTESIAN_POINT('Ctrl Pts',(28.6429585464946,-1.32141491426617E-14,
16.3750046770317));
#73448=CARTESIAN_POINT('Ctrl Pts',(28.9822189098709,-0.587616186362132,
16.4166713436984));
#73449=CARTESIAN_POINT('Ctrl Pts',(29.3214792732473,-1.17523237272425,16.4583380103651));
#73450=CARTESIAN_POINT('Ctrl Pts',(30.,-1.17523237272425,16.5000046770317));
#73451=CARTESIAN_POINT('Ctrl Pts',(30.6785207267527,-1.17523237272425,16.5416713436984));
#73452=CARTESIAN_POINT('Ctrl Pts',(31.017781090129,-0.587616186362132,16.5833380103651));
#73453=CARTESIAN_POINT('Ctrl Pts',(31.3570414535054,-1.35453513912972E-14,
16.6250046770317));
#73454=CARTESIAN_POINT('Ctrl Pts',(31.017781090129,0.587616186362104,16.6666713436984));
#73455=CARTESIAN_POINT('Ctrl Pts',(30.6785207267527,1.17523237272422,16.7083380103651));
#73456=CARTESIAN_POINT('Ctrl Pts',(30.,1.17523237272422,16.7500046770317));
#73457=CARTESIAN_POINT('Ctrl Pts',(29.3214792732473,1.17523237272422,16.7916713436984));
#73458=CARTESIAN_POINT('Ctrl Pts',(28.9822189098709,0.587616186362105,16.8333380103651));
#73459=CARTESIAN_POINT('Ctrl Pts',(28.6429585464946,-1.32141491426617E-14,
16.8750046770317));
#73460=CARTESIAN_POINT('Ctrl Pts',(28.9822189098709,-0.587616186362132,
16.9166713436984));
#73461=CARTESIAN_POINT('Ctrl Pts',(29.3214792732473,-1.17523237272425,16.9583380103651));
#73462=CARTESIAN_POINT('Ctrl Pts',(30.,-1.17523237272425,17.0000046770317));
#73463=CARTESIAN_POINT('Ctrl Pts',(30.6785207267527,-1.17523237272425,17.0416713436984));
#73464=CARTESIAN_POINT('Ctrl Pts',(31.017781090129,-0.587616186362132,17.0833380103651));
#73465=CARTESIAN_POINT('Ctrl Pts',(31.3570414535054,-1.35453513912972E-14,
17.1250046770317));
#73466=CARTESIAN_POINT('Ctrl Pts',(31.017781090129,0.587616186362104,17.1666713436984));
#73467=CARTESIAN_POINT('Ctrl Pts',(30.6785207267527,1.17523237272422,17.2083380103651));
#73468=CARTESIAN_POINT('Ctrl Pts',(30.,1.17523237272422,17.2500046770317));
#73469=CARTESIAN_POINT('Ctrl Pts',(29.3214792732473,1.17523237272422,17.2916713436984));
#73470=CARTESIAN_POINT('Ctrl Pts',(28.9822189098709,0.587616186362105,17.3333380103651));
#73471=CARTESIAN_POINT('Ctrl Pts',(28.6429585464946,-1.32141491426617E-14,
17.3750046770317));
#73472=CARTESIAN_POINT('Ctrl Pts',(28.9822189098709,-0.587616186362132,
17.4166713436984));
#73473=CARTESIAN_POINT('Ctrl Pts',(29.3214792732473,-1.17523237272425,17.4583380103651));
#73474=CARTESIAN_POINT('Ctrl Pts',(30.,-1.17523237272425,17.5000046770317));
#73475=CARTESIAN_POINT('Ctrl Pts',(30.6785207267527,-1.17523237272425,17.5416713436984));
#73476=CARTESIAN_POINT('Ctrl Pts',(31.017781090129,-0.587616186362132,17.5833380103651));
#73477=CARTESIAN_POINT('Ctrl Pts',(31.3570414535054,-1.35453513912972E-14,
17.6250046770317));
#73478=CARTESIAN_POINT('Ctrl Pts',(31.017781090129,0.587616186362104,17.6666713436984));
#73479=CARTESIAN_POINT('Ctrl Pts',(30.6785207267527,1.17523237272422,17.7083380103651));
#73480=CARTESIAN_POINT('Ctrl Pts',(30.,1.17523237272422,17.7500046770317));
#73481=CARTESIAN_POINT('Ctrl Pts',(29.3214792732473,1.17523237272422,17.7916713436984));
#73482=CARTESIAN_POINT('Ctrl Pts',(28.9822189098709,0.587616186362105,17.8333380103651));
#73483=CARTESIAN_POINT('Ctrl Pts',(28.6429585464946,-1.32141491426617E-14,
17.8750046770317));
#73484=CARTESIAN_POINT('Ctrl Pts',(28.9822189098709,-0.587616186362132,
17.9166713436984));
#73485=CARTESIAN_POINT('Ctrl Pts',(29.3214792732473,-1.17523237272425,17.9583380103651));
#73486=CARTESIAN_POINT('Ctrl Pts',(30.,-1.17523237272425,18.0000046770317));
#73487=CARTESIAN_POINT('Ctrl Pts',(30.6785207267527,-1.17523237272425,18.0416713436984));
#73488=CARTESIAN_POINT('Ctrl Pts',(31.017781090129,-0.587616186362132,18.0833380103651));
#73489=CARTESIAN_POINT('Ctrl Pts',(31.3570414535054,-1.35453513912972E-14,
18.1250046770317));
#73490=CARTESIAN_POINT('Ctrl Pts',(31.017781090129,0.587616186362104,18.1666713436984));
#73491=CARTESIAN_POINT('Ctrl Pts',(30.6785207267527,1.17523237272422,18.2083380103651));
#73492=CARTESIAN_POINT('Ctrl Pts',(30.,1.17523237272422,18.2500046770317));
#73493=CARTESIAN_POINT('Ctrl Pts',(29.3214792732473,1.17523237272422,18.2916713436984));
#73494=CARTESIAN_POINT('Ctrl Pts',(28.9822189098709,0.587616186362105,18.3333380103651));
#73495=CARTESIAN_POINT('Ctrl Pts',(28.6429585464946,-1.32141491426617E-14,
18.3750046770317));
#73496=CARTESIAN_POINT('Ctrl Pts',(28.9822189098709,-0.587616186362132,
18.4166713436984));
#73497=CARTESIAN_POINT('Ctrl Pts',(29.3214792732473,-1.17523237272425,18.4583380103651));
#73498=CARTESIAN_POINT('Ctrl Pts',(30.,-1.17523237272425,18.5000046770317));
#73499=CARTESIAN_POINT('Ctrl Pts',(30.6785207267527,-1.17523237272425,18.5416713436984));
#73500=CARTESIAN_POINT('Ctrl Pts',(31.017781090129,-0.587616186362132,18.5833380103651));
#73501=CARTESIAN_POINT('Ctrl Pts',(31.3570414535054,-1.35453513912972E-14,
18.6250046770317));
#73502=CARTESIAN_POINT('Ctrl Pts',(31.017781090129,0.587616186362104,18.6666713436984));
#73503=CARTESIAN_POINT('Ctrl Pts',(30.6785207267527,1.17523237272422,18.7083380103651));
#73504=CARTESIAN_POINT('Ctrl Pts',(30.,1.17523237272422,18.7500046770317));
#73505=CARTESIAN_POINT('Ctrl Pts',(29.3214792732473,1.17523237272422,18.7916713436984));
#73506=CARTESIAN_POINT('Ctrl Pts',(28.9822189098709,0.587616186362105,18.8333380103651));
#73507=CARTESIAN_POINT('Ctrl Pts',(28.6429585464946,-1.32141491426617E-14,
18.8750046770317));
#73508=CARTESIAN_POINT('Ctrl Pts',(28.9822189098709,-0.587616186362132,
18.9166713436984));
#73509=CARTESIAN_POINT('Ctrl Pts',(29.3214792732473,-1.17523237272425,18.9583380103651));
#73510=CARTESIAN_POINT('Ctrl Pts',(30.,-1.17523237272425,19.0000046770317));
#73511=CARTESIAN_POINT('Ctrl Pts',(30.6785207267527,-1.17523237272425,19.0416713436984));
#73512=CARTESIAN_POINT('Ctrl Pts',(31.017781090129,-0.587616186362132,19.0833380103651));
#73513=CARTESIAN_POINT('Ctrl Pts',(31.3570414535054,-1.35453513912972E-14,
19.1250046770317));
#73514=CARTESIAN_POINT('Ctrl Pts',(31.017781090129,0.587616186362104,19.1666713436984));
#73515=CARTESIAN_POINT('Ctrl Pts',(30.6785207267527,1.17523237272422,19.2083380103651));
#73516=CARTESIAN_POINT('Ctrl Pts',(30.,1.17523237272422,19.2500046770317));
#73517=CARTESIAN_POINT('Ctrl Pts',(29.3214792732473,1.17523237272422,19.2916713436984));
#73518=CARTESIAN_POINT('Ctrl Pts',(28.9822189098709,0.587616186362105,19.3333380103651));
#73519=CARTESIAN_POINT('Ctrl Pts',(28.6429585464946,-1.32141491426617E-14,
19.3750046770317));
#73520=CARTESIAN_POINT('Ctrl Pts',(28.9822189098709,-0.587616186362132,
19.4166713436984));
#73521=CARTESIAN_POINT('Ctrl Pts',(29.3214792732473,-1.17523237272425,19.4583380103651));
#73522=CARTESIAN_POINT('Ctrl Pts',(30.,-1.17523237272425,19.5000046770317));
#73523=CARTESIAN_POINT('Ctrl Pts',(30.6785207267527,-1.17523237272425,19.5416713436984));
#73524=CARTESIAN_POINT('Ctrl Pts',(31.017781090129,-0.587616186362132,19.5833380103651));
#73525=CARTESIAN_POINT('Ctrl Pts',(31.3570414535054,-1.35453513912972E-14,
19.6250046770317));
#73526=CARTESIAN_POINT('Ctrl Pts',(31.017781090129,0.587616186362104,19.6666713436984));
#73527=CARTESIAN_POINT('Ctrl Pts',(30.6785207267527,1.17523237272422,19.7083380103651));
#73528=CARTESIAN_POINT('Ctrl Pts',(30.,1.17523237272422,19.7500046770317));
#73529=CARTESIAN_POINT('Ctrl Pts',(29.3214792732473,1.17523237272422,19.7916713436984));
#73530=CARTESIAN_POINT('Ctrl Pts',(28.9822189098709,0.587616186362105,19.8333380103651));
#73531=CARTESIAN_POINT('Ctrl Pts',(28.6429585464946,-1.32141491426617E-14,
19.8750046770317));
#73532=CARTESIAN_POINT('Ctrl Pts',(28.9822189098709,-0.587616186362132,
19.9166713436984));
#73533=CARTESIAN_POINT('Ctrl Pts',(29.3214792732473,-1.17523237272425,19.9583380103651));
#73534=CARTESIAN_POINT('Ctrl Pts',(30.,-1.17523237272425,20.0000046770317));
#73535=CARTESIAN_POINT('Ctrl Pts',(30.6785207267527,-1.17523237272425,20.0416713436984));
#73536=CARTESIAN_POINT('Ctrl Pts',(31.017781090129,-0.587616186362132,20.0833380103651));
#73537=CARTESIAN_POINT('Ctrl Pts',(31.3570414535054,-1.35453513912972E-14,
20.1250046770317));
#73538=CARTESIAN_POINT('Ctrl Pts',(31.017781090129,0.587616186362104,20.1666713436984));
#73539=CARTESIAN_POINT('Ctrl Pts',(30.6785207267527,1.17523237272422,20.2083380103651));
#73540=CARTESIAN_POINT('Ctrl Pts',(30.,1.17523237272422,20.2500046770317));
#73541=CARTESIAN_POINT('Ctrl Pts',(29.3214792732473,1.17523237272422,20.2916713436984));
#73542=CARTESIAN_POINT('Ctrl Pts',(28.9822189098709,0.587616186362105,20.3333380103651));
#73543=CARTESIAN_POINT('Ctrl Pts',(28.6429585464946,-1.32141491426617E-14,
20.3750046770317));
#73544=CARTESIAN_POINT('Ctrl Pts',(28.9822189098709,-0.587616186362132,
20.4166713436984));
#73545=CARTESIAN_POINT('Ctrl Pts',(29.3214792732473,-1.17523237272425,20.4583380103651));
#73546=CARTESIAN_POINT('Ctrl Pts',(30.,-1.17523237272425,20.5000046770317));
#73547=CARTESIAN_POINT('Ctrl Pts',(30.6785207267527,-1.17523237272425,20.5416713436984));
#73548=CARTESIAN_POINT('Ctrl Pts',(31.017781090129,-0.587616186362132,20.5833380103651));
#73549=CARTESIAN_POINT('Ctrl Pts',(31.3570414535054,-1.35453513912972E-14,
20.6250046770317));
#73550=CARTESIAN_POINT('Ctrl Pts',(31.017781090129,0.587616186362104,20.6666713436984));
#73551=CARTESIAN_POINT('Ctrl Pts',(30.6785207267527,1.17523237272422,20.7083380103651));
#73552=CARTESIAN_POINT('Ctrl Pts',(30.,1.17523237272422,20.7500046770317));
#73553=CARTESIAN_POINT('Ctrl Pts',(29.3214792732473,1.17523237272422,20.7916713436984));
#73554=CARTESIAN_POINT('Ctrl Pts',(28.9822189098709,0.587616186362105,20.8333380103651));
#73555=CARTESIAN_POINT('Ctrl Pts',(28.6429585464946,-1.32141491426617E-14,
20.8750046770317));
#73556=CARTESIAN_POINT('Ctrl Pts',(28.9822189098709,-0.587616186362132,
20.9166713436984));
#73557=CARTESIAN_POINT('Ctrl Pts',(29.3214792732473,-1.17523237272425,20.9583380103651));
#73558=CARTESIAN_POINT('Ctrl Pts',(30.,-1.17523237272425,21.0000046770317));
#73559=CARTESIAN_POINT('Ctrl Pts',(30.6785207267527,-1.17523237272425,21.0416713436984));
#73560=CARTESIAN_POINT('Ctrl Pts',(31.017781090129,-0.587616186362132,21.0833380103651));
#73561=CARTESIAN_POINT('Ctrl Pts',(31.3570414535054,-1.35453513912972E-14,
21.1250046770317));
#73562=CARTESIAN_POINT('Ctrl Pts',(31.017781090129,0.587616186362104,21.1666713436984));
#73563=CARTESIAN_POINT('Ctrl Pts',(30.6785207267527,1.17523237272422,21.2083380103651));
#73564=CARTESIAN_POINT('Ctrl Pts',(30.,1.17523237272422,21.2500046770317));
#73565=CARTESIAN_POINT('Ctrl Pts',(29.3214792732473,1.17523237272422,21.2916713436984));
#73566=CARTESIAN_POINT('Ctrl Pts',(28.9822189098709,0.587616186362105,21.3333380103651));
#73567=CARTESIAN_POINT('Ctrl Pts',(28.6429585464946,-1.32141491426617E-14,
21.3750046770317));
#73568=CARTESIAN_POINT('Ctrl Pts',(28.9822189098709,-0.587616186362132,
21.4166713436984));
#73569=CARTESIAN_POINT('Ctrl Pts',(29.3214792732473,-1.17523237272425,21.4583380103651));
#73570=CARTESIAN_POINT('Ctrl Pts',(30.,-1.17523237272425,21.5000046770317));
#73571=CARTESIAN_POINT('Ctrl Pts',(30.6785207267527,-1.17523237272425,21.5416713436984));
#73572=CARTESIAN_POINT('Ctrl Pts',(31.017781090129,-0.587616186362132,21.5833380103651));
#73573=CARTESIAN_POINT('Ctrl Pts',(31.3570414535054,-1.35453513912972E-14,
21.6250046770317));
#73574=CARTESIAN_POINT('Ctrl Pts',(31.017781090129,0.587616186362104,21.6666713436984));
#73575=CARTESIAN_POINT('Ctrl Pts',(30.6785207267527,1.17523237272422,21.7083380103651));
#73576=CARTESIAN_POINT('Ctrl Pts',(30.,1.17523237272422,21.7500046770317));
#73577=CARTESIAN_POINT('Ctrl Pts',(29.3214792732473,1.17523237272422,21.7916713436984));
#73578=CARTESIAN_POINT('Ctrl Pts',(28.9822189098709,0.587616186362105,21.8333380103651));
#73579=CARTESIAN_POINT('Ctrl Pts',(28.6429585464946,-1.32141491426617E-14,
21.8750046770317));
#73580=CARTESIAN_POINT('Ctrl Pts',(28.9822189098709,-0.587616186362132,
21.9166713436984));
#73581=CARTESIAN_POINT('Ctrl Pts',(29.3214792732473,-1.17523237272425,21.9583380103651));
#73582=CARTESIAN_POINT('Ctrl Pts',(30.,-1.17523237272425,22.0000046770317));
#73583=CARTESIAN_POINT('Ctrl Pts',(30.6785207267527,-1.17523237272425,22.0416713436984));
#73584=CARTESIAN_POINT('Ctrl Pts',(31.017781090129,-0.587616186362132,22.0833380103651));
#73585=CARTESIAN_POINT('Ctrl Pts',(31.3570414535054,-1.35453513912972E-14,
22.1250046770317));
#73586=CARTESIAN_POINT('Ctrl Pts',(31.017781090129,0.587616186362104,22.1666713436984));
#73587=CARTESIAN_POINT('Ctrl Pts',(30.6785207267527,1.17523237272422,22.2083380103651));
#73588=CARTESIAN_POINT('Ctrl Pts',(30.,1.17523237272422,22.2500046770317));
#73589=CARTESIAN_POINT('Ctrl Pts',(29.3214792732473,1.17523237272422,22.2916713436984));
#73590=CARTESIAN_POINT('Ctrl Pts',(28.9822189098709,0.587616186362105,22.3333380103651));
#73591=CARTESIAN_POINT('Ctrl Pts',(28.6429585464946,-1.32141491426617E-14,
22.3750046770317));
#73592=CARTESIAN_POINT('Ctrl Pts',(28.9822189098709,-0.587616186362132,
22.4166713436984));
#73593=CARTESIAN_POINT('Ctrl Pts',(29.3214792732473,-1.17523237272425,22.4583380103651));
#73594=CARTESIAN_POINT('Ctrl Pts',(30.,-1.17523237272425,22.5000046770317));
#73595=CARTESIAN_POINT('Ctrl Pts',(30.6785207267527,-1.17523237272425,22.5416713436984));
#73596=CARTESIAN_POINT('Ctrl Pts',(31.017781090129,-0.587616186362132,22.5833380103651));
#73597=CARTESIAN_POINT('Ctrl Pts',(31.3570414535054,-1.35453513912972E-14,
22.6250046770317));
#73598=CARTESIAN_POINT('Ctrl Pts',(31.017781090129,0.587616186362104,22.6666713436984));
#73599=CARTESIAN_POINT('Ctrl Pts',(30.6785207267527,1.17523237272422,22.7083380103651));
#73600=CARTESIAN_POINT('Ctrl Pts',(30.,1.17523237272422,22.7500046770317));
#73601=CARTESIAN_POINT('Ctrl Pts',(29.3214792732473,1.17523237272422,22.7916713436984));
#73602=CARTESIAN_POINT('Ctrl Pts',(28.9822189098709,0.587616186362105,22.8333380103651));
#73603=CARTESIAN_POINT('Ctrl Pts',(28.6429585464946,-1.32141491426617E-14,
22.8750046770317));
#73604=CARTESIAN_POINT('Ctrl Pts',(28.9822189098709,-0.587616186362132,
22.9166713436984));
#73605=CARTESIAN_POINT('Ctrl Pts',(29.3214792732473,-1.17523237272425,22.9583380103651));
#73606=CARTESIAN_POINT('Ctrl Pts',(30.,-1.17523237272425,23.0000046770317));
#73607=CARTESIAN_POINT('Ctrl Pts',(30.6785207267527,-1.17523237272425,23.0416713436984));
#73608=CARTESIAN_POINT('Ctrl Pts',(31.017781090129,-0.587616186362132,23.0833380103651));
#73609=CARTESIAN_POINT('Ctrl Pts',(31.3570414535054,-1.35453513912972E-14,
23.1250046770317));
#73610=CARTESIAN_POINT('Ctrl Pts',(31.017781090129,0.587616186362104,23.1666713436984));
#73611=CARTESIAN_POINT('Ctrl Pts',(30.6785207267527,1.17523237272422,23.2083380103651));
#73612=CARTESIAN_POINT('Ctrl Pts',(30.,1.17523237272422,23.2500046770317));
#73613=CARTESIAN_POINT('Ctrl Pts',(29.3214792732473,1.17523237272422,23.2916713436984));
#73614=CARTESIAN_POINT('Ctrl Pts',(28.9822189098709,0.587616186362105,23.3333380103651));
#73615=CARTESIAN_POINT('Ctrl Pts',(28.6429585464946,-1.32141491426617E-14,
23.3750046770317));
#73616=CARTESIAN_POINT('Ctrl Pts',(28.9822189098709,-0.587616186362132,
23.4166713436984));
#73617=CARTESIAN_POINT('Ctrl Pts',(29.3214792732473,-1.17523237272425,23.4583380103651));
#73618=CARTESIAN_POINT('Ctrl Pts',(30.,-1.17523237272425,23.5000046770317));
#73619=CARTESIAN_POINT('Ctrl Pts',(30.6785207267527,-1.17523237272425,23.5416713436984));
#73620=CARTESIAN_POINT('Ctrl Pts',(31.017781090129,-0.587616186362132,23.5833380103651));
#73621=CARTESIAN_POINT('Ctrl Pts',(31.3570414535054,-1.35453513912972E-14,
23.6250046770317));
#73622=CARTESIAN_POINT('Ctrl Pts',(31.017781090129,0.587616186362104,23.6666713436984));
#73623=CARTESIAN_POINT('Ctrl Pts',(30.6785207267527,1.17523237272422,23.7083380103651));
#73624=CARTESIAN_POINT('Ctrl Pts',(30.,1.17523237272422,23.7500046770317));
#73625=CARTESIAN_POINT('Ctrl Pts',(29.3214792732473,1.17523237272422,23.7916713436984));
#73626=CARTESIAN_POINT('Ctrl Pts',(28.9822189098709,0.587616186362105,23.8333380103651));
#73627=CARTESIAN_POINT('Ctrl Pts',(28.6429585464946,-1.32141491426617E-14,
23.8750046770317));
#73628=CARTESIAN_POINT('Ctrl Pts',(28.9822189098709,-0.587616186362132,
23.9166713436984));
#73629=CARTESIAN_POINT('Ctrl Pts',(29.3214792732473,-1.17523237272425,23.9583380103651));
#73630=CARTESIAN_POINT('Ctrl Pts',(30.,-1.17523237272425,24.0000046770317));
#73631=CARTESIAN_POINT('Ctrl Pts',(30.6785207267527,-1.17523237272425,24.0416713436984));
#73632=CARTESIAN_POINT('Ctrl Pts',(31.017781090129,-0.587616186362132,24.0833380103651));
#73633=CARTESIAN_POINT('Ctrl Pts',(31.3570414535054,-1.35453513912972E-14,
24.1250046770317));
#73634=CARTESIAN_POINT('Ctrl Pts',(31.017781090129,0.587616186362104,24.1666713436984));
#73635=CARTESIAN_POINT('Ctrl Pts',(30.6785207267527,1.17523237272422,24.2083380103651));
#73636=CARTESIAN_POINT('Ctrl Pts',(30.,1.17523237272422,24.2500046770317));
#73637=CARTESIAN_POINT('Ctrl Pts',(29.3214792732473,1.17523237272422,24.2916713436984));
#73638=CARTESIAN_POINT('Ctrl Pts',(28.9822189098709,0.587616186362105,24.3333380103651));
#73639=CARTESIAN_POINT('Ctrl Pts',(28.6429585464946,-1.32141491426617E-14,
24.3750046770317));
#73640=CARTESIAN_POINT('Ctrl Pts',(28.9822189098709,-0.587616186362132,
24.4166713436984));
#73641=CARTESIAN_POINT('Ctrl Pts',(29.3214792732473,-1.17523237272425,24.4583380103651));
#73642=CARTESIAN_POINT('Ctrl Pts',(30.,-1.17523237272425,24.5000046770317));
#73643=CARTESIAN_POINT('Ctrl Pts',(30.6785207267527,-1.17523237272425,24.5416713436984));
#73644=CARTESIAN_POINT('Ctrl Pts',(31.017781090129,-0.587616186362132,24.5833380103651));
#73645=CARTESIAN_POINT('Ctrl Pts',(31.3570414535054,-1.35453513912972E-14,
24.6250046770317));
#73646=CARTESIAN_POINT('Ctrl Pts',(31.017781090129,0.587616186362104,24.6666713436984));
#73647=CARTESIAN_POINT('Ctrl Pts',(30.6785207267527,1.17523237272422,24.7083380103651));
#73648=CARTESIAN_POINT('Ctrl Pts',(30.,1.17523237272422,24.7500046770317));
#73649=CARTESIAN_POINT('Ctrl Pts',(29.3214792732473,1.17523237272422,24.7916713436984));
#73650=CARTESIAN_POINT('Ctrl Pts',(28.9822189098709,0.587616186362105,24.8333380103651));
#73651=CARTESIAN_POINT('Ctrl Pts',(28.6429585464946,-1.32141491426617E-14,
24.8750046770317));
#73652=CARTESIAN_POINT('Ctrl Pts',(28.9822189098709,-0.587616186362132,
24.9166713436984));
#73653=CARTESIAN_POINT('Ctrl Pts',(29.3214792732473,-1.17523237272425,24.9583380103651));
#73654=CARTESIAN_POINT('Ctrl Pts',(30.,-1.17523237272425,25.0000046770317));
#73655=CARTESIAN_POINT('Ctrl Pts',(30.6785207267527,-1.17523237272425,25.0416713436984));
#73656=CARTESIAN_POINT('Ctrl Pts',(31.017781090129,-0.587616186362132,25.0833380103651));
#73657=CARTESIAN_POINT('Ctrl Pts',(31.3570414535054,-1.35453513912972E-14,
25.1250046770317));
#73658=CARTESIAN_POINT('Ctrl Pts',(31.017781090129,0.587616186362104,25.1666713436984));
#73659=CARTESIAN_POINT('Ctrl Pts',(30.6785207267527,1.17523237272422,25.2083380103651));
#73660=CARTESIAN_POINT('Ctrl Pts',(30.,1.17523237272422,25.2500046770317));
#73661=CARTESIAN_POINT('Ctrl Pts',(29.3214792732473,1.17523237272422,25.2916713436984));
#73662=CARTESIAN_POINT('Ctrl Pts',(28.9822189098709,0.587616186362105,25.3333380103651));
#73663=CARTESIAN_POINT('Ctrl Pts',(28.6429585464946,-1.32141491426617E-14,
25.3750046770317));
#73664=CARTESIAN_POINT('Ctrl Pts',(28.9822189098709,-0.587616186362132,
25.4166713436984));
#73665=CARTESIAN_POINT('Ctrl Pts',(29.3214792732473,-1.17523237272425,25.4583380103651));
#73666=CARTESIAN_POINT('Ctrl Pts',(30.,-1.17523237272425,25.5000046770317));
#73667=CARTESIAN_POINT('Ctrl Pts',(30.6785207267527,-1.17523237272425,25.5416713436984));
#73668=CARTESIAN_POINT('Ctrl Pts',(31.017781090129,-0.587616186362132,25.5833380103651));
#73669=CARTESIAN_POINT('Ctrl Pts',(31.3570414535054,-1.35453513912972E-14,
25.6250046770317));
#73670=CARTESIAN_POINT('Ctrl Pts',(31.017781090129,0.587616186362104,25.6666713436984));
#73671=CARTESIAN_POINT('Ctrl Pts',(30.6785207267527,1.17523237272422,25.7083380103651));
#73672=CARTESIAN_POINT('Ctrl Pts',(30.,1.17523237272422,25.7500046770317));
#73673=CARTESIAN_POINT('Ctrl Pts',(29.3214792732473,1.17523237272422,25.7916713436984));
#73674=CARTESIAN_POINT('Ctrl Pts',(28.9822189098709,0.587616186362105,25.8333380103651));
#73675=CARTESIAN_POINT('Ctrl Pts',(28.6429585464946,-1.32141491426617E-14,
25.8750046770317));
#73676=CARTESIAN_POINT('Ctrl Pts',(28.9822189098709,-0.587616186362132,
25.9166713436984));
#73677=CARTESIAN_POINT('Ctrl Pts',(29.3214792732473,-1.17523237272425,25.9583380103651));
#73678=CARTESIAN_POINT('Ctrl Pts',(30.,-1.17523237272425,26.0000046770317));
#73679=CARTESIAN_POINT('Ctrl Pts',(30.6785207267527,-1.17523237272425,26.0416713436984));
#73680=CARTESIAN_POINT('Ctrl Pts',(31.017781090129,-0.587616186362132,26.0833380103651));
#73681=CARTESIAN_POINT('Ctrl Pts',(31.3570414535054,-1.35453513912972E-14,
26.1250046770317));
#73682=CARTESIAN_POINT('Ctrl Pts',(31.017781090129,0.587616186362104,26.1666713436984));
#73683=CARTESIAN_POINT('Ctrl Pts',(30.6785207267527,1.17523237272422,26.2083380103651));
#73684=CARTESIAN_POINT('Ctrl Pts',(30.,1.17523237272422,26.2500046770317));
#73685=CARTESIAN_POINT('Ctrl Pts',(29.3214792732473,1.17523237272422,26.2916713436984));
#73686=CARTESIAN_POINT('Ctrl Pts',(28.9822189098709,0.587616186362105,26.3333380103651));
#73687=CARTESIAN_POINT('Ctrl Pts',(28.6429585464946,-1.32141491426617E-14,
26.3750046770317));
#73688=CARTESIAN_POINT('Ctrl Pts',(28.9822189098709,-0.587616186362132,
26.4166713436984));
#73689=CARTESIAN_POINT('Ctrl Pts',(29.3214792732473,-1.17523237272425,26.4583380103651));
#73690=CARTESIAN_POINT('Ctrl Pts',(30.,-1.17523237272425,26.5000046770317));
#73691=CARTESIAN_POINT('Ctrl Pts',(30.6785207267527,-1.17523237272425,26.5416713436984));
#73692=CARTESIAN_POINT('Ctrl Pts',(31.017781090129,-0.587616186362132,26.5833380103651));
#73693=CARTESIAN_POINT('Ctrl Pts',(31.3570414535054,-1.35453513912972E-14,
26.6250046770317));
#73694=CARTESIAN_POINT('Ctrl Pts',(31.017781090129,0.587616186362104,26.6666713436984));
#73695=CARTESIAN_POINT('Ctrl Pts',(30.6785207267527,1.17523237272422,26.7083380103651));
#73696=CARTESIAN_POINT('Ctrl Pts',(30.,1.17523237272422,26.7500046770317));
#73697=CARTESIAN_POINT('Ctrl Pts',(29.3214792732473,1.17523237272422,26.7916713436984));
#73698=CARTESIAN_POINT('Ctrl Pts',(28.9822189098709,0.587616186362105,26.8333380103651));
#73699=CARTESIAN_POINT('Ctrl Pts',(28.6429585464946,-1.32141491426617E-14,
26.8750046770317));
#73700=CARTESIAN_POINT('Ctrl Pts',(28.9822189098709,-0.587616186362132,
26.9166713436984));
#73701=CARTESIAN_POINT('Ctrl Pts',(29.3214792732473,-1.17523237272425,26.9583380103651));
#73702=CARTESIAN_POINT('Ctrl Pts',(30.,-1.17523237272425,27.0000046770317));
#73703=CARTESIAN_POINT('Ctrl Pts',(30.6785207267527,-1.17523237272425,27.0416713436984));
#73704=CARTESIAN_POINT('Ctrl Pts',(31.017781090129,-0.587616186362132,27.0833380103651));
#73705=CARTESIAN_POINT('Ctrl Pts',(31.3570414535054,-1.35453513912972E-14,
27.1250046770317));
#73706=CARTESIAN_POINT('Ctrl Pts',(31.017781090129,0.587616186362104,27.1666713436984));
#73707=CARTESIAN_POINT('Ctrl Pts',(30.6785207267527,1.17523237272422,27.2083380103651));
#73708=CARTESIAN_POINT('Ctrl Pts',(30.,1.17523237272422,27.2500046770317));
#73709=CARTESIAN_POINT('Ctrl Pts',(29.3214792732473,1.17523237272422,27.2916713436984));
#73710=CARTESIAN_POINT('Ctrl Pts',(28.9822189098709,0.587616186362105,27.3333380103651));
#73711=CARTESIAN_POINT('Ctrl Pts',(28.6429585464946,-1.32141491426617E-14,
27.3750046770317));
#73712=CARTESIAN_POINT('Ctrl Pts',(28.9822189098709,-0.587616186362132,
27.4166713436984));
#73713=CARTESIAN_POINT('Ctrl Pts',(29.3214792732473,-1.17523237272425,27.4583380103651));
#73714=CARTESIAN_POINT('Ctrl Pts',(30.,-1.17523237272425,27.5000046770317));
#73715=CARTESIAN_POINT('Ctrl Pts',(30.6785207267527,-1.17523237272425,27.5416713436984));
#73716=CARTESIAN_POINT('Ctrl Pts',(31.017781090129,-0.587616186362132,27.5833380103651));
#73717=CARTESIAN_POINT('Ctrl Pts',(31.3570414535054,-1.35453513912972E-14,
27.6250046770317));
#73718=CARTESIAN_POINT('Ctrl Pts',(31.017781090129,0.587616186362104,27.6666713436984));
#73719=CARTESIAN_POINT('Ctrl Pts',(30.6785207267527,1.17523237272422,27.7083380103651));
#73720=CARTESIAN_POINT('Ctrl Pts',(30.,1.17523237272422,27.7500046770317));
#73721=CARTESIAN_POINT('Ctrl Pts',(29.3214792732473,1.17523237272422,27.7916713436984));
#73722=CARTESIAN_POINT('Ctrl Pts',(28.9822189098709,0.587616186362105,27.8333380103651));
#73723=CARTESIAN_POINT('Ctrl Pts',(28.6429585464946,-1.32141491426617E-14,
27.8750046770317));
#73724=CARTESIAN_POINT('Ctrl Pts',(28.9822189098709,-0.587616186362132,
27.9166713436984));
#73725=CARTESIAN_POINT('Ctrl Pts',(29.3214792732473,-1.17523237272425,27.9583380103651));
#73726=CARTESIAN_POINT('Ctrl Pts',(30.,-1.17523237272425,28.0000046770317));
#73727=CARTESIAN_POINT('Ctrl Pts',(30.6785207267527,-1.17523237272425,28.0416713436984));
#73728=CARTESIAN_POINT('Ctrl Pts',(31.017781090129,-0.587616186362132,28.0833380103651));
#73729=CARTESIAN_POINT('Ctrl Pts',(31.3570414535054,-1.35453513912972E-14,
28.1250046770317));
#73730=CARTESIAN_POINT('Ctrl Pts',(31.017781090129,0.587616186362104,28.1666713436984));
#73731=CARTESIAN_POINT('Ctrl Pts',(30.6785207267527,1.17523237272422,28.2083380103651));
#73732=CARTESIAN_POINT('Ctrl Pts',(30.,1.17523237272422,28.2500046770317));
#73733=CARTESIAN_POINT('Ctrl Pts',(29.3214792732473,1.17523237272422,28.2916713436984));
#73734=CARTESIAN_POINT('Ctrl Pts',(28.9822189098709,0.587616186362105,28.3333380103651));
#73735=CARTESIAN_POINT('Ctrl Pts',(28.6429585464946,-1.32141491426617E-14,
28.3750046770317));
#73736=CARTESIAN_POINT('Ctrl Pts',(28.9822189098709,-0.587616186362132,
28.4166713436984));
#73737=CARTESIAN_POINT('Ctrl Pts',(29.3214792732473,-1.17523237272425,28.4583380103651));
#73738=CARTESIAN_POINT('Ctrl Pts',(30.,-1.17523237272425,28.5000046770317));
#73739=CARTESIAN_POINT('Ctrl Pts',(30.6785207267527,-1.17523237272425,28.5416713436984));
#73740=CARTESIAN_POINT('Ctrl Pts',(31.017781090129,-0.587616186362132,28.5833380103651));
#73741=CARTESIAN_POINT('Ctrl Pts',(31.3570414535054,-1.35453513912972E-14,
28.6250046770317));
#73742=CARTESIAN_POINT('Ctrl Pts',(31.017781090129,0.587616186362104,28.6666713436984));
#73743=CARTESIAN_POINT('Ctrl Pts',(30.6785207267527,1.17523237272422,28.7083380103651));
#73744=CARTESIAN_POINT('Ctrl Pts',(30.,1.17523237272422,28.7500046770317));
#73745=CARTESIAN_POINT('Ctrl Pts',(29.3214792732473,1.17523237272422,28.7916713436984));
#73746=CARTESIAN_POINT('Ctrl Pts',(28.9822189098709,0.587616186362105,28.8333380103651));
#73747=CARTESIAN_POINT('Ctrl Pts',(28.6429585464946,-1.32141491426617E-14,
28.8750046770317));
#73748=CARTESIAN_POINT('Ctrl Pts',(28.9822189098709,-0.587616186362132,
28.9166713436984));
#73749=CARTESIAN_POINT('Ctrl Pts',(29.3214792732473,-1.17523237272425,28.9583380103651));
#73750=CARTESIAN_POINT('Ctrl Pts',(30.,-1.17523237272425,29.0000046770317));
#73751=CARTESIAN_POINT('Ctrl Pts',(30.6785207267527,-1.17523237272425,29.0416713436984));
#73752=CARTESIAN_POINT('Ctrl Pts',(31.017781090129,-0.587616186362132,29.0833380103651));
#73753=CARTESIAN_POINT('Ctrl Pts',(31.3570414535054,-1.35453513912972E-14,
29.1250046770317));
#73754=CARTESIAN_POINT('Ctrl Pts',(31.017781090129,0.587616186362104,29.1666713436984));
#73755=CARTESIAN_POINT('Ctrl Pts',(30.6785207267527,1.17523237272422,29.2083380103651));
#73756=CARTESIAN_POINT('Ctrl Pts',(30.,1.17523237272422,29.2500046770317));
#73757=CARTESIAN_POINT('Ctrl Pts',(29.3214792732473,1.17523237272422,29.2916713436984));
#73758=CARTESIAN_POINT('Ctrl Pts',(28.9822189098709,0.587616186362105,29.3333380103651));
#73759=CARTESIAN_POINT('Ctrl Pts',(28.6429585464946,-1.32141491426617E-14,
29.3750046770317));
#73760=CARTESIAN_POINT('Ctrl Pts',(28.9822189098709,-0.587616186362132,
29.4166713436984));
#73761=CARTESIAN_POINT('Ctrl Pts',(29.3214792732473,-1.17523237272425,29.4583380103651));
#73762=CARTESIAN_POINT('Ctrl Pts',(30.,-1.17523237272425,29.5000046770317));
#73763=CARTESIAN_POINT('Ctrl Pts',(30.6785207267527,-1.17523237272425,29.5416713436984));
#73764=CARTESIAN_POINT('Ctrl Pts',(31.017781090129,-0.587616186362132,29.5833380103651));
#73765=CARTESIAN_POINT('Ctrl Pts',(31.3570414535054,-1.35453513912972E-14,
29.6250046770317));
#73766=CARTESIAN_POINT('Ctrl Pts',(31.017781090129,0.587616186362104,29.6666713436984));
#73767=CARTESIAN_POINT('Ctrl Pts',(30.6785207267527,1.17523237272422,29.7083380103651));
#73768=CARTESIAN_POINT('Ctrl Pts',(30.,1.17523237272422,29.7500046770317));
#73769=CARTESIAN_POINT('Ctrl Pts',(29.3214792732473,1.17523237272422,29.7916713436984));
#73770=CARTESIAN_POINT('Ctrl Pts',(28.9822189098709,0.587616186362105,29.8333380103651));
#73771=CARTESIAN_POINT('Ctrl Pts',(28.6429585464946,-1.32141491426617E-14,
29.8750046770317));
#73772=CARTESIAN_POINT('Ctrl Pts',(28.9822189098709,-0.587616186362132,
29.9166713436984));
#73773=CARTESIAN_POINT('Ctrl Pts',(29.3214792732473,-1.17523237272425,29.9583380103651));
#73774=CARTESIAN_POINT('Ctrl Pts',(30.,-1.17523237272425,30.0000046770317));
#73775=CARTESIAN_POINT('Ctrl Pts',(30.6785207267527,-1.17523237272425,30.0416713436984));
#73776=CARTESIAN_POINT('Ctrl Pts',(31.017781090129,-0.587616186362132,30.0833380103651));
#73777=CARTESIAN_POINT('Ctrl Pts',(31.3570414535054,-1.35453513912972E-14,
30.1250046770317));
#73778=CARTESIAN_POINT('Ctrl Pts',(31.017781090129,0.587616186362104,30.1666713436984));
#73779=CARTESIAN_POINT('Ctrl Pts',(30.6785207267527,1.17523237272422,30.2083380103651));
#73780=CARTESIAN_POINT('Ctrl Pts',(30.,1.17523237272422,30.2500046770317));
#73781=CARTESIAN_POINT('Ctrl Pts',(29.3214792732473,1.17523237272422,30.2916713436984));
#73782=CARTESIAN_POINT('Ctrl Pts',(28.9822189098709,0.587616186362105,30.3333380103651));
#73783=CARTESIAN_POINT('Ctrl Pts',(28.6429585464946,-1.32141491426617E-14,
30.3750046770317));
#73784=CARTESIAN_POINT('Ctrl Pts',(28.9822189098709,-0.587616186362132,
30.4166713436984));
#73785=CARTESIAN_POINT('Ctrl Pts',(29.3214792732473,-1.17523237272425,30.4583380103651));
#73786=CARTESIAN_POINT('Ctrl Pts',(30.,-1.17523237272425,30.5000046770317));
#73787=CARTESIAN_POINT('Ctrl Pts',(30.6785207267527,-1.17523237272425,30.5416713436984));
#73788=CARTESIAN_POINT('Ctrl Pts',(31.017781090129,-0.587616186362132,30.5833380103651));
#73789=CARTESIAN_POINT('Ctrl Pts',(31.3570414535054,-1.35453513912972E-14,
30.6250046770317));
#73790=CARTESIAN_POINT('Ctrl Pts',(31.017781090129,0.587616186362104,30.6666713436984));
#73791=CARTESIAN_POINT('Ctrl Pts',(30.6785207267527,1.17523237272422,30.7083380103651));
#73792=CARTESIAN_POINT('Ctrl Pts',(30.,1.17523237272422,30.7500046770317));
#73793=CARTESIAN_POINT('Ctrl Pts',(29.3214792732473,1.17523237272422,30.7916713436984));
#73794=CARTESIAN_POINT('Ctrl Pts',(28.9822189098709,0.587616186362105,30.8333380103651));
#73795=CARTESIAN_POINT('Ctrl Pts',(28.6429585464946,-1.32141491426617E-14,
30.8750046770317));
#73796=CARTESIAN_POINT('Ctrl Pts',(28.9822189098709,-0.587616186362132,
30.9166713436984));
#73797=CARTESIAN_POINT('Ctrl Pts',(29.3214792732473,-1.17523237272425,30.9583380103651));
#73798=CARTESIAN_POINT('Ctrl Pts',(30.,-1.17523237272425,31.0000046770317));
#73799=CARTESIAN_POINT('Ctrl Pts',(30.6785207267527,-1.17523237272425,31.0416713436984));
#73800=CARTESIAN_POINT('Ctrl Pts',(31.017781090129,-0.587616186362132,31.0833380103651));
#73801=CARTESIAN_POINT('Ctrl Pts',(31.3570414535054,-1.35453513912972E-14,
31.1250046770317));
#73802=CARTESIAN_POINT('Ctrl Pts',(31.017781090129,0.587616186362104,31.1666713436984));
#73803=CARTESIAN_POINT('Ctrl Pts',(30.6785207267527,1.17523237272422,31.2083380103651));
#73804=CARTESIAN_POINT('Ctrl Pts',(30.,1.17523237272422,31.2500046770317));
#73805=CARTESIAN_POINT('Ctrl Pts',(30.,1.52706329386825,15.546875));
#73806=CARTESIAN_POINT('Ctrl Pts',(29.1183495962155,1.52706329386825,15.5885416666667));
#73807=CARTESIAN_POINT('Ctrl Pts',(28.6775243943233,0.76353164693412,15.6302083333334));
#73808=CARTESIAN_POINT('Ctrl Pts',(28.2366991924311,-1.31894491186926E-14,
15.671875));
#73809=CARTESIAN_POINT('Ctrl Pts',(28.6775243943233,-0.763531646934146,
15.7135416666667));
#73810=CARTESIAN_POINT('Ctrl Pts',(29.1183495962155,-1.52706329386828,15.7552083333334));
#73811=CARTESIAN_POINT('Ctrl Pts',(30.,-1.52706329386828,15.796875));
#73812=CARTESIAN_POINT('Ctrl Pts',(30.8816504037844,-1.52706329386828,15.8385416666667));
#73813=CARTESIAN_POINT('Ctrl Pts',(31.3224756056766,-0.763531646934147,
15.8802083333334));
#73814=CARTESIAN_POINT('Ctrl Pts',(31.7633008075689,-1.36198038370242E-14,
15.921875));
#73815=CARTESIAN_POINT('Ctrl Pts',(31.3224756056766,0.763531646934118,15.9635416666667));
#73816=CARTESIAN_POINT('Ctrl Pts',(30.8816504037844,1.52706329386825,16.0052083333334));
#73817=CARTESIAN_POINT('Ctrl Pts',(30.,1.52706329386825,16.046875));
#73818=CARTESIAN_POINT('Ctrl Pts',(29.1183495962155,1.52706329386825,16.0885416666667));
#73819=CARTESIAN_POINT('Ctrl Pts',(28.6775243943233,0.76353164693412,16.1302083333334));
#73820=CARTESIAN_POINT('Ctrl Pts',(28.2366991924311,-1.31894491186926E-14,
16.171875));
#73821=CARTESIAN_POINT('Ctrl Pts',(28.6775243943233,-0.763531646934146,
16.2135416666667));
#73822=CARTESIAN_POINT('Ctrl Pts',(29.1183495962155,-1.52706329386828,16.2552083333334));
#73823=CARTESIAN_POINT('Ctrl Pts',(30.,-1.52706329386828,16.296875));
#73824=CARTESIAN_POINT('Ctrl Pts',(30.8816504037844,-1.52706329386828,16.3385416666667));
#73825=CARTESIAN_POINT('Ctrl Pts',(31.3224756056766,-0.763531646934147,
16.3802083333334));
#73826=CARTESIAN_POINT('Ctrl Pts',(31.7633008075689,-1.36198038370242E-14,
16.421875));
#73827=CARTESIAN_POINT('Ctrl Pts',(31.3224756056766,0.763531646934118,16.4635416666667));
#73828=CARTESIAN_POINT('Ctrl Pts',(30.8816504037844,1.52706329386825,16.5052083333334));
#73829=CARTESIAN_POINT('Ctrl Pts',(30.,1.52706329386825,16.546875));
#73830=CARTESIAN_POINT('Ctrl Pts',(29.1183495962155,1.52706329386825,16.5885416666667));
#73831=CARTESIAN_POINT('Ctrl Pts',(28.6775243943233,0.76353164693412,16.6302083333334));
#73832=CARTESIAN_POINT('Ctrl Pts',(28.2366991924311,-1.31894491186926E-14,
16.671875));
#73833=CARTESIAN_POINT('Ctrl Pts',(28.6775243943233,-0.763531646934146,
16.7135416666667));
#73834=CARTESIAN_POINT('Ctrl Pts',(29.1183495962155,-1.52706329386828,16.7552083333334));
#73835=CARTESIAN_POINT('Ctrl Pts',(30.,-1.52706329386828,16.796875));
#73836=CARTESIAN_POINT('Ctrl Pts',(30.8816504037844,-1.52706329386828,16.8385416666667));
#73837=CARTESIAN_POINT('Ctrl Pts',(31.3224756056766,-0.763531646934147,
16.8802083333334));
#73838=CARTESIAN_POINT('Ctrl Pts',(31.7633008075689,-1.36198038370242E-14,
16.921875));
#73839=CARTESIAN_POINT('Ctrl Pts',(31.3224756056766,0.763531646934118,16.9635416666667));
#73840=CARTESIAN_POINT('Ctrl Pts',(30.8816504037844,1.52706329386825,17.0052083333334));
#73841=CARTESIAN_POINT('Ctrl Pts',(30.,1.52706329386825,17.046875));
#73842=CARTESIAN_POINT('Ctrl Pts',(29.1183495962155,1.52706329386825,17.0885416666667));
#73843=CARTESIAN_POINT('Ctrl Pts',(28.6775243943233,0.76353164693412,17.1302083333334));
#73844=CARTESIAN_POINT('Ctrl Pts',(28.2366991924311,-1.31894491186926E-14,
17.171875));
#73845=CARTESIAN_POINT('Ctrl Pts',(28.6775243943233,-0.763531646934146,
17.2135416666667));
#73846=CARTESIAN_POINT('Ctrl Pts',(29.1183495962155,-1.52706329386828,17.2552083333334));
#73847=CARTESIAN_POINT('Ctrl Pts',(30.,-1.52706329386828,17.296875));
#73848=CARTESIAN_POINT('Ctrl Pts',(30.8816504037844,-1.52706329386828,17.3385416666667));
#73849=CARTESIAN_POINT('Ctrl Pts',(31.3224756056766,-0.763531646934147,
17.3802083333334));
#73850=CARTESIAN_POINT('Ctrl Pts',(31.7633008075689,-1.36198038370242E-14,
17.421875));
#73851=CARTESIAN_POINT('Ctrl Pts',(31.3224756056766,0.763531646934118,17.4635416666667));
#73852=CARTESIAN_POINT('Ctrl Pts',(30.8816504037844,1.52706329386825,17.5052083333334));
#73853=CARTESIAN_POINT('Ctrl Pts',(30.,1.52706329386825,17.546875));
#73854=CARTESIAN_POINT('Ctrl Pts',(29.1183495962155,1.52706329386825,17.5885416666667));
#73855=CARTESIAN_POINT('Ctrl Pts',(28.6775243943233,0.76353164693412,17.6302083333334));
#73856=CARTESIAN_POINT('Ctrl Pts',(28.2366991924311,-1.31894491186926E-14,
17.671875));
#73857=CARTESIAN_POINT('Ctrl Pts',(28.6775243943233,-0.763531646934146,
17.7135416666667));
#73858=CARTESIAN_POINT('Ctrl Pts',(29.1183495962155,-1.52706329386828,17.7552083333334));
#73859=CARTESIAN_POINT('Ctrl Pts',(30.,-1.52706329386828,17.796875));
#73860=CARTESIAN_POINT('Ctrl Pts',(30.8816504037844,-1.52706329386828,17.8385416666667));
#73861=CARTESIAN_POINT('Ctrl Pts',(31.3224756056766,-0.763531646934147,
17.8802083333334));
#73862=CARTESIAN_POINT('Ctrl Pts',(31.7633008075689,-1.36198038370242E-14,
17.921875));
#73863=CARTESIAN_POINT('Ctrl Pts',(31.3224756056766,0.763531646934118,17.9635416666667));
#73864=CARTESIAN_POINT('Ctrl Pts',(30.8816504037844,1.52706329386825,18.0052083333334));
#73865=CARTESIAN_POINT('Ctrl Pts',(30.,1.52706329386825,18.046875));
#73866=CARTESIAN_POINT('Ctrl Pts',(29.1183495962155,1.52706329386825,18.0885416666667));
#73867=CARTESIAN_POINT('Ctrl Pts',(28.6775243943233,0.76353164693412,18.1302083333334));
#73868=CARTESIAN_POINT('Ctrl Pts',(28.2366991924311,-1.31894491186926E-14,
18.171875));
#73869=CARTESIAN_POINT('Ctrl Pts',(28.6775243943233,-0.763531646934146,
18.2135416666667));
#73870=CARTESIAN_POINT('Ctrl Pts',(29.1183495962155,-1.52706329386828,18.2552083333334));
#73871=CARTESIAN_POINT('Ctrl Pts',(30.,-1.52706329386828,18.296875));
#73872=CARTESIAN_POINT('Ctrl Pts',(30.8816504037844,-1.52706329386828,18.3385416666667));
#73873=CARTESIAN_POINT('Ctrl Pts',(31.3224756056766,-0.763531646934147,
18.3802083333334));
#73874=CARTESIAN_POINT('Ctrl Pts',(31.7633008075689,-1.36198038370242E-14,
18.421875));
#73875=CARTESIAN_POINT('Ctrl Pts',(31.3224756056766,0.763531646934118,18.4635416666667));
#73876=CARTESIAN_POINT('Ctrl Pts',(30.8816504037844,1.52706329386825,18.5052083333334));
#73877=CARTESIAN_POINT('Ctrl Pts',(30.,1.52706329386825,18.546875));
#73878=CARTESIAN_POINT('Ctrl Pts',(29.1183495962155,1.52706329386825,18.5885416666667));
#73879=CARTESIAN_POINT('Ctrl Pts',(28.6775243943233,0.76353164693412,18.6302083333334));
#73880=CARTESIAN_POINT('Ctrl Pts',(28.2366991924311,-1.31894491186926E-14,
18.671875));
#73881=CARTESIAN_POINT('Ctrl Pts',(28.6775243943233,-0.763531646934146,
18.7135416666667));
#73882=CARTESIAN_POINT('Ctrl Pts',(29.1183495962155,-1.52706329386828,18.7552083333334));
#73883=CARTESIAN_POINT('Ctrl Pts',(30.,-1.52706329386828,18.796875));
#73884=CARTESIAN_POINT('Ctrl Pts',(30.8816504037844,-1.52706329386828,18.8385416666667));
#73885=CARTESIAN_POINT('Ctrl Pts',(31.3224756056766,-0.763531646934147,
18.8802083333334));
#73886=CARTESIAN_POINT('Ctrl Pts',(31.7633008075689,-1.36198038370242E-14,
18.921875));
#73887=CARTESIAN_POINT('Ctrl Pts',(31.3224756056766,0.763531646934118,18.9635416666667));
#73888=CARTESIAN_POINT('Ctrl Pts',(30.8816504037844,1.52706329386825,19.0052083333334));
#73889=CARTESIAN_POINT('Ctrl Pts',(30.,1.52706329386825,19.046875));
#73890=CARTESIAN_POINT('Ctrl Pts',(29.1183495962155,1.52706329386825,19.0885416666667));
#73891=CARTESIAN_POINT('Ctrl Pts',(28.6775243943233,0.76353164693412,19.1302083333334));
#73892=CARTESIAN_POINT('Ctrl Pts',(28.2366991924311,-1.31894491186926E-14,
19.171875));
#73893=CARTESIAN_POINT('Ctrl Pts',(28.6775243943233,-0.763531646934146,
19.2135416666667));
#73894=CARTESIAN_POINT('Ctrl Pts',(29.1183495962155,-1.52706329386828,19.2552083333334));
#73895=CARTESIAN_POINT('Ctrl Pts',(30.,-1.52706329386828,19.296875));
#73896=CARTESIAN_POINT('Ctrl Pts',(30.8816504037844,-1.52706329386828,19.3385416666667));
#73897=CARTESIAN_POINT('Ctrl Pts',(31.3224756056766,-0.763531646934147,
19.3802083333334));
#73898=CARTESIAN_POINT('Ctrl Pts',(31.7633008075689,-1.36198038370242E-14,
19.421875));
#73899=CARTESIAN_POINT('Ctrl Pts',(31.3224756056766,0.763531646934118,19.4635416666667));
#73900=CARTESIAN_POINT('Ctrl Pts',(30.8816504037844,1.52706329386825,19.5052083333334));
#73901=CARTESIAN_POINT('Ctrl Pts',(30.,1.52706329386825,19.546875));
#73902=CARTESIAN_POINT('Ctrl Pts',(29.1183495962155,1.52706329386825,19.5885416666667));
#73903=CARTESIAN_POINT('Ctrl Pts',(28.6775243943233,0.76353164693412,19.6302083333334));
#73904=CARTESIAN_POINT('Ctrl Pts',(28.2366991924311,-1.31894491186926E-14,
19.671875));
#73905=CARTESIAN_POINT('Ctrl Pts',(28.6775243943233,-0.763531646934146,
19.7135416666667));
#73906=CARTESIAN_POINT('Ctrl Pts',(29.1183495962155,-1.52706329386828,19.7552083333334));
#73907=CARTESIAN_POINT('Ctrl Pts',(30.,-1.52706329386828,19.796875));
#73908=CARTESIAN_POINT('Ctrl Pts',(30.8816504037844,-1.52706329386828,19.8385416666667));
#73909=CARTESIAN_POINT('Ctrl Pts',(31.3224756056766,-0.763531646934147,
19.8802083333334));
#73910=CARTESIAN_POINT('Ctrl Pts',(31.7633008075689,-1.36198038370242E-14,
19.921875));
#73911=CARTESIAN_POINT('Ctrl Pts',(31.3224756056766,0.763531646934118,19.9635416666667));
#73912=CARTESIAN_POINT('Ctrl Pts',(30.8816504037844,1.52706329386825,20.0052083333334));
#73913=CARTESIAN_POINT('Ctrl Pts',(30.,1.52706329386825,20.046875));
#73914=CARTESIAN_POINT('Ctrl Pts',(29.1183495962155,1.52706329386825,20.0885416666667));
#73915=CARTESIAN_POINT('Ctrl Pts',(28.6775243943233,0.76353164693412,20.1302083333334));
#73916=CARTESIAN_POINT('Ctrl Pts',(28.2366991924311,-1.31894491186926E-14,
20.171875));
#73917=CARTESIAN_POINT('Ctrl Pts',(28.6775243943233,-0.763531646934146,
20.2135416666667));
#73918=CARTESIAN_POINT('Ctrl Pts',(29.1183495962155,-1.52706329386828,20.2552083333334));
#73919=CARTESIAN_POINT('Ctrl Pts',(30.,-1.52706329386828,20.296875));
#73920=CARTESIAN_POINT('Ctrl Pts',(30.8816504037844,-1.52706329386828,20.3385416666667));
#73921=CARTESIAN_POINT('Ctrl Pts',(31.3224756056766,-0.763531646934147,
20.3802083333334));
#73922=CARTESIAN_POINT('Ctrl Pts',(31.7633008075689,-1.36198038370242E-14,
20.421875));
#73923=CARTESIAN_POINT('Ctrl Pts',(31.3224756056766,0.763531646934118,20.4635416666667));
#73924=CARTESIAN_POINT('Ctrl Pts',(30.8816504037844,1.52706329386825,20.5052083333334));
#73925=CARTESIAN_POINT('Ctrl Pts',(30.,1.52706329386825,20.546875));
#73926=CARTESIAN_POINT('Ctrl Pts',(29.1183495962155,1.52706329386825,20.5885416666667));
#73927=CARTESIAN_POINT('Ctrl Pts',(28.6775243943233,0.76353164693412,20.6302083333334));
#73928=CARTESIAN_POINT('Ctrl Pts',(28.2366991924311,-1.31894491186926E-14,
20.671875));
#73929=CARTESIAN_POINT('Ctrl Pts',(28.6775243943233,-0.763531646934146,
20.7135416666667));
#73930=CARTESIAN_POINT('Ctrl Pts',(29.1183495962155,-1.52706329386828,20.7552083333334));
#73931=CARTESIAN_POINT('Ctrl Pts',(30.,-1.52706329386828,20.796875));
#73932=CARTESIAN_POINT('Ctrl Pts',(30.8816504037844,-1.52706329386828,20.8385416666667));
#73933=CARTESIAN_POINT('Ctrl Pts',(31.3224756056766,-0.763531646934147,
20.8802083333334));
#73934=CARTESIAN_POINT('Ctrl Pts',(31.7633008075689,-1.36198038370242E-14,
20.921875));
#73935=CARTESIAN_POINT('Ctrl Pts',(31.3224756056766,0.763531646934118,20.9635416666667));
#73936=CARTESIAN_POINT('Ctrl Pts',(30.8816504037844,1.52706329386825,21.0052083333334));
#73937=CARTESIAN_POINT('Ctrl Pts',(30.,1.52706329386825,21.046875));
#73938=CARTESIAN_POINT('Ctrl Pts',(29.1183495962155,1.52706329386825,21.0885416666667));
#73939=CARTESIAN_POINT('Ctrl Pts',(28.6775243943233,0.76353164693412,21.1302083333334));
#73940=CARTESIAN_POINT('Ctrl Pts',(28.2366991924311,-1.31894491186926E-14,
21.171875));
#73941=CARTESIAN_POINT('Ctrl Pts',(28.6775243943233,-0.763531646934146,
21.2135416666667));
#73942=CARTESIAN_POINT('Ctrl Pts',(29.1183495962155,-1.52706329386828,21.2552083333334));
#73943=CARTESIAN_POINT('Ctrl Pts',(30.,-1.52706329386828,21.296875));
#73944=CARTESIAN_POINT('Ctrl Pts',(30.8816504037844,-1.52706329386828,21.3385416666667));
#73945=CARTESIAN_POINT('Ctrl Pts',(31.3224756056766,-0.763531646934147,
21.3802083333334));
#73946=CARTESIAN_POINT('Ctrl Pts',(31.7633008075689,-1.36198038370242E-14,
21.421875));
#73947=CARTESIAN_POINT('Ctrl Pts',(31.3224756056766,0.763531646934118,21.4635416666667));
#73948=CARTESIAN_POINT('Ctrl Pts',(30.8816504037844,1.52706329386825,21.5052083333334));
#73949=CARTESIAN_POINT('Ctrl Pts',(30.,1.52706329386825,21.546875));
#73950=CARTESIAN_POINT('Ctrl Pts',(29.1183495962155,1.52706329386825,21.5885416666667));
#73951=CARTESIAN_POINT('Ctrl Pts',(28.6775243943233,0.76353164693412,21.6302083333334));
#73952=CARTESIAN_POINT('Ctrl Pts',(28.2366991924311,-1.31894491186926E-14,
21.671875));
#73953=CARTESIAN_POINT('Ctrl Pts',(28.6775243943233,-0.763531646934146,
21.7135416666667));
#73954=CARTESIAN_POINT('Ctrl Pts',(29.1183495962155,-1.52706329386828,21.7552083333334));
#73955=CARTESIAN_POINT('Ctrl Pts',(30.,-1.52706329386828,21.796875));
#73956=CARTESIAN_POINT('Ctrl Pts',(30.8816504037844,-1.52706329386828,21.8385416666667));
#73957=CARTESIAN_POINT('Ctrl Pts',(31.3224756056766,-0.763531646934147,
21.8802083333334));
#73958=CARTESIAN_POINT('Ctrl Pts',(31.7633008075689,-1.36198038370242E-14,
21.921875));
#73959=CARTESIAN_POINT('Ctrl Pts',(31.3224756056766,0.763531646934118,21.9635416666667));
#73960=CARTESIAN_POINT('Ctrl Pts',(30.8816504037844,1.52706329386825,22.0052083333334));
#73961=CARTESIAN_POINT('Ctrl Pts',(30.,1.52706329386825,22.046875));
#73962=CARTESIAN_POINT('Ctrl Pts',(29.1183495962155,1.52706329386825,22.0885416666667));
#73963=CARTESIAN_POINT('Ctrl Pts',(28.6775243943233,0.76353164693412,22.1302083333334));
#73964=CARTESIAN_POINT('Ctrl Pts',(28.2366991924311,-1.31894491186926E-14,
22.171875));
#73965=CARTESIAN_POINT('Ctrl Pts',(28.6775243943233,-0.763531646934146,
22.2135416666667));
#73966=CARTESIAN_POINT('Ctrl Pts',(29.1183495962155,-1.52706329386828,22.2552083333334));
#73967=CARTESIAN_POINT('Ctrl Pts',(30.,-1.52706329386828,22.296875));
#73968=CARTESIAN_POINT('Ctrl Pts',(30.8816504037844,-1.52706329386828,22.3385416666667));
#73969=CARTESIAN_POINT('Ctrl Pts',(31.3224756056766,-0.763531646934147,
22.3802083333334));
#73970=CARTESIAN_POINT('Ctrl Pts',(31.7633008075689,-1.36198038370242E-14,
22.421875));
#73971=CARTESIAN_POINT('Ctrl Pts',(31.3224756056766,0.763531646934118,22.4635416666667));
#73972=CARTESIAN_POINT('Ctrl Pts',(30.8816504037844,1.52706329386825,22.5052083333334));
#73973=CARTESIAN_POINT('Ctrl Pts',(30.,1.52706329386825,22.546875));
#73974=CARTESIAN_POINT('Ctrl Pts',(29.1183495962155,1.52706329386825,22.5885416666667));
#73975=CARTESIAN_POINT('Ctrl Pts',(28.6775243943233,0.76353164693412,22.6302083333334));
#73976=CARTESIAN_POINT('Ctrl Pts',(28.2366991924311,-1.31894491186926E-14,
22.671875));
#73977=CARTESIAN_POINT('Ctrl Pts',(28.6775243943233,-0.763531646934146,
22.7135416666667));
#73978=CARTESIAN_POINT('Ctrl Pts',(29.1183495962155,-1.52706329386828,22.7552083333334));
#73979=CARTESIAN_POINT('Ctrl Pts',(30.,-1.52706329386828,22.796875));
#73980=CARTESIAN_POINT('Ctrl Pts',(30.8816504037844,-1.52706329386828,22.8385416666667));
#73981=CARTESIAN_POINT('Ctrl Pts',(31.3224756056766,-0.763531646934147,
22.8802083333334));
#73982=CARTESIAN_POINT('Ctrl Pts',(31.7633008075689,-1.36198038370242E-14,
22.921875));
#73983=CARTESIAN_POINT('Ctrl Pts',(31.3224756056766,0.763531646934118,22.9635416666667));
#73984=CARTESIAN_POINT('Ctrl Pts',(30.8816504037844,1.52706329386825,23.0052083333334));
#73985=CARTESIAN_POINT('Ctrl Pts',(30.,1.52706329386825,23.046875));
#73986=CARTESIAN_POINT('Ctrl Pts',(29.1183495962155,1.52706329386825,23.0885416666667));
#73987=CARTESIAN_POINT('Ctrl Pts',(28.6775243943233,0.76353164693412,23.1302083333334));
#73988=CARTESIAN_POINT('Ctrl Pts',(28.2366991924311,-1.31894491186926E-14,
23.171875));
#73989=CARTESIAN_POINT('Ctrl Pts',(28.6775243943233,-0.763531646934146,
23.2135416666667));
#73990=CARTESIAN_POINT('Ctrl Pts',(29.1183495962155,-1.52706329386828,23.2552083333334));
#73991=CARTESIAN_POINT('Ctrl Pts',(30.,-1.52706329386828,23.296875));
#73992=CARTESIAN_POINT('Ctrl Pts',(30.8816504037844,-1.52706329386828,23.3385416666667));
#73993=CARTESIAN_POINT('Ctrl Pts',(31.3224756056766,-0.763531646934147,
23.3802083333334));
#73994=CARTESIAN_POINT('Ctrl Pts',(31.7633008075689,-1.36198038370242E-14,
23.421875));
#73995=CARTESIAN_POINT('Ctrl Pts',(31.3224756056766,0.763531646934118,23.4635416666667));
#73996=CARTESIAN_POINT('Ctrl Pts',(30.8816504037844,1.52706329386825,23.5052083333334));
#73997=CARTESIAN_POINT('Ctrl Pts',(30.,1.52706329386825,23.546875));
#73998=CARTESIAN_POINT('Ctrl Pts',(29.1183495962155,1.52706329386825,23.5885416666667));
#73999=CARTESIAN_POINT('Ctrl Pts',(28.6775243943233,0.76353164693412,23.6302083333334));
#74000=CARTESIAN_POINT('Ctrl Pts',(28.2366991924311,-1.31894491186926E-14,
23.671875));
#74001=CARTESIAN_POINT('Ctrl Pts',(28.6775243943233,-0.763531646934146,
23.7135416666667));
#74002=CARTESIAN_POINT('Ctrl Pts',(29.1183495962155,-1.52706329386828,23.7552083333334));
#74003=CARTESIAN_POINT('Ctrl Pts',(30.,-1.52706329386828,23.796875));
#74004=CARTESIAN_POINT('Ctrl Pts',(30.8816504037844,-1.52706329386828,23.8385416666667));
#74005=CARTESIAN_POINT('Ctrl Pts',(31.3224756056766,-0.763531646934147,
23.8802083333334));
#74006=CARTESIAN_POINT('Ctrl Pts',(31.7633008075689,-1.36198038370242E-14,
23.921875));
#74007=CARTESIAN_POINT('Ctrl Pts',(31.3224756056766,0.763531646934118,23.9635416666667));
#74008=CARTESIAN_POINT('Ctrl Pts',(30.8816504037844,1.52706329386825,24.0052083333334));
#74009=CARTESIAN_POINT('Ctrl Pts',(30.,1.52706329386825,24.046875));
#74010=CARTESIAN_POINT('Ctrl Pts',(29.1183495962155,1.52706329386825,24.0885416666667));
#74011=CARTESIAN_POINT('Ctrl Pts',(28.6775243943233,0.76353164693412,24.1302083333334));
#74012=CARTESIAN_POINT('Ctrl Pts',(28.2366991924311,-1.31894491186926E-14,
24.171875));
#74013=CARTESIAN_POINT('Ctrl Pts',(28.6775243943233,-0.763531646934146,
24.2135416666667));
#74014=CARTESIAN_POINT('Ctrl Pts',(29.1183495962155,-1.52706329386828,24.2552083333334));
#74015=CARTESIAN_POINT('Ctrl Pts',(30.,-1.52706329386828,24.296875));
#74016=CARTESIAN_POINT('Ctrl Pts',(30.8816504037844,-1.52706329386828,24.3385416666667));
#74017=CARTESIAN_POINT('Ctrl Pts',(31.3224756056766,-0.763531646934147,
24.3802083333334));
#74018=CARTESIAN_POINT('Ctrl Pts',(31.7633008075689,-1.36198038370242E-14,
24.421875));
#74019=CARTESIAN_POINT('Ctrl Pts',(31.3224756056766,0.763531646934118,24.4635416666667));
#74020=CARTESIAN_POINT('Ctrl Pts',(30.8816504037844,1.52706329386825,24.5052083333334));
#74021=CARTESIAN_POINT('Ctrl Pts',(30.,1.52706329386825,24.546875));
#74022=CARTESIAN_POINT('Ctrl Pts',(29.1183495962155,1.52706329386825,24.5885416666667));
#74023=CARTESIAN_POINT('Ctrl Pts',(28.6775243943233,0.76353164693412,24.6302083333334));
#74024=CARTESIAN_POINT('Ctrl Pts',(28.2366991924311,-1.31894491186926E-14,
24.671875));
#74025=CARTESIAN_POINT('Ctrl Pts',(28.6775243943233,-0.763531646934146,
24.7135416666667));
#74026=CARTESIAN_POINT('Ctrl Pts',(29.1183495962155,-1.52706329386828,24.7552083333334));
#74027=CARTESIAN_POINT('Ctrl Pts',(30.,-1.52706329386828,24.796875));
#74028=CARTESIAN_POINT('Ctrl Pts',(30.8816504037844,-1.52706329386828,24.8385416666667));
#74029=CARTESIAN_POINT('Ctrl Pts',(31.3224756056766,-0.763531646934147,
24.8802083333334));
#74030=CARTESIAN_POINT('Ctrl Pts',(31.7633008075689,-1.36198038370242E-14,
24.921875));
#74031=CARTESIAN_POINT('Ctrl Pts',(31.3224756056766,0.763531646934118,24.9635416666667));
#74032=CARTESIAN_POINT('Ctrl Pts',(30.8816504037844,1.52706329386825,25.0052083333334));
#74033=CARTESIAN_POINT('Ctrl Pts',(30.,1.52706329386825,25.046875));
#74034=CARTESIAN_POINT('Ctrl Pts',(29.1183495962155,1.52706329386825,25.0885416666667));
#74035=CARTESIAN_POINT('Ctrl Pts',(28.6775243943233,0.76353164693412,25.1302083333334));
#74036=CARTESIAN_POINT('Ctrl Pts',(28.2366991924311,-1.31894491186926E-14,
25.171875));
#74037=CARTESIAN_POINT('Ctrl Pts',(28.6775243943233,-0.763531646934146,
25.2135416666667));
#74038=CARTESIAN_POINT('Ctrl Pts',(29.1183495962155,-1.52706329386828,25.2552083333334));
#74039=CARTESIAN_POINT('Ctrl Pts',(30.,-1.52706329386828,25.296875));
#74040=CARTESIAN_POINT('Ctrl Pts',(30.8816504037844,-1.52706329386828,25.3385416666667));
#74041=CARTESIAN_POINT('Ctrl Pts',(31.3224756056766,-0.763531646934147,
25.3802083333334));
#74042=CARTESIAN_POINT('Ctrl Pts',(31.7633008075689,-1.36198038370242E-14,
25.421875));
#74043=CARTESIAN_POINT('Ctrl Pts',(31.3224756056766,0.763531646934118,25.4635416666667));
#74044=CARTESIAN_POINT('Ctrl Pts',(30.8816504037844,1.52706329386825,25.5052083333334));
#74045=CARTESIAN_POINT('Ctrl Pts',(30.,1.52706329386825,25.546875));
#74046=CARTESIAN_POINT('Ctrl Pts',(29.1183495962155,1.52706329386825,25.5885416666667));
#74047=CARTESIAN_POINT('Ctrl Pts',(28.6775243943233,0.76353164693412,25.6302083333334));
#74048=CARTESIAN_POINT('Ctrl Pts',(28.2366991924311,-1.31894491186926E-14,
25.671875));
#74049=CARTESIAN_POINT('Ctrl Pts',(28.6775243943233,-0.763531646934146,
25.7135416666667));
#74050=CARTESIAN_POINT('Ctrl Pts',(29.1183495962155,-1.52706329386828,25.7552083333334));
#74051=CARTESIAN_POINT('Ctrl Pts',(30.,-1.52706329386828,25.796875));
#74052=CARTESIAN_POINT('Ctrl Pts',(30.8816504037844,-1.52706329386828,25.8385416666667));
#74053=CARTESIAN_POINT('Ctrl Pts',(31.3224756056766,-0.763531646934147,
25.8802083333334));
#74054=CARTESIAN_POINT('Ctrl Pts',(31.7633008075689,-1.36198038370242E-14,
25.921875));
#74055=CARTESIAN_POINT('Ctrl Pts',(31.3224756056766,0.763531646934118,25.9635416666667));
#74056=CARTESIAN_POINT('Ctrl Pts',(30.8816504037844,1.52706329386825,26.0052083333334));
#74057=CARTESIAN_POINT('Ctrl Pts',(30.,1.52706329386825,26.046875));
#74058=CARTESIAN_POINT('Ctrl Pts',(29.1183495962155,1.52706329386825,26.0885416666667));
#74059=CARTESIAN_POINT('Ctrl Pts',(28.6775243943233,0.76353164693412,26.1302083333334));
#74060=CARTESIAN_POINT('Ctrl Pts',(28.2366991924311,-1.31894491186926E-14,
26.171875));
#74061=CARTESIAN_POINT('Ctrl Pts',(28.6775243943233,-0.763531646934146,
26.2135416666667));
#74062=CARTESIAN_POINT('Ctrl Pts',(29.1183495962155,-1.52706329386828,26.2552083333334));
#74063=CARTESIAN_POINT('Ctrl Pts',(30.,-1.52706329386828,26.296875));
#74064=CARTESIAN_POINT('Ctrl Pts',(30.8816504037844,-1.52706329386828,26.3385416666667));
#74065=CARTESIAN_POINT('Ctrl Pts',(31.3224756056766,-0.763531646934147,
26.3802083333334));
#74066=CARTESIAN_POINT('Ctrl Pts',(31.7633008075689,-1.36198038370242E-14,
26.421875));
#74067=CARTESIAN_POINT('Ctrl Pts',(31.3224756056766,0.763531646934118,26.4635416666667));
#74068=CARTESIAN_POINT('Ctrl Pts',(30.8816504037844,1.52706329386825,26.5052083333334));
#74069=CARTESIAN_POINT('Ctrl Pts',(30.,1.52706329386825,26.546875));
#74070=CARTESIAN_POINT('Ctrl Pts',(29.1183495962155,1.52706329386825,26.5885416666667));
#74071=CARTESIAN_POINT('Ctrl Pts',(28.6775243943233,0.76353164693412,26.6302083333334));
#74072=CARTESIAN_POINT('Ctrl Pts',(28.2366991924311,-1.31894491186926E-14,
26.671875));
#74073=CARTESIAN_POINT('Ctrl Pts',(28.6775243943233,-0.763531646934146,
26.7135416666667));
#74074=CARTESIAN_POINT('Ctrl Pts',(29.1183495962155,-1.52706329386828,26.7552083333334));
#74075=CARTESIAN_POINT('Ctrl Pts',(30.,-1.52706329386828,26.796875));
#74076=CARTESIAN_POINT('Ctrl Pts',(30.8816504037844,-1.52706329386828,26.8385416666667));
#74077=CARTESIAN_POINT('Ctrl Pts',(31.3224756056766,-0.763531646934147,
26.8802083333334));
#74078=CARTESIAN_POINT('Ctrl Pts',(31.7633008075689,-1.36198038370242E-14,
26.921875));
#74079=CARTESIAN_POINT('Ctrl Pts',(31.3224756056766,0.763531646934118,26.9635416666667));
#74080=CARTESIAN_POINT('Ctrl Pts',(30.8816504037844,1.52706329386825,27.0052083333334));
#74081=CARTESIAN_POINT('Ctrl Pts',(30.,1.52706329386825,27.046875));
#74082=CARTESIAN_POINT('Ctrl Pts',(29.1183495962155,1.52706329386825,27.0885416666667));
#74083=CARTESIAN_POINT('Ctrl Pts',(28.6775243943233,0.76353164693412,27.1302083333334));
#74084=CARTESIAN_POINT('Ctrl Pts',(28.2366991924311,-1.31894491186926E-14,
27.171875));
#74085=CARTESIAN_POINT('Ctrl Pts',(28.6775243943233,-0.763531646934146,
27.2135416666667));
#74086=CARTESIAN_POINT('Ctrl Pts',(29.1183495962155,-1.52706329386828,27.2552083333334));
#74087=CARTESIAN_POINT('Ctrl Pts',(30.,-1.52706329386828,27.296875));
#74088=CARTESIAN_POINT('Ctrl Pts',(30.8816504037844,-1.52706329386828,27.3385416666667));
#74089=CARTESIAN_POINT('Ctrl Pts',(31.3224756056766,-0.763531646934147,
27.3802083333334));
#74090=CARTESIAN_POINT('Ctrl Pts',(31.7633008075689,-1.36198038370242E-14,
27.421875));
#74091=CARTESIAN_POINT('Ctrl Pts',(31.3224756056766,0.763531646934118,27.4635416666667));
#74092=CARTESIAN_POINT('Ctrl Pts',(30.8816504037844,1.52706329386825,27.5052083333334));
#74093=CARTESIAN_POINT('Ctrl Pts',(30.,1.52706329386825,27.546875));
#74094=CARTESIAN_POINT('Ctrl Pts',(29.1183495962155,1.52706329386825,27.5885416666667));
#74095=CARTESIAN_POINT('Ctrl Pts',(28.6775243943233,0.76353164693412,27.6302083333334));
#74096=CARTESIAN_POINT('Ctrl Pts',(28.2366991924311,-1.31894491186926E-14,
27.671875));
#74097=CARTESIAN_POINT('Ctrl Pts',(28.6775243943233,-0.763531646934146,
27.7135416666667));
#74098=CARTESIAN_POINT('Ctrl Pts',(29.1183495962155,-1.52706329386828,27.7552083333334));
#74099=CARTESIAN_POINT('Ctrl Pts',(30.,-1.52706329386828,27.796875));
#74100=CARTESIAN_POINT('Ctrl Pts',(30.8816504037844,-1.52706329386828,27.8385416666667));
#74101=CARTESIAN_POINT('Ctrl Pts',(31.3224756056766,-0.763531646934147,
27.8802083333334));
#74102=CARTESIAN_POINT('Ctrl Pts',(31.7633008075689,-1.36198038370242E-14,
27.921875));
#74103=CARTESIAN_POINT('Ctrl Pts',(31.3224756056766,0.763531646934118,27.9635416666667));
#74104=CARTESIAN_POINT('Ctrl Pts',(30.8816504037844,1.52706329386825,28.0052083333334));
#74105=CARTESIAN_POINT('Ctrl Pts',(30.,1.52706329386825,28.046875));
#74106=CARTESIAN_POINT('Ctrl Pts',(29.1183495962155,1.52706329386825,28.0885416666667));
#74107=CARTESIAN_POINT('Ctrl Pts',(28.6775243943233,0.76353164693412,28.1302083333334));
#74108=CARTESIAN_POINT('Ctrl Pts',(28.2366991924311,-1.31894491186926E-14,
28.171875));
#74109=CARTESIAN_POINT('Ctrl Pts',(28.6775243943233,-0.763531646934146,
28.2135416666667));
#74110=CARTESIAN_POINT('Ctrl Pts',(29.1183495962155,-1.52706329386828,28.2552083333334));
#74111=CARTESIAN_POINT('Ctrl Pts',(30.,-1.52706329386828,28.296875));
#74112=CARTESIAN_POINT('Ctrl Pts',(30.8816504037844,-1.52706329386828,28.3385416666667));
#74113=CARTESIAN_POINT('Ctrl Pts',(31.3224756056766,-0.763531646934147,
28.3802083333334));
#74114=CARTESIAN_POINT('Ctrl Pts',(31.7633008075689,-1.36198038370242E-14,
28.421875));
#74115=CARTESIAN_POINT('Ctrl Pts',(31.3224756056766,0.763531646934118,28.4635416666667));
#74116=CARTESIAN_POINT('Ctrl Pts',(30.8816504037844,1.52706329386825,28.5052083333334));
#74117=CARTESIAN_POINT('Ctrl Pts',(30.,1.52706329386825,28.546875));
#74118=CARTESIAN_POINT('Ctrl Pts',(29.1183495962155,1.52706329386825,28.5885416666667));
#74119=CARTESIAN_POINT('Ctrl Pts',(28.6775243943233,0.76353164693412,28.6302083333334));
#74120=CARTESIAN_POINT('Ctrl Pts',(28.2366991924311,-1.31894491186926E-14,
28.671875));
#74121=CARTESIAN_POINT('Ctrl Pts',(28.6775243943233,-0.763531646934146,
28.7135416666667));
#74122=CARTESIAN_POINT('Ctrl Pts',(29.1183495962155,-1.52706329386828,28.7552083333334));
#74123=CARTESIAN_POINT('Ctrl Pts',(30.,-1.52706329386828,28.796875));
#74124=CARTESIAN_POINT('Ctrl Pts',(30.8816504037844,-1.52706329386828,28.8385416666667));
#74125=CARTESIAN_POINT('Ctrl Pts',(31.3224756056766,-0.763531646934147,
28.8802083333334));
#74126=CARTESIAN_POINT('Ctrl Pts',(31.7633008075689,-1.36198038370242E-14,
28.921875));
#74127=CARTESIAN_POINT('Ctrl Pts',(31.3224756056766,0.763531646934118,28.9635416666667));
#74128=CARTESIAN_POINT('Ctrl Pts',(30.8816504037844,1.52706329386825,29.0052083333334));
#74129=CARTESIAN_POINT('Ctrl Pts',(30.,1.52706329386825,29.046875));
#74130=CARTESIAN_POINT('Ctrl Pts',(29.1183495962155,1.52706329386825,29.0885416666667));
#74131=CARTESIAN_POINT('Ctrl Pts',(28.6775243943233,0.76353164693412,29.1302083333334));
#74132=CARTESIAN_POINT('Ctrl Pts',(28.2366991924311,-1.31894491186926E-14,
29.171875));
#74133=CARTESIAN_POINT('Ctrl Pts',(28.6775243943233,-0.763531646934146,
29.2135416666667));
#74134=CARTESIAN_POINT('Ctrl Pts',(29.1183495962155,-1.52706329386828,29.2552083333334));
#74135=CARTESIAN_POINT('Ctrl Pts',(30.,-1.52706329386828,29.296875));
#74136=CARTESIAN_POINT('Ctrl Pts',(30.8816504037844,-1.52706329386828,29.3385416666667));
#74137=CARTESIAN_POINT('Ctrl Pts',(31.3224756056766,-0.763531646934147,
29.3802083333334));
#74138=CARTESIAN_POINT('Ctrl Pts',(31.7633008075689,-1.36198038370242E-14,
29.421875));
#74139=CARTESIAN_POINT('Ctrl Pts',(31.3224756056766,0.763531646934118,29.4635416666667));
#74140=CARTESIAN_POINT('Ctrl Pts',(30.8816504037844,1.52706329386825,29.5052083333334));
#74141=CARTESIAN_POINT('Ctrl Pts',(30.,1.52706329386825,29.546875));
#74142=CARTESIAN_POINT('Ctrl Pts',(29.1183495962155,1.52706329386825,29.5885416666667));
#74143=CARTESIAN_POINT('Ctrl Pts',(28.6775243943233,0.76353164693412,29.6302083333334));
#74144=CARTESIAN_POINT('Ctrl Pts',(28.2366991924311,-1.31894491186926E-14,
29.671875));
#74145=CARTESIAN_POINT('Ctrl Pts',(28.6775243943233,-0.763531646934146,
29.7135416666667));
#74146=CARTESIAN_POINT('Ctrl Pts',(29.1183495962155,-1.52706329386828,29.7552083333334));
#74147=CARTESIAN_POINT('Ctrl Pts',(30.,-1.52706329386828,29.796875));
#74148=CARTESIAN_POINT('Ctrl Pts',(30.8816504037844,-1.52706329386828,29.8385416666667));
#74149=CARTESIAN_POINT('Ctrl Pts',(31.3224756056766,-0.763531646934147,
29.8802083333334));
#74150=CARTESIAN_POINT('Ctrl Pts',(31.7633008075689,-1.36198038370242E-14,
29.921875));
#74151=CARTESIAN_POINT('Ctrl Pts',(31.3224756056766,0.763531646934118,29.9635416666667));
#74152=CARTESIAN_POINT('Ctrl Pts',(30.8816504037844,1.52706329386825,30.0052083333334));
#74153=CARTESIAN_POINT('Ctrl Pts',(30.,1.52706329386825,30.046875));
#74154=CARTESIAN_POINT('Ctrl Pts',(29.1183495962155,1.52706329386825,30.0885416666667));
#74155=CARTESIAN_POINT('Ctrl Pts',(28.6775243943233,0.76353164693412,30.1302083333334));
#74156=CARTESIAN_POINT('Ctrl Pts',(28.2366991924311,-1.31894491186926E-14,
30.171875));
#74157=CARTESIAN_POINT('Ctrl Pts',(28.6775243943233,-0.763531646934146,
30.2135416666667));
#74158=CARTESIAN_POINT('Ctrl Pts',(29.1183495962155,-1.52706329386828,30.2552083333334));
#74159=CARTESIAN_POINT('Ctrl Pts',(30.,-1.52706329386828,30.296875));
#74160=CARTESIAN_POINT('Ctrl Pts',(30.8816504037844,-1.52706329386828,30.3385416666667));
#74161=CARTESIAN_POINT('Ctrl Pts',(31.3224756056766,-0.763531646934147,
30.3802083333334));
#74162=CARTESIAN_POINT('Ctrl Pts',(31.7633008075689,-1.36198038370242E-14,
30.421875));
#74163=CARTESIAN_POINT('Ctrl Pts',(31.3224756056766,0.763531646934118,30.4635416666667));
#74164=CARTESIAN_POINT('Ctrl Pts',(30.8816504037844,1.52706329386825,30.5052083333334));
#74165=CARTESIAN_POINT('Ctrl Pts',(30.,1.52706329386825,30.546875));
#74166=CARTESIAN_POINT('Ctrl Pts',(29.1183495962155,1.52706329386825,30.5885416666667));
#74167=CARTESIAN_POINT('Ctrl Pts',(28.6775243943233,0.76353164693412,30.6302083333334));
#74168=CARTESIAN_POINT('Ctrl Pts',(28.2366991924311,-1.31894491186926E-14,
30.671875));
#74169=CARTESIAN_POINT('Ctrl Pts',(28.6775243943233,-0.763531646934146,
30.7135416666667));
#74170=CARTESIAN_POINT('Ctrl Pts',(29.1183495962155,-1.52706329386828,30.7552083333334));
#74171=CARTESIAN_POINT('Ctrl Pts',(30.,-1.52706329386828,30.796875));
#74172=CARTESIAN_POINT('Ctrl Pts',(30.8816504037844,-1.52706329386828,30.8385416666667));
#74173=CARTESIAN_POINT('Ctrl Pts',(31.3224756056766,-0.763531646934147,
30.8802083333334));
#74174=CARTESIAN_POINT('Ctrl Pts',(31.7633008075689,-1.36198038370242E-14,
30.921875));
#74175=CARTESIAN_POINT('Ctrl Pts',(31.3224756056766,0.763531646934118,30.9635416666667));
#74176=CARTESIAN_POINT('Ctrl Pts',(30.8816504037844,1.52706329386825,31.0052083333334));
#74177=CARTESIAN_POINT('Ctrl Pts',(30.,1.52706329386825,31.046875));
#74178=CARTESIAN_POINT('Ctrl Pts',(30.8234003400376,-0.838570603170131,
30.5624996575278));
#74179=CARTESIAN_POINT('Ctrl Pts',(30.9252409219315,-0.749808119816165,
30.5671289662449));
#74180=CARTESIAN_POINT('Ctrl Pts',(31.0094069192668,-0.645130506686946,
30.571193014068));
#74181=CARTESIAN_POINT('Ctrl Pts',(31.1396529784097,-0.412074319923831,
30.5795221820465));
#74182=CARTESIAN_POINT('Ctrl Pts',(31.1849584507844,-0.287685440765051,
30.5838904393726));
#74183=CARTESIAN_POINT('Ctrl Pts',(31.2386945750578,-0.00655181811616603,
30.5935664195233));
#74184=CARTESIAN_POINT('Ctrl Pts',(31.2387490550162,0.149503133824081,30.5988162542928));
#74185=CARTESIAN_POINT('Ctrl Pts',(31.1719223736106,0.500568259068406,30.610386374166));
#74186=CARTESIAN_POINT('Ctrl Pts',(31.0923154827319,0.652496494934345,30.6150433766711));
#74187=CARTESIAN_POINT('Ctrl Pts',(30.9283336729762,0.900293879400657,30.6239504439807));
#74188=CARTESIAN_POINT('Ctrl Pts',(30.8055598520391,1.02369588322745,30.6294622341334));
#74189=CARTESIAN_POINT('Ctrl Pts',(30.5288337282237,1.20882504193349,30.6401101417162));
#74190=CARTESIAN_POINT('Ctrl Pts',(30.3799906896905,1.27260041719159,30.6451552807199));
#74191=CARTESIAN_POINT('Ctrl Pts',(30.0014927028803,1.35728019461807,30.6565651904367));
#74192=CARTESIAN_POINT('Ctrl Pts',(29.8132785668206,1.33887636851719,30.6613880776071));
#74193=CARTESIAN_POINT('Ctrl Pts',(29.5198061598154,1.28660005614596,30.6701589170659));
#74194=CARTESIAN_POINT('Ctrl Pts',(29.3521505621284,1.22147978200258,30.6756096035631));
#74195=CARTESIAN_POINT('Ctrl Pts',(29.0485837866741,1.02916361274227,30.6863949411503));
#74196=CARTESIAN_POINT('Ctrl Pts',(28.9162494293832,0.902843317652004,30.6916208752244));
#74197=CARTESIAN_POINT('Ctrl Pts',(28.7272437086822,0.633185410868888,30.7002552651022));
#74198=CARTESIAN_POINT('Ctrl Pts',(28.6461891944724,0.476094037694283,30.7048351996635));
#74199=CARTESIAN_POINT('Ctrl Pts',(28.551105022901,0.105569064666544,30.715730913862));
#74200=CARTESIAN_POINT('Ctrl Pts',(28.5402826505383,-0.0831493783931786,
30.7211721595761));
#74201=CARTESIAN_POINT('Ctrl Pts',(28.5859138822382,-0.415083694084825,
30.7305650693331));
#74202=CARTESIAN_POINT('Ctrl Pts',(28.6283908398168,-0.557537406078615,
30.7345346397522));
#74203=CARTESIAN_POINT('Ctrl Pts',(28.7447696187018,-0.802908073480822,
30.7412906353098));
#74204=CARTESIAN_POINT('Ctrl Pts',(28.8264704242263,-0.938163811130005,
30.7451577422722));
#74205=CARTESIAN_POINT('Ctrl Pts',(28.9490560961683,-1.07028823734174,30.7500000000014));
#74206=CARTESIAN_POINT('Ctrl Pts',(30.,1.52706329386825,16.015625));
#74207=CARTESIAN_POINT('Ctrl Pts',(29.1183495962155,1.52706329386825,16.0572916666666));
#74208=CARTESIAN_POINT('Ctrl Pts',(28.6775243943233,0.76353164693412,16.0989583333333));
#74209=CARTESIAN_POINT('Ctrl Pts',(28.2366991924311,-1.31894491186926E-14,
16.140625));
#74210=CARTESIAN_POINT('Ctrl Pts',(28.6775243943233,-0.763531646934146,
16.1822916666666));
#74211=CARTESIAN_POINT('Ctrl Pts',(29.1183495962155,-1.52706329386828,16.2239583333333));
#74212=CARTESIAN_POINT('Ctrl Pts',(30.,-1.52706329386828,16.265625));
#74213=CARTESIAN_POINT('Ctrl Pts',(30.8816504037844,-1.52706329386828,16.3072916666666));
#74214=CARTESIAN_POINT('Ctrl Pts',(31.3224756056766,-0.763531646934147,
16.3489583333333));
#74215=CARTESIAN_POINT('Ctrl Pts',(31.7633008075689,-1.36198038370242E-14,
16.390625));
#74216=CARTESIAN_POINT('Ctrl Pts',(31.3224756056766,0.763531646934118,16.4322916666666));
#74217=CARTESIAN_POINT('Ctrl Pts',(30.8816504037844,1.52706329386825,16.4739583333333));
#74218=CARTESIAN_POINT('Ctrl Pts',(30.,1.52706329386825,16.515625));
#74219=CARTESIAN_POINT('Ctrl Pts',(29.1183495962155,1.52706329386825,16.5572916666666));
#74220=CARTESIAN_POINT('Ctrl Pts',(28.6775243943233,0.76353164693412,16.5989583333333));
#74221=CARTESIAN_POINT('Ctrl Pts',(28.2366991924311,-1.31894491186926E-14,
16.640625));
#74222=CARTESIAN_POINT('Ctrl Pts',(28.6775243943233,-0.763531646934146,
16.6822916666666));
#74223=CARTESIAN_POINT('Ctrl Pts',(29.1183495962155,-1.52706329386828,16.7239583333333));
#74224=CARTESIAN_POINT('Ctrl Pts',(30.,-1.52706329386828,16.765625));
#74225=CARTESIAN_POINT('Ctrl Pts',(30.8816504037844,-1.52706329386828,16.8072916666666));
#74226=CARTESIAN_POINT('Ctrl Pts',(31.3224756056766,-0.763531646934147,
16.8489583333333));
#74227=CARTESIAN_POINT('Ctrl Pts',(31.7633008075689,-1.36198038370242E-14,
16.890625));
#74228=CARTESIAN_POINT('Ctrl Pts',(31.3224756056766,0.763531646934118,16.9322916666666));
#74229=CARTESIAN_POINT('Ctrl Pts',(30.8816504037844,1.52706329386825,16.9739583333333));
#74230=CARTESIAN_POINT('Ctrl Pts',(30.,1.52706329386825,17.015625));
#74231=CARTESIAN_POINT('Ctrl Pts',(29.1183495962155,1.52706329386825,17.0572916666666));
#74232=CARTESIAN_POINT('Ctrl Pts',(28.6775243943233,0.76353164693412,17.0989583333333));
#74233=CARTESIAN_POINT('Ctrl Pts',(28.2366991924311,-1.31894491186926E-14,
17.140625));
#74234=CARTESIAN_POINT('Ctrl Pts',(28.6775243943233,-0.763531646934146,
17.1822916666666));
#74235=CARTESIAN_POINT('Ctrl Pts',(29.1183495962155,-1.52706329386828,17.2239583333333));
#74236=CARTESIAN_POINT('Ctrl Pts',(30.,-1.52706329386828,17.265625));
#74237=CARTESIAN_POINT('Ctrl Pts',(30.8816504037844,-1.52706329386828,17.3072916666666));
#74238=CARTESIAN_POINT('Ctrl Pts',(31.3224756056766,-0.763531646934147,
17.3489583333333));
#74239=CARTESIAN_POINT('Ctrl Pts',(31.7633008075689,-1.36198038370242E-14,
17.390625));
#74240=CARTESIAN_POINT('Ctrl Pts',(31.3224756056766,0.763531646934118,17.4322916666666));
#74241=CARTESIAN_POINT('Ctrl Pts',(30.8816504037844,1.52706329386825,17.4739583333333));
#74242=CARTESIAN_POINT('Ctrl Pts',(30.,1.52706329386825,17.515625));
#74243=CARTESIAN_POINT('Ctrl Pts',(29.1183495962155,1.52706329386825,17.5572916666666));
#74244=CARTESIAN_POINT('Ctrl Pts',(28.6775243943233,0.76353164693412,17.5989583333333));
#74245=CARTESIAN_POINT('Ctrl Pts',(28.2366991924311,-1.31894491186926E-14,
17.640625));
#74246=CARTESIAN_POINT('Ctrl Pts',(28.6775243943233,-0.763531646934146,
17.6822916666666));
#74247=CARTESIAN_POINT('Ctrl Pts',(29.1183495962155,-1.52706329386828,17.7239583333333));
#74248=CARTESIAN_POINT('Ctrl Pts',(30.,-1.52706329386828,17.765625));
#74249=CARTESIAN_POINT('Ctrl Pts',(30.8816504037844,-1.52706329386828,17.8072916666666));
#74250=CARTESIAN_POINT('Ctrl Pts',(31.3224756056766,-0.763531646934147,
17.8489583333333));
#74251=CARTESIAN_POINT('Ctrl Pts',(31.7633008075689,-1.36198038370242E-14,
17.890625));
#74252=CARTESIAN_POINT('Ctrl Pts',(31.3224756056766,0.763531646934118,17.9322916666666));
#74253=CARTESIAN_POINT('Ctrl Pts',(30.8816504037844,1.52706329386825,17.9739583333333));
#74254=CARTESIAN_POINT('Ctrl Pts',(30.,1.52706329386825,18.015625));
#74255=CARTESIAN_POINT('Ctrl Pts',(29.1183495962155,1.52706329386825,18.0572916666666));
#74256=CARTESIAN_POINT('Ctrl Pts',(28.6775243943233,0.76353164693412,18.0989583333333));
#74257=CARTESIAN_POINT('Ctrl Pts',(28.2366991924311,-1.31894491186926E-14,
18.140625));
#74258=CARTESIAN_POINT('Ctrl Pts',(28.6775243943233,-0.763531646934146,
18.1822916666666));
#74259=CARTESIAN_POINT('Ctrl Pts',(29.1183495962155,-1.52706329386828,18.2239583333333));
#74260=CARTESIAN_POINT('Ctrl Pts',(30.,-1.52706329386828,18.265625));
#74261=CARTESIAN_POINT('Ctrl Pts',(30.8816504037844,-1.52706329386828,18.3072916666666));
#74262=CARTESIAN_POINT('Ctrl Pts',(31.3224756056766,-0.763531646934147,
18.3489583333333));
#74263=CARTESIAN_POINT('Ctrl Pts',(31.7633008075689,-1.36198038370242E-14,
18.390625));
#74264=CARTESIAN_POINT('Ctrl Pts',(31.3224756056766,0.763531646934118,18.4322916666666));
#74265=CARTESIAN_POINT('Ctrl Pts',(30.8816504037844,1.52706329386825,18.4739583333333));
#74266=CARTESIAN_POINT('Ctrl Pts',(30.,1.52706329386825,18.515625));
#74267=CARTESIAN_POINT('Ctrl Pts',(29.1183495962155,1.52706329386825,18.5572916666666));
#74268=CARTESIAN_POINT('Ctrl Pts',(28.6775243943233,0.76353164693412,18.5989583333333));
#74269=CARTESIAN_POINT('Ctrl Pts',(28.2366991924311,-1.31894491186926E-14,
18.640625));
#74270=CARTESIAN_POINT('Ctrl Pts',(28.6775243943233,-0.763531646934146,
18.6822916666666));
#74271=CARTESIAN_POINT('Ctrl Pts',(29.1183495962155,-1.52706329386828,18.7239583333333));
#74272=CARTESIAN_POINT('Ctrl Pts',(30.,-1.52706329386828,18.765625));
#74273=CARTESIAN_POINT('Ctrl Pts',(30.8816504037844,-1.52706329386828,18.8072916666666));
#74274=CARTESIAN_POINT('Ctrl Pts',(31.3224756056766,-0.763531646934147,
18.8489583333333));
#74275=CARTESIAN_POINT('Ctrl Pts',(31.7633008075689,-1.36198038370242E-14,
18.890625));
#74276=CARTESIAN_POINT('Ctrl Pts',(31.3224756056766,0.763531646934118,18.9322916666666));
#74277=CARTESIAN_POINT('Ctrl Pts',(30.8816504037844,1.52706329386825,18.9739583333333));
#74278=CARTESIAN_POINT('Ctrl Pts',(30.,1.52706329386825,19.015625));
#74279=CARTESIAN_POINT('Ctrl Pts',(29.1183495962155,1.52706329386825,19.0572916666666));
#74280=CARTESIAN_POINT('Ctrl Pts',(28.6775243943233,0.76353164693412,19.0989583333333));
#74281=CARTESIAN_POINT('Ctrl Pts',(28.2366991924311,-1.31894491186926E-14,
19.140625));
#74282=CARTESIAN_POINT('Ctrl Pts',(28.6775243943233,-0.763531646934146,
19.1822916666666));
#74283=CARTESIAN_POINT('Ctrl Pts',(29.1183495962155,-1.52706329386828,19.2239583333333));
#74284=CARTESIAN_POINT('Ctrl Pts',(30.,-1.52706329386828,19.265625));
#74285=CARTESIAN_POINT('Ctrl Pts',(30.8816504037844,-1.52706329386828,19.3072916666666));
#74286=CARTESIAN_POINT('Ctrl Pts',(31.3224756056766,-0.763531646934147,
19.3489583333333));
#74287=CARTESIAN_POINT('Ctrl Pts',(31.7633008075689,-1.36198038370242E-14,
19.390625));
#74288=CARTESIAN_POINT('Ctrl Pts',(31.3224756056766,0.763531646934118,19.4322916666666));
#74289=CARTESIAN_POINT('Ctrl Pts',(30.8816504037844,1.52706329386825,19.4739583333333));
#74290=CARTESIAN_POINT('Ctrl Pts',(30.,1.52706329386825,19.515625));
#74291=CARTESIAN_POINT('Ctrl Pts',(29.1183495962155,1.52706329386825,19.5572916666666));
#74292=CARTESIAN_POINT('Ctrl Pts',(28.6775243943233,0.76353164693412,19.5989583333333));
#74293=CARTESIAN_POINT('Ctrl Pts',(28.2366991924311,-1.31894491186926E-14,
19.640625));
#74294=CARTESIAN_POINT('Ctrl Pts',(28.6775243943233,-0.763531646934146,
19.6822916666666));
#74295=CARTESIAN_POINT('Ctrl Pts',(29.1183495962155,-1.52706329386828,19.7239583333333));
#74296=CARTESIAN_POINT('Ctrl Pts',(30.,-1.52706329386828,19.765625));
#74297=CARTESIAN_POINT('Ctrl Pts',(30.8816504037844,-1.52706329386828,19.8072916666666));
#74298=CARTESIAN_POINT('Ctrl Pts',(31.3224756056766,-0.763531646934147,
19.8489583333333));
#74299=CARTESIAN_POINT('Ctrl Pts',(31.7633008075689,-1.36198038370242E-14,
19.890625));
#74300=CARTESIAN_POINT('Ctrl Pts',(31.3224756056766,0.763531646934118,19.9322916666666));
#74301=CARTESIAN_POINT('Ctrl Pts',(30.8816504037844,1.52706329386825,19.9739583333333));
#74302=CARTESIAN_POINT('Ctrl Pts',(30.,1.52706329386825,20.015625));
#74303=CARTESIAN_POINT('Ctrl Pts',(29.1183495962155,1.52706329386825,20.0572916666666));
#74304=CARTESIAN_POINT('Ctrl Pts',(28.6775243943233,0.76353164693412,20.0989583333333));
#74305=CARTESIAN_POINT('Ctrl Pts',(28.2366991924311,-1.31894491186926E-14,
20.140625));
#74306=CARTESIAN_POINT('Ctrl Pts',(28.6775243943233,-0.763531646934146,
20.1822916666666));
#74307=CARTESIAN_POINT('Ctrl Pts',(29.1183495962155,-1.52706329386828,20.2239583333333));
#74308=CARTESIAN_POINT('Ctrl Pts',(30.,-1.52706329386828,20.265625));
#74309=CARTESIAN_POINT('Ctrl Pts',(30.8816504037844,-1.52706329386828,20.3072916666666));
#74310=CARTESIAN_POINT('Ctrl Pts',(31.3224756056766,-0.763531646934147,
20.3489583333333));
#74311=CARTESIAN_POINT('Ctrl Pts',(31.7633008075689,-1.36198038370242E-14,
20.390625));
#74312=CARTESIAN_POINT('Ctrl Pts',(31.3224756056766,0.763531646934118,20.4322916666666));
#74313=CARTESIAN_POINT('Ctrl Pts',(30.8816504037844,1.52706329386825,20.4739583333333));
#74314=CARTESIAN_POINT('Ctrl Pts',(30.,1.52706329386825,20.515625));
#74315=CARTESIAN_POINT('Ctrl Pts',(29.1183495962155,1.52706329386825,20.5572916666666));
#74316=CARTESIAN_POINT('Ctrl Pts',(28.6775243943233,0.76353164693412,20.5989583333333));
#74317=CARTESIAN_POINT('Ctrl Pts',(28.2366991924311,-1.31894491186926E-14,
20.640625));
#74318=CARTESIAN_POINT('Ctrl Pts',(28.6775243943233,-0.763531646934146,
20.6822916666666));
#74319=CARTESIAN_POINT('Ctrl Pts',(29.1183495962155,-1.52706329386828,20.7239583333333));
#74320=CARTESIAN_POINT('Ctrl Pts',(30.,-1.52706329386828,20.765625));
#74321=CARTESIAN_POINT('Ctrl Pts',(30.8816504037844,-1.52706329386828,20.8072916666666));
#74322=CARTESIAN_POINT('Ctrl Pts',(31.3224756056766,-0.763531646934147,
20.8489583333333));
#74323=CARTESIAN_POINT('Ctrl Pts',(31.7633008075689,-1.36198038370242E-14,
20.890625));
#74324=CARTESIAN_POINT('Ctrl Pts',(31.3224756056766,0.763531646934118,20.9322916666666));
#74325=CARTESIAN_POINT('Ctrl Pts',(30.8816504037844,1.52706329386825,20.9739583333333));
#74326=CARTESIAN_POINT('Ctrl Pts',(30.,1.52706329386825,21.015625));
#74327=CARTESIAN_POINT('Ctrl Pts',(29.1183495962155,1.52706329386825,21.0572916666666));
#74328=CARTESIAN_POINT('Ctrl Pts',(28.6775243943233,0.76353164693412,21.0989583333333));
#74329=CARTESIAN_POINT('Ctrl Pts',(28.2366991924311,-1.31894491186926E-14,
21.140625));
#74330=CARTESIAN_POINT('Ctrl Pts',(28.6775243943233,-0.763531646934146,
21.1822916666666));
#74331=CARTESIAN_POINT('Ctrl Pts',(29.1183495962155,-1.52706329386828,21.2239583333333));
#74332=CARTESIAN_POINT('Ctrl Pts',(30.,-1.52706329386828,21.265625));
#74333=CARTESIAN_POINT('Ctrl Pts',(30.8816504037844,-1.52706329386828,21.3072916666666));
#74334=CARTESIAN_POINT('Ctrl Pts',(31.3224756056766,-0.763531646934147,
21.3489583333333));
#74335=CARTESIAN_POINT('Ctrl Pts',(31.7633008075689,-1.36198038370242E-14,
21.390625));
#74336=CARTESIAN_POINT('Ctrl Pts',(31.3224756056766,0.763531646934118,21.4322916666666));
#74337=CARTESIAN_POINT('Ctrl Pts',(30.8816504037844,1.52706329386825,21.4739583333333));
#74338=CARTESIAN_POINT('Ctrl Pts',(30.,1.52706329386825,21.515625));
#74339=CARTESIAN_POINT('Ctrl Pts',(29.1183495962155,1.52706329386825,21.5572916666666));
#74340=CARTESIAN_POINT('Ctrl Pts',(28.6775243943233,0.76353164693412,21.5989583333333));
#74341=CARTESIAN_POINT('Ctrl Pts',(28.2366991924311,-1.31894491186926E-14,
21.640625));
#74342=CARTESIAN_POINT('Ctrl Pts',(28.6775243943233,-0.763531646934146,
21.6822916666666));
#74343=CARTESIAN_POINT('Ctrl Pts',(29.1183495962155,-1.52706329386828,21.7239583333333));
#74344=CARTESIAN_POINT('Ctrl Pts',(30.,-1.52706329386828,21.765625));
#74345=CARTESIAN_POINT('Ctrl Pts',(30.8816504037844,-1.52706329386828,21.8072916666666));
#74346=CARTESIAN_POINT('Ctrl Pts',(31.3224756056766,-0.763531646934147,
21.8489583333333));
#74347=CARTESIAN_POINT('Ctrl Pts',(31.7633008075689,-1.36198038370242E-14,
21.890625));
#74348=CARTESIAN_POINT('Ctrl Pts',(31.3224756056766,0.763531646934118,21.9322916666666));
#74349=CARTESIAN_POINT('Ctrl Pts',(30.8816504037844,1.52706329386825,21.9739583333333));
#74350=CARTESIAN_POINT('Ctrl Pts',(30.,1.52706329386825,22.015625));
#74351=CARTESIAN_POINT('Ctrl Pts',(29.1183495962155,1.52706329386825,22.0572916666666));
#74352=CARTESIAN_POINT('Ctrl Pts',(28.6775243943233,0.76353164693412,22.0989583333333));
#74353=CARTESIAN_POINT('Ctrl Pts',(28.2366991924311,-1.31894491186926E-14,
22.140625));
#74354=CARTESIAN_POINT('Ctrl Pts',(28.6775243943233,-0.763531646934146,
22.1822916666666));
#74355=CARTESIAN_POINT('Ctrl Pts',(29.1183495962155,-1.52706329386828,22.2239583333333));
#74356=CARTESIAN_POINT('Ctrl Pts',(30.,-1.52706329386828,22.265625));
#74357=CARTESIAN_POINT('Ctrl Pts',(30.8816504037844,-1.52706329386828,22.3072916666666));
#74358=CARTESIAN_POINT('Ctrl Pts',(31.3224756056766,-0.763531646934147,
22.3489583333333));
#74359=CARTESIAN_POINT('Ctrl Pts',(31.7633008075689,-1.36198038370242E-14,
22.390625));
#74360=CARTESIAN_POINT('Ctrl Pts',(31.3224756056766,0.763531646934118,22.4322916666666));
#74361=CARTESIAN_POINT('Ctrl Pts',(30.8816504037844,1.52706329386825,22.4739583333333));
#74362=CARTESIAN_POINT('Ctrl Pts',(30.,1.52706329386825,22.515625));
#74363=CARTESIAN_POINT('Ctrl Pts',(29.1183495962155,1.52706329386825,22.5572916666666));
#74364=CARTESIAN_POINT('Ctrl Pts',(28.6775243943233,0.76353164693412,22.5989583333333));
#74365=CARTESIAN_POINT('Ctrl Pts',(28.2366991924311,-1.31894491186926E-14,
22.640625));
#74366=CARTESIAN_POINT('Ctrl Pts',(28.6775243943233,-0.763531646934146,
22.6822916666666));
#74367=CARTESIAN_POINT('Ctrl Pts',(29.1183495962155,-1.52706329386828,22.7239583333333));
#74368=CARTESIAN_POINT('Ctrl Pts',(30.,-1.52706329386828,22.765625));
#74369=CARTESIAN_POINT('Ctrl Pts',(30.8816504037844,-1.52706329386828,22.8072916666666));
#74370=CARTESIAN_POINT('Ctrl Pts',(31.3224756056766,-0.763531646934147,
22.8489583333333));
#74371=CARTESIAN_POINT('Ctrl Pts',(31.7633008075689,-1.36198038370242E-14,
22.890625));
#74372=CARTESIAN_POINT('Ctrl Pts',(31.3224756056766,0.763531646934118,22.9322916666666));
#74373=CARTESIAN_POINT('Ctrl Pts',(30.8816504037844,1.52706329386825,22.9739583333333));
#74374=CARTESIAN_POINT('Ctrl Pts',(30.,1.52706329386825,23.015625));
#74375=CARTESIAN_POINT('Ctrl Pts',(29.1183495962155,1.52706329386825,23.0572916666666));
#74376=CARTESIAN_POINT('Ctrl Pts',(28.6775243943233,0.76353164693412,23.0989583333333));
#74377=CARTESIAN_POINT('Ctrl Pts',(28.2366991924311,-1.31894491186926E-14,
23.140625));
#74378=CARTESIAN_POINT('Ctrl Pts',(28.6775243943233,-0.763531646934146,
23.1822916666666));
#74379=CARTESIAN_POINT('Ctrl Pts',(29.1183495962155,-1.52706329386828,23.2239583333333));
#74380=CARTESIAN_POINT('Ctrl Pts',(30.,-1.52706329386828,23.265625));
#74381=CARTESIAN_POINT('Ctrl Pts',(30.8816504037844,-1.52706329386828,23.3072916666666));
#74382=CARTESIAN_POINT('Ctrl Pts',(31.3224756056766,-0.763531646934147,
23.3489583333333));
#74383=CARTESIAN_POINT('Ctrl Pts',(31.7633008075689,-1.36198038370242E-14,
23.390625));
#74384=CARTESIAN_POINT('Ctrl Pts',(31.3224756056766,0.763531646934118,23.4322916666666));
#74385=CARTESIAN_POINT('Ctrl Pts',(30.8816504037844,1.52706329386825,23.4739583333333));
#74386=CARTESIAN_POINT('Ctrl Pts',(30.,1.52706329386825,23.515625));
#74387=CARTESIAN_POINT('Ctrl Pts',(29.1183495962155,1.52706329386825,23.5572916666666));
#74388=CARTESIAN_POINT('Ctrl Pts',(28.6775243943233,0.76353164693412,23.5989583333333));
#74389=CARTESIAN_POINT('Ctrl Pts',(28.2366991924311,-1.31894491186926E-14,
23.640625));
#74390=CARTESIAN_POINT('Ctrl Pts',(28.6775243943233,-0.763531646934146,
23.6822916666666));
#74391=CARTESIAN_POINT('Ctrl Pts',(29.1183495962155,-1.52706329386828,23.7239583333333));
#74392=CARTESIAN_POINT('Ctrl Pts',(30.,-1.52706329386828,23.765625));
#74393=CARTESIAN_POINT('Ctrl Pts',(30.8816504037844,-1.52706329386828,23.8072916666666));
#74394=CARTESIAN_POINT('Ctrl Pts',(31.3224756056766,-0.763531646934147,
23.8489583333333));
#74395=CARTESIAN_POINT('Ctrl Pts',(31.7633008075689,-1.36198038370242E-14,
23.890625));
#74396=CARTESIAN_POINT('Ctrl Pts',(31.3224756056766,0.763531646934118,23.9322916666666));
#74397=CARTESIAN_POINT('Ctrl Pts',(30.8816504037844,1.52706329386825,23.9739583333333));
#74398=CARTESIAN_POINT('Ctrl Pts',(30.,1.52706329386825,24.015625));
#74399=CARTESIAN_POINT('Ctrl Pts',(29.1183495962155,1.52706329386825,24.0572916666666));
#74400=CARTESIAN_POINT('Ctrl Pts',(28.6775243943233,0.76353164693412,24.0989583333333));
#74401=CARTESIAN_POINT('Ctrl Pts',(28.2366991924311,-1.31894491186926E-14,
24.140625));
#74402=CARTESIAN_POINT('Ctrl Pts',(28.6775243943233,-0.763531646934146,
24.1822916666666));
#74403=CARTESIAN_POINT('Ctrl Pts',(29.1183495962155,-1.52706329386828,24.2239583333333));
#74404=CARTESIAN_POINT('Ctrl Pts',(30.,-1.52706329386828,24.265625));
#74405=CARTESIAN_POINT('Ctrl Pts',(30.8816504037844,-1.52706329386828,24.3072916666666));
#74406=CARTESIAN_POINT('Ctrl Pts',(31.3224756056766,-0.763531646934147,
24.3489583333333));
#74407=CARTESIAN_POINT('Ctrl Pts',(31.7633008075689,-1.36198038370242E-14,
24.390625));
#74408=CARTESIAN_POINT('Ctrl Pts',(31.3224756056766,0.763531646934118,24.4322916666666));
#74409=CARTESIAN_POINT('Ctrl Pts',(30.8816504037844,1.52706329386825,24.4739583333333));
#74410=CARTESIAN_POINT('Ctrl Pts',(30.,1.52706329386825,24.515625));
#74411=CARTESIAN_POINT('Ctrl Pts',(29.1183495962155,1.52706329386825,24.5572916666666));
#74412=CARTESIAN_POINT('Ctrl Pts',(28.6775243943233,0.76353164693412,24.5989583333333));
#74413=CARTESIAN_POINT('Ctrl Pts',(28.2366991924311,-1.31894491186926E-14,
24.640625));
#74414=CARTESIAN_POINT('Ctrl Pts',(28.6775243943233,-0.763531646934146,
24.6822916666666));
#74415=CARTESIAN_POINT('Ctrl Pts',(29.1183495962155,-1.52706329386828,24.7239583333333));
#74416=CARTESIAN_POINT('Ctrl Pts',(30.,-1.52706329386828,24.765625));
#74417=CARTESIAN_POINT('Ctrl Pts',(30.8816504037844,-1.52706329386828,24.8072916666666));
#74418=CARTESIAN_POINT('Ctrl Pts',(31.3224756056766,-0.763531646934147,
24.8489583333333));
#74419=CARTESIAN_POINT('Ctrl Pts',(31.7633008075689,-1.36198038370242E-14,
24.890625));
#74420=CARTESIAN_POINT('Ctrl Pts',(31.3224756056766,0.763531646934118,24.9322916666666));
#74421=CARTESIAN_POINT('Ctrl Pts',(30.8816504037844,1.52706329386825,24.9739583333333));
#74422=CARTESIAN_POINT('Ctrl Pts',(30.,1.52706329386825,25.015625));
#74423=CARTESIAN_POINT('Ctrl Pts',(29.1183495962155,1.52706329386825,25.0572916666666));
#74424=CARTESIAN_POINT('Ctrl Pts',(28.6775243943233,0.76353164693412,25.0989583333333));
#74425=CARTESIAN_POINT('Ctrl Pts',(28.2366991924311,-1.31894491186926E-14,
25.140625));
#74426=CARTESIAN_POINT('Ctrl Pts',(28.6775243943233,-0.763531646934146,
25.1822916666666));
#74427=CARTESIAN_POINT('Ctrl Pts',(29.1183495962155,-1.52706329386828,25.2239583333333));
#74428=CARTESIAN_POINT('Ctrl Pts',(30.,-1.52706329386828,25.265625));
#74429=CARTESIAN_POINT('Ctrl Pts',(30.8816504037844,-1.52706329386828,25.3072916666666));
#74430=CARTESIAN_POINT('Ctrl Pts',(31.3224756056766,-0.763531646934147,
25.3489583333333));
#74431=CARTESIAN_POINT('Ctrl Pts',(31.7633008075689,-1.36198038370242E-14,
25.390625));
#74432=CARTESIAN_POINT('Ctrl Pts',(31.3224756056766,0.763531646934118,25.4322916666666));
#74433=CARTESIAN_POINT('Ctrl Pts',(30.8816504037844,1.52706329386825,25.4739583333333));
#74434=CARTESIAN_POINT('Ctrl Pts',(30.,1.52706329386825,25.515625));
#74435=CARTESIAN_POINT('Ctrl Pts',(29.1183495962155,1.52706329386825,25.5572916666666));
#74436=CARTESIAN_POINT('Ctrl Pts',(28.6775243943233,0.76353164693412,25.5989583333333));
#74437=CARTESIAN_POINT('Ctrl Pts',(28.2366991924311,-1.31894491186926E-14,
25.640625));
#74438=CARTESIAN_POINT('Ctrl Pts',(28.6775243943233,-0.763531646934146,
25.6822916666666));
#74439=CARTESIAN_POINT('Ctrl Pts',(29.1183495962155,-1.52706329386828,25.7239583333333));
#74440=CARTESIAN_POINT('Ctrl Pts',(30.,-1.52706329386828,25.765625));
#74441=CARTESIAN_POINT('Ctrl Pts',(30.8816504037844,-1.52706329386828,25.8072916666666));
#74442=CARTESIAN_POINT('Ctrl Pts',(31.3224756056766,-0.763531646934147,
25.8489583333333));
#74443=CARTESIAN_POINT('Ctrl Pts',(31.7633008075689,-1.36198038370242E-14,
25.890625));
#74444=CARTESIAN_POINT('Ctrl Pts',(31.3224756056766,0.763531646934118,25.9322916666666));
#74445=CARTESIAN_POINT('Ctrl Pts',(30.8816504037844,1.52706329386825,25.9739583333333));
#74446=CARTESIAN_POINT('Ctrl Pts',(30.,1.52706329386825,26.015625));
#74447=CARTESIAN_POINT('Ctrl Pts',(29.1183495962155,1.52706329386825,26.0572916666666));
#74448=CARTESIAN_POINT('Ctrl Pts',(28.6775243943233,0.76353164693412,26.0989583333333));
#74449=CARTESIAN_POINT('Ctrl Pts',(28.2366991924311,-1.31894491186926E-14,
26.140625));
#74450=CARTESIAN_POINT('Ctrl Pts',(28.6775243943233,-0.763531646934146,
26.1822916666666));
#74451=CARTESIAN_POINT('Ctrl Pts',(29.1183495962155,-1.52706329386828,26.2239583333333));
#74452=CARTESIAN_POINT('Ctrl Pts',(30.,-1.52706329386828,26.265625));
#74453=CARTESIAN_POINT('Ctrl Pts',(30.8816504037844,-1.52706329386828,26.3072916666666));
#74454=CARTESIAN_POINT('Ctrl Pts',(31.3224756056766,-0.763531646934147,
26.3489583333333));
#74455=CARTESIAN_POINT('Ctrl Pts',(31.7633008075689,-1.36198038370242E-14,
26.390625));
#74456=CARTESIAN_POINT('Ctrl Pts',(31.3224756056766,0.763531646934118,26.4322916666666));
#74457=CARTESIAN_POINT('Ctrl Pts',(30.8816504037844,1.52706329386825,26.4739583333333));
#74458=CARTESIAN_POINT('Ctrl Pts',(30.,1.52706329386825,26.515625));
#74459=CARTESIAN_POINT('Ctrl Pts',(29.1183495962155,1.52706329386825,26.5572916666666));
#74460=CARTESIAN_POINT('Ctrl Pts',(28.6775243943233,0.76353164693412,26.5989583333333));
#74461=CARTESIAN_POINT('Ctrl Pts',(28.2366991924311,-1.31894491186926E-14,
26.640625));
#74462=CARTESIAN_POINT('Ctrl Pts',(28.6775243943233,-0.763531646934146,
26.6822916666666));
#74463=CARTESIAN_POINT('Ctrl Pts',(29.1183495962155,-1.52706329386828,26.7239583333333));
#74464=CARTESIAN_POINT('Ctrl Pts',(30.,-1.52706329386828,26.765625));
#74465=CARTESIAN_POINT('Ctrl Pts',(30.8816504037844,-1.52706329386828,26.8072916666666));
#74466=CARTESIAN_POINT('Ctrl Pts',(31.3224756056766,-0.763531646934147,
26.8489583333333));
#74467=CARTESIAN_POINT('Ctrl Pts',(31.7633008075689,-1.36198038370242E-14,
26.890625));
#74468=CARTESIAN_POINT('Ctrl Pts',(31.3224756056766,0.763531646934118,26.9322916666666));
#74469=CARTESIAN_POINT('Ctrl Pts',(30.8816504037844,1.52706329386825,26.9739583333333));
#74470=CARTESIAN_POINT('Ctrl Pts',(30.,1.52706329386825,27.015625));
#74471=CARTESIAN_POINT('Ctrl Pts',(29.1183495962155,1.52706329386825,27.0572916666666));
#74472=CARTESIAN_POINT('Ctrl Pts',(28.6775243943233,0.76353164693412,27.0989583333333));
#74473=CARTESIAN_POINT('Ctrl Pts',(28.2366991924311,-1.31894491186926E-14,
27.140625));
#74474=CARTESIAN_POINT('Ctrl Pts',(28.6775243943233,-0.763531646934146,
27.1822916666666));
#74475=CARTESIAN_POINT('Ctrl Pts',(29.1183495962155,-1.52706329386828,27.2239583333333));
#74476=CARTESIAN_POINT('Ctrl Pts',(30.,-1.52706329386828,27.265625));
#74477=CARTESIAN_POINT('Ctrl Pts',(30.8816504037844,-1.52706329386828,27.3072916666666));
#74478=CARTESIAN_POINT('Ctrl Pts',(31.3224756056766,-0.763531646934147,
27.3489583333333));
#74479=CARTESIAN_POINT('Ctrl Pts',(31.7633008075689,-1.36198038370242E-14,
27.390625));
#74480=CARTESIAN_POINT('Ctrl Pts',(31.3224756056766,0.763531646934118,27.4322916666666));
#74481=CARTESIAN_POINT('Ctrl Pts',(30.8816504037844,1.52706329386825,27.4739583333333));
#74482=CARTESIAN_POINT('Ctrl Pts',(30.,1.52706329386825,27.515625));
#74483=CARTESIAN_POINT('Ctrl Pts',(29.1183495962155,1.52706329386825,27.5572916666666));
#74484=CARTESIAN_POINT('Ctrl Pts',(28.6775243943233,0.76353164693412,27.5989583333333));
#74485=CARTESIAN_POINT('Ctrl Pts',(28.2366991924311,-1.31894491186926E-14,
27.640625));
#74486=CARTESIAN_POINT('Ctrl Pts',(28.6775243943233,-0.763531646934146,
27.6822916666666));
#74487=CARTESIAN_POINT('Ctrl Pts',(29.1183495962155,-1.52706329386828,27.7239583333333));
#74488=CARTESIAN_POINT('Ctrl Pts',(30.,-1.52706329386828,27.765625));
#74489=CARTESIAN_POINT('Ctrl Pts',(30.8816504037844,-1.52706329386828,27.8072916666666));
#74490=CARTESIAN_POINT('Ctrl Pts',(31.3224756056766,-0.763531646934147,
27.8489583333333));
#74491=CARTESIAN_POINT('Ctrl Pts',(31.7633008075689,-1.36198038370242E-14,
27.890625));
#74492=CARTESIAN_POINT('Ctrl Pts',(31.3224756056766,0.763531646934118,27.9322916666666));
#74493=CARTESIAN_POINT('Ctrl Pts',(30.8816504037844,1.52706329386825,27.9739583333333));
#74494=CARTESIAN_POINT('Ctrl Pts',(30.,1.52706329386825,28.015625));
#74495=CARTESIAN_POINT('Ctrl Pts',(29.1183495962155,1.52706329386825,28.0572916666666));
#74496=CARTESIAN_POINT('Ctrl Pts',(28.6775243943233,0.76353164693412,28.0989583333333));
#74497=CARTESIAN_POINT('Ctrl Pts',(28.2366991924311,-1.31894491186926E-14,
28.140625));
#74498=CARTESIAN_POINT('Ctrl Pts',(28.6775243943233,-0.763531646934146,
28.1822916666666));
#74499=CARTESIAN_POINT('Ctrl Pts',(29.1183495962155,-1.52706329386828,28.2239583333333));
#74500=CARTESIAN_POINT('Ctrl Pts',(30.,-1.52706329386828,28.265625));
#74501=CARTESIAN_POINT('Ctrl Pts',(30.8816504037844,-1.52706329386828,28.3072916666666));
#74502=CARTESIAN_POINT('Ctrl Pts',(31.3224756056766,-0.763531646934147,
28.3489583333333));
#74503=CARTESIAN_POINT('Ctrl Pts',(31.7633008075689,-1.36198038370242E-14,
28.390625));
#74504=CARTESIAN_POINT('Ctrl Pts',(31.3224756056766,0.763531646934118,28.4322916666666));
#74505=CARTESIAN_POINT('Ctrl Pts',(30.8816504037844,1.52706329386825,28.4739583333333));
#74506=CARTESIAN_POINT('Ctrl Pts',(30.,1.52706329386825,28.515625));
#74507=CARTESIAN_POINT('Ctrl Pts',(29.1183495962155,1.52706329386825,28.5572916666666));
#74508=CARTESIAN_POINT('Ctrl Pts',(28.6775243943233,0.76353164693412,28.5989583333333));
#74509=CARTESIAN_POINT('Ctrl Pts',(28.2366991924311,-1.31894491186926E-14,
28.640625));
#74510=CARTESIAN_POINT('Ctrl Pts',(28.6775243943233,-0.763531646934146,
28.6822916666666));
#74511=CARTESIAN_POINT('Ctrl Pts',(29.1183495962155,-1.52706329386828,28.7239583333333));
#74512=CARTESIAN_POINT('Ctrl Pts',(30.,-1.52706329386828,28.765625));
#74513=CARTESIAN_POINT('Ctrl Pts',(30.8816504037844,-1.52706329386828,28.8072916666666));
#74514=CARTESIAN_POINT('Ctrl Pts',(31.3224756056766,-0.763531646934147,
28.8489583333333));
#74515=CARTESIAN_POINT('Ctrl Pts',(31.7633008075689,-1.36198038370242E-14,
28.890625));
#74516=CARTESIAN_POINT('Ctrl Pts',(31.3224756056766,0.763531646934118,28.9322916666666));
#74517=CARTESIAN_POINT('Ctrl Pts',(30.8816504037844,1.52706329386825,28.9739583333333));
#74518=CARTESIAN_POINT('Ctrl Pts',(30.,1.52706329386825,29.015625));
#74519=CARTESIAN_POINT('Ctrl Pts',(29.1183495962155,1.52706329386825,29.0572916666666));
#74520=CARTESIAN_POINT('Ctrl Pts',(28.6775243943233,0.76353164693412,29.0989583333333));
#74521=CARTESIAN_POINT('Ctrl Pts',(28.2366991924311,-1.31894491186926E-14,
29.140625));
#74522=CARTESIAN_POINT('Ctrl Pts',(28.6775243943233,-0.763531646934146,
29.1822916666666));
#74523=CARTESIAN_POINT('Ctrl Pts',(29.1183495962155,-1.52706329386828,29.2239583333333));
#74524=CARTESIAN_POINT('Ctrl Pts',(30.,-1.52706329386828,29.265625));
#74525=CARTESIAN_POINT('Ctrl Pts',(30.8816504037844,-1.52706329386828,29.3072916666666));
#74526=CARTESIAN_POINT('Ctrl Pts',(31.3224756056766,-0.763531646934147,
29.3489583333333));
#74527=CARTESIAN_POINT('Ctrl Pts',(31.7633008075689,-1.36198038370242E-14,
29.390625));
#74528=CARTESIAN_POINT('Ctrl Pts',(31.3224756056766,0.763531646934118,29.4322916666666));
#74529=CARTESIAN_POINT('Ctrl Pts',(30.8816504037844,1.52706329386825,29.4739583333333));
#74530=CARTESIAN_POINT('Ctrl Pts',(30.,1.52706329386825,29.515625));
#74531=CARTESIAN_POINT('Ctrl Pts',(29.1183495962155,1.52706329386825,29.5572916666666));
#74532=CARTESIAN_POINT('Ctrl Pts',(28.6775243943233,0.76353164693412,29.5989583333333));
#74533=CARTESIAN_POINT('Ctrl Pts',(28.2366991924311,-1.31894491186926E-14,
29.640625));
#74534=CARTESIAN_POINT('Ctrl Pts',(28.6775243943233,-0.763531646934146,
29.6822916666666));
#74535=CARTESIAN_POINT('Ctrl Pts',(29.1183495962155,-1.52706329386828,29.7239583333333));
#74536=CARTESIAN_POINT('Ctrl Pts',(30.,-1.52706329386828,29.765625));
#74537=CARTESIAN_POINT('Ctrl Pts',(30.8816504037844,-1.52706329386828,29.8072916666666));
#74538=CARTESIAN_POINT('Ctrl Pts',(31.3224756056766,-0.763531646934147,
29.8489583333333));
#74539=CARTESIAN_POINT('Ctrl Pts',(31.7633008075689,-1.36198038370242E-14,
29.890625));
#74540=CARTESIAN_POINT('Ctrl Pts',(31.3224756056766,0.763531646934118,29.9322916666666));
#74541=CARTESIAN_POINT('Ctrl Pts',(30.8816504037844,1.52706329386825,29.9739583333333));
#74542=CARTESIAN_POINT('Ctrl Pts',(30.,1.52706329386825,30.015625));
#74543=CARTESIAN_POINT('Ctrl Pts',(29.1183495962155,1.52706329386825,30.0572916666666));
#74544=CARTESIAN_POINT('Ctrl Pts',(28.6775243943233,0.76353164693412,30.0989583333333));
#74545=CARTESIAN_POINT('Ctrl Pts',(28.2366991924311,-1.31894491186926E-14,
30.140625));
#74546=CARTESIAN_POINT('Ctrl Pts',(28.6775243943233,-0.763531646934146,
30.1822916666666));
#74547=CARTESIAN_POINT('Ctrl Pts',(29.1183495962155,-1.52706329386828,30.2239583333333));
#74548=CARTESIAN_POINT('Ctrl Pts',(30.,-1.52706329386828,30.265625));
#74549=CARTESIAN_POINT('Ctrl Pts',(30.8816504037844,-1.52706329386828,30.3072916666666));
#74550=CARTESIAN_POINT('Ctrl Pts',(31.3224756056766,-0.763531646934147,
30.3489583333333));
#74551=CARTESIAN_POINT('Ctrl Pts',(31.7633008075689,-1.36198038370242E-14,
30.390625));
#74552=CARTESIAN_POINT('Ctrl Pts',(31.3224756056766,0.763531646934118,30.4322916666666));
#74553=CARTESIAN_POINT('Ctrl Pts',(30.8816504037844,1.52706329386825,30.4739583333333));
#74554=CARTESIAN_POINT('Ctrl Pts',(30.,1.52706329386825,30.515625));
#74555=CARTESIAN_POINT('Ctrl Pts',(29.1183495962155,1.52706329386825,30.5572916666666));
#74556=CARTESIAN_POINT('Ctrl Pts',(28.6775243943233,0.76353164693412,30.5989583333333));
#74557=CARTESIAN_POINT('Ctrl Pts',(28.2366991924311,-1.31894491186926E-14,
30.640625));
#74558=CARTESIAN_POINT('Ctrl Pts',(28.6775243943233,-0.763531646934146,
30.6822916666666));
#74559=CARTESIAN_POINT('Ctrl Pts',(29.1183495962155,-1.52706329386828,30.7239583333333));
#74560=CARTESIAN_POINT('Ctrl Pts',(30.,-1.52706329386828,30.765625));
#74561=CARTESIAN_POINT('Ctrl Pts',(30.8816504037844,-1.52706329386828,30.8072916666666));
#74562=CARTESIAN_POINT('Ctrl Pts',(31.3224756056766,-0.763531646934147,
30.8489583333333));
#74563=CARTESIAN_POINT('Ctrl Pts',(31.7633008075689,-1.36198038370242E-14,
30.890625));
#74564=CARTESIAN_POINT('Ctrl Pts',(31.3224756056766,0.763531646934118,30.9322916666666));
#74565=CARTESIAN_POINT('Ctrl Pts',(30.8816504037844,1.52706329386825,30.9739583333333));
#74566=CARTESIAN_POINT('Ctrl Pts',(30.,1.52706329386825,31.015625));
#74567=CARTESIAN_POINT('Ctrl Pts',(29.1183495962155,1.52706329386825,31.0572916666666));
#74568=CARTESIAN_POINT('Ctrl Pts',(28.6775243943233,0.76353164693412,31.0989583333333));
#74569=CARTESIAN_POINT('Ctrl Pts',(28.2366991924311,-1.31894491186926E-14,
31.140625));
#74570=CARTESIAN_POINT('Ctrl Pts',(28.6775243943233,-0.763531646934146,
31.1822916666666));
#74571=CARTESIAN_POINT('Ctrl Pts',(29.1183495962155,-1.52706329386828,31.2239583333333));
#74572=CARTESIAN_POINT('Ctrl Pts',(30.,-1.52706329386828,31.265625));
#74573=CARTESIAN_POINT('Ctrl Pts',(30.8816504037844,-1.52706329386828,31.3072916666666));
#74574=CARTESIAN_POINT('Ctrl Pts',(31.3224756056766,-0.763531646934147,
31.3489583333333));
#74575=CARTESIAN_POINT('Ctrl Pts',(31.7633008075689,-1.36198038370242E-14,
31.390625));
#74576=CARTESIAN_POINT('Ctrl Pts',(31.3224756056766,0.763531646934118,31.4322916666666));
#74577=CARTESIAN_POINT('Ctrl Pts',(30.8816504037844,1.52706329386825,31.4739583333333));
#74578=CARTESIAN_POINT('Ctrl Pts',(30.,1.52706329386825,31.515625));
#74579=CARTESIAN_POINT('Ctrl Pts',(30.,1.17523507120987,15.8124968809397));
#74580=CARTESIAN_POINT('Ctrl Pts',(29.3214777152758,1.17523507120987,15.8541635476064));
#74581=CARTESIAN_POINT('Ctrl Pts',(28.9822165729138,0.587617535604928,15.895830214273));
#74582=CARTESIAN_POINT('Ctrl Pts',(28.6429554305518,-1.32141489532166E-14,
15.9374968809397));
#74583=CARTESIAN_POINT('Ctrl Pts',(28.9822165729138,-0.587617535604954,
15.9791635476064));
#74584=CARTESIAN_POINT('Ctrl Pts',(29.3214777152758,-1.17523507120989,16.020830214273));
#74585=CARTESIAN_POINT('Ctrl Pts',(30.,-1.17523507120989,16.0624968809397));
#74586=CARTESIAN_POINT('Ctrl Pts',(30.6785222847241,-1.17523507120989,16.1041635476064));
#74587=CARTESIAN_POINT('Ctrl Pts',(31.0177834270861,-0.587617535604955,
16.145830214273));
#74588=CARTESIAN_POINT('Ctrl Pts',(31.3570445694482,-1.35453519623354E-14,
16.1874968809397));
#74589=CARTESIAN_POINT('Ctrl Pts',(31.0177834270861,0.587617535604927,16.2291635476064));
#74590=CARTESIAN_POINT('Ctrl Pts',(30.6785222847241,1.17523507120987,16.270830214273));
#74591=CARTESIAN_POINT('Ctrl Pts',(30.,1.17523507120987,16.3124968809397));
#74592=CARTESIAN_POINT('Ctrl Pts',(29.3214777152758,1.17523507120987,16.3541635476064));
#74593=CARTESIAN_POINT('Ctrl Pts',(28.9822165729138,0.587617535604928,16.395830214273));
#74594=CARTESIAN_POINT('Ctrl Pts',(28.6429554305518,-1.32141489532166E-14,
16.4374968809397));
#74595=CARTESIAN_POINT('Ctrl Pts',(28.9822165729138,-0.587617535604954,
16.4791635476064));
#74596=CARTESIAN_POINT('Ctrl Pts',(29.3214777152758,-1.17523507120989,16.520830214273));
#74597=CARTESIAN_POINT('Ctrl Pts',(30.,-1.17523507120989,16.5624968809397));
#74598=CARTESIAN_POINT('Ctrl Pts',(30.6785222847241,-1.17523507120989,16.6041635476064));
#74599=CARTESIAN_POINT('Ctrl Pts',(31.0177834270861,-0.587617535604955,
16.645830214273));
#74600=CARTESIAN_POINT('Ctrl Pts',(31.3570445694482,-1.35453519623354E-14,
16.6874968809397));
#74601=CARTESIAN_POINT('Ctrl Pts',(31.0177834270861,0.587617535604927,16.7291635476064));
#74602=CARTESIAN_POINT('Ctrl Pts',(30.6785222847241,1.17523507120987,16.770830214273));
#74603=CARTESIAN_POINT('Ctrl Pts',(30.,1.17523507120987,16.8124968809397));
#74604=CARTESIAN_POINT('Ctrl Pts',(29.3214777152758,1.17523507120987,16.8541635476064));
#74605=CARTESIAN_POINT('Ctrl Pts',(28.9822165729138,0.587617535604928,16.895830214273));
#74606=CARTESIAN_POINT('Ctrl Pts',(28.6429554305518,-1.32141489532166E-14,
16.9374968809397));
#74607=CARTESIAN_POINT('Ctrl Pts',(28.9822165729138,-0.587617535604954,
16.9791635476064));
#74608=CARTESIAN_POINT('Ctrl Pts',(29.3214777152758,-1.17523507120989,17.020830214273));
#74609=CARTESIAN_POINT('Ctrl Pts',(30.,-1.17523507120989,17.0624968809397));
#74610=CARTESIAN_POINT('Ctrl Pts',(30.6785222847241,-1.17523507120989,17.1041635476064));
#74611=CARTESIAN_POINT('Ctrl Pts',(31.0177834270861,-0.587617535604955,
17.145830214273));
#74612=CARTESIAN_POINT('Ctrl Pts',(31.3570445694482,-1.35453519623354E-14,
17.1874968809397));
#74613=CARTESIAN_POINT('Ctrl Pts',(31.0177834270861,0.587617535604927,17.2291635476064));
#74614=CARTESIAN_POINT('Ctrl Pts',(30.6785222847241,1.17523507120987,17.270830214273));
#74615=CARTESIAN_POINT('Ctrl Pts',(30.,1.17523507120987,17.3124968809397));
#74616=CARTESIAN_POINT('Ctrl Pts',(29.3214777152758,1.17523507120987,17.3541635476064));
#74617=CARTESIAN_POINT('Ctrl Pts',(28.9822165729138,0.587617535604928,17.395830214273));
#74618=CARTESIAN_POINT('Ctrl Pts',(28.6429554305518,-1.32141489532166E-14,
17.4374968809397));
#74619=CARTESIAN_POINT('Ctrl Pts',(28.9822165729138,-0.587617535604954,
17.4791635476064));
#74620=CARTESIAN_POINT('Ctrl Pts',(29.3214777152758,-1.17523507120989,17.520830214273));
#74621=CARTESIAN_POINT('Ctrl Pts',(30.,-1.17523507120989,17.5624968809397));
#74622=CARTESIAN_POINT('Ctrl Pts',(30.6785222847241,-1.17523507120989,17.6041635476064));
#74623=CARTESIAN_POINT('Ctrl Pts',(31.0177834270861,-0.587617535604955,
17.645830214273));
#74624=CARTESIAN_POINT('Ctrl Pts',(31.3570445694482,-1.35453519623354E-14,
17.6874968809397));
#74625=CARTESIAN_POINT('Ctrl Pts',(31.0177834270861,0.587617535604927,17.7291635476064));
#74626=CARTESIAN_POINT('Ctrl Pts',(30.6785222847241,1.17523507120987,17.770830214273));
#74627=CARTESIAN_POINT('Ctrl Pts',(30.,1.17523507120987,17.8124968809397));
#74628=CARTESIAN_POINT('Ctrl Pts',(29.3214777152758,1.17523507120987,17.8541635476064));
#74629=CARTESIAN_POINT('Ctrl Pts',(28.9822165729138,0.587617535604928,17.895830214273));
#74630=CARTESIAN_POINT('Ctrl Pts',(28.6429554305518,-1.32141489532166E-14,
17.9374968809397));
#74631=CARTESIAN_POINT('Ctrl Pts',(28.9822165729138,-0.587617535604954,
17.9791635476064));
#74632=CARTESIAN_POINT('Ctrl Pts',(29.3214777152758,-1.17523507120989,18.020830214273));
#74633=CARTESIAN_POINT('Ctrl Pts',(30.,-1.17523507120989,18.0624968809397));
#74634=CARTESIAN_POINT('Ctrl Pts',(30.6785222847241,-1.17523507120989,18.1041635476064));
#74635=CARTESIAN_POINT('Ctrl Pts',(31.0177834270861,-0.587617535604955,
18.145830214273));
#74636=CARTESIAN_POINT('Ctrl Pts',(31.3570445694482,-1.35453519623354E-14,
18.1874968809397));
#74637=CARTESIAN_POINT('Ctrl Pts',(31.0177834270861,0.587617535604927,18.2291635476064));
#74638=CARTESIAN_POINT('Ctrl Pts',(30.6785222847241,1.17523507120987,18.270830214273));
#74639=CARTESIAN_POINT('Ctrl Pts',(30.,1.17523507120987,18.3124968809397));
#74640=CARTESIAN_POINT('Ctrl Pts',(29.3214777152758,1.17523507120987,18.3541635476064));
#74641=CARTESIAN_POINT('Ctrl Pts',(28.9822165729138,0.587617535604928,18.395830214273));
#74642=CARTESIAN_POINT('Ctrl Pts',(28.6429554305518,-1.32141489532166E-14,
18.4374968809397));
#74643=CARTESIAN_POINT('Ctrl Pts',(28.9822165729138,-0.587617535604954,
18.4791635476064));
#74644=CARTESIAN_POINT('Ctrl Pts',(29.3214777152758,-1.17523507120989,18.520830214273));
#74645=CARTESIAN_POINT('Ctrl Pts',(30.,-1.17523507120989,18.5624968809397));
#74646=CARTESIAN_POINT('Ctrl Pts',(30.6785222847241,-1.17523507120989,18.6041635476064));
#74647=CARTESIAN_POINT('Ctrl Pts',(31.0177834270861,-0.587617535604955,
18.645830214273));
#74648=CARTESIAN_POINT('Ctrl Pts',(31.3570445694482,-1.35453519623354E-14,
18.6874968809397));
#74649=CARTESIAN_POINT('Ctrl Pts',(31.0177834270861,0.587617535604927,18.7291635476064));
#74650=CARTESIAN_POINT('Ctrl Pts',(30.6785222847241,1.17523507120987,18.770830214273));
#74651=CARTESIAN_POINT('Ctrl Pts',(30.,1.17523507120987,18.8124968809397));
#74652=CARTESIAN_POINT('Ctrl Pts',(29.3214777152758,1.17523507120987,18.8541635476064));
#74653=CARTESIAN_POINT('Ctrl Pts',(28.9822165729138,0.587617535604928,18.895830214273));
#74654=CARTESIAN_POINT('Ctrl Pts',(28.6429554305518,-1.32141489532166E-14,
18.9374968809397));
#74655=CARTESIAN_POINT('Ctrl Pts',(28.9822165729138,-0.587617535604954,
18.9791635476064));
#74656=CARTESIAN_POINT('Ctrl Pts',(29.3214777152758,-1.17523507120989,19.020830214273));
#74657=CARTESIAN_POINT('Ctrl Pts',(30.,-1.17523507120989,19.0624968809397));
#74658=CARTESIAN_POINT('Ctrl Pts',(30.6785222847241,-1.17523507120989,19.1041635476064));
#74659=CARTESIAN_POINT('Ctrl Pts',(31.0177834270861,-0.587617535604955,
19.145830214273));
#74660=CARTESIAN_POINT('Ctrl Pts',(31.3570445694482,-1.35453519623354E-14,
19.1874968809397));
#74661=CARTESIAN_POINT('Ctrl Pts',(31.0177834270861,0.587617535604927,19.2291635476064));
#74662=CARTESIAN_POINT('Ctrl Pts',(30.6785222847241,1.17523507120987,19.270830214273));
#74663=CARTESIAN_POINT('Ctrl Pts',(30.,1.17523507120987,19.3124968809397));
#74664=CARTESIAN_POINT('Ctrl Pts',(29.3214777152758,1.17523507120987,19.3541635476064));
#74665=CARTESIAN_POINT('Ctrl Pts',(28.9822165729138,0.587617535604928,19.395830214273));
#74666=CARTESIAN_POINT('Ctrl Pts',(28.6429554305518,-1.32141489532166E-14,
19.4374968809397));
#74667=CARTESIAN_POINT('Ctrl Pts',(28.9822165729138,-0.587617535604954,
19.4791635476064));
#74668=CARTESIAN_POINT('Ctrl Pts',(29.3214777152758,-1.17523507120989,19.520830214273));
#74669=CARTESIAN_POINT('Ctrl Pts',(30.,-1.17523507120989,19.5624968809397));
#74670=CARTESIAN_POINT('Ctrl Pts',(30.6785222847241,-1.17523507120989,19.6041635476064));
#74671=CARTESIAN_POINT('Ctrl Pts',(31.0177834270861,-0.587617535604955,
19.645830214273));
#74672=CARTESIAN_POINT('Ctrl Pts',(31.3570445694482,-1.35453519623354E-14,
19.6874968809397));
#74673=CARTESIAN_POINT('Ctrl Pts',(31.0177834270861,0.587617535604927,19.7291635476064));
#74674=CARTESIAN_POINT('Ctrl Pts',(30.6785222847241,1.17523507120987,19.770830214273));
#74675=CARTESIAN_POINT('Ctrl Pts',(30.,1.17523507120987,19.8124968809397));
#74676=CARTESIAN_POINT('Ctrl Pts',(29.3214777152758,1.17523507120987,19.8541635476064));
#74677=CARTESIAN_POINT('Ctrl Pts',(28.9822165729138,0.587617535604928,19.895830214273));
#74678=CARTESIAN_POINT('Ctrl Pts',(28.6429554305518,-1.32141489532166E-14,
19.9374968809397));
#74679=CARTESIAN_POINT('Ctrl Pts',(28.9822165729138,-0.587617535604954,
19.9791635476064));
#74680=CARTESIAN_POINT('Ctrl Pts',(29.3214777152758,-1.17523507120989,20.020830214273));
#74681=CARTESIAN_POINT('Ctrl Pts',(30.,-1.17523507120989,20.0624968809397));
#74682=CARTESIAN_POINT('Ctrl Pts',(30.6785222847241,-1.17523507120989,20.1041635476064));
#74683=CARTESIAN_POINT('Ctrl Pts',(31.0177834270861,-0.587617535604955,
20.145830214273));
#74684=CARTESIAN_POINT('Ctrl Pts',(31.3570445694482,-1.35453519623354E-14,
20.1874968809397));
#74685=CARTESIAN_POINT('Ctrl Pts',(31.0177834270861,0.587617535604927,20.2291635476064));
#74686=CARTESIAN_POINT('Ctrl Pts',(30.6785222847241,1.17523507120987,20.270830214273));
#74687=CARTESIAN_POINT('Ctrl Pts',(30.,1.17523507120987,20.3124968809397));
#74688=CARTESIAN_POINT('Ctrl Pts',(29.3214777152758,1.17523507120987,20.3541635476064));
#74689=CARTESIAN_POINT('Ctrl Pts',(28.9822165729138,0.587617535604928,20.395830214273));
#74690=CARTESIAN_POINT('Ctrl Pts',(28.6429554305518,-1.32141489532166E-14,
20.4374968809397));
#74691=CARTESIAN_POINT('Ctrl Pts',(28.9822165729138,-0.587617535604954,
20.4791635476064));
#74692=CARTESIAN_POINT('Ctrl Pts',(29.3214777152758,-1.17523507120989,20.520830214273));
#74693=CARTESIAN_POINT('Ctrl Pts',(30.,-1.17523507120989,20.5624968809397));
#74694=CARTESIAN_POINT('Ctrl Pts',(30.6785222847241,-1.17523507120989,20.6041635476064));
#74695=CARTESIAN_POINT('Ctrl Pts',(31.0177834270861,-0.587617535604955,
20.645830214273));
#74696=CARTESIAN_POINT('Ctrl Pts',(31.3570445694482,-1.35453519623354E-14,
20.6874968809397));
#74697=CARTESIAN_POINT('Ctrl Pts',(31.0177834270861,0.587617535604927,20.7291635476064));
#74698=CARTESIAN_POINT('Ctrl Pts',(30.6785222847241,1.17523507120987,20.770830214273));
#74699=CARTESIAN_POINT('Ctrl Pts',(30.,1.17523507120987,20.8124968809397));
#74700=CARTESIAN_POINT('Ctrl Pts',(29.3214777152758,1.17523507120987,20.8541635476064));
#74701=CARTESIAN_POINT('Ctrl Pts',(28.9822165729138,0.587617535604928,20.895830214273));
#74702=CARTESIAN_POINT('Ctrl Pts',(28.6429554305518,-1.32141489532166E-14,
20.9374968809397));
#74703=CARTESIAN_POINT('Ctrl Pts',(28.9822165729138,-0.587617535604954,
20.9791635476064));
#74704=CARTESIAN_POINT('Ctrl Pts',(29.3214777152758,-1.17523507120989,21.020830214273));
#74705=CARTESIAN_POINT('Ctrl Pts',(30.,-1.17523507120989,21.0624968809397));
#74706=CARTESIAN_POINT('Ctrl Pts',(30.6785222847241,-1.17523507120989,21.1041635476064));
#74707=CARTESIAN_POINT('Ctrl Pts',(31.0177834270861,-0.587617535604955,
21.145830214273));
#74708=CARTESIAN_POINT('Ctrl Pts',(31.3570445694482,-1.35453519623354E-14,
21.1874968809397));
#74709=CARTESIAN_POINT('Ctrl Pts',(31.0177834270861,0.587617535604927,21.2291635476064));
#74710=CARTESIAN_POINT('Ctrl Pts',(30.6785222847241,1.17523507120987,21.270830214273));
#74711=CARTESIAN_POINT('Ctrl Pts',(30.,1.17523507120987,21.3124968809397));
#74712=CARTESIAN_POINT('Ctrl Pts',(29.3214777152758,1.17523507120987,21.3541635476064));
#74713=CARTESIAN_POINT('Ctrl Pts',(28.9822165729138,0.587617535604928,21.395830214273));
#74714=CARTESIAN_POINT('Ctrl Pts',(28.6429554305518,-1.32141489532166E-14,
21.4374968809397));
#74715=CARTESIAN_POINT('Ctrl Pts',(28.9822165729138,-0.587617535604954,
21.4791635476064));
#74716=CARTESIAN_POINT('Ctrl Pts',(29.3214777152758,-1.17523507120989,21.520830214273));
#74717=CARTESIAN_POINT('Ctrl Pts',(30.,-1.17523507120989,21.5624968809397));
#74718=CARTESIAN_POINT('Ctrl Pts',(30.6785222847241,-1.17523507120989,21.6041635476064));
#74719=CARTESIAN_POINT('Ctrl Pts',(31.0177834270861,-0.587617535604955,
21.645830214273));
#74720=CARTESIAN_POINT('Ctrl Pts',(31.3570445694482,-1.35453519623354E-14,
21.6874968809397));
#74721=CARTESIAN_POINT('Ctrl Pts',(31.0177834270861,0.587617535604927,21.7291635476064));
#74722=CARTESIAN_POINT('Ctrl Pts',(30.6785222847241,1.17523507120987,21.770830214273));
#74723=CARTESIAN_POINT('Ctrl Pts',(30.,1.17523507120987,21.8124968809397));
#74724=CARTESIAN_POINT('Ctrl Pts',(29.3214777152758,1.17523507120987,21.8541635476064));
#74725=CARTESIAN_POINT('Ctrl Pts',(28.9822165729138,0.587617535604928,21.895830214273));
#74726=CARTESIAN_POINT('Ctrl Pts',(28.6429554305518,-1.32141489532166E-14,
21.9374968809397));
#74727=CARTESIAN_POINT('Ctrl Pts',(28.9822165729138,-0.587617535604954,
21.9791635476064));
#74728=CARTESIAN_POINT('Ctrl Pts',(29.3214777152758,-1.17523507120989,22.020830214273));
#74729=CARTESIAN_POINT('Ctrl Pts',(30.,-1.17523507120989,22.0624968809397));
#74730=CARTESIAN_POINT('Ctrl Pts',(30.6785222847241,-1.17523507120989,22.1041635476064));
#74731=CARTESIAN_POINT('Ctrl Pts',(31.0177834270861,-0.587617535604955,
22.145830214273));
#74732=CARTESIAN_POINT('Ctrl Pts',(31.3570445694482,-1.35453519623354E-14,
22.1874968809397));
#74733=CARTESIAN_POINT('Ctrl Pts',(31.0177834270861,0.587617535604927,22.2291635476064));
#74734=CARTESIAN_POINT('Ctrl Pts',(30.6785222847241,1.17523507120987,22.270830214273));
#74735=CARTESIAN_POINT('Ctrl Pts',(30.,1.17523507120987,22.3124968809397));
#74736=CARTESIAN_POINT('Ctrl Pts',(29.3214777152758,1.17523507120987,22.3541635476064));
#74737=CARTESIAN_POINT('Ctrl Pts',(28.9822165729138,0.587617535604928,22.395830214273));
#74738=CARTESIAN_POINT('Ctrl Pts',(28.6429554305518,-1.32141489532166E-14,
22.4374968809397));
#74739=CARTESIAN_POINT('Ctrl Pts',(28.9822165729138,-0.587617535604954,
22.4791635476064));
#74740=CARTESIAN_POINT('Ctrl Pts',(29.3214777152758,-1.17523507120989,22.520830214273));
#74741=CARTESIAN_POINT('Ctrl Pts',(30.,-1.17523507120989,22.5624968809397));
#74742=CARTESIAN_POINT('Ctrl Pts',(30.6785222847241,-1.17523507120989,22.6041635476064));
#74743=CARTESIAN_POINT('Ctrl Pts',(31.0177834270861,-0.587617535604955,
22.645830214273));
#74744=CARTESIAN_POINT('Ctrl Pts',(31.3570445694482,-1.35453519623354E-14,
22.6874968809397));
#74745=CARTESIAN_POINT('Ctrl Pts',(31.0177834270861,0.587617535604927,22.7291635476064));
#74746=CARTESIAN_POINT('Ctrl Pts',(30.6785222847241,1.17523507120987,22.770830214273));
#74747=CARTESIAN_POINT('Ctrl Pts',(30.,1.17523507120987,22.8124968809397));
#74748=CARTESIAN_POINT('Ctrl Pts',(29.3214777152758,1.17523507120987,22.8541635476064));
#74749=CARTESIAN_POINT('Ctrl Pts',(28.9822165729138,0.587617535604928,22.895830214273));
#74750=CARTESIAN_POINT('Ctrl Pts',(28.6429554305518,-1.32141489532166E-14,
22.9374968809397));
#74751=CARTESIAN_POINT('Ctrl Pts',(28.9822165729138,-0.587617535604954,
22.9791635476064));
#74752=CARTESIAN_POINT('Ctrl Pts',(29.3214777152758,-1.17523507120989,23.020830214273));
#74753=CARTESIAN_POINT('Ctrl Pts',(30.,-1.17523507120989,23.0624968809397));
#74754=CARTESIAN_POINT('Ctrl Pts',(30.6785222847241,-1.17523507120989,23.1041635476064));
#74755=CARTESIAN_POINT('Ctrl Pts',(31.0177834270861,-0.587617535604955,
23.145830214273));
#74756=CARTESIAN_POINT('Ctrl Pts',(31.3570445694482,-1.35453519623354E-14,
23.1874968809397));
#74757=CARTESIAN_POINT('Ctrl Pts',(31.0177834270861,0.587617535604927,23.2291635476064));
#74758=CARTESIAN_POINT('Ctrl Pts',(30.6785222847241,1.17523507120987,23.270830214273));
#74759=CARTESIAN_POINT('Ctrl Pts',(30.,1.17523507120987,23.3124968809397));
#74760=CARTESIAN_POINT('Ctrl Pts',(29.3214777152758,1.17523507120987,23.3541635476064));
#74761=CARTESIAN_POINT('Ctrl Pts',(28.9822165729138,0.587617535604928,23.395830214273));
#74762=CARTESIAN_POINT('Ctrl Pts',(28.6429554305518,-1.32141489532166E-14,
23.4374968809397));
#74763=CARTESIAN_POINT('Ctrl Pts',(28.9822165729138,-0.587617535604954,
23.4791635476064));
#74764=CARTESIAN_POINT('Ctrl Pts',(29.3214777152758,-1.17523507120989,23.520830214273));
#74765=CARTESIAN_POINT('Ctrl Pts',(30.,-1.17523507120989,23.5624968809397));
#74766=CARTESIAN_POINT('Ctrl Pts',(30.6785222847241,-1.17523507120989,23.6041635476064));
#74767=CARTESIAN_POINT('Ctrl Pts',(31.0177834270861,-0.587617535604955,
23.645830214273));
#74768=CARTESIAN_POINT('Ctrl Pts',(31.3570445694482,-1.35453519623354E-14,
23.6874968809397));
#74769=CARTESIAN_POINT('Ctrl Pts',(31.0177834270861,0.587617535604927,23.7291635476064));
#74770=CARTESIAN_POINT('Ctrl Pts',(30.6785222847241,1.17523507120987,23.770830214273));
#74771=CARTESIAN_POINT('Ctrl Pts',(30.,1.17523507120987,23.8124968809397));
#74772=CARTESIAN_POINT('Ctrl Pts',(29.3214777152758,1.17523507120987,23.8541635476064));
#74773=CARTESIAN_POINT('Ctrl Pts',(28.9822165729138,0.587617535604928,23.895830214273));
#74774=CARTESIAN_POINT('Ctrl Pts',(28.6429554305518,-1.32141489532166E-14,
23.9374968809397));
#74775=CARTESIAN_POINT('Ctrl Pts',(28.9822165729138,-0.587617535604954,
23.9791635476064));
#74776=CARTESIAN_POINT('Ctrl Pts',(29.3214777152758,-1.17523507120989,24.020830214273));
#74777=CARTESIAN_POINT('Ctrl Pts',(30.,-1.17523507120989,24.0624968809397));
#74778=CARTESIAN_POINT('Ctrl Pts',(30.6785222847241,-1.17523507120989,24.1041635476064));
#74779=CARTESIAN_POINT('Ctrl Pts',(31.0177834270861,-0.587617535604955,
24.145830214273));
#74780=CARTESIAN_POINT('Ctrl Pts',(31.3570445694482,-1.35453519623354E-14,
24.1874968809397));
#74781=CARTESIAN_POINT('Ctrl Pts',(31.0177834270861,0.587617535604927,24.2291635476064));
#74782=CARTESIAN_POINT('Ctrl Pts',(30.6785222847241,1.17523507120987,24.270830214273));
#74783=CARTESIAN_POINT('Ctrl Pts',(30.,1.17523507120987,24.3124968809397));
#74784=CARTESIAN_POINT('Ctrl Pts',(29.3214777152758,1.17523507120987,24.3541635476064));
#74785=CARTESIAN_POINT('Ctrl Pts',(28.9822165729138,0.587617535604928,24.395830214273));
#74786=CARTESIAN_POINT('Ctrl Pts',(28.6429554305518,-1.32141489532166E-14,
24.4374968809397));
#74787=CARTESIAN_POINT('Ctrl Pts',(28.9822165729138,-0.587617535604954,
24.4791635476064));
#74788=CARTESIAN_POINT('Ctrl Pts',(29.3214777152758,-1.17523507120989,24.520830214273));
#74789=CARTESIAN_POINT('Ctrl Pts',(30.,-1.17523507120989,24.5624968809397));
#74790=CARTESIAN_POINT('Ctrl Pts',(30.6785222847241,-1.17523507120989,24.6041635476064));
#74791=CARTESIAN_POINT('Ctrl Pts',(31.0177834270861,-0.587617535604955,
24.645830214273));
#74792=CARTESIAN_POINT('Ctrl Pts',(31.3570445694482,-1.35453519623354E-14,
24.6874968809397));
#74793=CARTESIAN_POINT('Ctrl Pts',(31.0177834270861,0.587617535604927,24.7291635476064));
#74794=CARTESIAN_POINT('Ctrl Pts',(30.6785222847241,1.17523507120987,24.770830214273));
#74795=CARTESIAN_POINT('Ctrl Pts',(30.,1.17523507120987,24.8124968809397));
#74796=CARTESIAN_POINT('Ctrl Pts',(29.3214777152758,1.17523507120987,24.8541635476064));
#74797=CARTESIAN_POINT('Ctrl Pts',(28.9822165729138,0.587617535604928,24.895830214273));
#74798=CARTESIAN_POINT('Ctrl Pts',(28.6429554305518,-1.32141489532166E-14,
24.9374968809397));
#74799=CARTESIAN_POINT('Ctrl Pts',(28.9822165729138,-0.587617535604954,
24.9791635476064));
#74800=CARTESIAN_POINT('Ctrl Pts',(29.3214777152758,-1.17523507120989,25.020830214273));
#74801=CARTESIAN_POINT('Ctrl Pts',(30.,-1.17523507120989,25.0624968809397));
#74802=CARTESIAN_POINT('Ctrl Pts',(30.6785222847241,-1.17523507120989,25.1041635476064));
#74803=CARTESIAN_POINT('Ctrl Pts',(31.0177834270861,-0.587617535604955,
25.145830214273));
#74804=CARTESIAN_POINT('Ctrl Pts',(31.3570445694482,-1.35453519623354E-14,
25.1874968809397));
#74805=CARTESIAN_POINT('Ctrl Pts',(31.0177834270861,0.587617535604927,25.2291635476064));
#74806=CARTESIAN_POINT('Ctrl Pts',(30.6785222847241,1.17523507120987,25.270830214273));
#74807=CARTESIAN_POINT('Ctrl Pts',(30.,1.17523507120987,25.3124968809397));
#74808=CARTESIAN_POINT('Ctrl Pts',(29.3214777152758,1.17523507120987,25.3541635476064));
#74809=CARTESIAN_POINT('Ctrl Pts',(28.9822165729138,0.587617535604928,25.395830214273));
#74810=CARTESIAN_POINT('Ctrl Pts',(28.6429554305518,-1.32141489532166E-14,
25.4374968809397));
#74811=CARTESIAN_POINT('Ctrl Pts',(28.9822165729138,-0.587617535604954,
25.4791635476064));
#74812=CARTESIAN_POINT('Ctrl Pts',(29.3214777152758,-1.17523507120989,25.520830214273));
#74813=CARTESIAN_POINT('Ctrl Pts',(30.,-1.17523507120989,25.5624968809397));
#74814=CARTESIAN_POINT('Ctrl Pts',(30.6785222847241,-1.17523507120989,25.6041635476064));
#74815=CARTESIAN_POINT('Ctrl Pts',(31.0177834270861,-0.587617535604955,
25.645830214273));
#74816=CARTESIAN_POINT('Ctrl Pts',(31.3570445694482,-1.35453519623354E-14,
25.6874968809397));
#74817=CARTESIAN_POINT('Ctrl Pts',(31.0177834270861,0.587617535604927,25.7291635476064));
#74818=CARTESIAN_POINT('Ctrl Pts',(30.6785222847241,1.17523507120987,25.770830214273));
#74819=CARTESIAN_POINT('Ctrl Pts',(30.,1.17523507120987,25.8124968809397));
#74820=CARTESIAN_POINT('Ctrl Pts',(29.3214777152758,1.17523507120987,25.8541635476064));
#74821=CARTESIAN_POINT('Ctrl Pts',(28.9822165729138,0.587617535604928,25.895830214273));
#74822=CARTESIAN_POINT('Ctrl Pts',(28.6429554305518,-1.32141489532166E-14,
25.9374968809397));
#74823=CARTESIAN_POINT('Ctrl Pts',(28.9822165729138,-0.587617535604954,
25.9791635476064));
#74824=CARTESIAN_POINT('Ctrl Pts',(29.3214777152758,-1.17523507120989,26.020830214273));
#74825=CARTESIAN_POINT('Ctrl Pts',(30.,-1.17523507120989,26.0624968809397));
#74826=CARTESIAN_POINT('Ctrl Pts',(30.6785222847241,-1.17523507120989,26.1041635476064));
#74827=CARTESIAN_POINT('Ctrl Pts',(31.0177834270861,-0.587617535604955,
26.145830214273));
#74828=CARTESIAN_POINT('Ctrl Pts',(31.3570445694482,-1.35453519623354E-14,
26.1874968809397));
#74829=CARTESIAN_POINT('Ctrl Pts',(31.0177834270861,0.587617535604927,26.2291635476064));
#74830=CARTESIAN_POINT('Ctrl Pts',(30.6785222847241,1.17523507120987,26.270830214273));
#74831=CARTESIAN_POINT('Ctrl Pts',(30.,1.17523507120987,26.3124968809397));
#74832=CARTESIAN_POINT('Ctrl Pts',(29.3214777152758,1.17523507120987,26.3541635476064));
#74833=CARTESIAN_POINT('Ctrl Pts',(28.9822165729138,0.587617535604928,26.395830214273));
#74834=CARTESIAN_POINT('Ctrl Pts',(28.6429554305518,-1.32141489532166E-14,
26.4374968809397));
#74835=CARTESIAN_POINT('Ctrl Pts',(28.9822165729138,-0.587617535604954,
26.4791635476064));
#74836=CARTESIAN_POINT('Ctrl Pts',(29.3214777152758,-1.17523507120989,26.520830214273));
#74837=CARTESIAN_POINT('Ctrl Pts',(30.,-1.17523507120989,26.5624968809397));
#74838=CARTESIAN_POINT('Ctrl Pts',(30.6785222847241,-1.17523507120989,26.6041635476064));
#74839=CARTESIAN_POINT('Ctrl Pts',(31.0177834270861,-0.587617535604955,
26.645830214273));
#74840=CARTESIAN_POINT('Ctrl Pts',(31.3570445694482,-1.35453519623354E-14,
26.6874968809397));
#74841=CARTESIAN_POINT('Ctrl Pts',(31.0177834270861,0.587617535604927,26.7291635476064));
#74842=CARTESIAN_POINT('Ctrl Pts',(30.6785222847241,1.17523507120987,26.770830214273));
#74843=CARTESIAN_POINT('Ctrl Pts',(30.,1.17523507120987,26.8124968809397));
#74844=CARTESIAN_POINT('Ctrl Pts',(29.3214777152758,1.17523507120987,26.8541635476064));
#74845=CARTESIAN_POINT('Ctrl Pts',(28.9822165729138,0.587617535604928,26.895830214273));
#74846=CARTESIAN_POINT('Ctrl Pts',(28.6429554305518,-1.32141489532166E-14,
26.9374968809397));
#74847=CARTESIAN_POINT('Ctrl Pts',(28.9822165729138,-0.587617535604954,
26.9791635476064));
#74848=CARTESIAN_POINT('Ctrl Pts',(29.3214777152758,-1.17523507120989,27.020830214273));
#74849=CARTESIAN_POINT('Ctrl Pts',(30.,-1.17523507120989,27.0624968809397));
#74850=CARTESIAN_POINT('Ctrl Pts',(30.6785222847241,-1.17523507120989,27.1041635476064));
#74851=CARTESIAN_POINT('Ctrl Pts',(31.0177834270861,-0.587617535604955,
27.145830214273));
#74852=CARTESIAN_POINT('Ctrl Pts',(31.3570445694482,-1.35453519623354E-14,
27.1874968809397));
#74853=CARTESIAN_POINT('Ctrl Pts',(31.0177834270861,0.587617535604927,27.2291635476064));
#74854=CARTESIAN_POINT('Ctrl Pts',(30.6785222847241,1.17523507120987,27.270830214273));
#74855=CARTESIAN_POINT('Ctrl Pts',(30.,1.17523507120987,27.3124968809397));
#74856=CARTESIAN_POINT('Ctrl Pts',(29.3214777152758,1.17523507120987,27.3541635476064));
#74857=CARTESIAN_POINT('Ctrl Pts',(28.9822165729138,0.587617535604928,27.395830214273));
#74858=CARTESIAN_POINT('Ctrl Pts',(28.6429554305518,-1.32141489532166E-14,
27.4374968809397));
#74859=CARTESIAN_POINT('Ctrl Pts',(28.9822165729138,-0.587617535604954,
27.4791635476064));
#74860=CARTESIAN_POINT('Ctrl Pts',(29.3214777152758,-1.17523507120989,27.520830214273));
#74861=CARTESIAN_POINT('Ctrl Pts',(30.,-1.17523507120989,27.5624968809397));
#74862=CARTESIAN_POINT('Ctrl Pts',(30.6785222847241,-1.17523507120989,27.6041635476064));
#74863=CARTESIAN_POINT('Ctrl Pts',(31.0177834270861,-0.587617535604955,
27.645830214273));
#74864=CARTESIAN_POINT('Ctrl Pts',(31.3570445694482,-1.35453519623354E-14,
27.6874968809397));
#74865=CARTESIAN_POINT('Ctrl Pts',(31.0177834270861,0.587617535604927,27.7291635476064));
#74866=CARTESIAN_POINT('Ctrl Pts',(30.6785222847241,1.17523507120987,27.770830214273));
#74867=CARTESIAN_POINT('Ctrl Pts',(30.,1.17523507120987,27.8124968809397));
#74868=CARTESIAN_POINT('Ctrl Pts',(29.3214777152758,1.17523507120987,27.8541635476064));
#74869=CARTESIAN_POINT('Ctrl Pts',(28.9822165729138,0.587617535604928,27.895830214273));
#74870=CARTESIAN_POINT('Ctrl Pts',(28.6429554305518,-1.32141489532166E-14,
27.9374968809397));
#74871=CARTESIAN_POINT('Ctrl Pts',(28.9822165729138,-0.587617535604954,
27.9791635476064));
#74872=CARTESIAN_POINT('Ctrl Pts',(29.3214777152758,-1.17523507120989,28.020830214273));
#74873=CARTESIAN_POINT('Ctrl Pts',(30.,-1.17523507120989,28.0624968809397));
#74874=CARTESIAN_POINT('Ctrl Pts',(30.6785222847241,-1.17523507120989,28.1041635476064));
#74875=CARTESIAN_POINT('Ctrl Pts',(31.0177834270861,-0.587617535604955,
28.145830214273));
#74876=CARTESIAN_POINT('Ctrl Pts',(31.3570445694482,-1.35453519623354E-14,
28.1874968809397));
#74877=CARTESIAN_POINT('Ctrl Pts',(31.0177834270861,0.587617535604927,28.2291635476064));
#74878=CARTESIAN_POINT('Ctrl Pts',(30.6785222847241,1.17523507120987,28.270830214273));
#74879=CARTESIAN_POINT('Ctrl Pts',(30.,1.17523507120987,28.3124968809397));
#74880=CARTESIAN_POINT('Ctrl Pts',(29.3214777152758,1.17523507120987,28.3541635476064));
#74881=CARTESIAN_POINT('Ctrl Pts',(28.9822165729138,0.587617535604928,28.395830214273));
#74882=CARTESIAN_POINT('Ctrl Pts',(28.6429554305518,-1.32141489532166E-14,
28.4374968809397));
#74883=CARTESIAN_POINT('Ctrl Pts',(28.9822165729138,-0.587617535604954,
28.4791635476064));
#74884=CARTESIAN_POINT('Ctrl Pts',(29.3214777152758,-1.17523507120989,28.520830214273));
#74885=CARTESIAN_POINT('Ctrl Pts',(30.,-1.17523507120989,28.5624968809397));
#74886=CARTESIAN_POINT('Ctrl Pts',(30.6785222847241,-1.17523507120989,28.6041635476064));
#74887=CARTESIAN_POINT('Ctrl Pts',(31.0177834270861,-0.587617535604955,
28.645830214273));
#74888=CARTESIAN_POINT('Ctrl Pts',(31.3570445694482,-1.35453519623354E-14,
28.6874968809397));
#74889=CARTESIAN_POINT('Ctrl Pts',(31.0177834270861,0.587617535604927,28.7291635476064));
#74890=CARTESIAN_POINT('Ctrl Pts',(30.6785222847241,1.17523507120987,28.770830214273));
#74891=CARTESIAN_POINT('Ctrl Pts',(30.,1.17523507120987,28.8124968809397));
#74892=CARTESIAN_POINT('Ctrl Pts',(29.3214777152758,1.17523507120987,28.8541635476064));
#74893=CARTESIAN_POINT('Ctrl Pts',(28.9822165729138,0.587617535604928,28.895830214273));
#74894=CARTESIAN_POINT('Ctrl Pts',(28.6429554305518,-1.32141489532166E-14,
28.9374968809397));
#74895=CARTESIAN_POINT('Ctrl Pts',(28.9822165729138,-0.587617535604954,
28.9791635476064));
#74896=CARTESIAN_POINT('Ctrl Pts',(29.3214777152758,-1.17523507120989,29.020830214273));
#74897=CARTESIAN_POINT('Ctrl Pts',(30.,-1.17523507120989,29.0624968809397));
#74898=CARTESIAN_POINT('Ctrl Pts',(30.6785222847241,-1.17523507120989,29.1041635476064));
#74899=CARTESIAN_POINT('Ctrl Pts',(31.0177834270861,-0.587617535604955,
29.145830214273));
#74900=CARTESIAN_POINT('Ctrl Pts',(31.3570445694482,-1.35453519623354E-14,
29.1874968809397));
#74901=CARTESIAN_POINT('Ctrl Pts',(31.0177834270861,0.587617535604927,29.2291635476064));
#74902=CARTESIAN_POINT('Ctrl Pts',(30.6785222847241,1.17523507120987,29.270830214273));
#74903=CARTESIAN_POINT('Ctrl Pts',(30.,1.17523507120987,29.3124968809397));
#74904=CARTESIAN_POINT('Ctrl Pts',(29.3214777152758,1.17523507120987,29.3541635476064));
#74905=CARTESIAN_POINT('Ctrl Pts',(28.9822165729138,0.587617535604928,29.395830214273));
#74906=CARTESIAN_POINT('Ctrl Pts',(28.6429554305518,-1.32141489532166E-14,
29.4374968809397));
#74907=CARTESIAN_POINT('Ctrl Pts',(28.9822165729138,-0.587617535604954,
29.4791635476064));
#74908=CARTESIAN_POINT('Ctrl Pts',(29.3214777152758,-1.17523507120989,29.520830214273));
#74909=CARTESIAN_POINT('Ctrl Pts',(30.,-1.17523507120989,29.5624968809397));
#74910=CARTESIAN_POINT('Ctrl Pts',(30.6785222847241,-1.17523507120989,29.6041635476064));
#74911=CARTESIAN_POINT('Ctrl Pts',(31.0177834270861,-0.587617535604955,
29.645830214273));
#74912=CARTESIAN_POINT('Ctrl Pts',(31.3570445694482,-1.35453519623354E-14,
29.6874968809397));
#74913=CARTESIAN_POINT('Ctrl Pts',(31.0177834270861,0.587617535604927,29.7291635476064));
#74914=CARTESIAN_POINT('Ctrl Pts',(30.6785222847241,1.17523507120987,29.770830214273));
#74915=CARTESIAN_POINT('Ctrl Pts',(30.,1.17523507120987,29.8124968809397));
#74916=CARTESIAN_POINT('Ctrl Pts',(29.3214777152758,1.17523507120987,29.8541635476064));
#74917=CARTESIAN_POINT('Ctrl Pts',(28.9822165729138,0.587617535604928,29.895830214273));
#74918=CARTESIAN_POINT('Ctrl Pts',(28.6429554305518,-1.32141489532166E-14,
29.9374968809397));
#74919=CARTESIAN_POINT('Ctrl Pts',(28.9822165729138,-0.587617535604954,
29.9791635476064));
#74920=CARTESIAN_POINT('Ctrl Pts',(29.3214777152758,-1.17523507120989,30.020830214273));
#74921=CARTESIAN_POINT('Ctrl Pts',(30.,-1.17523507120989,30.0624968809397));
#74922=CARTESIAN_POINT('Ctrl Pts',(30.6785222847241,-1.17523507120989,30.1041635476064));
#74923=CARTESIAN_POINT('Ctrl Pts',(31.0177834270861,-0.587617535604955,
30.145830214273));
#74924=CARTESIAN_POINT('Ctrl Pts',(31.3570445694482,-1.35453519623354E-14,
30.1874968809397));
#74925=CARTESIAN_POINT('Ctrl Pts',(31.0177834270861,0.587617535604927,30.2291635476064));
#74926=CARTESIAN_POINT('Ctrl Pts',(30.6785222847241,1.17523507120987,30.270830214273));
#74927=CARTESIAN_POINT('Ctrl Pts',(30.,1.17523507120987,30.3124968809397));
#74928=CARTESIAN_POINT('Ctrl Pts',(29.3214777152758,1.17523507120987,30.3541635476064));
#74929=CARTESIAN_POINT('Ctrl Pts',(28.9822165729138,0.587617535604928,30.395830214273));
#74930=CARTESIAN_POINT('Ctrl Pts',(28.6429554305518,-1.32141489532166E-14,
30.4374968809397));
#74931=CARTESIAN_POINT('Ctrl Pts',(28.9822165729138,-0.587617535604954,
30.4791635476064));
#74932=CARTESIAN_POINT('Ctrl Pts',(29.3214777152758,-1.17523507120989,30.520830214273));
#74933=CARTESIAN_POINT('Ctrl Pts',(30.,-1.17523507120989,30.5624968809397));
#74934=CARTESIAN_POINT('Ctrl Pts',(30.6785222847241,-1.17523507120989,30.6041635476064));
#74935=CARTESIAN_POINT('Ctrl Pts',(31.0177834270861,-0.587617535604955,
30.645830214273));
#74936=CARTESIAN_POINT('Ctrl Pts',(31.3570445694482,-1.35453519623354E-14,
30.6874968809397));
#74937=CARTESIAN_POINT('Ctrl Pts',(31.0177834270861,0.587617535604927,30.7291635476064));
#74938=CARTESIAN_POINT('Ctrl Pts',(30.6785222847241,1.17523507120987,30.770830214273));
#74939=CARTESIAN_POINT('Ctrl Pts',(30.,1.17523507120987,30.8124968809397));
#74940=CARTESIAN_POINT('Ctrl Pts',(29.3214777152758,1.17523507120987,30.8541635476064));
#74941=CARTESIAN_POINT('Ctrl Pts',(28.9822165729138,0.587617535604928,30.895830214273));
#74942=CARTESIAN_POINT('Ctrl Pts',(28.6429554305518,-1.32141489532166E-14,
30.9374968809397));
#74943=CARTESIAN_POINT('Ctrl Pts',(28.9822165729138,-0.587617535604954,
30.9791635476064));
#74944=CARTESIAN_POINT('Ctrl Pts',(29.3214777152758,-1.17523507120989,31.020830214273));
#74945=CARTESIAN_POINT('Ctrl Pts',(30.,-1.17523507120989,31.0624968809397));
#74946=CARTESIAN_POINT('Ctrl Pts',(30.6785222847241,-1.17523507120989,31.1041635476064));
#74947=CARTESIAN_POINT('Ctrl Pts',(31.0177834270861,-0.587617535604955,
31.145830214273));
#74948=CARTESIAN_POINT('Ctrl Pts',(31.3570445694482,-1.35453519623354E-14,
31.1874968809397));
#74949=CARTESIAN_POINT('Ctrl Pts',(31.0177834270861,0.587617535604927,31.2291635476064));
#74950=CARTESIAN_POINT('Ctrl Pts',(30.6785222847241,1.17523507120987,31.270830214273));
#74951=CARTESIAN_POINT('Ctrl Pts',(30.,1.17523507120987,31.3124968809397));
#74952=CARTESIAN_POINT('',(30.,-1.50000000000002,30.75));
#74953=CARTESIAN_POINT('Origin',(30.,-1.24258096838242E-13,1029.88397459622));
#74954=CARTESIAN_POINT('Origin',(30.06875,2.82851012598683,15.7235432561772));
#74955=CARTESIAN_POINT('',(30.012548982272,2.70302030326666,15.7235432561772));
#74956=CARTESIAN_POINT('Origin',(30.,2.70864040503946,15.7235432561772));
#74957=CARTESIAN_POINT('',(29.987451017728,2.70302030326666,15.7235432561772));
#74958=CARTESIAN_POINT('Origin',(29.987451017728,2.70302030326666,15.7235432561772));
#74959=CARTESIAN_POINT('Origin',(30.2904604134361,2.81439671040465,15.7235432561772));
#74960=CARTESIAN_POINT('',(30.224586826676,2.69370321195774,15.7235432561772));
#74961=CARTESIAN_POINT('Origin',(30.2125174768313,2.70029057063376,15.7235432561772));
#74962=CARTESIAN_POINT('',(30.1995662307806,2.69567237556048,15.7235432561772));
#74963=CARTESIAN_POINT('Origin',(30.1995662307806,2.69567237556048,15.7235432561772));
#74964=CARTESIAN_POINT('Origin',(29.8466157199522,2.82518483606723,15.7235432561772));
#74965=CARTESIAN_POINT('',(29.8004337692194,2.69567237556048,15.7235432561772));
#74966=CARTESIAN_POINT('Origin',(29.7874825231687,2.70029057063376,15.7235432561772));
#74967=CARTESIAN_POINT('',(29.775413173324,2.69370321195775,15.7235432561772));
#74968=CARTESIAN_POINT('Origin',(29.775413173324,2.69370321195775,15.7235432561772));
#74969=CARTESIAN_POINT('Origin',(29.6254271049963,2.804441342164,15.7235432561772));
#74970=CARTESIAN_POINT('',(29.589548948342,2.67170473125694,15.7235432561772));
#74971=CARTESIAN_POINT('Origin',(29.5762752872513,2.67529254692237,15.7235432561772));
#74972=CARTESIAN_POINT('',(29.5647599813892,2.6677785445999,15.7235432561772));
#74973=CARTESIAN_POINT('Origin',(29.5647599813892,2.6677785445999,15.7235432561772));
#74974=CARTESIAN_POINT('Origin',(29.4065478564962,2.76640753481494,15.7235432561772));
#74975=CARTESIAN_POINT('',(29.3811946946869,2.63126513885323,15.7235432561772));
#74976=CARTESIAN_POINT('Origin',(29.3676804550908,2.63380045503416,15.7235432561772));
#74977=CARTESIAN_POINT('',(29.3567901889011,2.6254061353882,15.7235432561772));
#74978=CARTESIAN_POINT('Origin',(29.3567901889011,2.6254061353882,15.7235432561772));
#74979=CARTESIAN_POINT('Origin',(29.1913274378037,2.71131790508989,15.7235432561772));
#74980=CARTESIAN_POINT('',(29.1766555815128,2.57460292188403,15.7235432561772));
#74981=CARTESIAN_POINT('Origin',(29.1629840831922,2.57607010751313,15.7235432561772));
#74982=CARTESIAN_POINT('',(29.1527859987874,2.56684722431571,15.7235432561772));
#74983=CARTESIAN_POINT('Origin',(29.1527859987874,2.56684722431571,15.7235432561772));
#74984=CARTESIAN_POINT('Origin',(28.9810927543681,2.63951209887526,15.7235432561772));
#74985=CARTESIAN_POINT('',(28.9771926604684,2.50206742175908,15.7235432561772));
#74986=CARTESIAN_POINT('Origin',(28.9634481927567,2.50245743114905,15.7235432561772));
#74987=CARTESIAN_POINT('',(28.9540051647184,2.49246284654199,15.7235432561772));
#74988=CARTESIAN_POINT('Origin',(28.9540051647184,2.49246284654199,15.7235432561772));
#74989=CARTESIAN_POINT('Origin',(28.7771399729228,2.55143282284423,15.7235432561772));
#74990=CARTESIAN_POINT('Origin',(28.7616732366375,2.40271160649133,15.7235432561772));
#74991=CARTESIAN_POINT('Origin',(28.5807265301867,2.44762311502286,15.7235432561772));
#74992=CARTESIAN_POINT('Origin',(28.5769760048382,2.29814685040398,15.7235432561772));
#74993=CARTESIAN_POINT('Origin',(28.3930633803483,2.32872299678009,15.7235432561772));
#74994=CARTESIAN_POINT('Origin',(28.4010521891726,2.1794132547725,15.7235432561772));
#74995=CARTESIAN_POINT('Origin',(28.2153075291307,2.1954655268832,15.7235432561772));
#74996=CARTESIAN_POINT('Origin',(28.2349864184648,2.0472428516969,15.7235432561772));
#74997=CARTESIAN_POINT('Origin',(28.0485549004665,2.0486722819467,15.7235432561772));
#74998=CARTESIAN_POINT('Origin',(28.0798025434137,1.90245051566326,15.7235432561772));
#74999=CARTESIAN_POINT('Origin',(27.8938335797622,1.88924829113933,15.7235432561772));
#75000=CARTESIAN_POINT('Origin',(27.9364573242129,1.74592893957157,15.7235432561772));
#75001=CARTESIAN_POINT('Origin',(27.7520974754101,1.71817645637828,15.7235432561772));
#75002=CARTESIAN_POINT('Origin',(27.805834531806,1.57864313098712,15.7235432561772));
#75003=CARTESIAN_POINT('Origin',(27.6242204376256,1.53651149241201,15.7235432561772));
#75004=CARTESIAN_POINT('Origin',(27.6887394991445,1.40162446254803,15.7235432561772));
#75005=CARTESIAN_POINT('Origin',(27.5109908708699,1.3453734241531,15.7235432561772));
#75006=CARTESIAN_POINT('Origin',(27.5858941560429,1.2159643132099,15.7235432561772));
#75007=CARTESIAN_POINT('Origin',(30.5103800418355,2.78293160322096,15.7235432561772));
#75008=CARTESIAN_POINT('',(30.4352400186108,2.66777854459989,15.7235432561772));
#75009=CARTESIAN_POINT('Origin',(30.4237247127487,2.67529254692237,15.7235432561772));
#75010=CARTESIAN_POINT('',(30.410451051658,2.67170473125694,15.7235432561772));
#75011=CARTESIAN_POINT('Origin',(30.410451051658,2.67170473125694,15.7235432561772));
#75012=CARTESIAN_POINT('Origin',(30.7271530075584,2.73430879728474,15.7235432561772));
#75013=CARTESIAN_POINT('',(30.6432098110989,2.62540613538819,15.7235432561772));
#75014=CARTESIAN_POINT('Origin',(30.6323195449092,2.63380045503415,15.7235432561772));
#75015=CARTESIAN_POINT('',(30.6188053053131,2.63126513885322,15.7235432561772));
#75016=CARTESIAN_POINT('Origin',(30.6188053053131,2.63126513885322,15.7235432561772));
#75017=CARTESIAN_POINT('Origin',(30.9394428331868,2.66882806836332,15.7235432561772));
#75018=CARTESIAN_POINT('',(30.8472140012126,2.5668472243157,15.7235432561772));
#75019=CARTESIAN_POINT('Origin',(30.8370159168078,2.57607010751312,15.7235432561772));
#75020=CARTESIAN_POINT('',(30.8233444184872,2.57460292188402,15.7235432561772));
#75021=CARTESIAN_POINT('Origin',(30.8233444184872,2.57460292188402,15.7235432561772));
#75022=CARTESIAN_POINT('Origin',(31.1459406813522,2.58689312692505,15.7235432561772));
#75023=CARTESIAN_POINT('',(31.0459948352816,2.49246284654197,15.7235432561772));
#75024=CARTESIAN_POINT('Origin',(31.0365518072432,2.50245743114904,15.7235432561772));
#75025=CARTESIAN_POINT('',(31.0228073395316,2.50206742175906,15.7235432561772));
#75026=CARTESIAN_POINT('Origin',(31.0228073395316,2.50206742175906,15.7235432561772));
#75027=CARTESIAN_POINT('Origin',(31.3453734241531,2.48900912913003,15.7235432561772));
#75028=CARTESIAN_POINT('',(31.2383267633625,2.40271160649132,15.7235432561772));
#75029=CARTESIAN_POINT('Origin',(31.2296970110986,2.41341627257038,15.7235432561772));
#75030=CARTESIAN_POINT('',(31.2159643132099,2.41410584395711,15.7235432561772));
#75031=CARTESIAN_POINT('Origin',(31.2159643132099,2.41410584395711,15.7235432561772));
#75032=CARTESIAN_POINT('Origin',(31.536511492412,2.3757795623744,15.7235432561772));
#75033=CARTESIAN_POINT('',(31.4230239951618,2.29814685040396,15.7235432561772));
#75034=CARTESIAN_POINT('Origin',(31.4152607239647,2.30949560012898,15.7235432561772));
#75035=CARTESIAN_POINT('',(31.401624462548,2.3112605008555,15.7235432561772));
#75036=CARTESIAN_POINT('Origin',(31.401624462548,2.3112605008555,15.7235432561772));
#75037=CARTESIAN_POINT('Origin',(31.7181764563782,2.24790252458986,15.7235432561772));
#75038=CARTESIAN_POINT('',(31.5989478108274,2.17941325477248,15.7235432561772));
#75039=CARTESIAN_POINT('Origin',(31.5920988838457,2.19133611932756,15.7235432561772));
#75040=CARTESIAN_POINT('',(31.5786431309871,2.19416546819402,15.7235432561772));
#75041=CARTESIAN_POINT('Origin',(31.5786431309871,2.19416546819402,15.7235432561772));
#75042=CARTESIAN_POINT('Origin',(31.8892482911393,2.10616642023777,15.7235432561772));
#75043=CARTESIAN_POINT('',(31.7650135815352,2.04724285169688,15.7235432561772));
#75044=CARTESIAN_POINT('Origin',(31.7591212246811,2.05966632265728,15.7235432561772));
#75045=CARTESIAN_POINT('',(31.7459289395715,2.06354267578706,15.7235432561772));
#75046=CARTESIAN_POINT('Origin',(31.7459289395715,2.06354267578706,15.7235432561772));
#75047=CARTESIAN_POINT('Origin',(32.0486722819467,1.95144509953352,15.7235432561772));
#75048=CARTESIAN_POINT('',(31.9201974565863,1.90245051566323,15.7235432561772));
#75049=CARTESIAN_POINT('Origin',(31.9152979981993,1.91529799819927,15.7235432561772));
#75050=CARTESIAN_POINT('',(31.9024505156632,1.9201974565863,15.7235432561772));
#75051=CARTESIAN_POINT('Origin',(31.9024505156632,1.9201974565863,15.7235432561772));
#75052=CARTESIAN_POINT('Origin',(32.1954655268832,1.7846924708693,15.7235432561772));
#75053=CARTESIAN_POINT('',(32.0635426757871,1.74592893957153,15.7235432561772));
#75054=CARTESIAN_POINT('Origin',(32.0596663226573,1.75912122468115,15.7235432561772));
#75055=CARTESIAN_POINT('',(32.0472428516969,1.76501358153524,15.7235432561772));
#75056=CARTESIAN_POINT('Origin',(32.0472428516969,1.76501358153524,15.7235432561772));
#75057=CARTESIAN_POINT('Origin',(32.3287229967801,1.6069366196517,15.7235432561772));
#75058=CARTESIAN_POINT('',(32.194165468194,1.57864313098709,15.7235432561772));
#75059=CARTESIAN_POINT('Origin',(32.1913361193276,1.59209888384569,15.7235432561772));
#75060=CARTESIAN_POINT('',(32.1794132547725,1.59894781082743,15.7235432561772));
#75061=CARTESIAN_POINT('Origin',(32.1794132547725,1.59894781082743,15.7235432561772));
#75062=CARTESIAN_POINT('Origin',(32.4476231150228,1.41927346981329,15.7235432561772));
#75063=CARTESIAN_POINT('',(32.3112605008555,1.401624462548,15.7235432561772));
#75064=CARTESIAN_POINT('Origin',(32.309495600129,1.41526072396473,15.7235432561772));
#75065=CARTESIAN_POINT('',(32.298146850404,1.42302399516178,15.7235432561772));
#75066=CARTESIAN_POINT('Origin',(32.298146850404,1.42302399516178,15.7235432561772));
#75067=CARTESIAN_POINT('Origin',(32.5514328228442,1.22286002707717,15.7235432561772));
#75068=CARTESIAN_POINT('',(32.4141058439571,1.21596431320987,15.7235432561772));
#75069=CARTESIAN_POINT('Origin',(32.4134162725704,1.22969701109858,15.7235432561772));
#75070=CARTESIAN_POINT('',(32.4027116064913,1.23832676336245,15.7235432561772));
#75071=CARTESIAN_POINT('Origin',(32.4027116064913,1.23832676336245,15.7235432561772));
#75072=CARTESIAN_POINT('Origin',(32.6395120988752,1.01890724563189,15.7235432561772));
#75073=CARTESIAN_POINT('',(32.5020674217591,1.02280733953163,15.7235432561772));
#75074=CARTESIAN_POINT('Origin',(32.502457431149,1.03655180724325,15.7235432561772));
#75075=CARTESIAN_POINT('',(32.492462846542,1.04599483528156,15.7235432561772));
#75076=CARTESIAN_POINT('Origin',(32.492462846542,1.04599483528156,15.7235432561772));
#75077=CARTESIAN_POINT('Origin',(32.7113179050899,0.808672562196245,15.7235432561772));
#75078=CARTESIAN_POINT('',(32.574602921884,0.823344418487232,15.7235432561772));
#75079=CARTESIAN_POINT('Origin',(32.5760701075131,0.837015916807817,15.7235432561772));
#75080=CARTESIAN_POINT('',(32.5668472243157,0.84721400121258,15.7235432561772));
#75081=CARTESIAN_POINT('Origin',(32.5668472243157,0.84721400121258,15.7235432561772));
#75082=CARTESIAN_POINT('Origin',(32.7664075348149,0.593452143503749,15.7235432561772));
#75083=CARTESIAN_POINT('',(32.6312651388532,0.618805305313054,15.7235432561772));
#75084=CARTESIAN_POINT('Origin',(32.6338004550341,0.632319544909225,15.7235432561772));
#75085=CARTESIAN_POINT('',(32.6254061353882,0.64320981109888,15.7235432561772));
#75086=CARTESIAN_POINT('Origin',(32.6254061353882,0.64320981109888,15.7235432561772));
#75087=CARTESIAN_POINT('Origin',(32.804441342164,0.37457289500369,15.7235432561772));
#75088=CARTESIAN_POINT('',(32.6717047312569,0.410451051657977,15.7235432561772));
#75089=CARTESIAN_POINT('Origin',(32.6752925469224,0.423724712748682,15.7235432561772));
#75090=CARTESIAN_POINT('',(32.6677785445999,0.435240018610789,15.7235432561772));
#75091=CARTESIAN_POINT('Origin',(32.6677785445999,0.435240018610789,15.7235432561772));
#75092=CARTESIAN_POINT('Origin',(32.8251848360672,0.153384280047806,15.7235432561772));
#75093=CARTESIAN_POINT('',(32.6956723755605,0.199566230780603,15.7235432561772));
#75094=CARTESIAN_POINT('Origin',(32.7002905706337,0.212517476831278,15.7235432561772));
#75095=CARTESIAN_POINT('',(32.6937032119577,0.224586826675969,15.7235432561772));
#75096=CARTESIAN_POINT('Origin',(32.6937032119577,0.224586826675969,15.7235432561772));
#75097=CARTESIAN_POINT('Origin',(32.8285101259868,-0.0687500000000229,15.7235432561772));
#75098=CARTESIAN_POINT('',(32.7030203032667,-0.0125489822720396,15.7235432561772));
#75099=CARTESIAN_POINT('Origin',(32.7086404050395,-2.31188656783185E-14,
15.7235432561772));
#75100=CARTESIAN_POINT('',(32.7030203032667,0.0125489822719939,15.7235432561772));
#75101=CARTESIAN_POINT('Origin',(32.7030203032667,0.0125489822719939,15.7235432561772));
#75102=CARTESIAN_POINT('Origin',(32.8143967104046,-0.290460413436156,15.7235432561772));
#75103=CARTESIAN_POINT('',(32.6937032119577,-0.224586826676015,15.7235432561772));
#75104=CARTESIAN_POINT('Origin',(32.7002905706337,-0.212517476831324,15.7235432561772));
#75105=CARTESIAN_POINT('',(32.6956723755605,-0.199566230780649,15.7235432561772));
#75106=CARTESIAN_POINT('Origin',(32.6956723755605,-0.199566230780649,15.7235432561772));
#75107=CARTESIAN_POINT('Origin',(32.7829316032209,-0.510380041835567,15.7235432561772));
#75108=CARTESIAN_POINT('',(32.6677785445999,-0.435240018610835,15.7235432561772));
#75109=CARTESIAN_POINT('Origin',(32.6752925469224,-0.423724712748728,15.7235432561772));
#75110=CARTESIAN_POINT('',(32.6717047312569,-0.410451051658023,15.7235432561772));
#75111=CARTESIAN_POINT('Origin',(32.6717047312569,-0.410451051658023,15.7235432561772));
#75112=CARTESIAN_POINT('Origin',(32.7343087972847,-0.727153007558476,15.7235432561772));
#75113=CARTESIAN_POINT('',(32.6254061353882,-0.643209811098926,15.7235432561772));
#75114=CARTESIAN_POINT('Origin',(32.6338004550341,-0.632319544909271,15.7235432561772));
#75115=CARTESIAN_POINT('',(32.6312651388532,-0.6188053053131,15.7235432561772));
#75116=CARTESIAN_POINT('Origin',(32.6312651388532,-0.6188053053131,15.7235432561772));
#75117=CARTESIAN_POINT('Origin',(32.6688280683633,-0.939442833186874,15.7235432561772));
#75118=CARTESIAN_POINT('',(32.5668472243157,-0.847214001212625,15.7235432561772));
#75119=CARTESIAN_POINT('Origin',(32.5760701075131,-0.837015916807863,15.7235432561772));
#75120=CARTESIAN_POINT('',(32.574602921884,-0.823344418487278,15.7235432561772));
#75121=CARTESIAN_POINT('Origin',(32.574602921884,-0.823344418487278,15.7235432561772));
#75122=CARTESIAN_POINT('Origin',(32.586893126925,-1.14594068135223,15.7235432561772));
#75123=CARTESIAN_POINT('',(32.492462846542,-1.0459948352816,15.7235432561772));
#75124=CARTESIAN_POINT('Origin',(32.502457431149,-1.0365518072433,15.7235432561772));
#75125=CARTESIAN_POINT('',(32.5020674217591,-1.02280733953168,15.7235432561772));
#75126=CARTESIAN_POINT('Origin',(32.5020674217591,-1.02280733953168,15.7235432561772));
#75127=CARTESIAN_POINT('Origin',(32.48900912913,-1.34537342415311,15.7235432561772));
#75128=CARTESIAN_POINT('',(32.4027116064913,-1.2383267633625,15.7235432561772));
#75129=CARTESIAN_POINT('Origin',(32.4134162725704,-1.22969701109862,15.7235432561772));
#75130=CARTESIAN_POINT('',(32.4141058439571,-1.21596431320991,15.7235432561772));
#75131=CARTESIAN_POINT('Origin',(32.4141058439571,-1.21596431320991,15.7235432561772));
#75132=CARTESIAN_POINT('Origin',(32.3757795623744,-1.53651149241202,15.7235432561772));
#75133=CARTESIAN_POINT('',(32.2981468504039,-1.42302399516182,15.7235432561772));
#75134=CARTESIAN_POINT('Origin',(32.309495600129,-1.41526072396478,15.7235432561772));
#75135=CARTESIAN_POINT('',(32.3112605008555,-1.40162446254804,15.7235432561772));
#75136=CARTESIAN_POINT('Origin',(32.3112605008555,-1.40162446254804,15.7235432561772));
#75137=CARTESIAN_POINT('Origin',(32.2479025245898,-1.71817645637829,15.7235432561772));
#75138=CARTESIAN_POINT('',(32.1794132547725,-1.59894781082747,15.7235432561772));
#75139=CARTESIAN_POINT('Origin',(32.1913361193275,-1.59209888384574,15.7235432561772));
#75140=CARTESIAN_POINT('',(32.194165468194,-1.57864313098713,15.7235432561772));
#75141=CARTESIAN_POINT('Origin',(32.194165468194,-1.57864313098713,15.7235432561772));
#75142=CARTESIAN_POINT('Origin',(32.1061664202378,-1.88924829113934,15.7235432561772));
#75143=CARTESIAN_POINT('',(32.0472428516969,-1.76501358153528,15.7235432561772));
#75144=CARTESIAN_POINT('Origin',(32.0596663226573,-1.75912122468119,15.7235432561772));
#75145=CARTESIAN_POINT('',(32.063542675787,-1.74592893957158,15.7235432561772));
#75146=CARTESIAN_POINT('Origin',(32.063542675787,-1.74592893957158,15.7235432561772));
#75147=CARTESIAN_POINT('Origin',(31.9514450995335,-2.04867228194671,15.7235432561772));
#75148=CARTESIAN_POINT('',(31.9024505156632,-1.92019745658634,15.7235432561772));
#75149=CARTESIAN_POINT('Origin',(31.9152979981993,-1.91529799819931,15.7235432561772));
#75150=CARTESIAN_POINT('',(31.9201974565863,-1.90245051566327,15.7235432561772));
#75151=CARTESIAN_POINT('Origin',(31.9201974565863,-1.90245051566327,15.7235432561772));
#75152=CARTESIAN_POINT('Origin',(31.7846924708693,-2.19546552688321,15.7235432561772));
#75153=CARTESIAN_POINT('',(31.7459289395715,-2.0635426757871,15.7235432561772));
#75154=CARTESIAN_POINT('Origin',(31.7591212246811,-2.05966632265732,15.7235432561772));
#75155=CARTESIAN_POINT('',(31.7650135815352,-2.04724285169692,15.7235432561772));
#75156=CARTESIAN_POINT('Origin',(31.7650135815352,-2.04724285169692,15.7235432561772));
#75157=CARTESIAN_POINT('Origin',(31.6069366196517,-2.32872299678011,15.7235432561772));
#75158=CARTESIAN_POINT('',(31.5786431309871,-2.19416546819406,15.7235432561772));
#75159=CARTESIAN_POINT('Origin',(31.5920988838457,-2.1913361193276,15.7235432561772));
#75160=CARTESIAN_POINT('',(31.5989478108274,-2.17941325477251,15.7235432561772));
#75161=CARTESIAN_POINT('Origin',(31.5989478108274,-2.17941325477251,15.7235432561772));
#75162=CARTESIAN_POINT('Origin',(31.4192734698133,-2.44762311502288,15.7235432561772));
#75163=CARTESIAN_POINT('',(31.401624462548,-2.31126050085554,15.7235432561772));
#75164=CARTESIAN_POINT('Origin',(31.4152607239647,-2.30949560012901,15.7235432561772));
#75165=CARTESIAN_POINT('',(31.4230239951618,-2.29814685040399,15.7235432561772));
#75166=CARTESIAN_POINT('Origin',(31.4230239951618,-2.29814685040399,15.7235432561772));
#75167=CARTESIAN_POINT('Origin',(31.2228600270771,-2.55143282284425,15.7235432561772));
#75168=CARTESIAN_POINT('',(31.2159643132098,-2.41410584395714,15.7235432561772));
#75169=CARTESIAN_POINT('Origin',(31.2296970110986,-2.41341627257041,15.7235432561772));
#75170=CARTESIAN_POINT('',(31.2383267633624,-2.40271160649135,15.7235432561772));
#75171=CARTESIAN_POINT('Origin',(31.2383267633624,-2.40271160649135,15.7235432561772));
#75172=CARTESIAN_POINT('Origin',(31.0189072456319,-2.63951209887528,15.7235432561772));
#75173=CARTESIAN_POINT('',(31.0228073395316,-2.5020674217591,15.7235432561772));
#75174=CARTESIAN_POINT('Origin',(31.0365518072432,-2.50245743114907,15.7235432561772));
#75175=CARTESIAN_POINT('',(31.0459948352815,-2.49246284654201,15.7235432561772));
#75176=CARTESIAN_POINT('Origin',(31.0459948352815,-2.49246284654201,15.7235432561772));
#75177=CARTESIAN_POINT('Origin',(30.8086725621962,-2.71131790508991,15.7235432561772));
#75178=CARTESIAN_POINT('',(30.8233444184872,-2.57460292188405,15.7235432561772));
#75179=CARTESIAN_POINT('Origin',(30.8370159168078,-2.57607010751315,15.7235432561772));
#75180=CARTESIAN_POINT('',(30.8472140012126,-2.56684722431573,15.7235432561772));
#75181=CARTESIAN_POINT('Origin',(30.8472140012126,-2.56684722431573,15.7235432561772));
#75182=CARTESIAN_POINT('Origin',(30.5934521435037,-2.76640753481496,15.7235432561772));
#75183=CARTESIAN_POINT('',(30.618805305313,-2.63126513885325,15.7235432561772));
#75184=CARTESIAN_POINT('Origin',(30.6323195449092,-2.63380045503418,15.7235432561772));
#75185=CARTESIAN_POINT('',(30.6432098110989,-2.62540613538822,15.7235432561772));
#75186=CARTESIAN_POINT('Origin',(30.6432098110989,-2.62540613538822,15.7235432561772));
#75187=CARTESIAN_POINT('Origin',(30.3745728950037,-2.80444134216402,15.7235432561772));
#75188=CARTESIAN_POINT('',(30.410451051658,-2.67170473125697,15.7235432561772));
#75189=CARTESIAN_POINT('Origin',(30.4237247127487,-2.67529254692239,15.7235432561772));
#75190=CARTESIAN_POINT('',(30.4352400186108,-2.66777854459992,15.7235432561772));
#75191=CARTESIAN_POINT('Origin',(30.4352400186108,-2.66777854459992,15.7235432561772));
#75192=CARTESIAN_POINT('Origin',(30.1533842800478,-2.82518483606726,15.7235432561772));
#75193=CARTESIAN_POINT('',(30.1995662307806,-2.69567237556051,15.7235432561772));
#75194=CARTESIAN_POINT('Origin',(30.2125174768313,-2.70029057063379,15.7235432561772));
#75195=CARTESIAN_POINT('',(30.224586826676,-2.69370321195777,15.7235432561772));
#75196=CARTESIAN_POINT('Origin',(30.224586826676,-2.69370321195777,15.7235432561772));
#75197=CARTESIAN_POINT('Origin',(29.93125,-2.82851012598686,15.7235432561772));
#75198=CARTESIAN_POINT('',(29.987451017728,-2.70302030326669,15.7235432561772));
#75199=CARTESIAN_POINT('Origin',(30.,-2.70864040503949,15.7235432561772));
#75200=CARTESIAN_POINT('',(30.012548982272,-2.70302030326669,15.7235432561772));
#75201=CARTESIAN_POINT('Origin',(30.012548982272,-2.70302030326669,15.7235432561772));
#75202=CARTESIAN_POINT('Origin',(29.7095395865638,-2.81439671040468,15.7235432561772));
#75203=CARTESIAN_POINT('',(29.775413173324,-2.69370321195777,15.7235432561772));
#75204=CARTESIAN_POINT('Origin',(29.7874825231687,-2.70029057063378,15.7235432561772));
#75205=CARTESIAN_POINT('',(29.8004337692193,-2.6956723755605,15.7235432561772));
#75206=CARTESIAN_POINT('Origin',(29.8004337692193,-2.6956723755605,15.7235432561772));
#75207=CARTESIAN_POINT('Origin',(29.4896199581644,-2.78293160322098,15.7235432561772));
#75208=CARTESIAN_POINT('',(29.5647599813891,-2.66777854459992,15.7235432561772));
#75209=CARTESIAN_POINT('Origin',(29.5762752872513,-2.67529254692239,15.7235432561772));
#75210=CARTESIAN_POINT('',(29.589548948342,-2.67170473125696,15.7235432561772));
#75211=CARTESIAN_POINT('Origin',(29.589548948342,-2.67170473125696,15.7235432561772));
#75212=CARTESIAN_POINT('Origin',(29.2728469924415,-2.73430879728476,15.7235432561772));
#75213=CARTESIAN_POINT('',(29.3567901889011,-2.62540613538822,15.7235432561772));
#75214=CARTESIAN_POINT('Origin',(29.3676804550907,-2.63380045503417,15.7235432561772));
#75215=CARTESIAN_POINT('',(29.3811946946869,-2.63126513885324,15.7235432561772));
#75216=CARTESIAN_POINT('Origin',(29.3811946946869,-2.63126513885324,15.7235432561772));
#75217=CARTESIAN_POINT('Origin',(29.0605571668131,-2.66882806836334,15.7235432561772));
#75218=CARTESIAN_POINT('',(29.1527859987874,-2.56684722431572,15.7235432561772));
#75219=CARTESIAN_POINT('Origin',(29.1629840831921,-2.57607010751314,15.7235432561772));
#75220=CARTESIAN_POINT('',(29.1766555815127,-2.57460292188404,15.7235432561772));
#75221=CARTESIAN_POINT('Origin',(29.1766555815127,-2.57460292188404,15.7235432561772));
#75222=CARTESIAN_POINT('Origin',(28.8540593186477,-2.58689312692507,15.7235432561772));
#75223=CARTESIAN_POINT('',(28.9540051647184,-2.49246284654199,15.7235432561772));
#75224=CARTESIAN_POINT('Origin',(28.9634481927567,-2.50245743114906,15.7235432561772));
#75225=CARTESIAN_POINT('',(28.9771926604683,-2.50206742175908,15.7235432561772));
#75226=CARTESIAN_POINT('Origin',(28.9771926604683,-2.50206742175908,15.7235432561772));
#75227=CARTESIAN_POINT('Origin',(28.6546265758469,-2.48900912913005,15.7235432561772));
#75228=CARTESIAN_POINT('',(28.7616732366375,-2.40271160649133,15.7235432561772));
#75229=CARTESIAN_POINT('Origin',(28.7703029889014,-2.4134162725704,15.7235432561772));
#75230=CARTESIAN_POINT('',(28.7840356867901,-2.41410584395713,15.7235432561772));
#75231=CARTESIAN_POINT('Origin',(28.7840356867901,-2.41410584395713,15.7235432561772));
#75232=CARTESIAN_POINT('Origin',(28.463488507588,-2.37577956237441,15.7235432561772));
#75233=CARTESIAN_POINT('',(28.5769760048382,-2.29814685040397,15.7235432561772));
#75234=CARTESIAN_POINT('Origin',(28.5847392760352,-2.30949560012899,15.7235432561772));
#75235=CARTESIAN_POINT('',(28.5983755374519,-2.31126050085552,15.7235432561772));
#75236=CARTESIAN_POINT('Origin',(28.5983755374519,-2.31126050085552,15.7235432561772));
#75237=CARTESIAN_POINT('Origin',(28.2818235436217,-2.24790252458987,15.7235432561772));
#75238=CARTESIAN_POINT('',(28.4010521891725,-2.17941325477249,15.7235432561772));
#75239=CARTESIAN_POINT('Origin',(28.4079011161542,-2.19133611932757,15.7235432561772));
#75240=CARTESIAN_POINT('',(28.4213568690129,-2.19416546819403,15.7235432561772));
#75241=CARTESIAN_POINT('Origin',(28.4213568690129,-2.19416546819403,15.7235432561772));
#75242=CARTESIAN_POINT('Origin',(28.1107517088606,-2.10616642023779,15.7235432561772));
#75243=CARTESIAN_POINT('',(28.2349864184647,-2.04724285169689,15.7235432561772));
#75244=CARTESIAN_POINT('Origin',(28.2408787753188,-2.0596663226573,15.7235432561772));
#75245=CARTESIAN_POINT('',(28.2540710604284,-2.06354267578707,15.7235432561772));
#75246=CARTESIAN_POINT('Origin',(28.2540710604284,-2.06354267578707,15.7235432561772));
#75247=CARTESIAN_POINT('Origin',(27.9513277180533,-1.95144509953353,15.7235432561772));
#75248=CARTESIAN_POINT('',(28.0798025434136,-1.90245051566325,15.7235432561772));
#75249=CARTESIAN_POINT('Origin',(28.0847020018007,-1.91529799819928,15.7235432561772));
#75250=CARTESIAN_POINT('',(28.0975494843367,-1.92019745658631,15.7235432561772));
#75251=CARTESIAN_POINT('Origin',(28.0975494843367,-1.92019745658631,15.7235432561772));
#75252=CARTESIAN_POINT('Origin',(27.8045344731168,-1.78469247086931,15.7235432561772));
#75253=CARTESIAN_POINT('',(27.9364573242129,-1.74592893957155,15.7235432561772));
#75254=CARTESIAN_POINT('Origin',(27.9403336773427,-1.75912122468116,15.7235432561772));
#75255=CARTESIAN_POINT('',(27.9527571483031,-1.76501358153525,15.7235432561772));
#75256=CARTESIAN_POINT('Origin',(27.9527571483031,-1.76501358153525,15.7235432561772));
#75257=CARTESIAN_POINT('Origin',(27.6712770032199,-1.6069366196517,15.7235432561772));
#75258=CARTESIAN_POINT('',(27.8058345318059,-1.5786431309871,15.7235432561772));
#75259=CARTESIAN_POINT('Origin',(27.8086638806724,-1.59209888384571,15.7235432561772));
#75260=CARTESIAN_POINT('',(27.8205867452275,-1.59894781082744,15.7235432561772));
#75261=CARTESIAN_POINT('Origin',(27.8205867452275,-1.59894781082744,15.7235432561772));
#75262=CARTESIAN_POINT('Origin',(27.5523768849771,-1.4192734698133,15.7235432561772));
#75263=CARTESIAN_POINT('',(27.6887394991444,-1.40162446254801,15.7235432561772));
#75264=CARTESIAN_POINT('Origin',(27.690504399871,-1.41526072396474,15.7235432561772));
#75265=CARTESIAN_POINT('',(27.701853149596,-1.42302399516179,15.7235432561772));
#75266=CARTESIAN_POINT('Origin',(27.701853149596,-1.42302399516179,15.7235432561772));
#75267=CARTESIAN_POINT('Origin',(27.4485671771557,-1.22286002707717,15.7235432561772));
#75268=CARTESIAN_POINT('',(27.5858941560428,-1.21596431320988,15.7235432561772));
#75269=CARTESIAN_POINT('Origin',(27.5865837274296,-1.22969701109859,15.7235432561772));
#75270=CARTESIAN_POINT('',(27.5972883935086,-1.23832676336246,15.7235432561772));
#75271=CARTESIAN_POINT('Origin',(27.5972883935086,-1.23832676336246,15.7235432561772));
#75272=CARTESIAN_POINT('Origin',(27.3604879011247,-1.01890724563189,15.7235432561772));
#75273=CARTESIAN_POINT('',(27.4979325782409,-1.02280733953164,15.7235432561772));
#75274=CARTESIAN_POINT('Origin',(27.4975425688509,-1.03655180724326,15.7235432561772));
#75275=CARTESIAN_POINT('',(27.507537153458,-1.04599483528157,15.7235432561772));
#75276=CARTESIAN_POINT('Origin',(27.507537153458,-1.04599483528157,15.7235432561772));
#75277=CARTESIAN_POINT('Origin',(27.2886820949101,-0.808672562196254,15.7235432561772));
#75278=CARTESIAN_POINT('',(27.4253970781159,-0.823344418487241,15.7235432561772));
#75279=CARTESIAN_POINT('Origin',(27.4239298924868,-0.837015916807826,15.7235432561772));
#75280=CARTESIAN_POINT('',(27.4331527756843,-0.847214001212589,15.7235432561772));
#75281=CARTESIAN_POINT('Origin',(27.4331527756843,-0.847214001212589,15.7235432561772));
#75282=CARTESIAN_POINT('Origin',(27.233592465185,-0.593452143503757,15.7235432561772));
#75283=CARTESIAN_POINT('',(27.3687348611467,-0.618805305313063,15.7235432561772));
#75284=CARTESIAN_POINT('Origin',(27.3661995449658,-0.632319544909233,15.7235432561772));
#75285=CARTESIAN_POINT('',(27.3745938646118,-0.643209811098888,15.7235432561772));
#75286=CARTESIAN_POINT('Origin',(27.3745938646118,-0.643209811098888,15.7235432561772));
#75287=CARTESIAN_POINT('Origin',(27.195558657836,-0.374572895003696,15.7235432561772));
#75288=CARTESIAN_POINT('',(27.328295268743,-0.410451051657984,15.7235432561772));
#75289=CARTESIAN_POINT('Origin',(27.3247074530776,-0.423724712748689,15.7235432561772));
#75290=CARTESIAN_POINT('',(27.3322214554001,-0.435240018610796,15.7235432561772));
#75291=CARTESIAN_POINT('Origin',(27.3322214554001,-0.435240018610796,15.7235432561772));
#75292=CARTESIAN_POINT('Origin',(27.1748151639327,-0.153384280047813,15.7235432561772));
#75293=CARTESIAN_POINT('',(27.3043276244395,-0.199566230780611,15.7235432561772));
#75294=CARTESIAN_POINT('Origin',(27.2997094293662,-0.212517476831286,15.7235432561772));
#75295=CARTESIAN_POINT('',(27.3062967880422,-0.224586826675978,15.7235432561772));
#75296=CARTESIAN_POINT('Origin',(27.3062967880422,-0.224586826675978,15.7235432561772));
#75297=CARTESIAN_POINT('Origin',(27.1714898740131,0.068750000000016,15.7235432561772));
#75298=CARTESIAN_POINT('Origin',(27.2969796967333,-0.0125489822720016,15.7235432561772));
#75299=CARTESIAN_POINT('Origin',(27.1856032895953,0.29046041343615,15.7235432561772));
#75300=CARTESIAN_POINT('Origin',(27.3043276244395,0.199566230780642,15.7235432561772));
#75301=CARTESIAN_POINT('Origin',(27.217068396779,0.510380041835561,15.7235432561772));
#75302=CARTESIAN_POINT('Origin',(27.328295268743,0.410451051658016,15.7235432561772));
#75303=CARTESIAN_POINT('Origin',(27.2656912027152,0.727153007558468,15.7235432561772));
#75304=CARTESIAN_POINT('Origin',(27.3687348611468,0.618805305313091,15.7235432561772));
#75305=CARTESIAN_POINT('Origin',(27.3311719316367,0.939442833186866,15.7235432561772));
#75306=CARTESIAN_POINT('Origin',(27.4253970781159,0.823344418487269,15.7235432561772));
#75307=CARTESIAN_POINT('Origin',(27.4131068730749,1.14594068135223,15.7235432561772));
#75308=CARTESIAN_POINT('Origin',(27.4979325782409,1.02280733953167,15.7235432561772));
#75309=CARTESIAN_POINT('',(0.,0.,0.));
#75310=CARTESIAN_POINT('',(2.66219623717201,3.90779490297551,-4.17888423737383));
#75311=CARTESIAN_POINT('',(-0.450437150538809,-3.29757629864905,13.6231784544421));
#75312=CARTESIAN_POINT('',(1.86458713476396,-0.0823799534263743,2.65415071831438));
#75313=CARTESIAN_POINT('',(-1.33226762955019E-14,-6.21898366137685E-15,
0.324647532568744));
#75314=CARTESIAN_POINT('',(6.52401103559491E-9,-0.000625648391467968,0.324647532568794));
#75315=CARTESIAN_POINT('',(-44.9999999934761,-25.9813877619247,0.324647532568666));
#75316=CARTESIAN_POINT('',(-45.0000000000001,25.9807621135332,0.324647532568713));
#75317=UNCERTAINTY_MEASURE_WITH_UNIT(LENGTH_MEASURE(0.01),#75337,
'DISTANCE_ACCURACY_VALUE',
'Maximum model space distance between geometric entities at asserted c
onnectivities');
#75318=UNCERTAINTY_MEASURE_WITH_UNIT(LENGTH_MEASURE(0.01),#75337,
'DISTANCE_ACCURACY_VALUE',
'Maximum model space distance between geometric entities at asserted c
onnectivities');
#75319=UNCERTAINTY_MEASURE_WITH_UNIT(LENGTH_MEASURE(0.01),#75337,
'DISTANCE_ACCURACY_VALUE',
'Maximum model space distance between geometric entities at asserted c
onnectivities');
#75320=UNCERTAINTY_MEASURE_WITH_UNIT(LENGTH_MEASURE(0.01),#75337,
'DISTANCE_ACCURACY_VALUE',
'Maximum model space distance between geometric entities at asserted c
onnectivities');
#75321=UNCERTAINTY_MEASURE_WITH_UNIT(LENGTH_MEASURE(0.01),#75337,
'DISTANCE_ACCURACY_VALUE',
'Maximum model space distance between geometric entities at asserted c
onnectivities');
#75322=UNCERTAINTY_MEASURE_WITH_UNIT(LENGTH_MEASURE(0.01),#75337,
'DISTANCE_ACCURACY_VALUE',
'Maximum model space distance between geometric entities at asserted c
onnectivities');
#75323=UNCERTAINTY_MEASURE_WITH_UNIT(LENGTH_MEASURE(0.01),#75337,
'DISTANCE_ACCURACY_VALUE',
'Maximum model space distance between geometric entities at asserted c
onnectivities');
#75324=UNCERTAINTY_MEASURE_WITH_UNIT(LENGTH_MEASURE(0.01),#75337,
'DISTANCE_ACCURACY_VALUE',
'Maximum model space distance between geometric entities at asserted c
onnectivities');
#75325=UNCERTAINTY_MEASURE_WITH_UNIT(LENGTH_MEASURE(0.01),#75337,
'DISTANCE_ACCURACY_VALUE',
'Maximum model space distance between geometric entities at asserted c
onnectivities');
#75326=UNCERTAINTY_MEASURE_WITH_UNIT(LENGTH_MEASURE(0.01),#75337,
'DISTANCE_ACCURACY_VALUE',
'Maximum model space distance between geometric entities at asserted c
onnectivities');
#75327=(
GEOMETRIC_REPRESENTATION_CONTEXT(3)
GLOBAL_UNCERTAINTY_ASSIGNED_CONTEXT((#75317))
GLOBAL_UNIT_ASSIGNED_CONTEXT((#75337,#75339,#75340))
REPRESENTATION_CONTEXT('','3D')
);
#75328=(
GEOMETRIC_REPRESENTATION_CONTEXT(3)
GLOBAL_UNCERTAINTY_ASSIGNED_CONTEXT((#75318))
GLOBAL_UNIT_ASSIGNED_CONTEXT((#75337,#75339,#75340))
REPRESENTATION_CONTEXT('','3D')
);
#75329=(
GEOMETRIC_REPRESENTATION_CONTEXT(3)
GLOBAL_UNCERTAINTY_ASSIGNED_CONTEXT((#75319))
GLOBAL_UNIT_ASSIGNED_CONTEXT((#75337,#75339,#75340))
REPRESENTATION_CONTEXT('','3D')
);
#75330=(
GEOMETRIC_REPRESENTATION_CONTEXT(3)
GLOBAL_UNCERTAINTY_ASSIGNED_CONTEXT((#75320))
GLOBAL_UNIT_ASSIGNED_CONTEXT((#75337,#75339,#75340))
REPRESENTATION_CONTEXT('','3D')
);
#75331=(
GEOMETRIC_REPRESENTATION_CONTEXT(3)
GLOBAL_UNCERTAINTY_ASSIGNED_CONTEXT((#75321))
GLOBAL_UNIT_ASSIGNED_CONTEXT((#75337,#75339,#75340))
REPRESENTATION_CONTEXT('','3D')
);
#75332=(
GEOMETRIC_REPRESENTATION_CONTEXT(3)
GLOBAL_UNCERTAINTY_ASSIGNED_CONTEXT((#75322))
GLOBAL_UNIT_ASSIGNED_CONTEXT((#75337,#75339,#75340))
REPRESENTATION_CONTEXT('','3D')
);
#75333=(
GEOMETRIC_REPRESENTATION_CONTEXT(3)
GLOBAL_UNCERTAINTY_ASSIGNED_CONTEXT((#75323))
GLOBAL_UNIT_ASSIGNED_CONTEXT((#75337,#75339,#75340))
REPRESENTATION_CONTEXT('','3D')
);
#75334=(
GEOMETRIC_REPRESENTATION_CONTEXT(3)
GLOBAL_UNCERTAINTY_ASSIGNED_CONTEXT((#75324))
GLOBAL_UNIT_ASSIGNED_CONTEXT((#75337,#75339,#75340))
REPRESENTATION_CONTEXT('','3D')
);
#75335=(
GEOMETRIC_REPRESENTATION_CONTEXT(3)
GLOBAL_UNCERTAINTY_ASSIGNED_CONTEXT((#75325))
GLOBAL_UNIT_ASSIGNED_CONTEXT((#75337,#75339,#75340))
REPRESENTATION_CONTEXT('','3D')
);
#75336=(
GEOMETRIC_REPRESENTATION_CONTEXT(3)
GLOBAL_UNCERTAINTY_ASSIGNED_CONTEXT((#75326))
GLOBAL_UNIT_ASSIGNED_CONTEXT((#75337,#75339,#75340))
REPRESENTATION_CONTEXT('','3D')
);
#75337=(
LENGTH_UNIT()
NAMED_UNIT(*)
SI_UNIT(.MILLI.,.METRE.)
);
#75338=(
LENGTH_UNIT()
NAMED_UNIT(*)
SI_UNIT($,.METRE.)
);
#75339=(
NAMED_UNIT(*)
PLANE_ANGLE_UNIT()
SI_UNIT($,.RADIAN.)
);
#75340=(
NAMED_UNIT(*)
SI_UNIT($,.STERADIAN.)
SOLID_ANGLE_UNIT()
);
#75341=SHAPE_DEFINITION_REPRESENTATION(#75350,#75367);
#75342=SHAPE_DEFINITION_REPRESENTATION(#75351,#75368);
#75343=SHAPE_DEFINITION_REPRESENTATION(#75352,#75369);
#75344=SHAPE_DEFINITION_REPRESENTATION(#75353,#75370);
#75345=SHAPE_DEFINITION_REPRESENTATION(#75354,#75371);
#75346=SHAPE_DEFINITION_REPRESENTATION(#75355,#75372);
#75347=SHAPE_DEFINITION_REPRESENTATION(#75356,#75373);
#75348=SHAPE_DEFINITION_REPRESENTATION(#75357,#75374);
#75349=SHAPE_DEFINITION_REPRESENTATION(#75358,#75375);
#75350=PRODUCT_DEFINITION_SHAPE('',$,#75377);
#75351=PRODUCT_DEFINITION_SHAPE('',$,#75378);
#75352=PRODUCT_DEFINITION_SHAPE('',$,#75379);
#75353=PRODUCT_DEFINITION_SHAPE('',$,#75380);
#75354=PRODUCT_DEFINITION_SHAPE('',$,#75381);
#75355=PRODUCT_DEFINITION_SHAPE('',$,#75382);
#75356=PRODUCT_DEFINITION_SHAPE('',$,#75383);
#75357=PRODUCT_DEFINITION_SHAPE('',$,#75384);
#75358=PRODUCT_DEFINITION_SHAPE('',$,#75385);
#75359=PRODUCT_DEFINITION_SHAPE($,$,#35);
#75360=PRODUCT_DEFINITION_SHAPE($,$,#36);
#75361=PRODUCT_DEFINITION_SHAPE($,$,#37);
#75362=PRODUCT_DEFINITION_SHAPE($,$,#38);
#75363=PRODUCT_DEFINITION_SHAPE($,$,#39);
#75364=PRODUCT_DEFINITION_SHAPE($,$,#40);
#75365=PRODUCT_DEFINITION_SHAPE($,$,#41);
#75366=PRODUCT_DEFINITION_SHAPE($,$,#42);
#75367=SHAPE_REPRESENTATION('',(#32118,#36337,#36338,#36339,#36340,#36341,
#36342,#36343,#36344),#75327);
#75368=SHAPE_REPRESENTATION('',(#32119),#75328);
#75369=SHAPE_REPRESENTATION('',(#32134),#75329);
#75370=SHAPE_REPRESENTATION('',(#32137),#75330);
#75371=SHAPE_REPRESENTATION('',(#32140),#75331);
#75372=SHAPE_REPRESENTATION('',(#32143),#75332);
#75373=SHAPE_REPRESENTATION('',(#32197),#75333);
#75374=SHAPE_REPRESENTATION('',(#33577),#75334);
#75375=SHAPE_REPRESENTATION('',(#34957),#75335);
#75376=PRODUCT_DEFINITION_CONTEXT('part definition',#75405,'design');
#75377=PRODUCT_DEFINITION('BR-152','BR-152',#75386,#75376);
#75378=PRODUCT_DEFINITION('base','Base',#75387,#75376);
#75379=PRODUCT_DEFINITION('Ball_01','Ball_01',#75388,#75376);
#75380=PRODUCT_DEFINITION('Ball_02','Ball_02',#75389,#75376);
#75381=PRODUCT_DEFINITION('Ball_03','Ball_03',#75390,#75376);
#75382=PRODUCT_DEFINITION('Top_Part','Top_Part',#75391,#75376);
#75383=PRODUCT_DEFINITION('Screw_01','Screw_01',#75392,#75376);
#75384=PRODUCT_DEFINITION('Screw_02','Screw_02',#75393,#75376);
#75385=PRODUCT_DEFINITION('Screw_03','Screw_03',#75394,#75376);
#75386=PRODUCT_DEFINITION_FORMATION('',$,#75407);
#75387=PRODUCT_DEFINITION_FORMATION('',$,#75408);
#75388=PRODUCT_DEFINITION_FORMATION('',$,#75409);
#75389=PRODUCT_DEFINITION_FORMATION('',$,#75410);
#75390=PRODUCT_DEFINITION_FORMATION('',$,#75411);
#75391=PRODUCT_DEFINITION_FORMATION('',$,#75412);
#75392=PRODUCT_DEFINITION_FORMATION('',$,#75413);
#75393=PRODUCT_DEFINITION_FORMATION('',$,#75414);
#75394=PRODUCT_DEFINITION_FORMATION('',$,#75415);
#75395=PRODUCT_RELATED_PRODUCT_CATEGORY('BR-152','BR-152',(#75407));
#75396=PRODUCT_RELATED_PRODUCT_CATEGORY('Base','Base',(#75408));
#75397=PRODUCT_RELATED_PRODUCT_CATEGORY('Ball_01','Ball_01',(#75409));
#75398=PRODUCT_RELATED_PRODUCT_CATEGORY('Ball_02','Ball_02',(#75410));
#75399=PRODUCT_RELATED_PRODUCT_CATEGORY('Ball_03','Ball_03',(#75411));
#75400=PRODUCT_RELATED_PRODUCT_CATEGORY('Top_Part','Top_Part',(#75412));
#75401=PRODUCT_RELATED_PRODUCT_CATEGORY('Screw_01','Screw_01',(#75413));
#75402=PRODUCT_RELATED_PRODUCT_CATEGORY('Screw_02','Screw_02',(#75414));
#75403=PRODUCT_RELATED_PRODUCT_CATEGORY('Screw_03','Screw_03',(#75415));
#75404=APPLICATION_PROTOCOL_DEFINITION('international standard',
'automotive_design',2009,#75405);
#75405=APPLICATION_CONTEXT(
'Core Data for Automotive Mechanical Design Process');
#75406=PRODUCT_CONTEXT('part definition',#75405,'mechanical');
#75407=PRODUCT('BR-152','BR-152',$,(#75406));
#75408=PRODUCT('base','Base',$,(#75406));
#75409=PRODUCT('Ball_01','Ball_01',$,(#75406));
#75410=PRODUCT('Ball_02','Ball_02',$,(#75406));
#75411=PRODUCT('Ball_03','Ball_03',$,(#75406));
#75412=PRODUCT('Top_Part','Top_Part',$,(#75406));
#75413=PRODUCT('Screw_01','Screw_01',$,(#75406));
#75414=PRODUCT('Screw_02','Screw_02',$,(#75406));
#75415=PRODUCT('Screw_03','Screw_03',$,(#75406));
#75416=PRESENTATION_STYLE_ASSIGNMENT((#75420));
#75417=PRESENTATION_STYLE_ASSIGNMENT((#75421));
#75418=PRESENTATION_STYLE_ASSIGNMENT((#75422));
#75419=PRESENTATION_STYLE_ASSIGNMENT((#75423));
#75420=SURFACE_STYLE_USAGE(.BOTH.,#75424);
#75421=SURFACE_STYLE_USAGE(.BOTH.,#75425);
#75422=SURFACE_STYLE_USAGE(.BOTH.,#75426);
#75423=SURFACE_STYLE_USAGE(.BOTH.,#75427);
#75424=SURFACE_SIDE_STYLE('',(#75428));
#75425=SURFACE_SIDE_STYLE('',(#75429));
#75426=SURFACE_SIDE_STYLE('',(#75430));
#75427=SURFACE_SIDE_STYLE('',(#75431));
#75428=SURFACE_STYLE_FILL_AREA(#75432);
#75429=SURFACE_STYLE_FILL_AREA(#75433);
#75430=SURFACE_STYLE_FILL_AREA(#75434);
#75431=SURFACE_STYLE_FILL_AREA(#75435);
#75432=FILL_AREA_STYLE('Steel - Satin',(#75436));
#75433=FILL_AREA_STYLE('Opaque(203,203,203)',(#75437));
#75434=FILL_AREA_STYLE('Opaque(200,203,41)',(#75438));
#75435=FILL_AREA_STYLE('Opaque(86,86,86)',(#75439));
#75436=FILL_AREA_STYLE_COLOUR('Steel - Satin',#75440);
#75437=FILL_AREA_STYLE_COLOUR('Opaque(203,203,203)',#75441);
#75438=FILL_AREA_STYLE_COLOUR('Opaque(200,203,41)',#75442);
#75439=FILL_AREA_STYLE_COLOUR('Opaque(86,86,86)',#75443);
#75440=COLOUR_RGB('Steel - Satin', 0.09019608, 0.27058824, 0.51372549);
#75441=COLOUR_RGB('Opaque(203,203,203)', 0.09019608, 0.27058824, 0.51372549);
#75442=COLOUR_RGB('Opaque(200,203,41)', 0.66274510, 0.83137255, 0.94901961);
#75443=COLOUR_RGB('Opaque(86,86,86)', 0.08235294, 0.09019608, 0.10196078);
ENDSEC;
END-ISO-10303-21;
